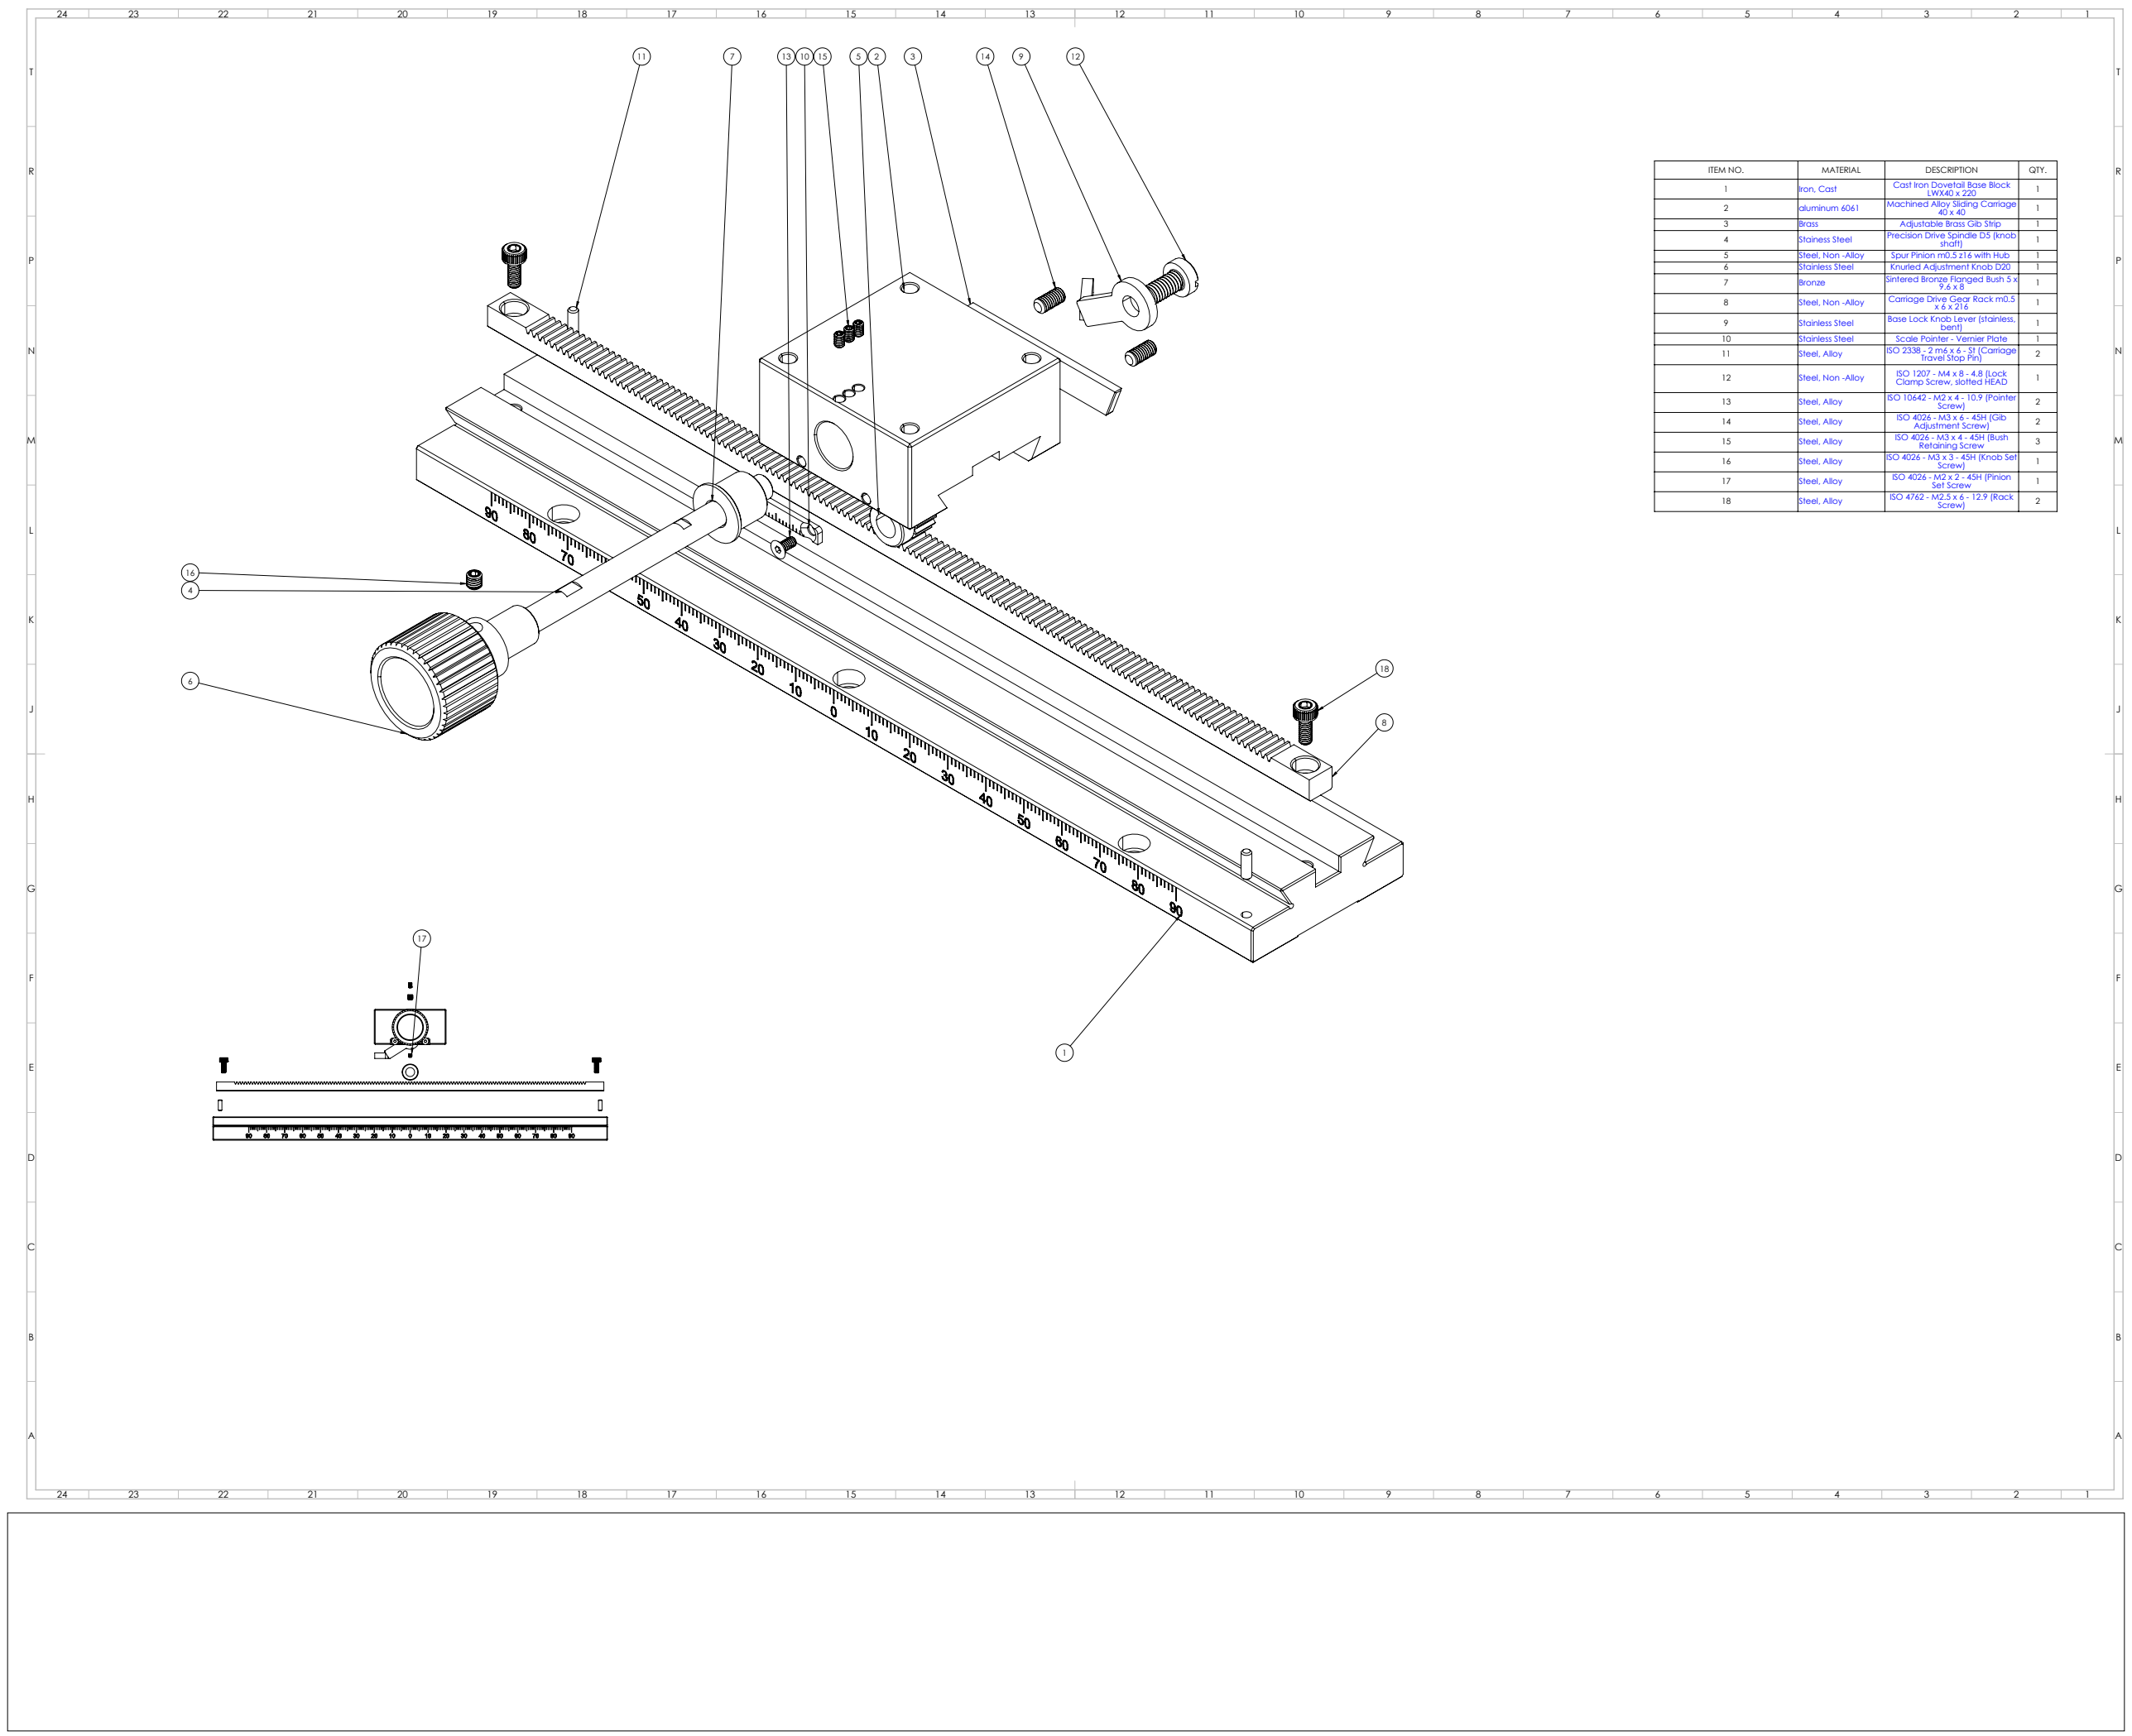
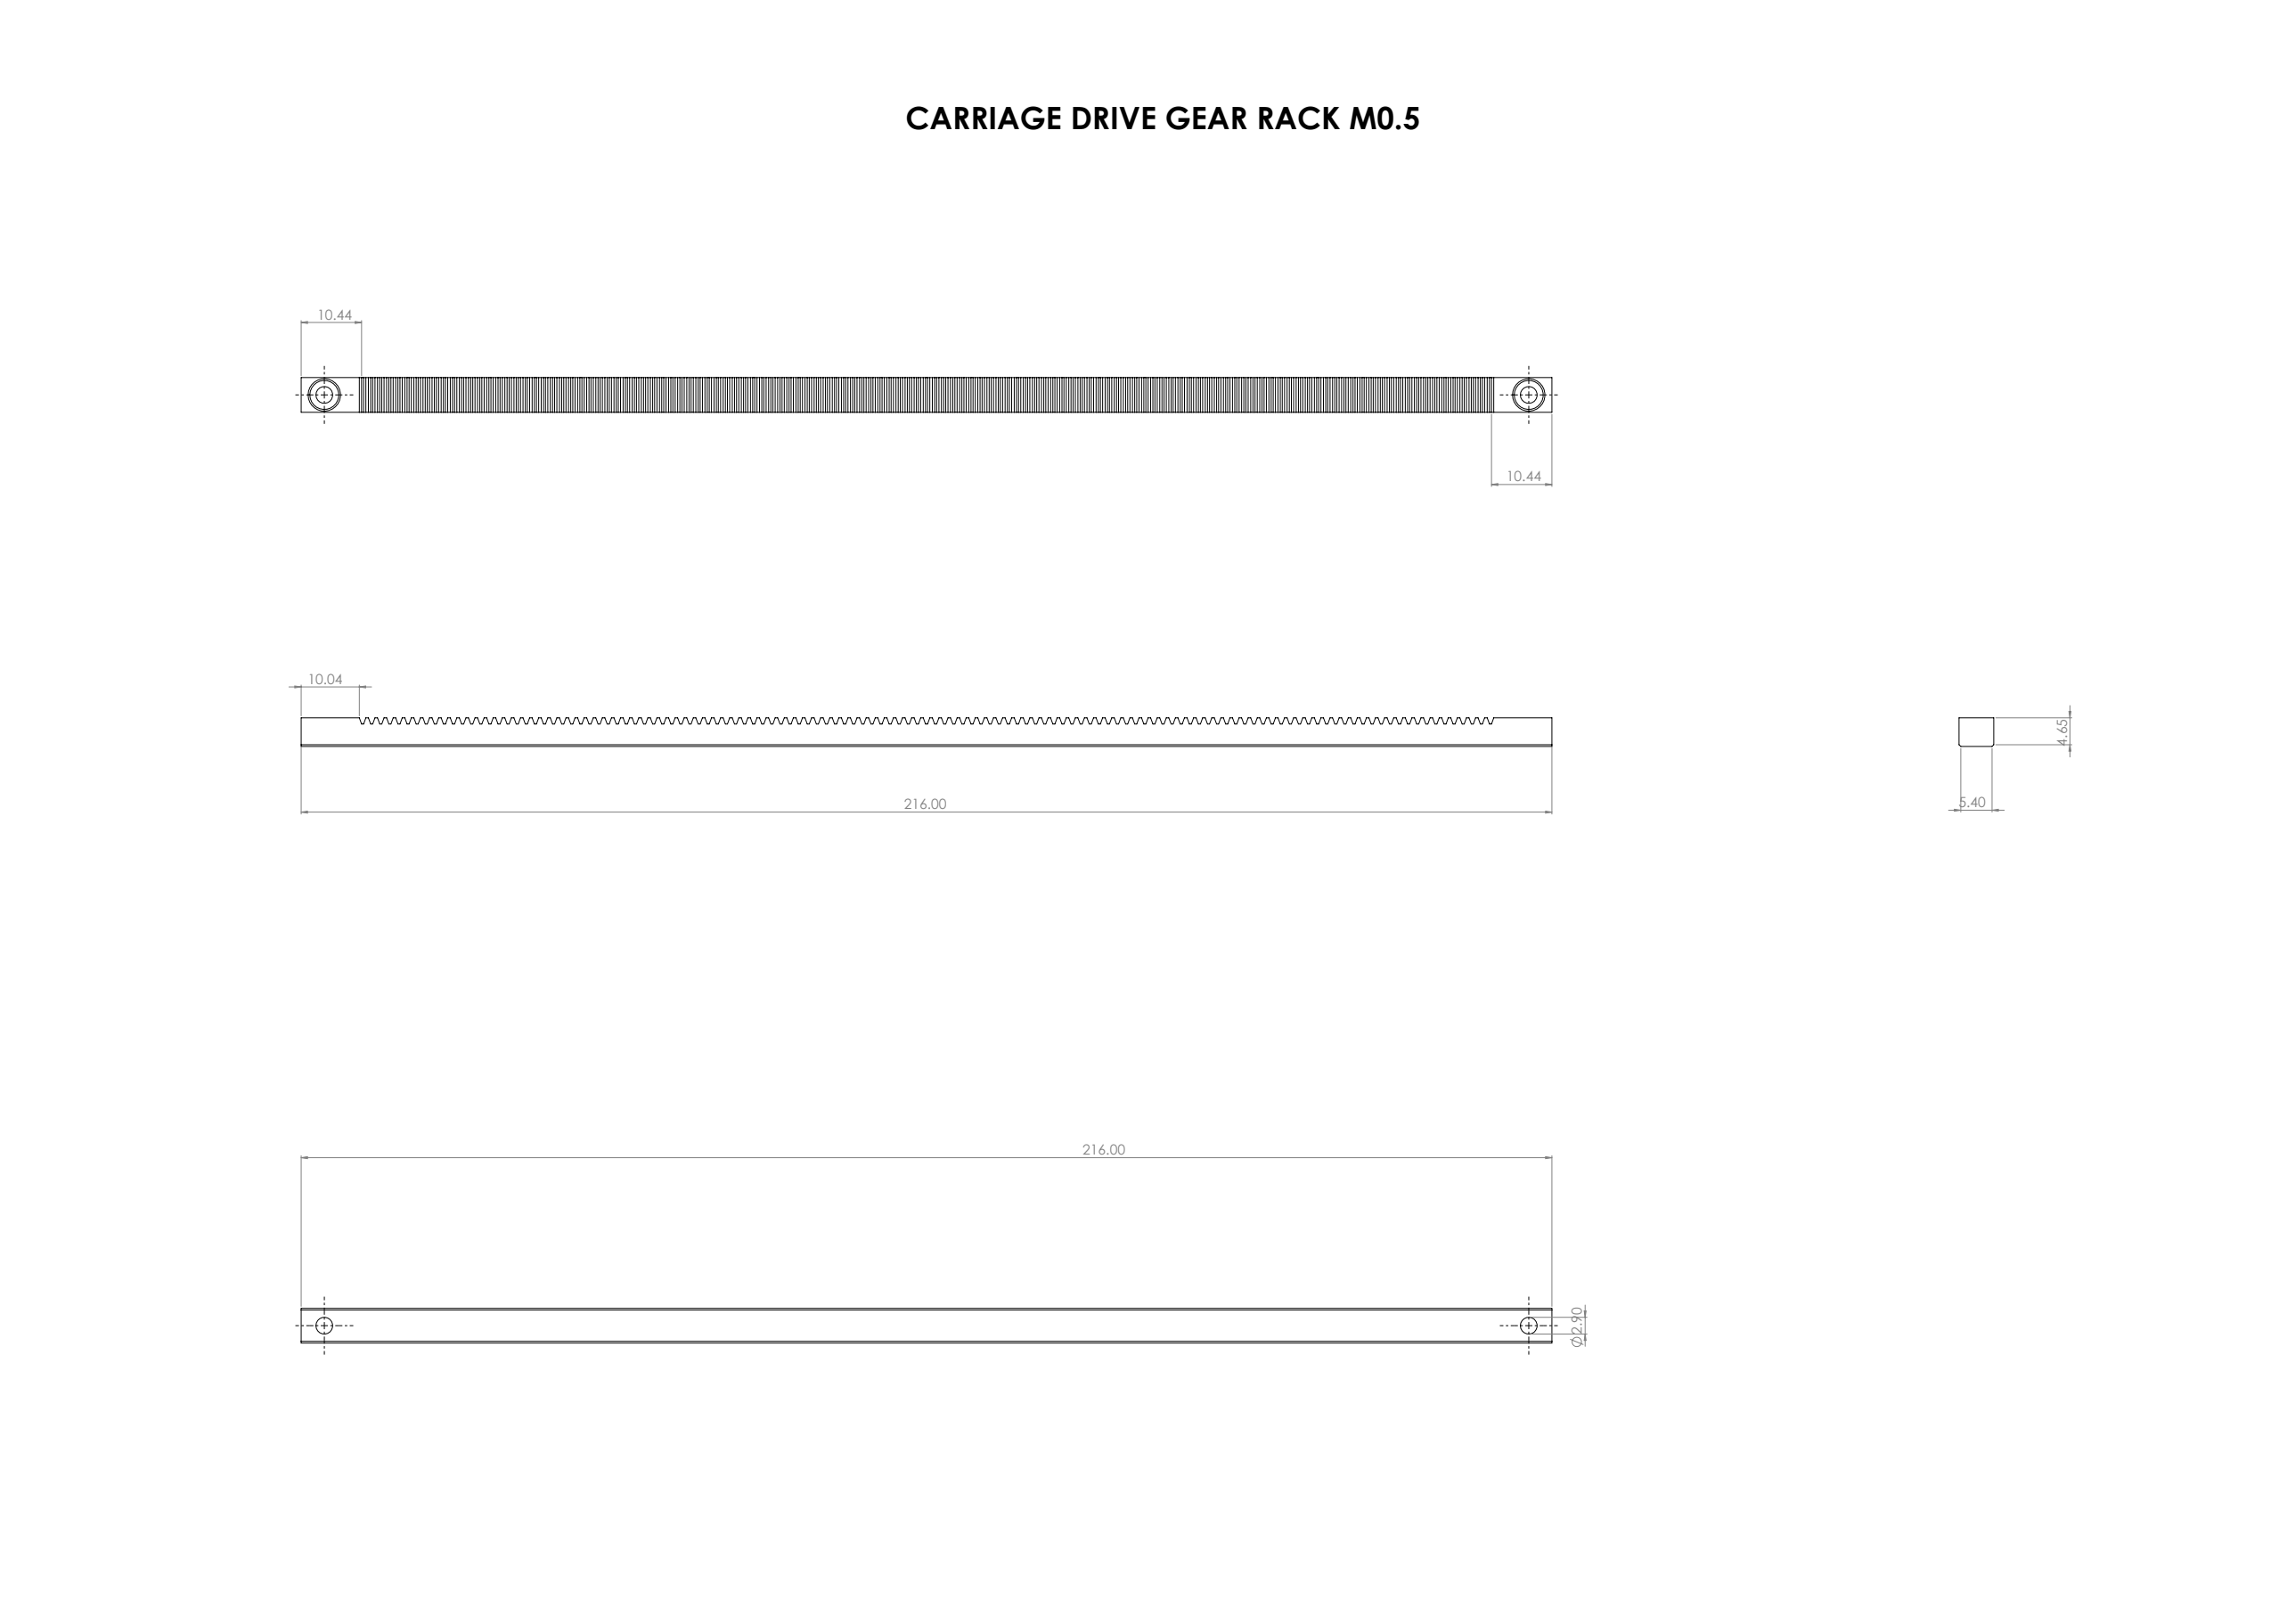
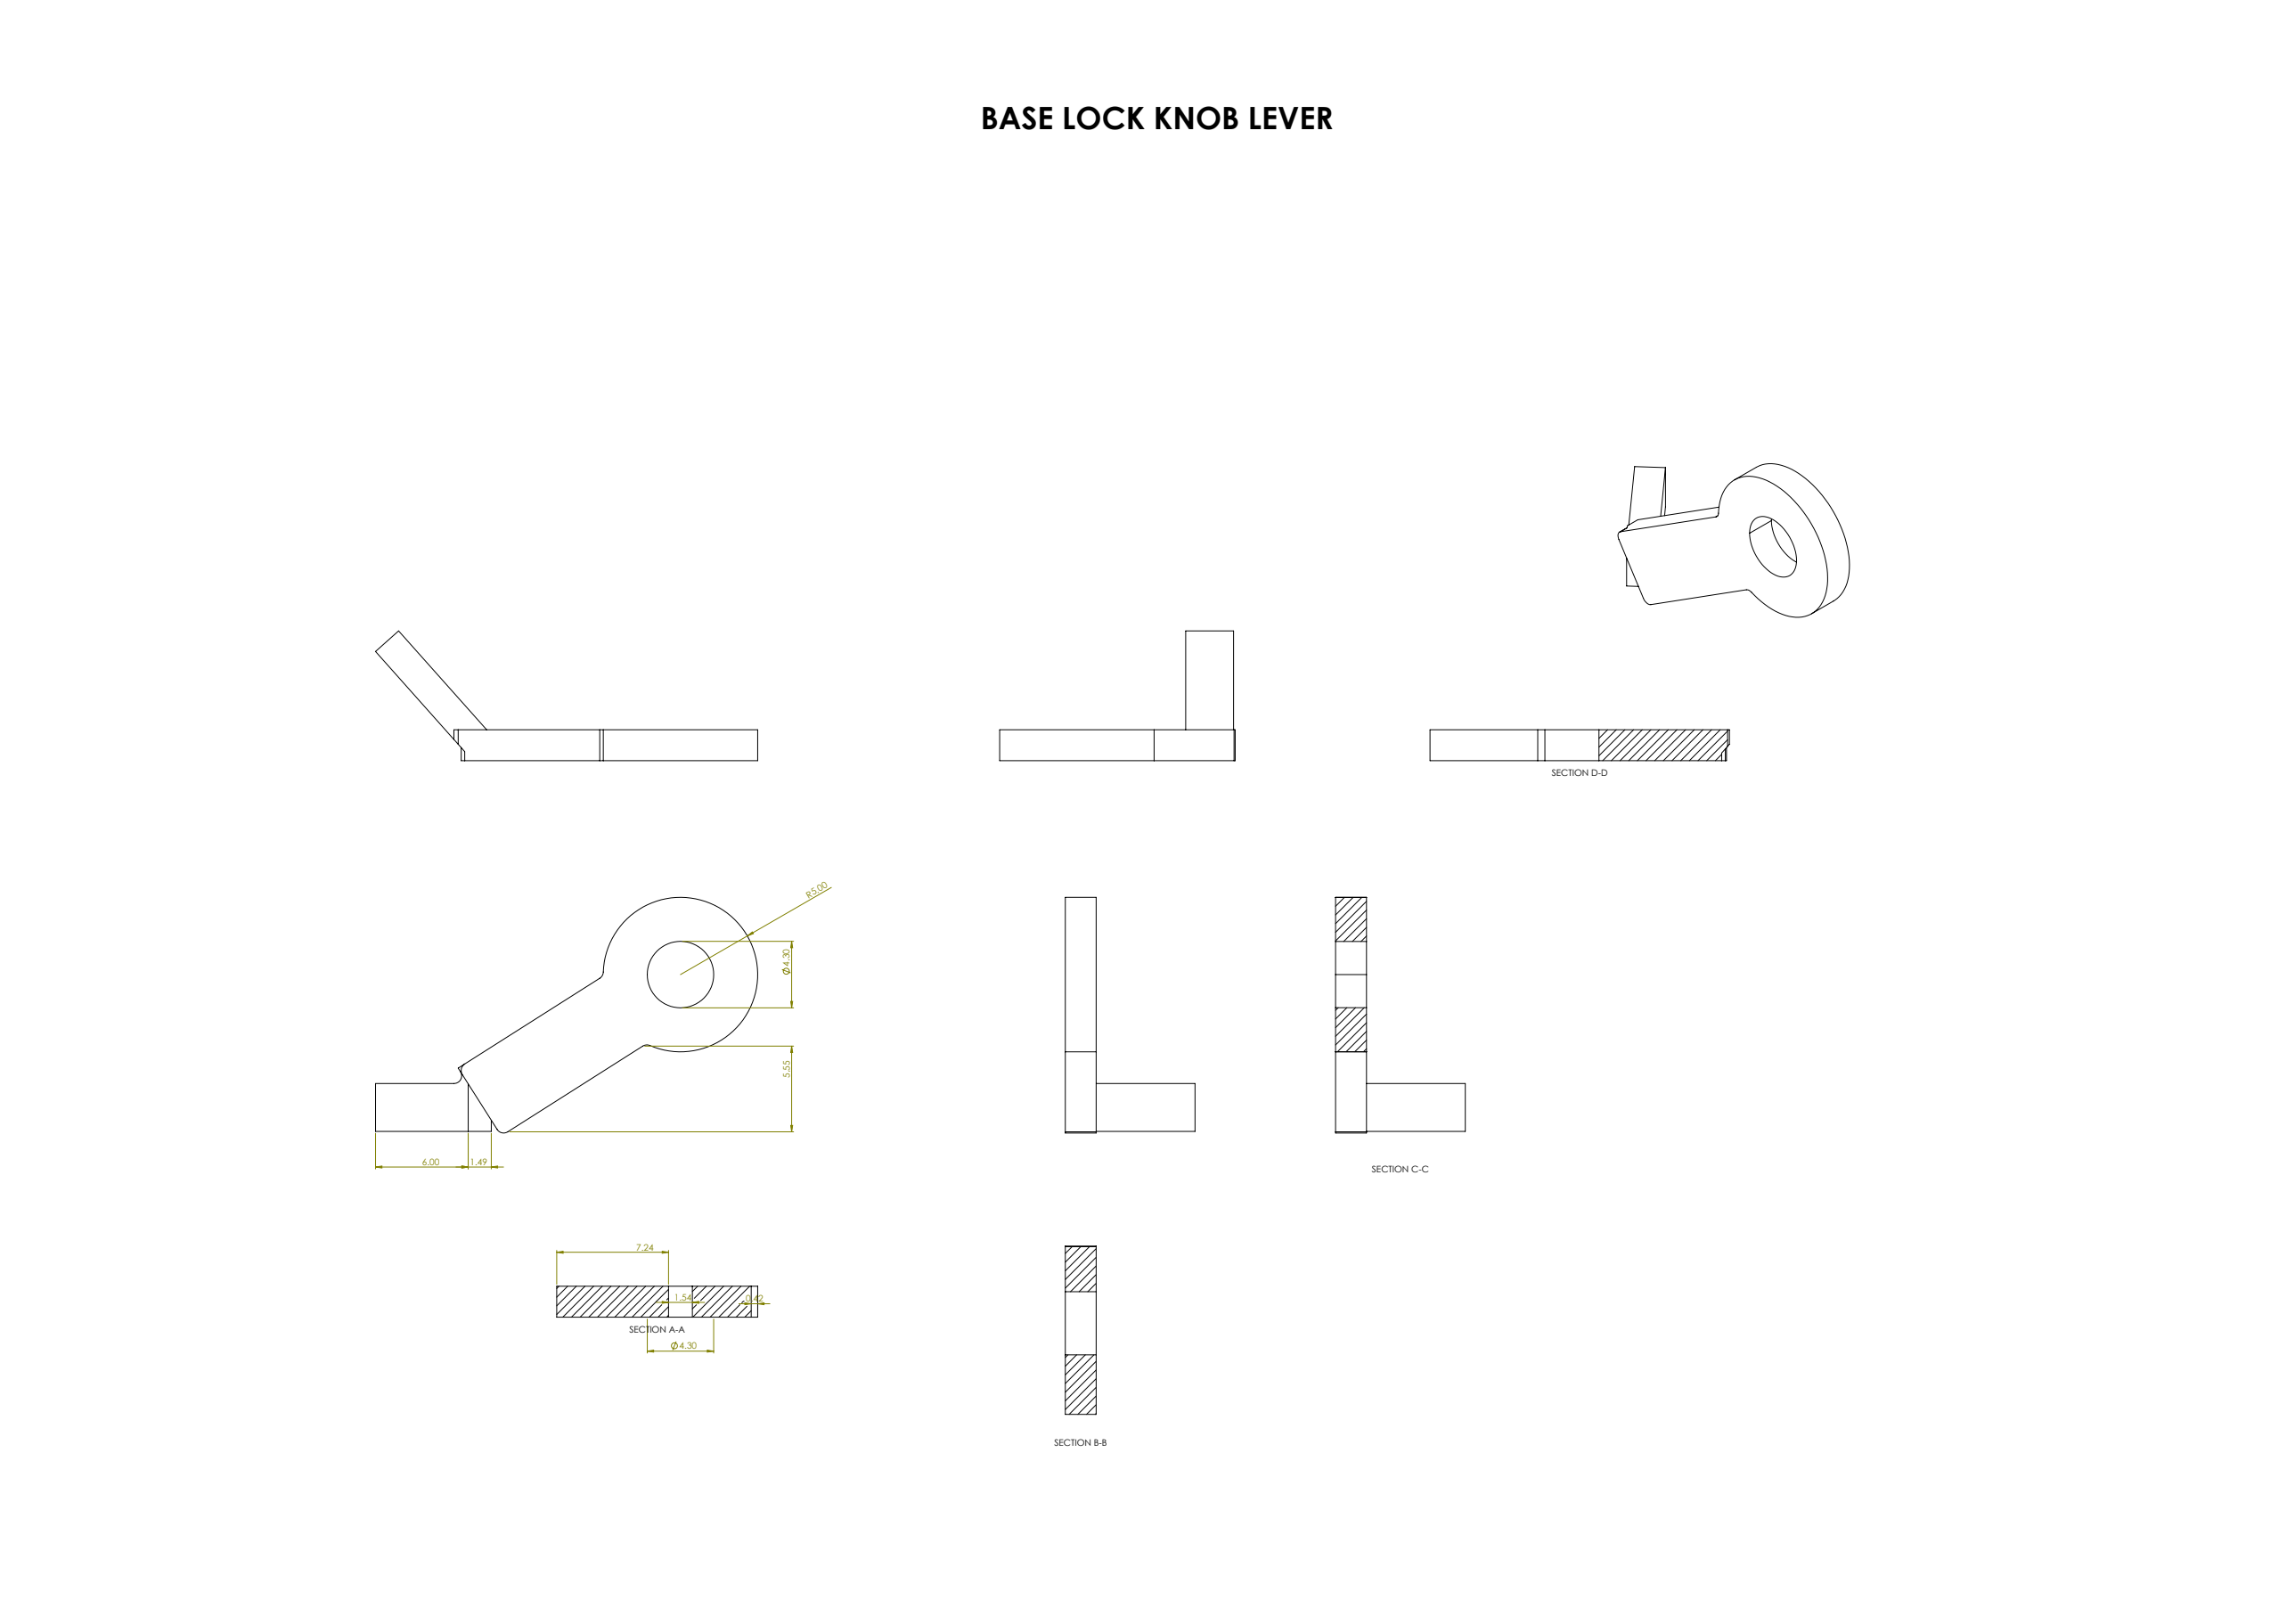
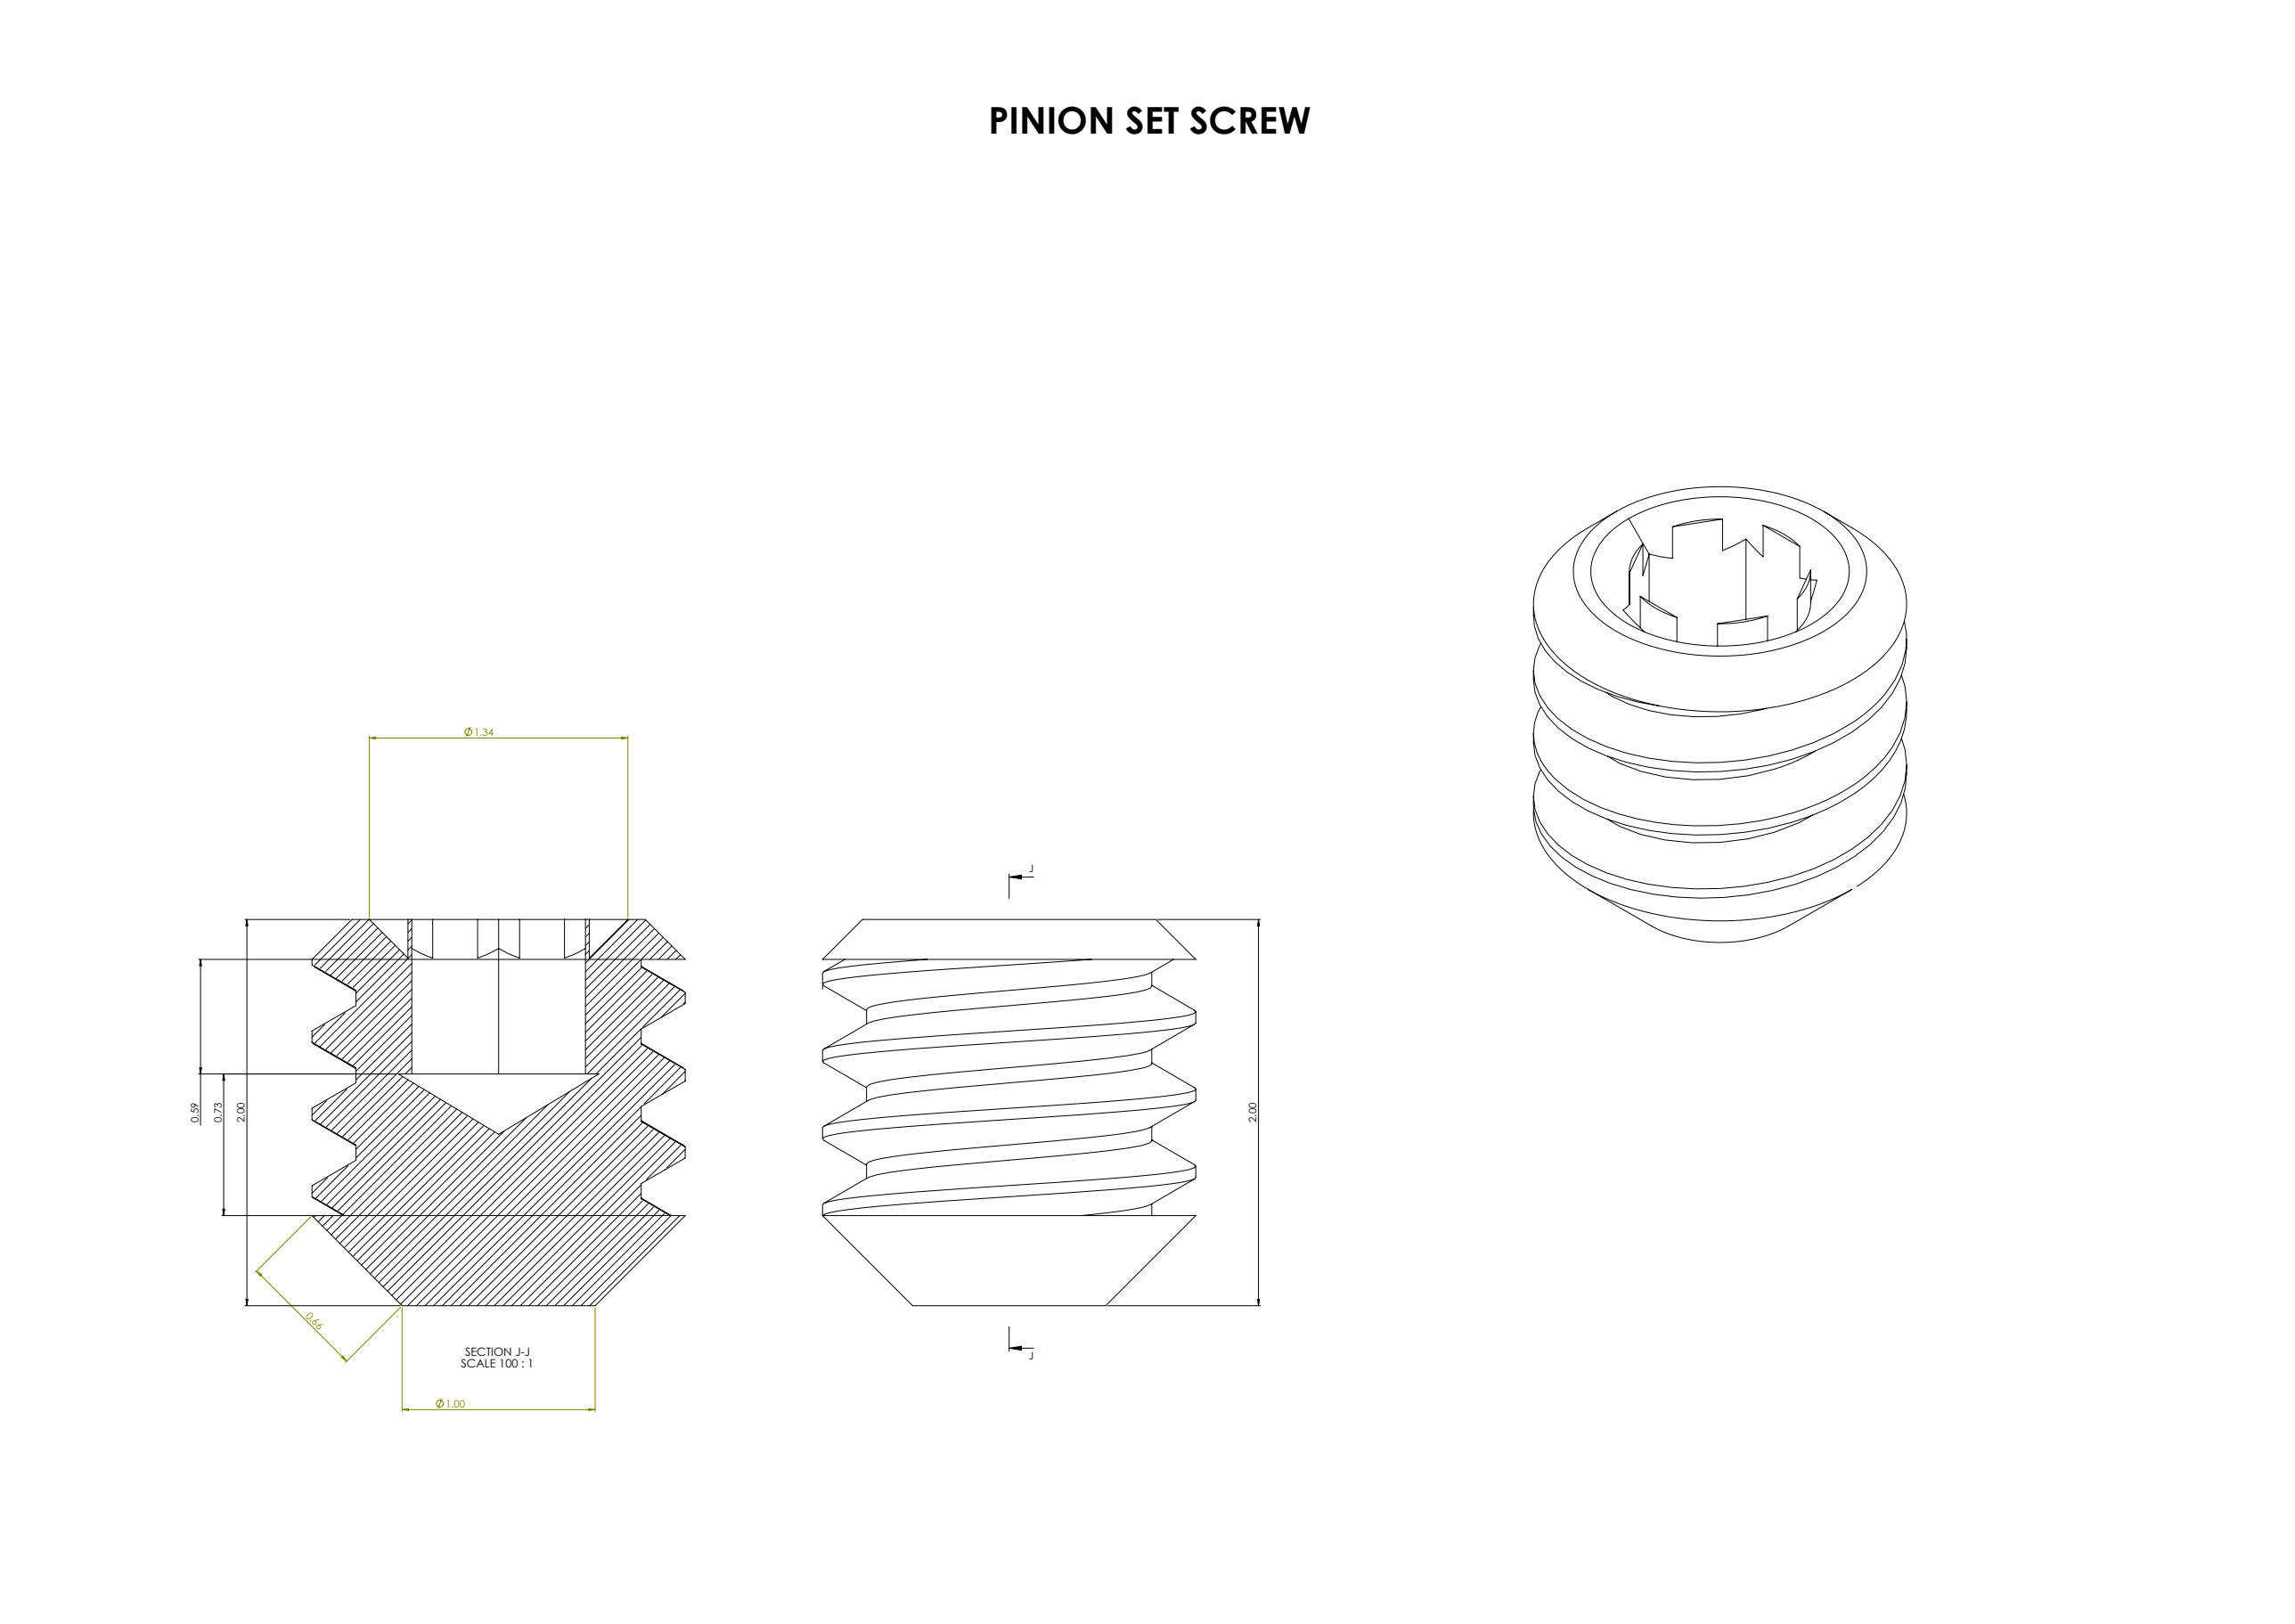
ISO-10303-21;
HEADER;
/* Generated by software containing ST-Developer
 * from STEP Tools, Inc. (www.steptools.com) 
 */

FILE_DESCRIPTION(
/* description */ (''),
/* implementation_level */ '2;1');

FILE_NAME(
/* name */ 'MAS-254',
/* time_stamp */ '2026-10-05T09:57:53+05:00',
/* author */ (''),
/* organization */ (''),
/* preprocessor_version */ 'ST-DEVELOPER v20.2',
/* originating_system */ 'Autodesk Translation Framework v15.15.0.0',
/* authorisation */ '');

FILE_SCHEMA (('AUTOMOTIVE_DESIGN { 1 0 10303 214 3 1 1 }'));
ENDSEC;

DATA;
#10=MECHANICAL_DESIGN_GEOMETRIC_PRESENTATION_REPRESENTATION('',(#551,#552,
#553,#554,#555,#556,#557,#558,#559,#560,#561,#562,#563,#564,#565,#566,#567,
#568),#113984);
#11=ITEM_DEFINED_TRANSFORMATION($,$,#60610,#63752);
#12=ITEM_DEFINED_TRANSFORMATION($,$,#61812,#63753);
#13=ITEM_DEFINED_TRANSFORMATION($,$,#61948,#63754);
#14=ITEM_DEFINED_TRANSFORMATION($,$,#61969,#63755);
#15=ITEM_DEFINED_TRANSFORMATION($,$,#61989,#63756);
#16=ITEM_DEFINED_TRANSFORMATION($,$,#62138,#63757);
#17=ITEM_DEFINED_TRANSFORMATION($,$,#62375,#63758);
#18=ITEM_DEFINED_TRANSFORMATION($,$,#62396,#63759);
#19=ITEM_DEFINED_TRANSFORMATION($,$,#62923,#63760);
#20=ITEM_DEFINED_TRANSFORMATION($,$,#62957,#63761);
#21=ITEM_DEFINED_TRANSFORMATION($,$,#63742,#63762);
#22=ITEM_DEFINED_TRANSFORMATION($,$,#63058,#63763);
#23=ITEM_DEFINED_TRANSFORMATION($,$,#63421,#63764);
#24=ITEM_DEFINED_TRANSFORMATION($,$,#63259,#63765);
#25=ITEM_DEFINED_TRANSFORMATION($,$,#63344,#63766);
#26=ITEM_DEFINED_TRANSFORMATION($,$,#63115,#63767);
#27=ITEM_DEFINED_TRANSFORMATION($,$,#63188,#63768);
#28=ITEM_DEFINED_TRANSFORMATION($,$,#63462,#63769);
#29=ITEM_DEFINED_TRANSFORMATION($,$,#63259,#63770);
#30=ITEM_DEFINED_TRANSFORMATION($,$,#63344,#63771);
#31=ITEM_DEFINED_TRANSFORMATION($,$,#63344,#63772);
#32=ITEM_DEFINED_TRANSFORMATION($,$,#63421,#63773);
#33=ITEM_DEFINED_TRANSFORMATION($,$,#63462,#63774);
#34=ITEM_DEFINED_TRANSFORMATION($,$,#63742,#63775);
#35=(
REPRESENTATION_RELATIONSHIP($,$,#114052,#114051)
REPRESENTATION_RELATIONSHIP_WITH_TRANSFORMATION(#11)
SHAPE_REPRESENTATION_RELATIONSHIP()
);
#36=(
REPRESENTATION_RELATIONSHIP($,$,#114053,#114051)
REPRESENTATION_RELATIONSHIP_WITH_TRANSFORMATION(#12)
SHAPE_REPRESENTATION_RELATIONSHIP()
);
#37=(
REPRESENTATION_RELATIONSHIP($,$,#114054,#114051)
REPRESENTATION_RELATIONSHIP_WITH_TRANSFORMATION(#13)
SHAPE_REPRESENTATION_RELATIONSHIP()
);
#38=(
REPRESENTATION_RELATIONSHIP($,$,#114055,#114051)
REPRESENTATION_RELATIONSHIP_WITH_TRANSFORMATION(#14)
SHAPE_REPRESENTATION_RELATIONSHIP()
);
#39=(
REPRESENTATION_RELATIONSHIP($,$,#114056,#114051)
REPRESENTATION_RELATIONSHIP_WITH_TRANSFORMATION(#15)
SHAPE_REPRESENTATION_RELATIONSHIP()
);
#40=(
REPRESENTATION_RELATIONSHIP($,$,#114057,#114051)
REPRESENTATION_RELATIONSHIP_WITH_TRANSFORMATION(#16)
SHAPE_REPRESENTATION_RELATIONSHIP()
);
#41=(
REPRESENTATION_RELATIONSHIP($,$,#114058,#114051)
REPRESENTATION_RELATIONSHIP_WITH_TRANSFORMATION(#17)
SHAPE_REPRESENTATION_RELATIONSHIP()
);
#42=(
REPRESENTATION_RELATIONSHIP($,$,#114059,#114051)
REPRESENTATION_RELATIONSHIP_WITH_TRANSFORMATION(#18)
SHAPE_REPRESENTATION_RELATIONSHIP()
);
#43=(
REPRESENTATION_RELATIONSHIP($,$,#114060,#114051)
REPRESENTATION_RELATIONSHIP_WITH_TRANSFORMATION(#19)
SHAPE_REPRESENTATION_RELATIONSHIP()
);
#44=(
REPRESENTATION_RELATIONSHIP($,$,#114061,#114051)
REPRESENTATION_RELATIONSHIP_WITH_TRANSFORMATION(#20)
SHAPE_REPRESENTATION_RELATIONSHIP()
);
#45=(
REPRESENTATION_RELATIONSHIP($,$,#114069,#114051)
REPRESENTATION_RELATIONSHIP_WITH_TRANSFORMATION(#21)
SHAPE_REPRESENTATION_RELATIONSHIP()
);
#46=(
REPRESENTATION_RELATIONSHIP($,$,#114062,#114051)
REPRESENTATION_RELATIONSHIP_WITH_TRANSFORMATION(#22)
SHAPE_REPRESENTATION_RELATIONSHIP()
);
#47=(
REPRESENTATION_RELATIONSHIP($,$,#114067,#114051)
REPRESENTATION_RELATIONSHIP_WITH_TRANSFORMATION(#23)
SHAPE_REPRESENTATION_RELATIONSHIP()
);
#48=(
REPRESENTATION_RELATIONSHIP($,$,#114065,#114051)
REPRESENTATION_RELATIONSHIP_WITH_TRANSFORMATION(#24)
SHAPE_REPRESENTATION_RELATIONSHIP()
);
#49=(
REPRESENTATION_RELATIONSHIP($,$,#114066,#114051)
REPRESENTATION_RELATIONSHIP_WITH_TRANSFORMATION(#25)
SHAPE_REPRESENTATION_RELATIONSHIP()
);
#50=(
REPRESENTATION_RELATIONSHIP($,$,#114063,#114051)
REPRESENTATION_RELATIONSHIP_WITH_TRANSFORMATION(#26)
SHAPE_REPRESENTATION_RELATIONSHIP()
);
#51=(
REPRESENTATION_RELATIONSHIP($,$,#114064,#114051)
REPRESENTATION_RELATIONSHIP_WITH_TRANSFORMATION(#27)
SHAPE_REPRESENTATION_RELATIONSHIP()
);
#52=(
REPRESENTATION_RELATIONSHIP($,$,#114068,#114051)
REPRESENTATION_RELATIONSHIP_WITH_TRANSFORMATION(#28)
SHAPE_REPRESENTATION_RELATIONSHIP()
);
#53=(
REPRESENTATION_RELATIONSHIP($,$,#114065,#114051)
REPRESENTATION_RELATIONSHIP_WITH_TRANSFORMATION(#29)
SHAPE_REPRESENTATION_RELATIONSHIP()
);
#54=(
REPRESENTATION_RELATIONSHIP($,$,#114066,#114051)
REPRESENTATION_RELATIONSHIP_WITH_TRANSFORMATION(#30)
SHAPE_REPRESENTATION_RELATIONSHIP()
);
#55=(
REPRESENTATION_RELATIONSHIP($,$,#114066,#114051)
REPRESENTATION_RELATIONSHIP_WITH_TRANSFORMATION(#31)
SHAPE_REPRESENTATION_RELATIONSHIP()
);
#56=(
REPRESENTATION_RELATIONSHIP($,$,#114067,#114051)
REPRESENTATION_RELATIONSHIP_WITH_TRANSFORMATION(#32)
SHAPE_REPRESENTATION_RELATIONSHIP()
);
#57=(
REPRESENTATION_RELATIONSHIP($,$,#114068,#114051)
REPRESENTATION_RELATIONSHIP_WITH_TRANSFORMATION(#33)
SHAPE_REPRESENTATION_RELATIONSHIP()
);
#58=(
REPRESENTATION_RELATIONSHIP($,$,#114069,#114051)
REPRESENTATION_RELATIONSHIP_WITH_TRANSFORMATION(#34)
SHAPE_REPRESENTATION_RELATIONSHIP()
);
#59=CONTEXT_DEPENDENT_SHAPE_REPRESENTATION(#35,#114027);
#60=CONTEXT_DEPENDENT_SHAPE_REPRESENTATION(#36,#114028);
#61=CONTEXT_DEPENDENT_SHAPE_REPRESENTATION(#37,#114029);
#62=CONTEXT_DEPENDENT_SHAPE_REPRESENTATION(#38,#114030);
#63=CONTEXT_DEPENDENT_SHAPE_REPRESENTATION(#39,#114031);
#64=CONTEXT_DEPENDENT_SHAPE_REPRESENTATION(#40,#114032);
#65=CONTEXT_DEPENDENT_SHAPE_REPRESENTATION(#41,#114033);
#66=CONTEXT_DEPENDENT_SHAPE_REPRESENTATION(#42,#114034);
#67=CONTEXT_DEPENDENT_SHAPE_REPRESENTATION(#43,#114035);
#68=CONTEXT_DEPENDENT_SHAPE_REPRESENTATION(#44,#114036);
#69=CONTEXT_DEPENDENT_SHAPE_REPRESENTATION(#45,#114037);
#70=CONTEXT_DEPENDENT_SHAPE_REPRESENTATION(#46,#114038);
#71=CONTEXT_DEPENDENT_SHAPE_REPRESENTATION(#47,#114039);
#72=CONTEXT_DEPENDENT_SHAPE_REPRESENTATION(#48,#114040);
#73=CONTEXT_DEPENDENT_SHAPE_REPRESENTATION(#49,#114041);
#74=CONTEXT_DEPENDENT_SHAPE_REPRESENTATION(#50,#114042);
#75=CONTEXT_DEPENDENT_SHAPE_REPRESENTATION(#51,#114043);
#76=CONTEXT_DEPENDENT_SHAPE_REPRESENTATION(#52,#114044);
#77=CONTEXT_DEPENDENT_SHAPE_REPRESENTATION(#53,#114045);
#78=CONTEXT_DEPENDENT_SHAPE_REPRESENTATION(#54,#114046);
#79=CONTEXT_DEPENDENT_SHAPE_REPRESENTATION(#55,#114047);
#80=CONTEXT_DEPENDENT_SHAPE_REPRESENTATION(#56,#114048);
#81=CONTEXT_DEPENDENT_SHAPE_REPRESENTATION(#57,#114049);
#82=CONTEXT_DEPENDENT_SHAPE_REPRESENTATION(#58,#114050);
#83=NEXT_ASSEMBLY_USAGE_OCCURRENCE(
'Cast Iron Dovetail Base Block LWX40 x 220:1',
'Cast Iron Dovetail Base Block LWX40 x 220:1',
'Cast Iron Dovetail Base Block LWX40 x 220:1',#114071,#114072,
'Cast Iron Dovetail Base Block LWX40 x 220:1');
#84=NEXT_ASSEMBLY_USAGE_OCCURRENCE(
'Machined Alloy Sliding Carriage 40 x 40:1',
'Machined Alloy Sliding Carriage 40 x 40:1',
'Machined Alloy Sliding Carriage 40 x 40:1',#114071,#114073,
'Machined Alloy Sliding Carriage 40 x 40:1');
#85=NEXT_ASSEMBLY_USAGE_OCCURRENCE('Adjustable Brass Gib Strip:1',
'Adjustable Brass Gib Strip:1','Adjustable Brass Gib Strip:1',#114071,#114074,
'Adjustable Brass Gib Strip:1');
#86=NEXT_ASSEMBLY_USAGE_OCCURRENCE(
'Precision Drive Spindle D5 (knob shaft):1',
'Precision Drive Spindle D5 (knob shaft):1',
'Precision Drive Spindle D5 (knob shaft):1',#114071,#114075,
'Precision Drive Spindle D5 (knob shaft):1');
#87=NEXT_ASSEMBLY_USAGE_OCCURRENCE('Spur Pinion m0.5 z16 with Hub:1',
'Spur Pinion m0.5 z16 with Hub:1','Spur Pinion m0.5 z16 with Hub:1',#114071,
#114076,'Spur Pinion m0.5 z16 with Hub:1');
#88=NEXT_ASSEMBLY_USAGE_OCCURRENCE('Knurled Adjustment Knob D20:1',
'Knurled Adjustment Knob D20:1','Knurled Adjustment Knob D20:1',#114071,
#114077,'Knurled Adjustment Knob D20:1');
#89=NEXT_ASSEMBLY_USAGE_OCCURRENCE(
'Sintered Bronze Flanged Bush 5 x 9.6 x 8:1',
'Sintered Bronze Flanged Bush 5 x 9.6 x 8:1',
'Sintered Bronze Flanged Bush 5 x 9.6 x 8:1',#114071,#114078,
'Sintered Bronze Flanged Bush 5 x 9.6 x 8:1');
#90=NEXT_ASSEMBLY_USAGE_OCCURRENCE(
'Carriage Drive Gear Rack m0.5 x 6 x 216:1',
'Carriage Drive Gear Rack m0.5 x 6 x 216:1',
'Carriage Drive Gear Rack m0.5 x 6 x 216:1',#114071,#114079,
'Carriage Drive Gear Rack m0.5 x 6 x 216:1');
#91=NEXT_ASSEMBLY_USAGE_OCCURRENCE(
'Base Lock Knob Lever (stainless, bent):1',
'Base Lock Knob Lever (stainless, bent):1',
'Base Lock Knob Lever (stainless, bent):1',#114071,#114080,
'Base Lock Knob Lever (stainless, bent):1');
#92=NEXT_ASSEMBLY_USAGE_OCCURRENCE('Scale Pointer - Vernier Plate:1',
'Scale Pointer - Vernier Plate:1','Scale Pointer - Vernier Plate:1',#114071,
#114081,'Scale Pointer - Vernier Plate:1');
#93=NEXT_ASSEMBLY_USAGE_OCCURRENCE(
'ISO 2338 - 2 m6 x 6 - St (Carriage Travel Stop Pin):1',
'ISO 2338 - 2 m6 x 6 - St (Carriage Travel Stop Pin):1',
'ISO 2338 - 2 m6 x 6 - St (Carriage Travel Stop Pin):1',#114071,#114089,
'ISO 2338 - 2 m6 x 6 - St (Carriage Travel Stop Pin):1');
#94=NEXT_ASSEMBLY_USAGE_OCCURRENCE(
'ISO 1207 - M4 x 8 - 4.8 (Lock Clamp Screw, slotted cheese head):1',
'ISO 1207 - M4 x 8 - 4.8 (Lock Clamp Screw, slotted cheese head):1',
'ISO 1207 - M4 x 8 - 4.8 (Lock Clamp Screw, slotted cheese head):1',#114071,
#114082,
'ISO 1207 - M4 x 8 - 4.8 (Lock Clamp Screw, slotted cheese head):1');
#95=NEXT_ASSEMBLY_USAGE_OCCURRENCE(
'ISO 10642 - M2 x 4 - 10.9 (Pointer Screw):1',
'ISO 10642 - M2 x 4 - 10.9 (Pointer Screw):1',
'ISO 10642 - M2 x 4 - 10.9 (Pointer Screw):1',#114071,#114087,
'ISO 10642 - M2 x 4 - 10.9 (Pointer Screw):1');
#96=NEXT_ASSEMBLY_USAGE_OCCURRENCE(
'ISO 4026 - M3 x 6 - 45H (Gib Adjustment Screw):1',
'ISO 4026 - M3 x 6 - 45H (Gib Adjustment Screw):1',
'ISO 4026 - M3 x 6 - 45H (Gib Adjustment Screw):1',#114071,#114085,
'ISO 4026 - M3 x 6 - 45H (Gib Adjustment Screw):1');
#97=NEXT_ASSEMBLY_USAGE_OCCURRENCE(
'ISO 4026 - M3 x 4 - 45H (Bush Retaining Screw):1',
'ISO 4026 - M3 x 4 - 45H (Bush Retaining Screw):1',
'ISO 4026 - M3 x 4 - 45H (Bush Retaining Screw):1',#114071,#114086,
'ISO 4026 - M3 x 4 - 45H (Bush Retaining Screw):1');
#98=NEXT_ASSEMBLY_USAGE_OCCURRENCE(
'ISO 4026 - M3 x 3 - 45H (Knob Set Screw):1',
'ISO 4026 - M3 x 3 - 45H (Knob Set Screw):1',
'ISO 4026 - M3 x 3 - 45H (Knob Set Screw):1',#114071,#114083,
'ISO 4026 - M3 x 3 - 45H (Knob Set Screw):1');
#99=NEXT_ASSEMBLY_USAGE_OCCURRENCE(
'ISO 4026 - M2 x 2 - 45H (Pinion Set Screw):1',
'ISO 4026 - M2 x 2 - 45H (Pinion Set Screw):1',
'ISO 4026 - M2 x 2 - 45H (Pinion Set Screw):1',#114071,#114084,
'ISO 4026 - M2 x 2 - 45H (Pinion Set Screw):1');
#100=NEXT_ASSEMBLY_USAGE_OCCURRENCE(
'ISO 4762 - M2.5 x 6 - 12.9 (Rack Screw):1',
'ISO 4762 - M2.5 x 6 - 12.9 (Rack Screw):1',
'ISO 4762 - M2.5 x 6 - 12.9 (Rack Screw):1',#114071,#114088,
'ISO 4762 - M2.5 x 6 - 12.9 (Rack Screw):1');
#101=NEXT_ASSEMBLY_USAGE_OCCURRENCE(
'ISO 4026 - M3 x 6 - 45H (Gib Adjustment Screw):2',
'ISO 4026 - M3 x 6 - 45H (Gib Adjustment Screw):2',
'ISO 4026 - M3 x 6 - 45H (Gib Adjustment Screw):2',#114071,#114085,
'ISO 4026 - M3 x 6 - 45H (Gib Adjustment Screw):2');
#102=NEXT_ASSEMBLY_USAGE_OCCURRENCE(
'ISO 4026 - M3 x 4 - 45H (Bush Retaining Screw):2',
'ISO 4026 - M3 x 4 - 45H (Bush Retaining Screw):2',
'ISO 4026 - M3 x 4 - 45H (Bush Retaining Screw):2',#114071,#114086,
'ISO 4026 - M3 x 4 - 45H (Bush Retaining Screw):2');
#103=NEXT_ASSEMBLY_USAGE_OCCURRENCE(
'ISO 4026 - M3 x 4 - 45H (Bush Retaining Screw):3',
'ISO 4026 - M3 x 4 - 45H (Bush Retaining Screw):3',
'ISO 4026 - M3 x 4 - 45H (Bush Retaining Screw):3',#114071,#114086,
'ISO 4026 - M3 x 4 - 45H (Bush Retaining Screw):3');
#104=NEXT_ASSEMBLY_USAGE_OCCURRENCE(
'ISO 10642 - M2 x 4 - 10.9 (Pointer Screw):2',
'ISO 10642 - M2 x 4 - 10.9 (Pointer Screw):2',
'ISO 10642 - M2 x 4 - 10.9 (Pointer Screw):2',#114071,#114087,
'ISO 10642 - M2 x 4 - 10.9 (Pointer Screw):2');
#105=NEXT_ASSEMBLY_USAGE_OCCURRENCE(
'ISO 4762 - M2.5 x 6 - 12.9 (Rack Screw):2',
'ISO 4762 - M2.5 x 6 - 12.9 (Rack Screw):2',
'ISO 4762 - M2.5 x 6 - 12.9 (Rack Screw):2',#114071,#114088,
'ISO 4762 - M2.5 x 6 - 12.9 (Rack Screw):2');
#106=NEXT_ASSEMBLY_USAGE_OCCURRENCE(
'ISO 2338 - 2 m6 x 6 - St (Carriage Travel Stop Pin):2',
'ISO 2338 - 2 m6 x 6 - St (Carriage Travel Stop Pin):2',
'ISO 2338 - 2 m6 x 6 - St (Carriage Travel Stop Pin):2',#114071,#114089,
'ISO 2338 - 2 m6 x 6 - St (Carriage Travel Stop Pin):2');
#107=TOROIDAL_SURFACE('',#63090,2.154,0.2);
#108=TOROIDAL_SURFACE('',#63498,1.315,0.1);
#109=TOROIDAL_SURFACE('',#63692,2.05,0.2);
#110=(
BOUNDED_SURFACE()
B_SPLINE_SURFACE(5,1,((#92751,#92752),(#92753,#92754),(#92755,#92756),(#92757,
#92758),(#92759,#92760),(#92761,#92762),(#92763,#92764),(#92765,#92766),
(#92767,#92768),(#92769,#92770),(#92771,#92772),(#92773,#92774),(#92775,
#92776),(#92777,#92778),(#92779,#92780),(#92781,#92782),(#92783,#92784),
(#92785,#92786),(#92787,#92788),(#92789,#92790),(#92791,#92792),(#92793,
#92794),(#92795,#92796),(#92797,#92798),(#92799,#92800),(#92801,#92802),
(#92803,#92804),(#92805,#92806),(#92807,#92808),(#92809,#92810),(#92811,
#92812),(#92813,#92814),(#92815,#92816),(#92817,#92818),(#92819,#92820)),
 .UNSPECIFIED.,.F.,.F.,.F.)
B_SPLINE_SURFACE_WITH_KNOTS((6,1,1,1,1,1,1,1,1,1,1,1,1,1,1,1,1,1,1,1,1,
1,1,1,1,1,1,1,1,1,6),(2,2),(-1.,-0.966666666666667,-0.933333333333333,-0.9,
-0.866666666666667,-0.833333333333333,-0.8,-0.766666666666667,-0.733333333333333,
-0.7,-0.666666666666667,-0.633333333333333,-0.6,-0.566666666666667,-0.533333333333333,
-0.5,-0.466666666666667,-0.433333333333333,-0.4,-0.366666666666667,-0.333333333333333,
-0.3,-0.266666666666667,-0.233333333333333,-0.2,-0.166666666666667,-0.133333333333333,
-0.1,-0.0666666666666667,-0.0333333333333333,0.),(0.,0.5),.UNSPECIFIED.)
GEOMETRIC_REPRESENTATION_ITEM()
RATIONAL_B_SPLINE_SURFACE(((1.,1.),(1.,1.),(1.,1.),(1.,1.),(1.,1.),(1.,
1.),(1.,1.),(1.,1.),(1.,1.),(1.,1.),(1.,1.),(1.,1.),(1.,1.),(1.,1.),(1.,
1.),(1.,1.),(1.,1.),(1.,1.),(1.,1.),(1.,1.),(1.,1.),(1.,1.),(1.,1.),(1.,
1.),(1.,1.),(1.,1.),(1.,1.),(1.,1.),(1.,1.),(1.,1.),(1.,1.),(1.,1.),(1.,
1.),(1.,1.),(1.,1.)))
REPRESENTATION_ITEM('')
SURFACE()
);
#111=(
BOUNDED_SURFACE()
B_SPLINE_SURFACE(5,1,((#92900,#92901),(#92902,#92903),(#92904,#92905),(#92906,
#92907),(#92908,#92909),(#92910,#92911),(#92912,#92913),(#92914,#92915),
(#92916,#92917),(#92918,#92919),(#92920,#92921),(#92922,#92923),(#92924,
#92925),(#92926,#92927),(#92928,#92929),(#92930,#92931),(#92932,#92933),
(#92934,#92935),(#92936,#92937),(#92938,#92939),(#92940,#92941),(#92942,
#92943),(#92944,#92945),(#92946,#92947),(#92948,#92949),(#92950,#92951),
(#92952,#92953),(#92954,#92955),(#92956,#92957),(#92958,#92959),(#92960,
#92961),(#92962,#92963),(#92964,#92965),(#92966,#92967),(#92968,#92969)),
 .UNSPECIFIED.,.F.,.F.,.F.)
B_SPLINE_SURFACE_WITH_KNOTS((6,1,1,1,1,1,1,1,1,1,1,1,1,1,1,1,1,1,1,1,1,
1,1,1,1,1,1,1,1,1,6),(2,2),(0.,0.0333333333333333,0.0666666666666667,0.1,
0.133333333333333,0.166666666666667,0.2,0.233333333333333,0.266666666666667,
0.3,0.333333333333333,0.366666666666667,0.4,0.433333333333333,0.466666666666667,
0.5,0.533333333333333,0.566666666666667,0.6,0.633333333333333,0.666666666666667,
0.7,0.733333333333333,0.766666666666667,0.8,0.833333333333333,0.866666666666667,
0.9,0.933333333333333,0.966666666666667,1.),(0.,0.5),.UNSPECIFIED.)
GEOMETRIC_REPRESENTATION_ITEM()
RATIONAL_B_SPLINE_SURFACE(((1.,1.),(1.,1.),(1.,1.),(1.,1.),(1.,1.),(1.,
1.),(1.,1.),(1.,1.),(1.,1.),(1.,1.),(1.,1.),(1.,1.),(1.,1.),(1.,1.),(1.,
1.),(1.,1.),(1.,1.),(1.,1.),(1.,1.),(1.,1.),(1.,1.),(1.,1.),(1.,1.),(1.,
1.),(1.,1.),(1.,1.),(1.,1.),(1.,1.),(1.,1.),(1.,1.),(1.,1.),(1.,1.),(1.,
1.),(1.,1.),(1.,1.)))
REPRESENTATION_ITEM('')
SURFACE()
);
#112=(
BOUNDED_SURFACE()
B_SPLINE_SURFACE(5,1,((#93181,#93182),(#93183,#93184),(#93185,#93186),(#93187,
#93188),(#93189,#93190),(#93191,#93192),(#93193,#93194),(#93195,#93196),
(#93197,#93198),(#93199,#93200),(#93201,#93202),(#93203,#93204),(#93205,
#93206),(#93207,#93208),(#93209,#93210),(#93211,#93212),(#93213,#93214),
(#93215,#93216),(#93217,#93218),(#93219,#93220),(#93221,#93222),(#93223,
#93224),(#93225,#93226),(#93227,#93228),(#93229,#93230),(#93231,#93232),
(#93233,#93234),(#93235,#93236),(#93237,#93238),(#93239,#93240),(#93241,
#93242),(#93243,#93244),(#93245,#93246),(#93247,#93248),(#93249,#93250)),
 .UNSPECIFIED.,.F.,.F.,.F.)
B_SPLINE_SURFACE_WITH_KNOTS((6,1,1,1,1,1,1,1,1,1,1,1,1,1,1,1,1,1,1,1,1,
1,1,1,1,1,1,1,1,1,6),(2,2),(-1.,-0.966666666666667,-0.933333333333333,-0.9,
-0.866666666666667,-0.833333333333333,-0.8,-0.766666666666667,-0.733333333333333,
-0.7,-0.666666666666667,-0.633333333333333,-0.6,-0.566666666666667,-0.533333333333333,
-0.5,-0.466666666666667,-0.433333333333333,-0.4,-0.366666666666667,-0.333333333333333,
-0.3,-0.266666666666667,-0.233333333333333,-0.2,-0.166666666666667,-0.133333333333333,
-0.1,-0.0666666666666667,-0.0333333333333333,0.),(0.,0.5),.UNSPECIFIED.)
GEOMETRIC_REPRESENTATION_ITEM()
RATIONAL_B_SPLINE_SURFACE(((1.,1.),(1.,1.),(1.,1.),(1.,1.),(1.,1.),(1.,
1.),(1.,1.),(1.,1.),(1.,1.),(1.,1.),(1.,1.),(1.,1.),(1.,1.),(1.,1.),(1.,
1.),(1.,1.),(1.,1.),(1.,1.),(1.,1.),(1.,1.),(1.,1.),(1.,1.),(1.,1.),(1.,
1.),(1.,1.),(1.,1.),(1.,1.),(1.,1.),(1.,1.),(1.,1.),(1.,1.),(1.,1.),(1.,
1.),(1.,1.),(1.,1.)))
REPRESENTATION_ITEM('')
SURFACE()
);
#113=(
BOUNDED_SURFACE()
B_SPLINE_SURFACE(5,1,((#93330,#93331),(#93332,#93333),(#93334,#93335),(#93336,
#93337),(#93338,#93339),(#93340,#93341),(#93342,#93343),(#93344,#93345),
(#93346,#93347),(#93348,#93349),(#93350,#93351),(#93352,#93353),(#93354,
#93355),(#93356,#93357),(#93358,#93359),(#93360,#93361),(#93362,#93363),
(#93364,#93365),(#93366,#93367),(#93368,#93369),(#93370,#93371),(#93372,
#93373),(#93374,#93375),(#93376,#93377),(#93378,#93379),(#93380,#93381),
(#93382,#93383),(#93384,#93385),(#93386,#93387),(#93388,#93389),(#93390,
#93391),(#93392,#93393),(#93394,#93395),(#93396,#93397),(#93398,#93399)),
 .UNSPECIFIED.,.F.,.F.,.F.)
B_SPLINE_SURFACE_WITH_KNOTS((6,1,1,1,1,1,1,1,1,1,1,1,1,1,1,1,1,1,1,1,1,
1,1,1,1,1,1,1,1,1,6),(2,2),(0.,0.0333333333333333,0.0666666666666667,0.1,
0.133333333333333,0.166666666666667,0.2,0.233333333333333,0.266666666666667,
0.3,0.333333333333333,0.366666666666667,0.4,0.433333333333333,0.466666666666667,
0.5,0.533333333333333,0.566666666666667,0.6,0.633333333333333,0.666666666666667,
0.7,0.733333333333333,0.766666666666667,0.8,0.833333333333333,0.866666666666667,
0.9,0.933333333333333,0.966666666666667,1.),(0.,0.5),.UNSPECIFIED.)
GEOMETRIC_REPRESENTATION_ITEM()
RATIONAL_B_SPLINE_SURFACE(((1.,1.),(1.,1.),(1.,1.),(1.,1.),(1.,1.),(1.,
1.),(1.,1.),(1.,1.),(1.,1.),(1.,1.),(1.,1.),(1.,1.),(1.,1.),(1.,1.),(1.,
1.),(1.,1.),(1.,1.),(1.,1.),(1.,1.),(1.,1.),(1.,1.),(1.,1.),(1.,1.),(1.,
1.),(1.,1.),(1.,1.),(1.,1.),(1.,1.),(1.,1.),(1.,1.),(1.,1.),(1.,1.),(1.,
1.),(1.,1.),(1.,1.)))
REPRESENTATION_ITEM('')
SURFACE()
);
#114=(
BOUNDED_SURFACE()
B_SPLINE_SURFACE(5,1,((#93483,#93484),(#93485,#93486),(#93487,#93488),(#93489,
#93490),(#93491,#93492),(#93493,#93494),(#93495,#93496),(#93497,#93498),
(#93499,#93500),(#93501,#93502),(#93503,#93504),(#93505,#93506),(#93507,
#93508),(#93509,#93510),(#93511,#93512),(#93513,#93514),(#93515,#93516),
(#93517,#93518),(#93519,#93520),(#93521,#93522),(#93523,#93524),(#93525,
#93526),(#93527,#93528),(#93529,#93530),(#93531,#93532),(#93533,#93534),
(#93535,#93536),(#93537,#93538),(#93539,#93540),(#93541,#93542),(#93543,
#93544),(#93545,#93546),(#93547,#93548),(#93549,#93550),(#93551,#93552)),
 .UNSPECIFIED.,.F.,.F.,.F.)
B_SPLINE_SURFACE_WITH_KNOTS((6,1,1,1,1,1,1,1,1,1,1,1,1,1,1,1,1,1,1,1,1,
1,1,1,1,1,1,1,1,1,6),(2,2),(-1.,-0.966666666666667,-0.933333333333333,-0.9,
-0.866666666666667,-0.833333333333333,-0.8,-0.766666666666667,-0.733333333333333,
-0.7,-0.666666666666667,-0.633333333333333,-0.6,-0.566666666666667,-0.533333333333333,
-0.5,-0.466666666666667,-0.433333333333333,-0.4,-0.366666666666667,-0.333333333333333,
-0.3,-0.266666666666667,-0.233333333333333,-0.2,-0.166666666666667,-0.133333333333333,
-0.1,-0.0666666666666667,-0.0333333333333333,0.),(0.,0.5),.UNSPECIFIED.)
GEOMETRIC_REPRESENTATION_ITEM()
RATIONAL_B_SPLINE_SURFACE(((1.,1.),(1.,1.),(1.,1.),(1.,1.),(1.,1.),(1.,
1.),(1.,1.),(1.,1.),(1.,1.),(1.,1.),(1.,1.),(1.,1.),(1.,1.),(1.,1.),(1.,
1.),(1.,1.),(1.,1.),(1.,1.),(1.,1.),(1.,1.),(1.,1.),(1.,1.),(1.,1.),(1.,
1.),(1.,1.),(1.,1.),(1.,1.),(1.,1.),(1.,1.),(1.,1.),(1.,1.),(1.,1.),(1.,
1.),(1.,1.),(1.,1.)))
REPRESENTATION_ITEM('')
SURFACE()
);
#115=(
BOUNDED_SURFACE()
B_SPLINE_SURFACE(5,1,((#93632,#93633),(#93634,#93635),(#93636,#93637),(#93638,
#93639),(#93640,#93641),(#93642,#93643),(#93644,#93645),(#93646,#93647),
(#93648,#93649),(#93650,#93651),(#93652,#93653),(#93654,#93655),(#93656,
#93657),(#93658,#93659),(#93660,#93661),(#93662,#93663),(#93664,#93665),
(#93666,#93667),(#93668,#93669),(#93670,#93671),(#93672,#93673),(#93674,
#93675),(#93676,#93677),(#93678,#93679),(#93680,#93681),(#93682,#93683),
(#93684,#93685),(#93686,#93687),(#93688,#93689),(#93690,#93691),(#93692,
#93693),(#93694,#93695),(#93696,#93697),(#93698,#93699),(#93700,#93701)),
 .UNSPECIFIED.,.F.,.F.,.F.)
B_SPLINE_SURFACE_WITH_KNOTS((6,1,1,1,1,1,1,1,1,1,1,1,1,1,1,1,1,1,1,1,1,
1,1,1,1,1,1,1,1,1,6),(2,2),(0.,0.0333333333333333,0.0666666666666667,0.1,
0.133333333333333,0.166666666666667,0.2,0.233333333333333,0.266666666666667,
0.3,0.333333333333333,0.366666666666667,0.4,0.433333333333333,0.466666666666667,
0.5,0.533333333333333,0.566666666666667,0.6,0.633333333333333,0.666666666666667,
0.7,0.733333333333333,0.766666666666667,0.8,0.833333333333333,0.866666666666667,
0.9,0.933333333333333,0.966666666666667,1.),(0.,0.5),.UNSPECIFIED.)
GEOMETRIC_REPRESENTATION_ITEM()
RATIONAL_B_SPLINE_SURFACE(((1.,1.),(1.,1.),(1.,1.),(1.,1.),(1.,1.),(1.,
1.),(1.,1.),(1.,1.),(1.,1.),(1.,1.),(1.,1.),(1.,1.),(1.,1.),(1.,1.),(1.,
1.),(1.,1.),(1.,1.),(1.,1.),(1.,1.),(1.,1.),(1.,1.),(1.,1.),(1.,1.),(1.,
1.),(1.,1.),(1.,1.),(1.,1.),(1.,1.),(1.,1.),(1.,1.),(1.,1.),(1.,1.),(1.,
1.),(1.,1.),(1.,1.)))
REPRESENTATION_ITEM('')
SURFACE()
);
#116=(
BOUNDED_SURFACE()
B_SPLINE_SURFACE(5,1,((#93785,#93786),(#93787,#93788),(#93789,#93790),(#93791,
#93792),(#93793,#93794),(#93795,#93796),(#93797,#93798),(#93799,#93800),
(#93801,#93802),(#93803,#93804),(#93805,#93806),(#93807,#93808),(#93809,
#93810),(#93811,#93812),(#93813,#93814),(#93815,#93816),(#93817,#93818),
(#93819,#93820),(#93821,#93822),(#93823,#93824),(#93825,#93826),(#93827,
#93828),(#93829,#93830),(#93831,#93832),(#93833,#93834),(#93835,#93836),
(#93837,#93838),(#93839,#93840),(#93841,#93842),(#93843,#93844),(#93845,
#93846),(#93847,#93848),(#93849,#93850),(#93851,#93852),(#93853,#93854)),
 .UNSPECIFIED.,.F.,.F.,.F.)
B_SPLINE_SURFACE_WITH_KNOTS((6,1,1,1,1,1,1,1,1,1,1,1,1,1,1,1,1,1,1,1,1,
1,1,1,1,1,1,1,1,1,6),(2,2),(-1.,-0.966666666666667,-0.933333333333333,-0.9,
-0.866666666666667,-0.833333333333333,-0.8,-0.766666666666667,-0.733333333333333,
-0.7,-0.666666666666667,-0.633333333333333,-0.6,-0.566666666666667,-0.533333333333333,
-0.5,-0.466666666666667,-0.433333333333333,-0.4,-0.366666666666667,-0.333333333333333,
-0.3,-0.266666666666667,-0.233333333333333,-0.2,-0.166666666666667,-0.133333333333333,
-0.1,-0.0666666666666667,-0.0333333333333333,0.),(0.,0.5),.UNSPECIFIED.)
GEOMETRIC_REPRESENTATION_ITEM()
RATIONAL_B_SPLINE_SURFACE(((1.,1.),(1.,1.),(1.,1.),(1.,1.),(1.,1.),(1.,
1.),(1.,1.),(1.,1.),(1.,1.),(1.,1.),(1.,1.),(1.,1.),(1.,1.),(1.,1.),(1.,
1.),(1.,1.),(1.,1.),(1.,1.),(1.,1.),(1.,1.),(1.,1.),(1.,1.),(1.,1.),(1.,
1.),(1.,1.),(1.,1.),(1.,1.),(1.,1.),(1.,1.),(1.,1.),(1.,1.),(1.,1.),(1.,
1.),(1.,1.),(1.,1.)))
REPRESENTATION_ITEM('')
SURFACE()
);
#117=(
BOUNDED_SURFACE()
B_SPLINE_SURFACE(5,1,((#93934,#93935),(#93936,#93937),(#93938,#93939),(#93940,
#93941),(#93942,#93943),(#93944,#93945),(#93946,#93947),(#93948,#93949),
(#93950,#93951),(#93952,#93953),(#93954,#93955),(#93956,#93957),(#93958,
#93959),(#93960,#93961),(#93962,#93963),(#93964,#93965),(#93966,#93967),
(#93968,#93969),(#93970,#93971),(#93972,#93973),(#93974,#93975),(#93976,
#93977),(#93978,#93979),(#93980,#93981),(#93982,#93983),(#93984,#93985),
(#93986,#93987),(#93988,#93989),(#93990,#93991),(#93992,#93993),(#93994,
#93995),(#93996,#93997),(#93998,#93999),(#94000,#94001),(#94002,#94003)),
 .UNSPECIFIED.,.F.,.F.,.F.)
B_SPLINE_SURFACE_WITH_KNOTS((6,1,1,1,1,1,1,1,1,1,1,1,1,1,1,1,1,1,1,1,1,
1,1,1,1,1,1,1,1,1,6),(2,2),(0.,0.0333333333333333,0.0666666666666667,0.1,
0.133333333333333,0.166666666666667,0.2,0.233333333333333,0.266666666666667,
0.3,0.333333333333333,0.366666666666667,0.4,0.433333333333333,0.466666666666667,
0.5,0.533333333333333,0.566666666666667,0.6,0.633333333333333,0.666666666666667,
0.7,0.733333333333333,0.766666666666667,0.8,0.833333333333333,0.866666666666667,
0.9,0.933333333333333,0.966666666666667,1.),(0.,0.5),.UNSPECIFIED.)
GEOMETRIC_REPRESENTATION_ITEM()
RATIONAL_B_SPLINE_SURFACE(((1.,1.),(1.,1.),(1.,1.),(1.,1.),(1.,1.),(1.,
1.),(1.,1.),(1.,1.),(1.,1.),(1.,1.),(1.,1.),(1.,1.),(1.,1.),(1.,1.),(1.,
1.),(1.,1.),(1.,1.),(1.,1.),(1.,1.),(1.,1.),(1.,1.),(1.,1.),(1.,1.),(1.,
1.),(1.,1.),(1.,1.),(1.,1.),(1.,1.),(1.,1.),(1.,1.),(1.,1.),(1.,1.),(1.,
1.),(1.,1.),(1.,1.)))
REPRESENTATION_ITEM('')
SURFACE()
);
#118=(
BOUNDED_SURFACE()
B_SPLINE_SURFACE(5,1,((#94087,#94088),(#94089,#94090),(#94091,#94092),(#94093,
#94094),(#94095,#94096),(#94097,#94098),(#94099,#94100),(#94101,#94102),
(#94103,#94104),(#94105,#94106),(#94107,#94108),(#94109,#94110),(#94111,
#94112),(#94113,#94114),(#94115,#94116),(#94117,#94118),(#94119,#94120),
(#94121,#94122),(#94123,#94124),(#94125,#94126),(#94127,#94128),(#94129,
#94130),(#94131,#94132),(#94133,#94134),(#94135,#94136),(#94137,#94138),
(#94139,#94140),(#94141,#94142),(#94143,#94144),(#94145,#94146),(#94147,
#94148),(#94149,#94150),(#94151,#94152),(#94153,#94154),(#94155,#94156)),
 .UNSPECIFIED.,.F.,.F.,.F.)
B_SPLINE_SURFACE_WITH_KNOTS((6,1,1,1,1,1,1,1,1,1,1,1,1,1,1,1,1,1,1,1,1,
1,1,1,1,1,1,1,1,1,6),(2,2),(-1.,-0.966666666666667,-0.933333333333333,-0.9,
-0.866666666666667,-0.833333333333333,-0.8,-0.766666666666667,-0.733333333333333,
-0.7,-0.666666666666667,-0.633333333333333,-0.6,-0.566666666666667,-0.533333333333333,
-0.5,-0.466666666666667,-0.433333333333333,-0.4,-0.366666666666667,-0.333333333333333,
-0.3,-0.266666666666667,-0.233333333333333,-0.2,-0.166666666666667,-0.133333333333333,
-0.1,-0.0666666666666667,-0.0333333333333333,0.),(0.,0.5),.UNSPECIFIED.)
GEOMETRIC_REPRESENTATION_ITEM()
RATIONAL_B_SPLINE_SURFACE(((1.,1.),(1.,1.),(1.,1.),(1.,1.),(1.,1.),(1.,
1.),(1.,1.),(1.,1.),(1.,1.),(1.,1.),(1.,1.),(1.,1.),(1.,1.),(1.,1.),(1.,
1.),(1.,1.),(1.,1.),(1.,1.),(1.,1.),(1.,1.),(1.,1.),(1.,1.),(1.,1.),(1.,
1.),(1.,1.),(1.,1.),(1.,1.),(1.,1.),(1.,1.),(1.,1.),(1.,1.),(1.,1.),(1.,
1.),(1.,1.),(1.,1.)))
REPRESENTATION_ITEM('')
SURFACE()
);
#119=(
BOUNDED_SURFACE()
B_SPLINE_SURFACE(5,1,((#94236,#94237),(#94238,#94239),(#94240,#94241),(#94242,
#94243),(#94244,#94245),(#94246,#94247),(#94248,#94249),(#94250,#94251),
(#94252,#94253),(#94254,#94255),(#94256,#94257),(#94258,#94259),(#94260,
#94261),(#94262,#94263),(#94264,#94265),(#94266,#94267),(#94268,#94269),
(#94270,#94271),(#94272,#94273),(#94274,#94275),(#94276,#94277),(#94278,
#94279),(#94280,#94281),(#94282,#94283),(#94284,#94285),(#94286,#94287),
(#94288,#94289),(#94290,#94291),(#94292,#94293),(#94294,#94295),(#94296,
#94297),(#94298,#94299),(#94300,#94301),(#94302,#94303),(#94304,#94305)),
 .UNSPECIFIED.,.F.,.F.,.F.)
B_SPLINE_SURFACE_WITH_KNOTS((6,1,1,1,1,1,1,1,1,1,1,1,1,1,1,1,1,1,1,1,1,
1,1,1,1,1,1,1,1,1,6),(2,2),(0.,0.0333333333333333,0.0666666666666667,0.1,
0.133333333333333,0.166666666666667,0.2,0.233333333333333,0.266666666666667,
0.3,0.333333333333333,0.366666666666667,0.4,0.433333333333333,0.466666666666667,
0.5,0.533333333333333,0.566666666666667,0.6,0.633333333333333,0.666666666666667,
0.7,0.733333333333333,0.766666666666667,0.8,0.833333333333333,0.866666666666667,
0.9,0.933333333333333,0.966666666666667,1.),(0.,0.5),.UNSPECIFIED.)
GEOMETRIC_REPRESENTATION_ITEM()
RATIONAL_B_SPLINE_SURFACE(((1.,1.),(1.,1.),(1.,1.),(1.,1.),(1.,1.),(1.,
1.),(1.,1.),(1.,1.),(1.,1.),(1.,1.),(1.,1.),(1.,1.),(1.,1.),(1.,1.),(1.,
1.),(1.,1.),(1.,1.),(1.,1.),(1.,1.),(1.,1.),(1.,1.),(1.,1.),(1.,1.),(1.,
1.),(1.,1.),(1.,1.),(1.,1.),(1.,1.),(1.,1.),(1.,1.),(1.,1.),(1.,1.),(1.,
1.),(1.,1.),(1.,1.)))
REPRESENTATION_ITEM('')
SURFACE()
);
#120=(
BOUNDED_SURFACE()
B_SPLINE_SURFACE(5,1,((#94389,#94390),(#94391,#94392),(#94393,#94394),(#94395,
#94396),(#94397,#94398),(#94399,#94400),(#94401,#94402),(#94403,#94404),
(#94405,#94406),(#94407,#94408),(#94409,#94410),(#94411,#94412),(#94413,
#94414),(#94415,#94416),(#94417,#94418),(#94419,#94420),(#94421,#94422),
(#94423,#94424),(#94425,#94426),(#94427,#94428),(#94429,#94430),(#94431,
#94432),(#94433,#94434),(#94435,#94436),(#94437,#94438),(#94439,#94440),
(#94441,#94442),(#94443,#94444),(#94445,#94446),(#94447,#94448),(#94449,
#94450),(#94451,#94452),(#94453,#94454),(#94455,#94456),(#94457,#94458)),
 .UNSPECIFIED.,.F.,.F.,.F.)
B_SPLINE_SURFACE_WITH_KNOTS((6,1,1,1,1,1,1,1,1,1,1,1,1,1,1,1,1,1,1,1,1,
1,1,1,1,1,1,1,1,1,6),(2,2),(-1.,-0.966666666666667,-0.933333333333333,-0.9,
-0.866666666666667,-0.833333333333333,-0.8,-0.766666666666667,-0.733333333333333,
-0.7,-0.666666666666667,-0.633333333333333,-0.6,-0.566666666666667,-0.533333333333333,
-0.5,-0.466666666666667,-0.433333333333333,-0.4,-0.366666666666667,-0.333333333333333,
-0.3,-0.266666666666667,-0.233333333333333,-0.2,-0.166666666666667,-0.133333333333333,
-0.1,-0.0666666666666667,-0.0333333333333333,0.),(0.,0.5),.UNSPECIFIED.)
GEOMETRIC_REPRESENTATION_ITEM()
RATIONAL_B_SPLINE_SURFACE(((1.,1.),(1.,1.),(1.,1.),(1.,1.),(1.,1.),(1.,
1.),(1.,1.),(1.,1.),(1.,1.),(1.,1.),(1.,1.),(1.,1.),(1.,1.),(1.,1.),(1.,
1.),(1.,1.),(1.,1.),(1.,1.),(1.,1.),(1.,1.),(1.,1.),(1.,1.),(1.,1.),(1.,
1.),(1.,1.),(1.,1.),(1.,1.),(1.,1.),(1.,1.),(1.,1.),(1.,1.),(1.,1.),(1.,
1.),(1.,1.),(1.,1.)))
REPRESENTATION_ITEM('')
SURFACE()
);
#121=(
BOUNDED_SURFACE()
B_SPLINE_SURFACE(5,1,((#94538,#94539),(#94540,#94541),(#94542,#94543),(#94544,
#94545),(#94546,#94547),(#94548,#94549),(#94550,#94551),(#94552,#94553),
(#94554,#94555),(#94556,#94557),(#94558,#94559),(#94560,#94561),(#94562,
#94563),(#94564,#94565),(#94566,#94567),(#94568,#94569),(#94570,#94571),
(#94572,#94573),(#94574,#94575),(#94576,#94577),(#94578,#94579),(#94580,
#94581),(#94582,#94583),(#94584,#94585),(#94586,#94587),(#94588,#94589),
(#94590,#94591),(#94592,#94593),(#94594,#94595),(#94596,#94597),(#94598,
#94599),(#94600,#94601),(#94602,#94603),(#94604,#94605),(#94606,#94607)),
 .UNSPECIFIED.,.F.,.F.,.F.)
B_SPLINE_SURFACE_WITH_KNOTS((6,1,1,1,1,1,1,1,1,1,1,1,1,1,1,1,1,1,1,1,1,
1,1,1,1,1,1,1,1,1,6),(2,2),(0.,0.0333333333333333,0.0666666666666667,0.1,
0.133333333333333,0.166666666666667,0.2,0.233333333333333,0.266666666666667,
0.3,0.333333333333333,0.366666666666667,0.4,0.433333333333333,0.466666666666667,
0.5,0.533333333333333,0.566666666666667,0.6,0.633333333333333,0.666666666666667,
0.7,0.733333333333333,0.766666666666667,0.8,0.833333333333333,0.866666666666667,
0.9,0.933333333333333,0.966666666666667,1.),(0.,0.5),.UNSPECIFIED.)
GEOMETRIC_REPRESENTATION_ITEM()
RATIONAL_B_SPLINE_SURFACE(((1.,1.),(1.,1.),(1.,1.),(1.,1.),(1.,1.),(1.,
1.),(1.,1.),(1.,1.),(1.,1.),(1.,1.),(1.,1.),(1.,1.),(1.,1.),(1.,1.),(1.,
1.),(1.,1.),(1.,1.),(1.,1.),(1.,1.),(1.,1.),(1.,1.),(1.,1.),(1.,1.),(1.,
1.),(1.,1.),(1.,1.),(1.,1.),(1.,1.),(1.,1.),(1.,1.),(1.,1.),(1.,1.),(1.,
1.),(1.,1.),(1.,1.)))
REPRESENTATION_ITEM('')
SURFACE()
);
#122=(
BOUNDED_SURFACE()
B_SPLINE_SURFACE(5,1,((#94691,#94692),(#94693,#94694),(#94695,#94696),(#94697,
#94698),(#94699,#94700),(#94701,#94702),(#94703,#94704),(#94705,#94706),
(#94707,#94708),(#94709,#94710),(#94711,#94712),(#94713,#94714),(#94715,
#94716),(#94717,#94718),(#94719,#94720),(#94721,#94722),(#94723,#94724),
(#94725,#94726),(#94727,#94728),(#94729,#94730),(#94731,#94732),(#94733,
#94734),(#94735,#94736),(#94737,#94738),(#94739,#94740),(#94741,#94742),
(#94743,#94744),(#94745,#94746),(#94747,#94748),(#94749,#94750),(#94751,
#94752),(#94753,#94754),(#94755,#94756),(#94757,#94758),(#94759,#94760)),
 .UNSPECIFIED.,.F.,.F.,.F.)
B_SPLINE_SURFACE_WITH_KNOTS((6,1,1,1,1,1,1,1,1,1,1,1,1,1,1,1,1,1,1,1,1,
1,1,1,1,1,1,1,1,1,6),(2,2),(-1.,-0.966666666666667,-0.933333333333333,-0.9,
-0.866666666666667,-0.833333333333333,-0.8,-0.766666666666667,-0.733333333333333,
-0.7,-0.666666666666667,-0.633333333333333,-0.6,-0.566666666666667,-0.533333333333333,
-0.5,-0.466666666666667,-0.433333333333333,-0.4,-0.366666666666667,-0.333333333333333,
-0.3,-0.266666666666667,-0.233333333333333,-0.2,-0.166666666666667,-0.133333333333333,
-0.1,-0.0666666666666667,-0.0333333333333333,0.),(0.,0.5),.UNSPECIFIED.)
GEOMETRIC_REPRESENTATION_ITEM()
RATIONAL_B_SPLINE_SURFACE(((1.,1.),(1.,1.),(1.,1.),(1.,1.),(1.,1.),(1.,
1.),(1.,1.),(1.,1.),(1.,1.),(1.,1.),(1.,1.),(1.,1.),(1.,1.),(1.,1.),(1.,
1.),(1.,1.),(1.,1.),(1.,1.),(1.,1.),(1.,1.),(1.,1.),(1.,1.),(1.,1.),(1.,
1.),(1.,1.),(1.,1.),(1.,1.),(1.,1.),(1.,1.),(1.,1.),(1.,1.),(1.,1.),(1.,
1.),(1.,1.),(1.,1.)))
REPRESENTATION_ITEM('')
SURFACE()
);
#123=(
BOUNDED_SURFACE()
B_SPLINE_SURFACE(5,1,((#94840,#94841),(#94842,#94843),(#94844,#94845),(#94846,
#94847),(#94848,#94849),(#94850,#94851),(#94852,#94853),(#94854,#94855),
(#94856,#94857),(#94858,#94859),(#94860,#94861),(#94862,#94863),(#94864,
#94865),(#94866,#94867),(#94868,#94869),(#94870,#94871),(#94872,#94873),
(#94874,#94875),(#94876,#94877),(#94878,#94879),(#94880,#94881),(#94882,
#94883),(#94884,#94885),(#94886,#94887),(#94888,#94889),(#94890,#94891),
(#94892,#94893),(#94894,#94895),(#94896,#94897),(#94898,#94899),(#94900,
#94901),(#94902,#94903),(#94904,#94905),(#94906,#94907),(#94908,#94909)),
 .UNSPECIFIED.,.F.,.F.,.F.)
B_SPLINE_SURFACE_WITH_KNOTS((6,1,1,1,1,1,1,1,1,1,1,1,1,1,1,1,1,1,1,1,1,
1,1,1,1,1,1,1,1,1,6),(2,2),(0.,0.0333333333333333,0.0666666666666667,0.1,
0.133333333333333,0.166666666666667,0.2,0.233333333333333,0.266666666666667,
0.3,0.333333333333333,0.366666666666667,0.4,0.433333333333333,0.466666666666667,
0.5,0.533333333333333,0.566666666666667,0.6,0.633333333333333,0.666666666666667,
0.7,0.733333333333333,0.766666666666667,0.8,0.833333333333333,0.866666666666667,
0.9,0.933333333333333,0.966666666666667,1.),(0.,0.5),.UNSPECIFIED.)
GEOMETRIC_REPRESENTATION_ITEM()
RATIONAL_B_SPLINE_SURFACE(((1.,1.),(1.,1.),(1.,1.),(1.,1.),(1.,1.),(1.,
1.),(1.,1.),(1.,1.),(1.,1.),(1.,1.),(1.,1.),(1.,1.),(1.,1.),(1.,1.),(1.,
1.),(1.,1.),(1.,1.),(1.,1.),(1.,1.),(1.,1.),(1.,1.),(1.,1.),(1.,1.),(1.,
1.),(1.,1.),(1.,1.),(1.,1.),(1.,1.),(1.,1.),(1.,1.),(1.,1.),(1.,1.),(1.,
1.),(1.,1.),(1.,1.)))
REPRESENTATION_ITEM('')
SURFACE()
);
#124=(
BOUNDED_SURFACE()
B_SPLINE_SURFACE(5,1,((#94993,#94994),(#94995,#94996),(#94997,#94998),(#94999,
#95000),(#95001,#95002),(#95003,#95004),(#95005,#95006),(#95007,#95008),
(#95009,#95010),(#95011,#95012),(#95013,#95014),(#95015,#95016),(#95017,
#95018),(#95019,#95020),(#95021,#95022),(#95023,#95024),(#95025,#95026),
(#95027,#95028),(#95029,#95030),(#95031,#95032),(#95033,#95034),(#95035,
#95036),(#95037,#95038),(#95039,#95040),(#95041,#95042),(#95043,#95044),
(#95045,#95046),(#95047,#95048),(#95049,#95050),(#95051,#95052),(#95053,
#95054),(#95055,#95056),(#95057,#95058),(#95059,#95060),(#95061,#95062)),
 .UNSPECIFIED.,.F.,.F.,.F.)
B_SPLINE_SURFACE_WITH_KNOTS((6,1,1,1,1,1,1,1,1,1,1,1,1,1,1,1,1,1,1,1,1,
1,1,1,1,1,1,1,1,1,6),(2,2),(-1.,-0.966666666666667,-0.933333333333333,-0.9,
-0.866666666666667,-0.833333333333333,-0.8,-0.766666666666667,-0.733333333333333,
-0.7,-0.666666666666667,-0.633333333333333,-0.6,-0.566666666666667,-0.533333333333333,
-0.5,-0.466666666666667,-0.433333333333333,-0.4,-0.366666666666667,-0.333333333333333,
-0.3,-0.266666666666667,-0.233333333333333,-0.2,-0.166666666666667,-0.133333333333333,
-0.1,-0.0666666666666667,-0.0333333333333333,0.),(0.,0.5),.UNSPECIFIED.)
GEOMETRIC_REPRESENTATION_ITEM()
RATIONAL_B_SPLINE_SURFACE(((1.,1.),(1.,1.),(1.,1.),(1.,1.),(1.,1.),(1.,
1.),(1.,1.),(1.,1.),(1.,1.),(1.,1.),(1.,1.),(1.,1.),(1.,1.),(1.,1.),(1.,
1.),(1.,1.),(1.,1.),(1.,1.),(1.,1.),(1.,1.),(1.,1.),(1.,1.),(1.,1.),(1.,
1.),(1.,1.),(1.,1.),(1.,1.),(1.,1.),(1.,1.),(1.,1.),(1.,1.),(1.,1.),(1.,
1.),(1.,1.),(1.,1.)))
REPRESENTATION_ITEM('')
SURFACE()
);
#125=(
BOUNDED_SURFACE()
B_SPLINE_SURFACE(5,1,((#95142,#95143),(#95144,#95145),(#95146,#95147),(#95148,
#95149),(#95150,#95151),(#95152,#95153),(#95154,#95155),(#95156,#95157),
(#95158,#95159),(#95160,#95161),(#95162,#95163),(#95164,#95165),(#95166,
#95167),(#95168,#95169),(#95170,#95171),(#95172,#95173),(#95174,#95175),
(#95176,#95177),(#95178,#95179),(#95180,#95181),(#95182,#95183),(#95184,
#95185),(#95186,#95187),(#95188,#95189),(#95190,#95191),(#95192,#95193),
(#95194,#95195),(#95196,#95197),(#95198,#95199),(#95200,#95201),(#95202,
#95203),(#95204,#95205),(#95206,#95207),(#95208,#95209),(#95210,#95211)),
 .UNSPECIFIED.,.F.,.F.,.F.)
B_SPLINE_SURFACE_WITH_KNOTS((6,1,1,1,1,1,1,1,1,1,1,1,1,1,1,1,1,1,1,1,1,
1,1,1,1,1,1,1,1,1,6),(2,2),(0.,0.0333333333333333,0.0666666666666667,0.1,
0.133333333333333,0.166666666666667,0.2,0.233333333333333,0.266666666666667,
0.3,0.333333333333333,0.366666666666667,0.4,0.433333333333333,0.466666666666667,
0.5,0.533333333333333,0.566666666666667,0.6,0.633333333333333,0.666666666666667,
0.7,0.733333333333333,0.766666666666667,0.8,0.833333333333333,0.866666666666667,
0.9,0.933333333333333,0.966666666666667,1.),(0.,0.5),.UNSPECIFIED.)
GEOMETRIC_REPRESENTATION_ITEM()
RATIONAL_B_SPLINE_SURFACE(((1.,1.),(1.,1.),(1.,1.),(1.,1.),(1.,1.),(1.,
1.),(1.,1.),(1.,1.),(1.,1.),(1.,1.),(1.,1.),(1.,1.),(1.,1.),(1.,1.),(1.,
1.),(1.,1.),(1.,1.),(1.,1.),(1.,1.),(1.,1.),(1.,1.),(1.,1.),(1.,1.),(1.,
1.),(1.,1.),(1.,1.),(1.,1.),(1.,1.),(1.,1.),(1.,1.),(1.,1.),(1.,1.),(1.,
1.),(1.,1.),(1.,1.)))
REPRESENTATION_ITEM('')
SURFACE()
);
#126=(
BOUNDED_SURFACE()
B_SPLINE_SURFACE(5,1,((#95295,#95296),(#95297,#95298),(#95299,#95300),(#95301,
#95302),(#95303,#95304),(#95305,#95306),(#95307,#95308),(#95309,#95310),
(#95311,#95312),(#95313,#95314),(#95315,#95316),(#95317,#95318),(#95319,
#95320),(#95321,#95322),(#95323,#95324),(#95325,#95326),(#95327,#95328),
(#95329,#95330),(#95331,#95332),(#95333,#95334),(#95335,#95336),(#95337,
#95338),(#95339,#95340),(#95341,#95342),(#95343,#95344),(#95345,#95346),
(#95347,#95348),(#95349,#95350),(#95351,#95352),(#95353,#95354),(#95355,
#95356),(#95357,#95358),(#95359,#95360),(#95361,#95362),(#95363,#95364)),
 .UNSPECIFIED.,.F.,.F.,.F.)
B_SPLINE_SURFACE_WITH_KNOTS((6,1,1,1,1,1,1,1,1,1,1,1,1,1,1,1,1,1,1,1,1,
1,1,1,1,1,1,1,1,1,6),(2,2),(-1.,-0.966666666666667,-0.933333333333333,-0.9,
-0.866666666666667,-0.833333333333333,-0.8,-0.766666666666667,-0.733333333333333,
-0.7,-0.666666666666667,-0.633333333333333,-0.6,-0.566666666666667,-0.533333333333333,
-0.5,-0.466666666666667,-0.433333333333333,-0.4,-0.366666666666667,-0.333333333333333,
-0.3,-0.266666666666667,-0.233333333333333,-0.2,-0.166666666666667,-0.133333333333333,
-0.1,-0.0666666666666667,-0.0333333333333333,0.),(0.,0.5),.UNSPECIFIED.)
GEOMETRIC_REPRESENTATION_ITEM()
RATIONAL_B_SPLINE_SURFACE(((1.,1.),(1.,1.),(1.,1.),(1.,1.),(1.,1.),(1.,
1.),(1.,1.),(1.,1.),(1.,1.),(1.,1.),(1.,1.),(1.,1.),(1.,1.),(1.,1.),(1.,
1.),(1.,1.),(1.,1.),(1.,1.),(1.,1.),(1.,1.),(1.,1.),(1.,1.),(1.,1.),(1.,
1.),(1.,1.),(1.,1.),(1.,1.),(1.,1.),(1.,1.),(1.,1.),(1.,1.),(1.,1.),(1.,
1.),(1.,1.),(1.,1.)))
REPRESENTATION_ITEM('')
SURFACE()
);
#127=(
BOUNDED_SURFACE()
B_SPLINE_SURFACE(5,1,((#95444,#95445),(#95446,#95447),(#95448,#95449),(#95450,
#95451),(#95452,#95453),(#95454,#95455),(#95456,#95457),(#95458,#95459),
(#95460,#95461),(#95462,#95463),(#95464,#95465),(#95466,#95467),(#95468,
#95469),(#95470,#95471),(#95472,#95473),(#95474,#95475),(#95476,#95477),
(#95478,#95479),(#95480,#95481),(#95482,#95483),(#95484,#95485),(#95486,
#95487),(#95488,#95489),(#95490,#95491),(#95492,#95493),(#95494,#95495),
(#95496,#95497),(#95498,#95499),(#95500,#95501),(#95502,#95503),(#95504,
#95505),(#95506,#95507),(#95508,#95509),(#95510,#95511),(#95512,#95513)),
 .UNSPECIFIED.,.F.,.F.,.F.)
B_SPLINE_SURFACE_WITH_KNOTS((6,1,1,1,1,1,1,1,1,1,1,1,1,1,1,1,1,1,1,1,1,
1,1,1,1,1,1,1,1,1,6),(2,2),(0.,0.0333333333333333,0.0666666666666667,0.1,
0.133333333333333,0.166666666666667,0.2,0.233333333333333,0.266666666666667,
0.3,0.333333333333333,0.366666666666667,0.4,0.433333333333333,0.466666666666667,
0.5,0.533333333333333,0.566666666666667,0.6,0.633333333333333,0.666666666666667,
0.7,0.733333333333333,0.766666666666667,0.8,0.833333333333333,0.866666666666667,
0.9,0.933333333333333,0.966666666666667,1.),(0.,0.5),.UNSPECIFIED.)
GEOMETRIC_REPRESENTATION_ITEM()
RATIONAL_B_SPLINE_SURFACE(((1.,1.),(1.,1.),(1.,1.),(1.,1.),(1.,1.),(1.,
1.),(1.,1.),(1.,1.),(1.,1.),(1.,1.),(1.,1.),(1.,1.),(1.,1.),(1.,1.),(1.,
1.),(1.,1.),(1.,1.),(1.,1.),(1.,1.),(1.,1.),(1.,1.),(1.,1.),(1.,1.),(1.,
1.),(1.,1.),(1.,1.),(1.,1.),(1.,1.),(1.,1.),(1.,1.),(1.,1.),(1.,1.),(1.,
1.),(1.,1.),(1.,1.)))
REPRESENTATION_ITEM('')
SURFACE()
);
#128=(
BOUNDED_SURFACE()
B_SPLINE_SURFACE(5,1,((#95597,#95598),(#95599,#95600),(#95601,#95602),(#95603,
#95604),(#95605,#95606),(#95607,#95608),(#95609,#95610),(#95611,#95612),
(#95613,#95614),(#95615,#95616),(#95617,#95618),(#95619,#95620),(#95621,
#95622),(#95623,#95624),(#95625,#95626),(#95627,#95628),(#95629,#95630),
(#95631,#95632),(#95633,#95634),(#95635,#95636),(#95637,#95638),(#95639,
#95640),(#95641,#95642),(#95643,#95644),(#95645,#95646),(#95647,#95648),
(#95649,#95650),(#95651,#95652),(#95653,#95654),(#95655,#95656),(#95657,
#95658),(#95659,#95660),(#95661,#95662),(#95663,#95664),(#95665,#95666)),
 .UNSPECIFIED.,.F.,.F.,.F.)
B_SPLINE_SURFACE_WITH_KNOTS((6,1,1,1,1,1,1,1,1,1,1,1,1,1,1,1,1,1,1,1,1,
1,1,1,1,1,1,1,1,1,6),(2,2),(-1.,-0.966666666666667,-0.933333333333333,-0.9,
-0.866666666666667,-0.833333333333333,-0.8,-0.766666666666667,-0.733333333333333,
-0.7,-0.666666666666667,-0.633333333333333,-0.6,-0.566666666666667,-0.533333333333333,
-0.5,-0.466666666666667,-0.433333333333333,-0.4,-0.366666666666667,-0.333333333333333,
-0.3,-0.266666666666667,-0.233333333333333,-0.2,-0.166666666666667,-0.133333333333333,
-0.1,-0.0666666666666667,-0.0333333333333333,0.),(0.,0.5),.UNSPECIFIED.)
GEOMETRIC_REPRESENTATION_ITEM()
RATIONAL_B_SPLINE_SURFACE(((1.,1.),(1.,1.),(1.,1.),(1.,1.),(1.,1.),(1.,
1.),(1.,1.),(1.,1.),(1.,1.),(1.,1.),(1.,1.),(1.,1.),(1.,1.),(1.,1.),(1.,
1.),(1.,1.),(1.,1.),(1.,1.),(1.,1.),(1.,1.),(1.,1.),(1.,1.),(1.,1.),(1.,
1.),(1.,1.),(1.,1.),(1.,1.),(1.,1.),(1.,1.),(1.,1.),(1.,1.),(1.,1.),(1.,
1.),(1.,1.),(1.,1.)))
REPRESENTATION_ITEM('')
SURFACE()
);
#129=(
BOUNDED_SURFACE()
B_SPLINE_SURFACE(5,1,((#95746,#95747),(#95748,#95749),(#95750,#95751),(#95752,
#95753),(#95754,#95755),(#95756,#95757),(#95758,#95759),(#95760,#95761),
(#95762,#95763),(#95764,#95765),(#95766,#95767),(#95768,#95769),(#95770,
#95771),(#95772,#95773),(#95774,#95775),(#95776,#95777),(#95778,#95779),
(#95780,#95781),(#95782,#95783),(#95784,#95785),(#95786,#95787),(#95788,
#95789),(#95790,#95791),(#95792,#95793),(#95794,#95795),(#95796,#95797),
(#95798,#95799),(#95800,#95801),(#95802,#95803),(#95804,#95805),(#95806,
#95807),(#95808,#95809),(#95810,#95811),(#95812,#95813),(#95814,#95815)),
 .UNSPECIFIED.,.F.,.F.,.F.)
B_SPLINE_SURFACE_WITH_KNOTS((6,1,1,1,1,1,1,1,1,1,1,1,1,1,1,1,1,1,1,1,1,
1,1,1,1,1,1,1,1,1,6),(2,2),(0.,0.0333333333333333,0.0666666666666667,0.1,
0.133333333333333,0.166666666666667,0.2,0.233333333333333,0.266666666666667,
0.3,0.333333333333333,0.366666666666667,0.4,0.433333333333333,0.466666666666667,
0.5,0.533333333333333,0.566666666666667,0.6,0.633333333333333,0.666666666666667,
0.7,0.733333333333333,0.766666666666667,0.8,0.833333333333333,0.866666666666667,
0.9,0.933333333333333,0.966666666666667,1.),(0.,0.5),.UNSPECIFIED.)
GEOMETRIC_REPRESENTATION_ITEM()
RATIONAL_B_SPLINE_SURFACE(((1.,1.),(1.,1.),(1.,1.),(1.,1.),(1.,1.),(1.,
1.),(1.,1.),(1.,1.),(1.,1.),(1.,1.),(1.,1.),(1.,1.),(1.,1.),(1.,1.),(1.,
1.),(1.,1.),(1.,1.),(1.,1.),(1.,1.),(1.,1.),(1.,1.),(1.,1.),(1.,1.),(1.,
1.),(1.,1.),(1.,1.),(1.,1.),(1.,1.),(1.,1.),(1.,1.),(1.,1.),(1.,1.),(1.,
1.),(1.,1.),(1.,1.)))
REPRESENTATION_ITEM('')
SURFACE()
);
#130=(
BOUNDED_SURFACE()
B_SPLINE_SURFACE(5,1,((#95899,#95900),(#95901,#95902),(#95903,#95904),(#95905,
#95906),(#95907,#95908),(#95909,#95910),(#95911,#95912),(#95913,#95914),
(#95915,#95916),(#95917,#95918),(#95919,#95920),(#95921,#95922),(#95923,
#95924),(#95925,#95926),(#95927,#95928),(#95929,#95930),(#95931,#95932),
(#95933,#95934),(#95935,#95936),(#95937,#95938),(#95939,#95940),(#95941,
#95942),(#95943,#95944),(#95945,#95946),(#95947,#95948),(#95949,#95950),
(#95951,#95952),(#95953,#95954),(#95955,#95956),(#95957,#95958),(#95959,
#95960),(#95961,#95962),(#95963,#95964),(#95965,#95966),(#95967,#95968)),
 .UNSPECIFIED.,.F.,.F.,.F.)
B_SPLINE_SURFACE_WITH_KNOTS((6,1,1,1,1,1,1,1,1,1,1,1,1,1,1,1,1,1,1,1,1,
1,1,1,1,1,1,1,1,1,6),(2,2),(-1.,-0.966666666666667,-0.933333333333333,-0.9,
-0.866666666666667,-0.833333333333333,-0.8,-0.766666666666667,-0.733333333333333,
-0.7,-0.666666666666667,-0.633333333333333,-0.6,-0.566666666666667,-0.533333333333333,
-0.5,-0.466666666666667,-0.433333333333333,-0.4,-0.366666666666667,-0.333333333333333,
-0.3,-0.266666666666667,-0.233333333333333,-0.2,-0.166666666666667,-0.133333333333333,
-0.1,-0.0666666666666667,-0.0333333333333333,0.),(0.,0.5),.UNSPECIFIED.)
GEOMETRIC_REPRESENTATION_ITEM()
RATIONAL_B_SPLINE_SURFACE(((1.,1.),(1.,1.),(1.,1.),(1.,1.),(1.,1.),(1.,
1.),(1.,1.),(1.,1.),(1.,1.),(1.,1.),(1.,1.),(1.,1.),(1.,1.),(1.,1.),(1.,
1.),(1.,1.),(1.,1.),(1.,1.),(1.,1.),(1.,1.),(1.,1.),(1.,1.),(1.,1.),(1.,
1.),(1.,1.),(1.,1.),(1.,1.),(1.,1.),(1.,1.),(1.,1.),(1.,1.),(1.,1.),(1.,
1.),(1.,1.),(1.,1.)))
REPRESENTATION_ITEM('')
SURFACE()
);
#131=(
BOUNDED_SURFACE()
B_SPLINE_SURFACE(5,1,((#96048,#96049),(#96050,#96051),(#96052,#96053),(#96054,
#96055),(#96056,#96057),(#96058,#96059),(#96060,#96061),(#96062,#96063),
(#96064,#96065),(#96066,#96067),(#96068,#96069),(#96070,#96071),(#96072,
#96073),(#96074,#96075),(#96076,#96077),(#96078,#96079),(#96080,#96081),
(#96082,#96083),(#96084,#96085),(#96086,#96087),(#96088,#96089),(#96090,
#96091),(#96092,#96093),(#96094,#96095),(#96096,#96097),(#96098,#96099),
(#96100,#96101),(#96102,#96103),(#96104,#96105),(#96106,#96107),(#96108,
#96109),(#96110,#96111),(#96112,#96113),(#96114,#96115),(#96116,#96117)),
 .UNSPECIFIED.,.F.,.F.,.F.)
B_SPLINE_SURFACE_WITH_KNOTS((6,1,1,1,1,1,1,1,1,1,1,1,1,1,1,1,1,1,1,1,1,
1,1,1,1,1,1,1,1,1,6),(2,2),(0.,0.0333333333333333,0.0666666666666667,0.1,
0.133333333333333,0.166666666666667,0.2,0.233333333333333,0.266666666666667,
0.3,0.333333333333333,0.366666666666667,0.4,0.433333333333333,0.466666666666667,
0.5,0.533333333333333,0.566666666666667,0.6,0.633333333333333,0.666666666666667,
0.7,0.733333333333333,0.766666666666667,0.8,0.833333333333333,0.866666666666667,
0.9,0.933333333333333,0.966666666666667,1.),(0.,0.5),.UNSPECIFIED.)
GEOMETRIC_REPRESENTATION_ITEM()
RATIONAL_B_SPLINE_SURFACE(((1.,1.),(1.,1.),(1.,1.),(1.,1.),(1.,1.),(1.,
1.),(1.,1.),(1.,1.),(1.,1.),(1.,1.),(1.,1.),(1.,1.),(1.,1.),(1.,1.),(1.,
1.),(1.,1.),(1.,1.),(1.,1.),(1.,1.),(1.,1.),(1.,1.),(1.,1.),(1.,1.),(1.,
1.),(1.,1.),(1.,1.),(1.,1.),(1.,1.),(1.,1.),(1.,1.),(1.,1.),(1.,1.),(1.,
1.),(1.,1.),(1.,1.)))
REPRESENTATION_ITEM('')
SURFACE()
);
#132=(
BOUNDED_SURFACE()
B_SPLINE_SURFACE(5,1,((#96201,#96202),(#96203,#96204),(#96205,#96206),(#96207,
#96208),(#96209,#96210),(#96211,#96212),(#96213,#96214),(#96215,#96216),
(#96217,#96218),(#96219,#96220),(#96221,#96222),(#96223,#96224),(#96225,
#96226),(#96227,#96228),(#96229,#96230),(#96231,#96232),(#96233,#96234),
(#96235,#96236),(#96237,#96238),(#96239,#96240),(#96241,#96242),(#96243,
#96244),(#96245,#96246),(#96247,#96248),(#96249,#96250),(#96251,#96252),
(#96253,#96254),(#96255,#96256),(#96257,#96258),(#96259,#96260),(#96261,
#96262),(#96263,#96264),(#96265,#96266),(#96267,#96268),(#96269,#96270)),
 .UNSPECIFIED.,.F.,.F.,.F.)
B_SPLINE_SURFACE_WITH_KNOTS((6,1,1,1,1,1,1,1,1,1,1,1,1,1,1,1,1,1,1,1,1,
1,1,1,1,1,1,1,1,1,6),(2,2),(-1.,-0.966666666666667,-0.933333333333333,-0.9,
-0.866666666666667,-0.833333333333333,-0.8,-0.766666666666667,-0.733333333333333,
-0.7,-0.666666666666667,-0.633333333333333,-0.6,-0.566666666666667,-0.533333333333333,
-0.5,-0.466666666666667,-0.433333333333333,-0.4,-0.366666666666667,-0.333333333333333,
-0.3,-0.266666666666667,-0.233333333333333,-0.2,-0.166666666666667,-0.133333333333333,
-0.1,-0.0666666666666667,-0.0333333333333333,0.),(0.,0.5),.UNSPECIFIED.)
GEOMETRIC_REPRESENTATION_ITEM()
RATIONAL_B_SPLINE_SURFACE(((1.,1.),(1.,1.),(1.,1.),(1.,1.),(1.,1.),(1.,
1.),(1.,1.),(1.,1.),(1.,1.),(1.,1.),(1.,1.),(1.,1.),(1.,1.),(1.,1.),(1.,
1.),(1.,1.),(1.,1.),(1.,1.),(1.,1.),(1.,1.),(1.,1.),(1.,1.),(1.,1.),(1.,
1.),(1.,1.),(1.,1.),(1.,1.),(1.,1.),(1.,1.),(1.,1.),(1.,1.),(1.,1.),(1.,
1.),(1.,1.),(1.,1.)))
REPRESENTATION_ITEM('')
SURFACE()
);
#133=(
BOUNDED_SURFACE()
B_SPLINE_SURFACE(5,1,((#96350,#96351),(#96352,#96353),(#96354,#96355),(#96356,
#96357),(#96358,#96359),(#96360,#96361),(#96362,#96363),(#96364,#96365),
(#96366,#96367),(#96368,#96369),(#96370,#96371),(#96372,#96373),(#96374,
#96375),(#96376,#96377),(#96378,#96379),(#96380,#96381),(#96382,#96383),
(#96384,#96385),(#96386,#96387),(#96388,#96389),(#96390,#96391),(#96392,
#96393),(#96394,#96395),(#96396,#96397),(#96398,#96399),(#96400,#96401),
(#96402,#96403),(#96404,#96405),(#96406,#96407),(#96408,#96409),(#96410,
#96411),(#96412,#96413),(#96414,#96415),(#96416,#96417),(#96418,#96419)),
 .UNSPECIFIED.,.F.,.F.,.F.)
B_SPLINE_SURFACE_WITH_KNOTS((6,1,1,1,1,1,1,1,1,1,1,1,1,1,1,1,1,1,1,1,1,
1,1,1,1,1,1,1,1,1,6),(2,2),(0.,0.0333333333333333,0.0666666666666667,0.1,
0.133333333333333,0.166666666666667,0.2,0.233333333333333,0.266666666666667,
0.3,0.333333333333333,0.366666666666667,0.4,0.433333333333333,0.466666666666667,
0.5,0.533333333333333,0.566666666666667,0.6,0.633333333333333,0.666666666666667,
0.7,0.733333333333333,0.766666666666667,0.8,0.833333333333333,0.866666666666667,
0.9,0.933333333333333,0.966666666666667,1.),(0.,0.5),.UNSPECIFIED.)
GEOMETRIC_REPRESENTATION_ITEM()
RATIONAL_B_SPLINE_SURFACE(((1.,1.),(1.,1.),(1.,1.),(1.,1.),(1.,1.),(1.,
1.),(1.,1.),(1.,1.),(1.,1.),(1.,1.),(1.,1.),(1.,1.),(1.,1.),(1.,1.),(1.,
1.),(1.,1.),(1.,1.),(1.,1.),(1.,1.),(1.,1.),(1.,1.),(1.,1.),(1.,1.),(1.,
1.),(1.,1.),(1.,1.),(1.,1.),(1.,1.),(1.,1.),(1.,1.),(1.,1.),(1.,1.),(1.,
1.),(1.,1.),(1.,1.)))
REPRESENTATION_ITEM('')
SURFACE()
);
#134=(
BOUNDED_SURFACE()
B_SPLINE_SURFACE(5,1,((#96503,#96504),(#96505,#96506),(#96507,#96508),(#96509,
#96510),(#96511,#96512),(#96513,#96514),(#96515,#96516),(#96517,#96518),
(#96519,#96520),(#96521,#96522),(#96523,#96524),(#96525,#96526),(#96527,
#96528),(#96529,#96530),(#96531,#96532),(#96533,#96534),(#96535,#96536),
(#96537,#96538),(#96539,#96540),(#96541,#96542),(#96543,#96544),(#96545,
#96546),(#96547,#96548),(#96549,#96550),(#96551,#96552),(#96553,#96554),
(#96555,#96556),(#96557,#96558),(#96559,#96560),(#96561,#96562),(#96563,
#96564),(#96565,#96566),(#96567,#96568),(#96569,#96570),(#96571,#96572)),
 .UNSPECIFIED.,.F.,.F.,.F.)
B_SPLINE_SURFACE_WITH_KNOTS((6,1,1,1,1,1,1,1,1,1,1,1,1,1,1,1,1,1,1,1,1,
1,1,1,1,1,1,1,1,1,6),(2,2),(-1.,-0.966666666666667,-0.933333333333333,-0.9,
-0.866666666666667,-0.833333333333333,-0.8,-0.766666666666667,-0.733333333333333,
-0.7,-0.666666666666667,-0.633333333333333,-0.6,-0.566666666666667,-0.533333333333333,
-0.5,-0.466666666666667,-0.433333333333333,-0.4,-0.366666666666667,-0.333333333333333,
-0.3,-0.266666666666667,-0.233333333333333,-0.2,-0.166666666666667,-0.133333333333333,
-0.1,-0.0666666666666667,-0.0333333333333333,0.),(0.,0.5),.UNSPECIFIED.)
GEOMETRIC_REPRESENTATION_ITEM()
RATIONAL_B_SPLINE_SURFACE(((1.,1.),(1.,1.),(1.,1.),(1.,1.),(1.,1.),(1.,
1.),(1.,1.),(1.,1.),(1.,1.),(1.,1.),(1.,1.),(1.,1.),(1.,1.),(1.,1.),(1.,
1.),(1.,1.),(1.,1.),(1.,1.),(1.,1.),(1.,1.),(1.,1.),(1.,1.),(1.,1.),(1.,
1.),(1.,1.),(1.,1.),(1.,1.),(1.,1.),(1.,1.),(1.,1.),(1.,1.),(1.,1.),(1.,
1.),(1.,1.),(1.,1.)))
REPRESENTATION_ITEM('')
SURFACE()
);
#135=(
BOUNDED_SURFACE()
B_SPLINE_SURFACE(5,1,((#96652,#96653),(#96654,#96655),(#96656,#96657),(#96658,
#96659),(#96660,#96661),(#96662,#96663),(#96664,#96665),(#96666,#96667),
(#96668,#96669),(#96670,#96671),(#96672,#96673),(#96674,#96675),(#96676,
#96677),(#96678,#96679),(#96680,#96681),(#96682,#96683),(#96684,#96685),
(#96686,#96687),(#96688,#96689),(#96690,#96691),(#96692,#96693),(#96694,
#96695),(#96696,#96697),(#96698,#96699),(#96700,#96701),(#96702,#96703),
(#96704,#96705),(#96706,#96707),(#96708,#96709),(#96710,#96711),(#96712,
#96713),(#96714,#96715),(#96716,#96717),(#96718,#96719),(#96720,#96721)),
 .UNSPECIFIED.,.F.,.F.,.F.)
B_SPLINE_SURFACE_WITH_KNOTS((6,1,1,1,1,1,1,1,1,1,1,1,1,1,1,1,1,1,1,1,1,
1,1,1,1,1,1,1,1,1,6),(2,2),(0.,0.0333333333333333,0.0666666666666667,0.1,
0.133333333333333,0.166666666666667,0.2,0.233333333333333,0.266666666666667,
0.3,0.333333333333333,0.366666666666667,0.4,0.433333333333333,0.466666666666667,
0.5,0.533333333333333,0.566666666666667,0.6,0.633333333333333,0.666666666666667,
0.7,0.733333333333333,0.766666666666667,0.8,0.833333333333333,0.866666666666667,
0.9,0.933333333333333,0.966666666666667,1.),(0.,0.5),.UNSPECIFIED.)
GEOMETRIC_REPRESENTATION_ITEM()
RATIONAL_B_SPLINE_SURFACE(((1.,1.),(1.,1.),(1.,1.),(1.,1.),(1.,1.),(1.,
1.),(1.,1.),(1.,1.),(1.,1.),(1.,1.),(1.,1.),(1.,1.),(1.,1.),(1.,1.),(1.,
1.),(1.,1.),(1.,1.),(1.,1.),(1.,1.),(1.,1.),(1.,1.),(1.,1.),(1.,1.),(1.,
1.),(1.,1.),(1.,1.),(1.,1.),(1.,1.),(1.,1.),(1.,1.),(1.,1.),(1.,1.),(1.,
1.),(1.,1.),(1.,1.)))
REPRESENTATION_ITEM('')
SURFACE()
);
#136=(
BOUNDED_SURFACE()
B_SPLINE_SURFACE(5,1,((#96805,#96806),(#96807,#96808),(#96809,#96810),(#96811,
#96812),(#96813,#96814),(#96815,#96816),(#96817,#96818),(#96819,#96820),
(#96821,#96822),(#96823,#96824),(#96825,#96826),(#96827,#96828),(#96829,
#96830),(#96831,#96832),(#96833,#96834),(#96835,#96836),(#96837,#96838),
(#96839,#96840),(#96841,#96842),(#96843,#96844),(#96845,#96846),(#96847,
#96848),(#96849,#96850),(#96851,#96852),(#96853,#96854),(#96855,#96856),
(#96857,#96858),(#96859,#96860),(#96861,#96862),(#96863,#96864),(#96865,
#96866),(#96867,#96868),(#96869,#96870),(#96871,#96872),(#96873,#96874)),
 .UNSPECIFIED.,.F.,.F.,.F.)
B_SPLINE_SURFACE_WITH_KNOTS((6,1,1,1,1,1,1,1,1,1,1,1,1,1,1,1,1,1,1,1,1,
1,1,1,1,1,1,1,1,1,6),(2,2),(-1.,-0.966666666666667,-0.933333333333333,-0.9,
-0.866666666666667,-0.833333333333333,-0.8,-0.766666666666667,-0.733333333333333,
-0.7,-0.666666666666667,-0.633333333333333,-0.6,-0.566666666666667,-0.533333333333333,
-0.5,-0.466666666666667,-0.433333333333333,-0.4,-0.366666666666667,-0.333333333333333,
-0.3,-0.266666666666667,-0.233333333333333,-0.2,-0.166666666666667,-0.133333333333333,
-0.1,-0.0666666666666667,-0.0333333333333333,0.),(0.,0.5),.UNSPECIFIED.)
GEOMETRIC_REPRESENTATION_ITEM()
RATIONAL_B_SPLINE_SURFACE(((1.,1.),(1.,1.),(1.,1.),(1.,1.),(1.,1.),(1.,
1.),(1.,1.),(1.,1.),(1.,1.),(1.,1.),(1.,1.),(1.,1.),(1.,1.),(1.,1.),(1.,
1.),(1.,1.),(1.,1.),(1.,1.),(1.,1.),(1.,1.),(1.,1.),(1.,1.),(1.,1.),(1.,
1.),(1.,1.),(1.,1.),(1.,1.),(1.,1.),(1.,1.),(1.,1.),(1.,1.),(1.,1.),(1.,
1.),(1.,1.),(1.,1.)))
REPRESENTATION_ITEM('')
SURFACE()
);
#137=(
BOUNDED_SURFACE()
B_SPLINE_SURFACE(5,1,((#96954,#96955),(#96956,#96957),(#96958,#96959),(#96960,
#96961),(#96962,#96963),(#96964,#96965),(#96966,#96967),(#96968,#96969),
(#96970,#96971),(#96972,#96973),(#96974,#96975),(#96976,#96977),(#96978,
#96979),(#96980,#96981),(#96982,#96983),(#96984,#96985),(#96986,#96987),
(#96988,#96989),(#96990,#96991),(#96992,#96993),(#96994,#96995),(#96996,
#96997),(#96998,#96999),(#97000,#97001),(#97002,#97003),(#97004,#97005),
(#97006,#97007),(#97008,#97009),(#97010,#97011),(#97012,#97013),(#97014,
#97015),(#97016,#97017),(#97018,#97019),(#97020,#97021),(#97022,#97023)),
 .UNSPECIFIED.,.F.,.F.,.F.)
B_SPLINE_SURFACE_WITH_KNOTS((6,1,1,1,1,1,1,1,1,1,1,1,1,1,1,1,1,1,1,1,1,
1,1,1,1,1,1,1,1,1,6),(2,2),(0.,0.0333333333333333,0.0666666666666667,0.1,
0.133333333333333,0.166666666666667,0.2,0.233333333333333,0.266666666666667,
0.3,0.333333333333333,0.366666666666667,0.4,0.433333333333333,0.466666666666667,
0.5,0.533333333333333,0.566666666666667,0.6,0.633333333333333,0.666666666666667,
0.7,0.733333333333333,0.766666666666667,0.8,0.833333333333333,0.866666666666667,
0.9,0.933333333333333,0.966666666666667,1.),(0.,0.5),.UNSPECIFIED.)
GEOMETRIC_REPRESENTATION_ITEM()
RATIONAL_B_SPLINE_SURFACE(((1.,1.),(1.,1.),(1.,1.),(1.,1.),(1.,1.),(1.,
1.),(1.,1.),(1.,1.),(1.,1.),(1.,1.),(1.,1.),(1.,1.),(1.,1.),(1.,1.),(1.,
1.),(1.,1.),(1.,1.),(1.,1.),(1.,1.),(1.,1.),(1.,1.),(1.,1.),(1.,1.),(1.,
1.),(1.,1.),(1.,1.),(1.,1.),(1.,1.),(1.,1.),(1.,1.),(1.,1.),(1.,1.),(1.,
1.),(1.,1.),(1.,1.)))
REPRESENTATION_ITEM('')
SURFACE()
);
#138=(
BOUNDED_SURFACE()
B_SPLINE_SURFACE(5,1,((#97107,#97108),(#97109,#97110),(#97111,#97112),(#97113,
#97114),(#97115,#97116),(#97117,#97118),(#97119,#97120),(#97121,#97122),
(#97123,#97124),(#97125,#97126),(#97127,#97128),(#97129,#97130),(#97131,
#97132),(#97133,#97134),(#97135,#97136),(#97137,#97138),(#97139,#97140),
(#97141,#97142),(#97143,#97144),(#97145,#97146),(#97147,#97148),(#97149,
#97150),(#97151,#97152),(#97153,#97154),(#97155,#97156),(#97157,#97158),
(#97159,#97160),(#97161,#97162),(#97163,#97164),(#97165,#97166),(#97167,
#97168),(#97169,#97170),(#97171,#97172),(#97173,#97174),(#97175,#97176)),
 .UNSPECIFIED.,.F.,.F.,.F.)
B_SPLINE_SURFACE_WITH_KNOTS((6,1,1,1,1,1,1,1,1,1,1,1,1,1,1,1,1,1,1,1,1,
1,1,1,1,1,1,1,1,1,6),(2,2),(-1.,-0.966666666666667,-0.933333333333333,-0.9,
-0.866666666666667,-0.833333333333333,-0.8,-0.766666666666667,-0.733333333333333,
-0.7,-0.666666666666667,-0.633333333333333,-0.6,-0.566666666666667,-0.533333333333333,
-0.5,-0.466666666666667,-0.433333333333333,-0.4,-0.366666666666667,-0.333333333333333,
-0.3,-0.266666666666667,-0.233333333333333,-0.2,-0.166666666666667,-0.133333333333333,
-0.1,-0.0666666666666667,-0.0333333333333333,0.),(0.,0.5),.UNSPECIFIED.)
GEOMETRIC_REPRESENTATION_ITEM()
RATIONAL_B_SPLINE_SURFACE(((1.,1.),(1.,1.),(1.,1.),(1.,1.),(1.,1.),(1.,
1.),(1.,1.),(1.,1.),(1.,1.),(1.,1.),(1.,1.),(1.,1.),(1.,1.),(1.,1.),(1.,
1.),(1.,1.),(1.,1.),(1.,1.),(1.,1.),(1.,1.),(1.,1.),(1.,1.),(1.,1.),(1.,
1.),(1.,1.),(1.,1.),(1.,1.),(1.,1.),(1.,1.),(1.,1.),(1.,1.),(1.,1.),(1.,
1.),(1.,1.),(1.,1.)))
REPRESENTATION_ITEM('')
SURFACE()
);
#139=(
BOUNDED_SURFACE()
B_SPLINE_SURFACE(5,1,((#97256,#97257),(#97258,#97259),(#97260,#97261),(#97262,
#97263),(#97264,#97265),(#97266,#97267),(#97268,#97269),(#97270,#97271),
(#97272,#97273),(#97274,#97275),(#97276,#97277),(#97278,#97279),(#97280,
#97281),(#97282,#97283),(#97284,#97285),(#97286,#97287),(#97288,#97289),
(#97290,#97291),(#97292,#97293),(#97294,#97295),(#97296,#97297),(#97298,
#97299),(#97300,#97301),(#97302,#97303),(#97304,#97305),(#97306,#97307),
(#97308,#97309),(#97310,#97311),(#97312,#97313),(#97314,#97315),(#97316,
#97317),(#97318,#97319),(#97320,#97321),(#97322,#97323),(#97324,#97325)),
 .UNSPECIFIED.,.F.,.F.,.F.)
B_SPLINE_SURFACE_WITH_KNOTS((6,1,1,1,1,1,1,1,1,1,1,1,1,1,1,1,1,1,1,1,1,
1,1,1,1,1,1,1,1,1,6),(2,2),(0.,0.0333333333333333,0.0666666666666667,0.1,
0.133333333333333,0.166666666666667,0.2,0.233333333333333,0.266666666666667,
0.3,0.333333333333333,0.366666666666667,0.4,0.433333333333333,0.466666666666667,
0.5,0.533333333333333,0.566666666666667,0.6,0.633333333333333,0.666666666666667,
0.7,0.733333333333333,0.766666666666667,0.8,0.833333333333333,0.866666666666667,
0.9,0.933333333333333,0.966666666666667,1.),(0.,0.5),.UNSPECIFIED.)
GEOMETRIC_REPRESENTATION_ITEM()
RATIONAL_B_SPLINE_SURFACE(((1.,1.),(1.,1.),(1.,1.),(1.,1.),(1.,1.),(1.,
1.),(1.,1.),(1.,1.),(1.,1.),(1.,1.),(1.,1.),(1.,1.),(1.,1.),(1.,1.),(1.,
1.),(1.,1.),(1.,1.),(1.,1.),(1.,1.),(1.,1.),(1.,1.),(1.,1.),(1.,1.),(1.,
1.),(1.,1.),(1.,1.),(1.,1.),(1.,1.),(1.,1.),(1.,1.),(1.,1.),(1.,1.),(1.,
1.),(1.,1.),(1.,1.)))
REPRESENTATION_ITEM('')
SURFACE()
);
#140=(
BOUNDED_SURFACE()
B_SPLINE_SURFACE(5,1,((#97403,#97404),(#97405,#97406),(#97407,#97408),(#97409,
#97410),(#97411,#97412),(#97413,#97414),(#97415,#97416),(#97417,#97418),
(#97419,#97420),(#97421,#97422),(#97423,#97424),(#97425,#97426),(#97427,
#97428),(#97429,#97430),(#97431,#97432),(#97433,#97434),(#97435,#97436),
(#97437,#97438),(#97439,#97440),(#97441,#97442),(#97443,#97444),(#97445,
#97446),(#97447,#97448),(#97449,#97450),(#97451,#97452),(#97453,#97454),
(#97455,#97456),(#97457,#97458),(#97459,#97460),(#97461,#97462),(#97463,
#97464),(#97465,#97466),(#97467,#97468),(#97469,#97470),(#97471,#97472)),
 .UNSPECIFIED.,.F.,.F.,.F.)
B_SPLINE_SURFACE_WITH_KNOTS((6,1,1,1,1,1,1,1,1,1,1,1,1,1,1,1,1,1,1,1,1,
1,1,1,1,1,1,1,1,1,6),(2,2),(-1.,-0.966666666666667,-0.933333333333333,-0.9,
-0.866666666666667,-0.833333333333333,-0.8,-0.766666666666667,-0.733333333333333,
-0.7,-0.666666666666667,-0.633333333333333,-0.6,-0.566666666666667,-0.533333333333333,
-0.5,-0.466666666666667,-0.433333333333333,-0.4,-0.366666666666667,-0.333333333333333,
-0.3,-0.266666666666667,-0.233333333333333,-0.2,-0.166666666666667,-0.133333333333333,
-0.1,-0.0666666666666667,-0.0333333333333333,0.),(0.,0.5),.UNSPECIFIED.)
GEOMETRIC_REPRESENTATION_ITEM()
RATIONAL_B_SPLINE_SURFACE(((1.,1.),(1.,1.),(1.,1.),(1.,1.),(1.,1.),(1.,
1.),(1.,1.),(1.,1.),(1.,1.),(1.,1.),(1.,1.),(1.,1.),(1.,1.),(1.,1.),(1.,
1.),(1.,1.),(1.,1.),(1.,1.),(1.,1.),(1.,1.),(1.,1.),(1.,1.),(1.,1.),(1.,
1.),(1.,1.),(1.,1.),(1.,1.),(1.,1.),(1.,1.),(1.,1.),(1.,1.),(1.,1.),(1.,
1.),(1.,1.),(1.,1.)))
REPRESENTATION_ITEM('')
SURFACE()
);
#141=(
BOUNDED_SURFACE()
B_SPLINE_SURFACE(5,1,((#97552,#97553),(#97554,#97555),(#97556,#97557),(#97558,
#97559),(#97560,#97561),(#97562,#97563),(#97564,#97565),(#97566,#97567),
(#97568,#97569),(#97570,#97571),(#97572,#97573),(#97574,#97575),(#97576,
#97577),(#97578,#97579),(#97580,#97581),(#97582,#97583),(#97584,#97585),
(#97586,#97587),(#97588,#97589),(#97590,#97591),(#97592,#97593),(#97594,
#97595),(#97596,#97597),(#97598,#97599),(#97600,#97601),(#97602,#97603),
(#97604,#97605),(#97606,#97607),(#97608,#97609),(#97610,#97611),(#97612,
#97613),(#97614,#97615),(#97616,#97617),(#97618,#97619),(#97620,#97621)),
 .UNSPECIFIED.,.F.,.F.,.F.)
B_SPLINE_SURFACE_WITH_KNOTS((6,1,1,1,1,1,1,1,1,1,1,1,1,1,1,1,1,1,1,1,1,
1,1,1,1,1,1,1,1,1,6),(2,2),(0.,0.0333333333333333,0.0666666666666667,0.1,
0.133333333333333,0.166666666666667,0.2,0.233333333333333,0.266666666666667,
0.3,0.333333333333333,0.366666666666667,0.4,0.433333333333333,0.466666666666667,
0.5,0.533333333333333,0.566666666666667,0.6,0.633333333333333,0.666666666666667,
0.7,0.733333333333333,0.766666666666667,0.8,0.833333333333333,0.866666666666667,
0.9,0.933333333333333,0.966666666666667,1.),(0.,0.5),.UNSPECIFIED.)
GEOMETRIC_REPRESENTATION_ITEM()
RATIONAL_B_SPLINE_SURFACE(((1.,1.),(1.,1.),(1.,1.),(1.,1.),(1.,1.),(1.,
1.),(1.,1.),(1.,1.),(1.,1.),(1.,1.),(1.,1.),(1.,1.),(1.,1.),(1.,1.),(1.,
1.),(1.,1.),(1.,1.),(1.,1.),(1.,1.),(1.,1.),(1.,1.),(1.,1.),(1.,1.),(1.,
1.),(1.,1.),(1.,1.),(1.,1.),(1.,1.),(1.,1.),(1.,1.),(1.,1.),(1.,1.),(1.,
1.),(1.,1.),(1.,1.)))
REPRESENTATION_ITEM('')
SURFACE()
);
#142=(
BOUNDED_CURVE()
B_SPLINE_CURVE(2,(#92151,#92152,#92153),.UNSPECIFIED.,.F.,.F.)
B_SPLINE_CURVE_WITH_KNOTS((3,3),(0.,0.16248076809272),.UNSPECIFIED.)
CURVE()
GEOMETRIC_REPRESENTATION_ITEM()
RATIONAL_B_SPLINE_CURVE((1.,1.,1.))
REPRESENTATION_ITEM('')
);
#143=(
BOUNDED_CURVE()
B_SPLINE_CURVE(2,(#92201,#92202,#92203),.UNSPECIFIED.,.F.,.F.)
B_SPLINE_CURVE_WITH_KNOTS((3,3),(0.,0.0845576726264383),.UNSPECIFIED.)
CURVE()
GEOMETRIC_REPRESENTATION_ITEM()
RATIONAL_B_SPLINE_CURVE((1.,1.,1.))
REPRESENTATION_ITEM('')
);
#144=(
BOUNDED_CURVE()
B_SPLINE_CURVE(2,(#92222,#92223,#92224),.UNSPECIFIED.,.F.,.F.)
B_SPLINE_CURVE_WITH_KNOTS((3,3),(0.,0.0845576726264383),.UNSPECIFIED.)
CURVE()
GEOMETRIC_REPRESENTATION_ITEM()
RATIONAL_B_SPLINE_CURVE((1.,1.,1.))
REPRESENTATION_ITEM('')
);
#145=(
BOUNDED_CURVE()
B_SPLINE_CURVE(2,(#92227,#92228,#92229),.UNSPECIFIED.,.F.,.F.)
B_SPLINE_CURVE_WITH_KNOTS((3,3),(0.16248076809272,0.324961536185439),
 .UNSPECIFIED.)
CURVE()
GEOMETRIC_REPRESENTATION_ITEM()
RATIONAL_B_SPLINE_CURVE((1.,1.,1.))
REPRESENTATION_ITEM('')
);
#146=(
BOUNDED_CURVE()
B_SPLINE_CURVE(2,(#92262,#92263,#92264),.UNSPECIFIED.,.F.,.F.)
B_SPLINE_CURVE_WITH_KNOTS((3,3),(0.,0.13564659966251),.UNSPECIFIED.)
CURVE()
GEOMETRIC_REPRESENTATION_ITEM()
RATIONAL_B_SPLINE_CURVE((1.,1.,1.))
REPRESENTATION_ITEM('')
);
#147=(
BOUNDED_CURVE()
B_SPLINE_CURVE(5,(#92822,#92823,#92824,#92825,#92826,#92827,#92828,#92829,
#92830,#92831,#92832,#92833,#92834,#92835,#92836,#92837,#92838,#92839,#92840,
#92841,#92842,#92843,#92844,#92845,#92846,#92847,#92848,#92849,#92850,#92851,
#92852,#92853,#92854,#92855,#92856),.UNSPECIFIED.,.F.,.F.)
B_SPLINE_CURVE_WITH_KNOTS((6,1,1,1,1,1,1,1,1,1,1,1,1,1,1,1,1,1,1,1,1,1,
1,1,1,1,1,1,1,1,6),(0.,0.0333333333333333,0.0666666666666667,0.1,0.133333333333333,
0.166666666666667,0.2,0.233333333333333,0.266666666666667,0.3,0.333333333333333,
0.366666666666667,0.4,0.433333333333333,0.466666666666667,0.5,0.533333333333333,
0.566666666666667,0.6,0.633333333333333,0.666666666666667,0.7,0.733333333333333,
0.766666666666667,0.8,0.833333333333333,0.866666666666667,0.9,0.933333333333333,
0.966666666666667,1.),.UNSPECIFIED.)
CURVE()
GEOMETRIC_REPRESENTATION_ITEM()
RATIONAL_B_SPLINE_CURVE((1.,1.,1.,1.,1.,1.,1.,1.,1.,1.,1.,1.,1.,1.,1.,1.,
1.,1.,1.,1.,1.,1.,1.,1.,1.,1.,1.,1.,1.,1.,1.,1.,1.,1.,1.))
REPRESENTATION_ITEM('')
);
#148=(
BOUNDED_CURVE()
B_SPLINE_CURVE(5,(#92858,#92859,#92860,#92861,#92862,#92863,#92864,#92865,
#92866,#92867,#92868,#92869,#92870,#92871,#92872,#92873,#92874,#92875,#92876,
#92877,#92878,#92879,#92880,#92881,#92882,#92883,#92884,#92885,#92886,#92887,
#92888,#92889,#92890,#92891,#92892),.UNSPECIFIED.,.F.,.F.)
B_SPLINE_CURVE_WITH_KNOTS((6,1,1,1,1,1,1,1,1,1,1,1,1,1,1,1,1,1,1,1,1,1,
1,1,1,1,1,1,1,1,6),(-1.,-0.966666666666667,-0.933333333333333,-0.9,-0.866666666666667,
-0.833333333333333,-0.8,-0.766666666666667,-0.733333333333333,-0.7,-0.666666666666667,
-0.633333333333333,-0.6,-0.566666666666667,-0.533333333333333,-0.5,-0.466666666666667,
-0.433333333333333,-0.4,-0.366666666666667,-0.333333333333333,-0.3,-0.266666666666667,
-0.233333333333333,-0.2,-0.166666666666667,-0.133333333333333,-0.1,-0.0666666666666667,
-0.0333333333333333,0.),.UNSPECIFIED.)
CURVE()
GEOMETRIC_REPRESENTATION_ITEM()
RATIONAL_B_SPLINE_CURVE((1.,1.,1.,1.,1.,1.,1.,1.,1.,1.,1.,1.,1.,1.,1.,1.,
1.,1.,1.,1.,1.,1.,1.,1.,1.,1.,1.,1.,1.,1.,1.,1.,1.,1.,1.))
REPRESENTATION_ITEM('')
);
#149=(
BOUNDED_CURVE()
B_SPLINE_CURVE(5,(#92970,#92971,#92972,#92973,#92974,#92975,#92976,#92977,
#92978,#92979,#92980,#92981,#92982,#92983,#92984,#92985,#92986,#92987,#92988,
#92989,#92990,#92991,#92992,#92993,#92994,#92995,#92996,#92997,#92998,#92999,
#93000,#93001,#93002,#93003,#93004),.UNSPECIFIED.,.F.,.F.)
B_SPLINE_CURVE_WITH_KNOTS((6,1,1,1,1,1,1,1,1,1,1,1,1,1,1,1,1,1,1,1,1,1,
1,1,1,1,1,1,1,1,6),(0.,0.0333333333333333,0.0666666666666667,0.1,0.133333333333333,
0.166666666666667,0.2,0.233333333333333,0.266666666666667,0.3,0.333333333333333,
0.366666666666667,0.4,0.433333333333333,0.466666666666667,0.5,0.533333333333333,
0.566666666666667,0.6,0.633333333333333,0.666666666666667,0.7,0.733333333333333,
0.766666666666667,0.8,0.833333333333333,0.866666666666667,0.9,0.933333333333333,
0.966666666666667,1.),.UNSPECIFIED.)
CURVE()
GEOMETRIC_REPRESENTATION_ITEM()
RATIONAL_B_SPLINE_CURVE((1.,1.,1.,1.,1.,1.,1.,1.,1.,1.,1.,1.,1.,1.,1.,1.,
1.,1.,1.,1.,1.,1.,1.,1.,1.,1.,1.,1.,1.,1.,1.,1.,1.,1.,1.))
REPRESENTATION_ITEM('')
);
#150=(
BOUNDED_CURVE()
B_SPLINE_CURVE(5,(#93005,#93006,#93007,#93008,#93009,#93010,#93011,#93012,
#93013,#93014,#93015,#93016,#93017,#93018,#93019,#93020,#93021,#93022,#93023,
#93024,#93025,#93026,#93027,#93028,#93029,#93030,#93031,#93032,#93033,#93034,
#93035,#93036,#93037,#93038,#93039),.UNSPECIFIED.,.F.,.F.)
B_SPLINE_CURVE_WITH_KNOTS((6,1,1,1,1,1,1,1,1,1,1,1,1,1,1,1,1,1,1,1,1,1,
1,1,1,1,1,1,1,1,6),(0.,0.0333333333333333,0.0666666666666667,0.1,0.133333333333333,
0.166666666666667,0.2,0.233333333333333,0.266666666666667,0.3,0.333333333333333,
0.366666666666667,0.4,0.433333333333333,0.466666666666667,0.5,0.533333333333333,
0.566666666666667,0.6,0.633333333333333,0.666666666666667,0.7,0.733333333333333,
0.766666666666667,0.8,0.833333333333333,0.866666666666667,0.9,0.933333333333333,
0.966666666666667,1.),.UNSPECIFIED.)
CURVE()
GEOMETRIC_REPRESENTATION_ITEM()
RATIONAL_B_SPLINE_CURVE((1.,1.,1.,1.,1.,1.,1.,1.,1.,1.,1.,1.,1.,1.,1.,1.,
1.,1.,1.,1.,1.,1.,1.,1.,1.,1.,1.,1.,1.,1.,1.,1.,1.,1.,1.))
REPRESENTATION_ITEM('')
);
#151=(
BOUNDED_CURVE()
B_SPLINE_CURVE(5,(#93252,#93253,#93254,#93255,#93256,#93257,#93258,#93259,
#93260,#93261,#93262,#93263,#93264,#93265,#93266,#93267,#93268,#93269,#93270,
#93271,#93272,#93273,#93274,#93275,#93276,#93277,#93278,#93279,#93280,#93281,
#93282,#93283,#93284,#93285,#93286),.UNSPECIFIED.,.F.,.F.)
B_SPLINE_CURVE_WITH_KNOTS((6,1,1,1,1,1,1,1,1,1,1,1,1,1,1,1,1,1,1,1,1,1,
1,1,1,1,1,1,1,1,6),(0.,0.0333333333333333,0.0666666666666667,0.1,0.133333333333333,
0.166666666666667,0.2,0.233333333333333,0.266666666666667,0.3,0.333333333333333,
0.366666666666667,0.4,0.433333333333333,0.466666666666667,0.5,0.533333333333333,
0.566666666666667,0.6,0.633333333333333,0.666666666666667,0.7,0.733333333333333,
0.766666666666667,0.8,0.833333333333333,0.866666666666667,0.9,0.933333333333333,
0.966666666666667,1.),.UNSPECIFIED.)
CURVE()
GEOMETRIC_REPRESENTATION_ITEM()
RATIONAL_B_SPLINE_CURVE((1.,1.,1.,1.,1.,1.,1.,1.,1.,1.,1.,1.,1.,1.,1.,1.,
1.,1.,1.,1.,1.,1.,1.,1.,1.,1.,1.,1.,1.,1.,1.,1.,1.,1.,1.))
REPRESENTATION_ITEM('')
);
#152=(
BOUNDED_CURVE()
B_SPLINE_CURVE(5,(#93288,#93289,#93290,#93291,#93292,#93293,#93294,#93295,
#93296,#93297,#93298,#93299,#93300,#93301,#93302,#93303,#93304,#93305,#93306,
#93307,#93308,#93309,#93310,#93311,#93312,#93313,#93314,#93315,#93316,#93317,
#93318,#93319,#93320,#93321,#93322),.UNSPECIFIED.,.F.,.F.)
B_SPLINE_CURVE_WITH_KNOTS((6,1,1,1,1,1,1,1,1,1,1,1,1,1,1,1,1,1,1,1,1,1,
1,1,1,1,1,1,1,1,6),(-1.,-0.966666666666667,-0.933333333333333,-0.9,-0.866666666666667,
-0.833333333333333,-0.8,-0.766666666666667,-0.733333333333333,-0.7,-0.666666666666667,
-0.633333333333333,-0.6,-0.566666666666667,-0.533333333333333,-0.5,-0.466666666666667,
-0.433333333333333,-0.4,-0.366666666666667,-0.333333333333333,-0.3,-0.266666666666667,
-0.233333333333333,-0.2,-0.166666666666667,-0.133333333333333,-0.1,-0.0666666666666667,
-0.0333333333333333,0.),.UNSPECIFIED.)
CURVE()
GEOMETRIC_REPRESENTATION_ITEM()
RATIONAL_B_SPLINE_CURVE((1.,1.,1.,1.,1.,1.,1.,1.,1.,1.,1.,1.,1.,1.,1.,1.,
1.,1.,1.,1.,1.,1.,1.,1.,1.,1.,1.,1.,1.,1.,1.,1.,1.,1.,1.))
REPRESENTATION_ITEM('')
);
#153=(
BOUNDED_CURVE()
B_SPLINE_CURVE(5,(#93400,#93401,#93402,#93403,#93404,#93405,#93406,#93407,
#93408,#93409,#93410,#93411,#93412,#93413,#93414,#93415,#93416,#93417,#93418,
#93419,#93420,#93421,#93422,#93423,#93424,#93425,#93426,#93427,#93428,#93429,
#93430,#93431,#93432,#93433,#93434),.UNSPECIFIED.,.F.,.F.)
B_SPLINE_CURVE_WITH_KNOTS((6,1,1,1,1,1,1,1,1,1,1,1,1,1,1,1,1,1,1,1,1,1,
1,1,1,1,1,1,1,1,6),(0.,0.0333333333333333,0.0666666666666667,0.1,0.133333333333333,
0.166666666666667,0.2,0.233333333333333,0.266666666666667,0.3,0.333333333333333,
0.366666666666667,0.4,0.433333333333333,0.466666666666667,0.5,0.533333333333333,
0.566666666666667,0.6,0.633333333333333,0.666666666666667,0.7,0.733333333333333,
0.766666666666667,0.8,0.833333333333333,0.866666666666667,0.9,0.933333333333333,
0.966666666666667,1.),.UNSPECIFIED.)
CURVE()
GEOMETRIC_REPRESENTATION_ITEM()
RATIONAL_B_SPLINE_CURVE((1.,1.,1.,1.,1.,1.,1.,1.,1.,1.,1.,1.,1.,1.,1.,1.,
1.,1.,1.,1.,1.,1.,1.,1.,1.,1.,1.,1.,1.,1.,1.,1.,1.,1.,1.))
REPRESENTATION_ITEM('')
);
#154=(
BOUNDED_CURVE()
B_SPLINE_CURVE(5,(#93435,#93436,#93437,#93438,#93439,#93440,#93441,#93442,
#93443,#93444,#93445,#93446,#93447,#93448,#93449,#93450,#93451,#93452,#93453,
#93454,#93455,#93456,#93457,#93458,#93459,#93460,#93461,#93462,#93463,#93464,
#93465,#93466,#93467,#93468,#93469),.UNSPECIFIED.,.F.,.F.)
B_SPLINE_CURVE_WITH_KNOTS((6,1,1,1,1,1,1,1,1,1,1,1,1,1,1,1,1,1,1,1,1,1,
1,1,1,1,1,1,1,1,6),(0.,0.0333333333333333,0.0666666666666667,0.1,0.133333333333333,
0.166666666666667,0.2,0.233333333333333,0.266666666666667,0.3,0.333333333333333,
0.366666666666667,0.4,0.433333333333333,0.466666666666667,0.5,0.533333333333333,
0.566666666666667,0.6,0.633333333333333,0.666666666666667,0.7,0.733333333333333,
0.766666666666667,0.8,0.833333333333333,0.866666666666667,0.9,0.933333333333333,
0.966666666666667,1.),.UNSPECIFIED.)
CURVE()
GEOMETRIC_REPRESENTATION_ITEM()
RATIONAL_B_SPLINE_CURVE((1.,1.,1.,1.,1.,1.,1.,1.,1.,1.,1.,1.,1.,1.,1.,1.,
1.,1.,1.,1.,1.,1.,1.,1.,1.,1.,1.,1.,1.,1.,1.,1.,1.,1.,1.))
REPRESENTATION_ITEM('')
);
#155=(
BOUNDED_CURVE()
B_SPLINE_CURVE(5,(#93554,#93555,#93556,#93557,#93558,#93559,#93560,#93561,
#93562,#93563,#93564,#93565,#93566,#93567,#93568,#93569,#93570,#93571,#93572,
#93573,#93574,#93575,#93576,#93577,#93578,#93579,#93580,#93581,#93582,#93583,
#93584,#93585,#93586,#93587,#93588),.UNSPECIFIED.,.F.,.F.)
B_SPLINE_CURVE_WITH_KNOTS((6,1,1,1,1,1,1,1,1,1,1,1,1,1,1,1,1,1,1,1,1,1,
1,1,1,1,1,1,1,1,6),(0.,0.0333333333333333,0.0666666666666667,0.1,0.133333333333333,
0.166666666666667,0.2,0.233333333333333,0.266666666666667,0.3,0.333333333333333,
0.366666666666667,0.4,0.433333333333333,0.466666666666667,0.5,0.533333333333333,
0.566666666666667,0.6,0.633333333333333,0.666666666666667,0.7,0.733333333333333,
0.766666666666667,0.8,0.833333333333333,0.866666666666667,0.9,0.933333333333333,
0.966666666666667,1.),.UNSPECIFIED.)
CURVE()
GEOMETRIC_REPRESENTATION_ITEM()
RATIONAL_B_SPLINE_CURVE((1.,1.,1.,1.,1.,1.,1.,1.,1.,1.,1.,1.,1.,1.,1.,1.,
1.,1.,1.,1.,1.,1.,1.,1.,1.,1.,1.,1.,1.,1.,1.,1.,1.,1.,1.))
REPRESENTATION_ITEM('')
);
#156=(
BOUNDED_CURVE()
B_SPLINE_CURVE(5,(#93590,#93591,#93592,#93593,#93594,#93595,#93596,#93597,
#93598,#93599,#93600,#93601,#93602,#93603,#93604,#93605,#93606,#93607,#93608,
#93609,#93610,#93611,#93612,#93613,#93614,#93615,#93616,#93617,#93618,#93619,
#93620,#93621,#93622,#93623,#93624),.UNSPECIFIED.,.F.,.F.)
B_SPLINE_CURVE_WITH_KNOTS((6,1,1,1,1,1,1,1,1,1,1,1,1,1,1,1,1,1,1,1,1,1,
1,1,1,1,1,1,1,1,6),(-1.,-0.966666666666667,-0.933333333333333,-0.9,-0.866666666666667,
-0.833333333333333,-0.8,-0.766666666666667,-0.733333333333333,-0.7,-0.666666666666667,
-0.633333333333333,-0.6,-0.566666666666667,-0.533333333333333,-0.5,-0.466666666666667,
-0.433333333333333,-0.4,-0.366666666666667,-0.333333333333333,-0.3,-0.266666666666667,
-0.233333333333333,-0.2,-0.166666666666667,-0.133333333333333,-0.1,-0.0666666666666667,
-0.0333333333333333,0.),.UNSPECIFIED.)
CURVE()
GEOMETRIC_REPRESENTATION_ITEM()
RATIONAL_B_SPLINE_CURVE((1.,1.,1.,1.,1.,1.,1.,1.,1.,1.,1.,1.,1.,1.,1.,1.,
1.,1.,1.,1.,1.,1.,1.,1.,1.,1.,1.,1.,1.,1.,1.,1.,1.,1.,1.))
REPRESENTATION_ITEM('')
);
#157=(
BOUNDED_CURVE()
B_SPLINE_CURVE(5,(#93702,#93703,#93704,#93705,#93706,#93707,#93708,#93709,
#93710,#93711,#93712,#93713,#93714,#93715,#93716,#93717,#93718,#93719,#93720,
#93721,#93722,#93723,#93724,#93725,#93726,#93727,#93728,#93729,#93730,#93731,
#93732,#93733,#93734,#93735,#93736),.UNSPECIFIED.,.F.,.F.)
B_SPLINE_CURVE_WITH_KNOTS((6,1,1,1,1,1,1,1,1,1,1,1,1,1,1,1,1,1,1,1,1,1,
1,1,1,1,1,1,1,1,6),(0.,0.0333333333333333,0.0666666666666667,0.1,0.133333333333333,
0.166666666666667,0.2,0.233333333333333,0.266666666666667,0.3,0.333333333333333,
0.366666666666667,0.4,0.433333333333333,0.466666666666667,0.5,0.533333333333333,
0.566666666666667,0.6,0.633333333333333,0.666666666666667,0.7,0.733333333333333,
0.766666666666667,0.8,0.833333333333333,0.866666666666667,0.9,0.933333333333333,
0.966666666666667,1.),.UNSPECIFIED.)
CURVE()
GEOMETRIC_REPRESENTATION_ITEM()
RATIONAL_B_SPLINE_CURVE((1.,1.,1.,1.,1.,1.,1.,1.,1.,1.,1.,1.,1.,1.,1.,1.,
1.,1.,1.,1.,1.,1.,1.,1.,1.,1.,1.,1.,1.,1.,1.,1.,1.,1.,1.))
REPRESENTATION_ITEM('')
);
#158=(
BOUNDED_CURVE()
B_SPLINE_CURVE(5,(#93737,#93738,#93739,#93740,#93741,#93742,#93743,#93744,
#93745,#93746,#93747,#93748,#93749,#93750,#93751,#93752,#93753,#93754,#93755,
#93756,#93757,#93758,#93759,#93760,#93761,#93762,#93763,#93764,#93765,#93766,
#93767,#93768,#93769,#93770,#93771),.UNSPECIFIED.,.F.,.F.)
B_SPLINE_CURVE_WITH_KNOTS((6,1,1,1,1,1,1,1,1,1,1,1,1,1,1,1,1,1,1,1,1,1,
1,1,1,1,1,1,1,1,6),(0.,0.0333333333333333,0.0666666666666667,0.1,0.133333333333333,
0.166666666666667,0.2,0.233333333333333,0.266666666666667,0.3,0.333333333333333,
0.366666666666667,0.4,0.433333333333333,0.466666666666667,0.5,0.533333333333333,
0.566666666666667,0.6,0.633333333333333,0.666666666666667,0.7,0.733333333333333,
0.766666666666667,0.8,0.833333333333333,0.866666666666667,0.9,0.933333333333333,
0.966666666666667,1.),.UNSPECIFIED.)
CURVE()
GEOMETRIC_REPRESENTATION_ITEM()
RATIONAL_B_SPLINE_CURVE((1.,1.,1.,1.,1.,1.,1.,1.,1.,1.,1.,1.,1.,1.,1.,1.,
1.,1.,1.,1.,1.,1.,1.,1.,1.,1.,1.,1.,1.,1.,1.,1.,1.,1.,1.))
REPRESENTATION_ITEM('')
);
#159=(
BOUNDED_CURVE()
B_SPLINE_CURVE(5,(#93856,#93857,#93858,#93859,#93860,#93861,#93862,#93863,
#93864,#93865,#93866,#93867,#93868,#93869,#93870,#93871,#93872,#93873,#93874,
#93875,#93876,#93877,#93878,#93879,#93880,#93881,#93882,#93883,#93884,#93885,
#93886,#93887,#93888,#93889,#93890),.UNSPECIFIED.,.F.,.F.)
B_SPLINE_CURVE_WITH_KNOTS((6,1,1,1,1,1,1,1,1,1,1,1,1,1,1,1,1,1,1,1,1,1,
1,1,1,1,1,1,1,1,6),(0.,0.0333333333333333,0.0666666666666667,0.1,0.133333333333333,
0.166666666666667,0.2,0.233333333333333,0.266666666666667,0.3,0.333333333333333,
0.366666666666667,0.4,0.433333333333333,0.466666666666667,0.5,0.533333333333333,
0.566666666666667,0.6,0.633333333333333,0.666666666666667,0.7,0.733333333333333,
0.766666666666667,0.8,0.833333333333333,0.866666666666667,0.9,0.933333333333333,
0.966666666666667,1.),.UNSPECIFIED.)
CURVE()
GEOMETRIC_REPRESENTATION_ITEM()
RATIONAL_B_SPLINE_CURVE((1.,1.,1.,1.,1.,1.,1.,1.,1.,1.,1.,1.,1.,1.,1.,1.,
1.,1.,1.,1.,1.,1.,1.,1.,1.,1.,1.,1.,1.,1.,1.,1.,1.,1.,1.))
REPRESENTATION_ITEM('')
);
#160=(
BOUNDED_CURVE()
B_SPLINE_CURVE(5,(#93892,#93893,#93894,#93895,#93896,#93897,#93898,#93899,
#93900,#93901,#93902,#93903,#93904,#93905,#93906,#93907,#93908,#93909,#93910,
#93911,#93912,#93913,#93914,#93915,#93916,#93917,#93918,#93919,#93920,#93921,
#93922,#93923,#93924,#93925,#93926),.UNSPECIFIED.,.F.,.F.)
B_SPLINE_CURVE_WITH_KNOTS((6,1,1,1,1,1,1,1,1,1,1,1,1,1,1,1,1,1,1,1,1,1,
1,1,1,1,1,1,1,1,6),(-1.,-0.966666666666667,-0.933333333333333,-0.9,-0.866666666666667,
-0.833333333333333,-0.8,-0.766666666666667,-0.733333333333333,-0.7,-0.666666666666667,
-0.633333333333333,-0.6,-0.566666666666667,-0.533333333333333,-0.5,-0.466666666666667,
-0.433333333333333,-0.4,-0.366666666666667,-0.333333333333333,-0.3,-0.266666666666667,
-0.233333333333333,-0.2,-0.166666666666667,-0.133333333333333,-0.1,-0.0666666666666667,
-0.0333333333333333,0.),.UNSPECIFIED.)
CURVE()
GEOMETRIC_REPRESENTATION_ITEM()
RATIONAL_B_SPLINE_CURVE((1.,1.,1.,1.,1.,1.,1.,1.,1.,1.,1.,1.,1.,1.,1.,1.,
1.,1.,1.,1.,1.,1.,1.,1.,1.,1.,1.,1.,1.,1.,1.,1.,1.,1.,1.))
REPRESENTATION_ITEM('')
);
#161=(
BOUNDED_CURVE()
B_SPLINE_CURVE(5,(#94004,#94005,#94006,#94007,#94008,#94009,#94010,#94011,
#94012,#94013,#94014,#94015,#94016,#94017,#94018,#94019,#94020,#94021,#94022,
#94023,#94024,#94025,#94026,#94027,#94028,#94029,#94030,#94031,#94032,#94033,
#94034,#94035,#94036,#94037,#94038),.UNSPECIFIED.,.F.,.F.)
B_SPLINE_CURVE_WITH_KNOTS((6,1,1,1,1,1,1,1,1,1,1,1,1,1,1,1,1,1,1,1,1,1,
1,1,1,1,1,1,1,1,6),(0.,0.0333333333333333,0.0666666666666667,0.1,0.133333333333333,
0.166666666666667,0.2,0.233333333333333,0.266666666666667,0.3,0.333333333333333,
0.366666666666667,0.4,0.433333333333333,0.466666666666667,0.5,0.533333333333333,
0.566666666666667,0.6,0.633333333333333,0.666666666666667,0.7,0.733333333333333,
0.766666666666667,0.8,0.833333333333333,0.866666666666667,0.9,0.933333333333333,
0.966666666666667,1.),.UNSPECIFIED.)
CURVE()
GEOMETRIC_REPRESENTATION_ITEM()
RATIONAL_B_SPLINE_CURVE((1.,1.,1.,1.,1.,1.,1.,1.,1.,1.,1.,1.,1.,1.,1.,1.,
1.,1.,1.,1.,1.,1.,1.,1.,1.,1.,1.,1.,1.,1.,1.,1.,1.,1.,1.))
REPRESENTATION_ITEM('')
);
#162=(
BOUNDED_CURVE()
B_SPLINE_CURVE(5,(#94039,#94040,#94041,#94042,#94043,#94044,#94045,#94046,
#94047,#94048,#94049,#94050,#94051,#94052,#94053,#94054,#94055,#94056,#94057,
#94058,#94059,#94060,#94061,#94062,#94063,#94064,#94065,#94066,#94067,#94068,
#94069,#94070,#94071,#94072,#94073),.UNSPECIFIED.,.F.,.F.)
B_SPLINE_CURVE_WITH_KNOTS((6,1,1,1,1,1,1,1,1,1,1,1,1,1,1,1,1,1,1,1,1,1,
1,1,1,1,1,1,1,1,6),(0.,0.0333333333333333,0.0666666666666667,0.1,0.133333333333333,
0.166666666666667,0.2,0.233333333333333,0.266666666666667,0.3,0.333333333333333,
0.366666666666667,0.4,0.433333333333333,0.466666666666667,0.5,0.533333333333333,
0.566666666666667,0.6,0.633333333333333,0.666666666666667,0.7,0.733333333333333,
0.766666666666667,0.8,0.833333333333333,0.866666666666667,0.9,0.933333333333333,
0.966666666666667,1.),.UNSPECIFIED.)
CURVE()
GEOMETRIC_REPRESENTATION_ITEM()
RATIONAL_B_SPLINE_CURVE((1.,1.,1.,1.,1.,1.,1.,1.,1.,1.,1.,1.,1.,1.,1.,1.,
1.,1.,1.,1.,1.,1.,1.,1.,1.,1.,1.,1.,1.,1.,1.,1.,1.,1.,1.))
REPRESENTATION_ITEM('')
);
#163=(
BOUNDED_CURVE()
B_SPLINE_CURVE(5,(#94158,#94159,#94160,#94161,#94162,#94163,#94164,#94165,
#94166,#94167,#94168,#94169,#94170,#94171,#94172,#94173,#94174,#94175,#94176,
#94177,#94178,#94179,#94180,#94181,#94182,#94183,#94184,#94185,#94186,#94187,
#94188,#94189,#94190,#94191,#94192),.UNSPECIFIED.,.F.,.F.)
B_SPLINE_CURVE_WITH_KNOTS((6,1,1,1,1,1,1,1,1,1,1,1,1,1,1,1,1,1,1,1,1,1,
1,1,1,1,1,1,1,1,6),(0.,0.0333333333333333,0.0666666666666667,0.1,0.133333333333333,
0.166666666666667,0.2,0.233333333333333,0.266666666666667,0.3,0.333333333333333,
0.366666666666667,0.4,0.433333333333333,0.466666666666667,0.5,0.533333333333333,
0.566666666666667,0.6,0.633333333333333,0.666666666666667,0.7,0.733333333333333,
0.766666666666667,0.8,0.833333333333333,0.866666666666667,0.9,0.933333333333333,
0.966666666666667,1.),.UNSPECIFIED.)
CURVE()
GEOMETRIC_REPRESENTATION_ITEM()
RATIONAL_B_SPLINE_CURVE((1.,1.,1.,1.,1.,1.,1.,1.,1.,1.,1.,1.,1.,1.,1.,1.,
1.,1.,1.,1.,1.,1.,1.,1.,1.,1.,1.,1.,1.,1.,1.,1.,1.,1.,1.))
REPRESENTATION_ITEM('')
);
#164=(
BOUNDED_CURVE()
B_SPLINE_CURVE(5,(#94194,#94195,#94196,#94197,#94198,#94199,#94200,#94201,
#94202,#94203,#94204,#94205,#94206,#94207,#94208,#94209,#94210,#94211,#94212,
#94213,#94214,#94215,#94216,#94217,#94218,#94219,#94220,#94221,#94222,#94223,
#94224,#94225,#94226,#94227,#94228),.UNSPECIFIED.,.F.,.F.)
B_SPLINE_CURVE_WITH_KNOTS((6,1,1,1,1,1,1,1,1,1,1,1,1,1,1,1,1,1,1,1,1,1,
1,1,1,1,1,1,1,1,6),(-1.,-0.966666666666667,-0.933333333333333,-0.9,-0.866666666666667,
-0.833333333333333,-0.8,-0.766666666666667,-0.733333333333333,-0.7,-0.666666666666667,
-0.633333333333333,-0.6,-0.566666666666667,-0.533333333333333,-0.5,-0.466666666666667,
-0.433333333333333,-0.4,-0.366666666666667,-0.333333333333333,-0.3,-0.266666666666667,
-0.233333333333333,-0.2,-0.166666666666667,-0.133333333333333,-0.1,-0.0666666666666667,
-0.0333333333333333,0.),.UNSPECIFIED.)
CURVE()
GEOMETRIC_REPRESENTATION_ITEM()
RATIONAL_B_SPLINE_CURVE((1.,1.,1.,1.,1.,1.,1.,1.,1.,1.,1.,1.,1.,1.,1.,1.,
1.,1.,1.,1.,1.,1.,1.,1.,1.,1.,1.,1.,1.,1.,1.,1.,1.,1.,1.))
REPRESENTATION_ITEM('')
);
#165=(
BOUNDED_CURVE()
B_SPLINE_CURVE(5,(#94306,#94307,#94308,#94309,#94310,#94311,#94312,#94313,
#94314,#94315,#94316,#94317,#94318,#94319,#94320,#94321,#94322,#94323,#94324,
#94325,#94326,#94327,#94328,#94329,#94330,#94331,#94332,#94333,#94334,#94335,
#94336,#94337,#94338,#94339,#94340),.UNSPECIFIED.,.F.,.F.)
B_SPLINE_CURVE_WITH_KNOTS((6,1,1,1,1,1,1,1,1,1,1,1,1,1,1,1,1,1,1,1,1,1,
1,1,1,1,1,1,1,1,6),(0.,0.0333333333333333,0.0666666666666667,0.1,0.133333333333333,
0.166666666666667,0.2,0.233333333333333,0.266666666666667,0.3,0.333333333333333,
0.366666666666667,0.4,0.433333333333333,0.466666666666667,0.5,0.533333333333333,
0.566666666666667,0.6,0.633333333333333,0.666666666666667,0.7,0.733333333333333,
0.766666666666667,0.8,0.833333333333333,0.866666666666667,0.9,0.933333333333333,
0.966666666666667,1.),.UNSPECIFIED.)
CURVE()
GEOMETRIC_REPRESENTATION_ITEM()
RATIONAL_B_SPLINE_CURVE((1.,1.,1.,1.,1.,1.,1.,1.,1.,1.,1.,1.,1.,1.,1.,1.,
1.,1.,1.,1.,1.,1.,1.,1.,1.,1.,1.,1.,1.,1.,1.,1.,1.,1.,1.))
REPRESENTATION_ITEM('')
);
#166=(
BOUNDED_CURVE()
B_SPLINE_CURVE(5,(#94341,#94342,#94343,#94344,#94345,#94346,#94347,#94348,
#94349,#94350,#94351,#94352,#94353,#94354,#94355,#94356,#94357,#94358,#94359,
#94360,#94361,#94362,#94363,#94364,#94365,#94366,#94367,#94368,#94369,#94370,
#94371,#94372,#94373,#94374,#94375),.UNSPECIFIED.,.F.,.F.)
B_SPLINE_CURVE_WITH_KNOTS((6,1,1,1,1,1,1,1,1,1,1,1,1,1,1,1,1,1,1,1,1,1,
1,1,1,1,1,1,1,1,6),(0.,0.0333333333333333,0.0666666666666667,0.1,0.133333333333333,
0.166666666666667,0.2,0.233333333333333,0.266666666666667,0.3,0.333333333333333,
0.366666666666667,0.4,0.433333333333333,0.466666666666667,0.5,0.533333333333333,
0.566666666666667,0.6,0.633333333333333,0.666666666666667,0.7,0.733333333333333,
0.766666666666667,0.8,0.833333333333333,0.866666666666667,0.9,0.933333333333333,
0.966666666666667,1.),.UNSPECIFIED.)
CURVE()
GEOMETRIC_REPRESENTATION_ITEM()
RATIONAL_B_SPLINE_CURVE((1.,1.,1.,1.,1.,1.,1.,1.,1.,1.,1.,1.,1.,1.,1.,1.,
1.,1.,1.,1.,1.,1.,1.,1.,1.,1.,1.,1.,1.,1.,1.,1.,1.,1.,1.))
REPRESENTATION_ITEM('')
);
#167=(
BOUNDED_CURVE()
B_SPLINE_CURVE(5,(#94460,#94461,#94462,#94463,#94464,#94465,#94466,#94467,
#94468,#94469,#94470,#94471,#94472,#94473,#94474,#94475,#94476,#94477,#94478,
#94479,#94480,#94481,#94482,#94483,#94484,#94485,#94486,#94487,#94488,#94489,
#94490,#94491,#94492,#94493,#94494),.UNSPECIFIED.,.F.,.F.)
B_SPLINE_CURVE_WITH_KNOTS((6,1,1,1,1,1,1,1,1,1,1,1,1,1,1,1,1,1,1,1,1,1,
1,1,1,1,1,1,1,1,6),(0.,0.0333333333333333,0.0666666666666667,0.1,0.133333333333333,
0.166666666666667,0.2,0.233333333333333,0.266666666666667,0.3,0.333333333333333,
0.366666666666667,0.4,0.433333333333333,0.466666666666667,0.5,0.533333333333333,
0.566666666666667,0.6,0.633333333333333,0.666666666666667,0.7,0.733333333333333,
0.766666666666667,0.8,0.833333333333333,0.866666666666667,0.9,0.933333333333333,
0.966666666666667,1.),.UNSPECIFIED.)
CURVE()
GEOMETRIC_REPRESENTATION_ITEM()
RATIONAL_B_SPLINE_CURVE((1.,1.,1.,1.,1.,1.,1.,1.,1.,1.,1.,1.,1.,1.,1.,1.,
1.,1.,1.,1.,1.,1.,1.,1.,1.,1.,1.,1.,1.,1.,1.,1.,1.,1.,1.))
REPRESENTATION_ITEM('')
);
#168=(
BOUNDED_CURVE()
B_SPLINE_CURVE(5,(#94496,#94497,#94498,#94499,#94500,#94501,#94502,#94503,
#94504,#94505,#94506,#94507,#94508,#94509,#94510,#94511,#94512,#94513,#94514,
#94515,#94516,#94517,#94518,#94519,#94520,#94521,#94522,#94523,#94524,#94525,
#94526,#94527,#94528,#94529,#94530),.UNSPECIFIED.,.F.,.F.)
B_SPLINE_CURVE_WITH_KNOTS((6,1,1,1,1,1,1,1,1,1,1,1,1,1,1,1,1,1,1,1,1,1,
1,1,1,1,1,1,1,1,6),(-1.,-0.966666666666667,-0.933333333333333,-0.9,-0.866666666666667,
-0.833333333333333,-0.8,-0.766666666666667,-0.733333333333333,-0.7,-0.666666666666667,
-0.633333333333333,-0.6,-0.566666666666667,-0.533333333333333,-0.5,-0.466666666666667,
-0.433333333333333,-0.4,-0.366666666666667,-0.333333333333333,-0.3,-0.266666666666667,
-0.233333333333333,-0.2,-0.166666666666667,-0.133333333333333,-0.1,-0.0666666666666667,
-0.0333333333333333,0.),.UNSPECIFIED.)
CURVE()
GEOMETRIC_REPRESENTATION_ITEM()
RATIONAL_B_SPLINE_CURVE((1.,1.,1.,1.,1.,1.,1.,1.,1.,1.,1.,1.,1.,1.,1.,1.,
1.,1.,1.,1.,1.,1.,1.,1.,1.,1.,1.,1.,1.,1.,1.,1.,1.,1.,1.))
REPRESENTATION_ITEM('')
);
#169=(
BOUNDED_CURVE()
B_SPLINE_CURVE(5,(#94608,#94609,#94610,#94611,#94612,#94613,#94614,#94615,
#94616,#94617,#94618,#94619,#94620,#94621,#94622,#94623,#94624,#94625,#94626,
#94627,#94628,#94629,#94630,#94631,#94632,#94633,#94634,#94635,#94636,#94637,
#94638,#94639,#94640,#94641,#94642),.UNSPECIFIED.,.F.,.F.)
B_SPLINE_CURVE_WITH_KNOTS((6,1,1,1,1,1,1,1,1,1,1,1,1,1,1,1,1,1,1,1,1,1,
1,1,1,1,1,1,1,1,6),(0.,0.0333333333333333,0.0666666666666667,0.1,0.133333333333333,
0.166666666666667,0.2,0.233333333333333,0.266666666666667,0.3,0.333333333333333,
0.366666666666667,0.4,0.433333333333333,0.466666666666667,0.5,0.533333333333333,
0.566666666666667,0.6,0.633333333333333,0.666666666666667,0.7,0.733333333333333,
0.766666666666667,0.8,0.833333333333333,0.866666666666667,0.9,0.933333333333333,
0.966666666666667,1.),.UNSPECIFIED.)
CURVE()
GEOMETRIC_REPRESENTATION_ITEM()
RATIONAL_B_SPLINE_CURVE((1.,1.,1.,1.,1.,1.,1.,1.,1.,1.,1.,1.,1.,1.,1.,1.,
1.,1.,1.,1.,1.,1.,1.,1.,1.,1.,1.,1.,1.,1.,1.,1.,1.,1.,1.))
REPRESENTATION_ITEM('')
);
#170=(
BOUNDED_CURVE()
B_SPLINE_CURVE(5,(#94643,#94644,#94645,#94646,#94647,#94648,#94649,#94650,
#94651,#94652,#94653,#94654,#94655,#94656,#94657,#94658,#94659,#94660,#94661,
#94662,#94663,#94664,#94665,#94666,#94667,#94668,#94669,#94670,#94671,#94672,
#94673,#94674,#94675,#94676,#94677),.UNSPECIFIED.,.F.,.F.)
B_SPLINE_CURVE_WITH_KNOTS((6,1,1,1,1,1,1,1,1,1,1,1,1,1,1,1,1,1,1,1,1,1,
1,1,1,1,1,1,1,1,6),(0.,0.0333333333333333,0.0666666666666667,0.1,0.133333333333333,
0.166666666666667,0.2,0.233333333333333,0.266666666666667,0.3,0.333333333333333,
0.366666666666667,0.4,0.433333333333333,0.466666666666667,0.5,0.533333333333333,
0.566666666666667,0.6,0.633333333333333,0.666666666666667,0.7,0.733333333333333,
0.766666666666667,0.8,0.833333333333333,0.866666666666667,0.9,0.933333333333333,
0.966666666666667,1.),.UNSPECIFIED.)
CURVE()
GEOMETRIC_REPRESENTATION_ITEM()
RATIONAL_B_SPLINE_CURVE((1.,1.,1.,1.,1.,1.,1.,1.,1.,1.,1.,1.,1.,1.,1.,1.,
1.,1.,1.,1.,1.,1.,1.,1.,1.,1.,1.,1.,1.,1.,1.,1.,1.,1.,1.))
REPRESENTATION_ITEM('')
);
#171=(
BOUNDED_CURVE()
B_SPLINE_CURVE(5,(#94762,#94763,#94764,#94765,#94766,#94767,#94768,#94769,
#94770,#94771,#94772,#94773,#94774,#94775,#94776,#94777,#94778,#94779,#94780,
#94781,#94782,#94783,#94784,#94785,#94786,#94787,#94788,#94789,#94790,#94791,
#94792,#94793,#94794,#94795,#94796),.UNSPECIFIED.,.F.,.F.)
B_SPLINE_CURVE_WITH_KNOTS((6,1,1,1,1,1,1,1,1,1,1,1,1,1,1,1,1,1,1,1,1,1,
1,1,1,1,1,1,1,1,6),(0.,0.0333333333333333,0.0666666666666667,0.1,0.133333333333333,
0.166666666666667,0.2,0.233333333333333,0.266666666666667,0.3,0.333333333333333,
0.366666666666667,0.4,0.433333333333333,0.466666666666667,0.5,0.533333333333333,
0.566666666666667,0.6,0.633333333333333,0.666666666666667,0.7,0.733333333333333,
0.766666666666667,0.8,0.833333333333333,0.866666666666667,0.9,0.933333333333333,
0.966666666666667,1.),.UNSPECIFIED.)
CURVE()
GEOMETRIC_REPRESENTATION_ITEM()
RATIONAL_B_SPLINE_CURVE((1.,1.,1.,1.,1.,1.,1.,1.,1.,1.,1.,1.,1.,1.,1.,1.,
1.,1.,1.,1.,1.,1.,1.,1.,1.,1.,1.,1.,1.,1.,1.,1.,1.,1.,1.))
REPRESENTATION_ITEM('')
);
#172=(
BOUNDED_CURVE()
B_SPLINE_CURVE(5,(#94798,#94799,#94800,#94801,#94802,#94803,#94804,#94805,
#94806,#94807,#94808,#94809,#94810,#94811,#94812,#94813,#94814,#94815,#94816,
#94817,#94818,#94819,#94820,#94821,#94822,#94823,#94824,#94825,#94826,#94827,
#94828,#94829,#94830,#94831,#94832),.UNSPECIFIED.,.F.,.F.)
B_SPLINE_CURVE_WITH_KNOTS((6,1,1,1,1,1,1,1,1,1,1,1,1,1,1,1,1,1,1,1,1,1,
1,1,1,1,1,1,1,1,6),(-1.,-0.966666666666667,-0.933333333333333,-0.9,-0.866666666666667,
-0.833333333333333,-0.8,-0.766666666666667,-0.733333333333333,-0.7,-0.666666666666667,
-0.633333333333333,-0.6,-0.566666666666667,-0.533333333333333,-0.5,-0.466666666666667,
-0.433333333333333,-0.4,-0.366666666666667,-0.333333333333333,-0.3,-0.266666666666667,
-0.233333333333333,-0.2,-0.166666666666667,-0.133333333333333,-0.1,-0.0666666666666667,
-0.0333333333333333,0.),.UNSPECIFIED.)
CURVE()
GEOMETRIC_REPRESENTATION_ITEM()
RATIONAL_B_SPLINE_CURVE((1.,1.,1.,1.,1.,1.,1.,1.,1.,1.,1.,1.,1.,1.,1.,1.,
1.,1.,1.,1.,1.,1.,1.,1.,1.,1.,1.,1.,1.,1.,1.,1.,1.,1.,1.))
REPRESENTATION_ITEM('')
);
#173=(
BOUNDED_CURVE()
B_SPLINE_CURVE(5,(#94910,#94911,#94912,#94913,#94914,#94915,#94916,#94917,
#94918,#94919,#94920,#94921,#94922,#94923,#94924,#94925,#94926,#94927,#94928,
#94929,#94930,#94931,#94932,#94933,#94934,#94935,#94936,#94937,#94938,#94939,
#94940,#94941,#94942,#94943,#94944),.UNSPECIFIED.,.F.,.F.)
B_SPLINE_CURVE_WITH_KNOTS((6,1,1,1,1,1,1,1,1,1,1,1,1,1,1,1,1,1,1,1,1,1,
1,1,1,1,1,1,1,1,6),(0.,0.0333333333333333,0.0666666666666667,0.1,0.133333333333333,
0.166666666666667,0.2,0.233333333333333,0.266666666666667,0.3,0.333333333333333,
0.366666666666667,0.4,0.433333333333333,0.466666666666667,0.5,0.533333333333333,
0.566666666666667,0.6,0.633333333333333,0.666666666666667,0.7,0.733333333333333,
0.766666666666667,0.8,0.833333333333333,0.866666666666667,0.9,0.933333333333333,
0.966666666666667,1.),.UNSPECIFIED.)
CURVE()
GEOMETRIC_REPRESENTATION_ITEM()
RATIONAL_B_SPLINE_CURVE((1.,1.,1.,1.,1.,1.,1.,1.,1.,1.,1.,1.,1.,1.,1.,1.,
1.,1.,1.,1.,1.,1.,1.,1.,1.,1.,1.,1.,1.,1.,1.,1.,1.,1.,1.))
REPRESENTATION_ITEM('')
);
#174=(
BOUNDED_CURVE()
B_SPLINE_CURVE(5,(#94945,#94946,#94947,#94948,#94949,#94950,#94951,#94952,
#94953,#94954,#94955,#94956,#94957,#94958,#94959,#94960,#94961,#94962,#94963,
#94964,#94965,#94966,#94967,#94968,#94969,#94970,#94971,#94972,#94973,#94974,
#94975,#94976,#94977,#94978,#94979),.UNSPECIFIED.,.F.,.F.)
B_SPLINE_CURVE_WITH_KNOTS((6,1,1,1,1,1,1,1,1,1,1,1,1,1,1,1,1,1,1,1,1,1,
1,1,1,1,1,1,1,1,6),(0.,0.0333333333333333,0.0666666666666667,0.1,0.133333333333333,
0.166666666666667,0.2,0.233333333333333,0.266666666666667,0.3,0.333333333333333,
0.366666666666667,0.4,0.433333333333333,0.466666666666667,0.5,0.533333333333333,
0.566666666666667,0.6,0.633333333333333,0.666666666666667,0.7,0.733333333333333,
0.766666666666667,0.8,0.833333333333333,0.866666666666667,0.9,0.933333333333333,
0.966666666666667,1.),.UNSPECIFIED.)
CURVE()
GEOMETRIC_REPRESENTATION_ITEM()
RATIONAL_B_SPLINE_CURVE((1.,1.,1.,1.,1.,1.,1.,1.,1.,1.,1.,1.,1.,1.,1.,1.,
1.,1.,1.,1.,1.,1.,1.,1.,1.,1.,1.,1.,1.,1.,1.,1.,1.,1.,1.))
REPRESENTATION_ITEM('')
);
#175=(
BOUNDED_CURVE()
B_SPLINE_CURVE(5,(#95064,#95065,#95066,#95067,#95068,#95069,#95070,#95071,
#95072,#95073,#95074,#95075,#95076,#95077,#95078,#95079,#95080,#95081,#95082,
#95083,#95084,#95085,#95086,#95087,#95088,#95089,#95090,#95091,#95092,#95093,
#95094,#95095,#95096,#95097,#95098),.UNSPECIFIED.,.F.,.F.)
B_SPLINE_CURVE_WITH_KNOTS((6,1,1,1,1,1,1,1,1,1,1,1,1,1,1,1,1,1,1,1,1,1,
1,1,1,1,1,1,1,1,6),(0.,0.0333333333333333,0.0666666666666667,0.1,0.133333333333333,
0.166666666666667,0.2,0.233333333333333,0.266666666666667,0.3,0.333333333333333,
0.366666666666667,0.4,0.433333333333333,0.466666666666667,0.5,0.533333333333333,
0.566666666666667,0.6,0.633333333333333,0.666666666666667,0.7,0.733333333333333,
0.766666666666667,0.8,0.833333333333333,0.866666666666667,0.9,0.933333333333333,
0.966666666666667,1.),.UNSPECIFIED.)
CURVE()
GEOMETRIC_REPRESENTATION_ITEM()
RATIONAL_B_SPLINE_CURVE((1.,1.,1.,1.,1.,1.,1.,1.,1.,1.,1.,1.,1.,1.,1.,1.,
1.,1.,1.,1.,1.,1.,1.,1.,1.,1.,1.,1.,1.,1.,1.,1.,1.,1.,1.))
REPRESENTATION_ITEM('')
);
#176=(
BOUNDED_CURVE()
B_SPLINE_CURVE(5,(#95100,#95101,#95102,#95103,#95104,#95105,#95106,#95107,
#95108,#95109,#95110,#95111,#95112,#95113,#95114,#95115,#95116,#95117,#95118,
#95119,#95120,#95121,#95122,#95123,#95124,#95125,#95126,#95127,#95128,#95129,
#95130,#95131,#95132,#95133,#95134),.UNSPECIFIED.,.F.,.F.)
B_SPLINE_CURVE_WITH_KNOTS((6,1,1,1,1,1,1,1,1,1,1,1,1,1,1,1,1,1,1,1,1,1,
1,1,1,1,1,1,1,1,6),(-1.,-0.966666666666667,-0.933333333333333,-0.9,-0.866666666666667,
-0.833333333333333,-0.8,-0.766666666666667,-0.733333333333333,-0.7,-0.666666666666667,
-0.633333333333333,-0.6,-0.566666666666667,-0.533333333333333,-0.5,-0.466666666666667,
-0.433333333333333,-0.4,-0.366666666666667,-0.333333333333333,-0.3,-0.266666666666667,
-0.233333333333333,-0.2,-0.166666666666667,-0.133333333333333,-0.1,-0.0666666666666667,
-0.0333333333333333,0.),.UNSPECIFIED.)
CURVE()
GEOMETRIC_REPRESENTATION_ITEM()
RATIONAL_B_SPLINE_CURVE((1.,1.,1.,1.,1.,1.,1.,1.,1.,1.,1.,1.,1.,1.,1.,1.,
1.,1.,1.,1.,1.,1.,1.,1.,1.,1.,1.,1.,1.,1.,1.,1.,1.,1.,1.))
REPRESENTATION_ITEM('')
);
#177=(
BOUNDED_CURVE()
B_SPLINE_CURVE(5,(#95212,#95213,#95214,#95215,#95216,#95217,#95218,#95219,
#95220,#95221,#95222,#95223,#95224,#95225,#95226,#95227,#95228,#95229,#95230,
#95231,#95232,#95233,#95234,#95235,#95236,#95237,#95238,#95239,#95240,#95241,
#95242,#95243,#95244,#95245,#95246),.UNSPECIFIED.,.F.,.F.)
B_SPLINE_CURVE_WITH_KNOTS((6,1,1,1,1,1,1,1,1,1,1,1,1,1,1,1,1,1,1,1,1,1,
1,1,1,1,1,1,1,1,6),(0.,0.0333333333333333,0.0666666666666667,0.1,0.133333333333333,
0.166666666666667,0.2,0.233333333333333,0.266666666666667,0.3,0.333333333333333,
0.366666666666667,0.4,0.433333333333333,0.466666666666667,0.5,0.533333333333333,
0.566666666666667,0.6,0.633333333333333,0.666666666666667,0.7,0.733333333333333,
0.766666666666667,0.8,0.833333333333333,0.866666666666667,0.9,0.933333333333333,
0.966666666666667,1.),.UNSPECIFIED.)
CURVE()
GEOMETRIC_REPRESENTATION_ITEM()
RATIONAL_B_SPLINE_CURVE((1.,1.,1.,1.,1.,1.,1.,1.,1.,1.,1.,1.,1.,1.,1.,1.,
1.,1.,1.,1.,1.,1.,1.,1.,1.,1.,1.,1.,1.,1.,1.,1.,1.,1.,1.))
REPRESENTATION_ITEM('')
);
#178=(
BOUNDED_CURVE()
B_SPLINE_CURVE(5,(#95247,#95248,#95249,#95250,#95251,#95252,#95253,#95254,
#95255,#95256,#95257,#95258,#95259,#95260,#95261,#95262,#95263,#95264,#95265,
#95266,#95267,#95268,#95269,#95270,#95271,#95272,#95273,#95274,#95275,#95276,
#95277,#95278,#95279,#95280,#95281),.UNSPECIFIED.,.F.,.F.)
B_SPLINE_CURVE_WITH_KNOTS((6,1,1,1,1,1,1,1,1,1,1,1,1,1,1,1,1,1,1,1,1,1,
1,1,1,1,1,1,1,1,6),(0.,0.0333333333333333,0.0666666666666667,0.1,0.133333333333333,
0.166666666666667,0.2,0.233333333333333,0.266666666666667,0.3,0.333333333333333,
0.366666666666667,0.4,0.433333333333333,0.466666666666667,0.5,0.533333333333333,
0.566666666666667,0.6,0.633333333333333,0.666666666666667,0.7,0.733333333333333,
0.766666666666667,0.8,0.833333333333333,0.866666666666667,0.9,0.933333333333333,
0.966666666666667,1.),.UNSPECIFIED.)
CURVE()
GEOMETRIC_REPRESENTATION_ITEM()
RATIONAL_B_SPLINE_CURVE((1.,1.,1.,1.,1.,1.,1.,1.,1.,1.,1.,1.,1.,1.,1.,1.,
1.,1.,1.,1.,1.,1.,1.,1.,1.,1.,1.,1.,1.,1.,1.,1.,1.,1.,1.))
REPRESENTATION_ITEM('')
);
#179=(
BOUNDED_CURVE()
B_SPLINE_CURVE(5,(#95366,#95367,#95368,#95369,#95370,#95371,#95372,#95373,
#95374,#95375,#95376,#95377,#95378,#95379,#95380,#95381,#95382,#95383,#95384,
#95385,#95386,#95387,#95388,#95389,#95390,#95391,#95392,#95393,#95394,#95395,
#95396,#95397,#95398,#95399,#95400),.UNSPECIFIED.,.F.,.F.)
B_SPLINE_CURVE_WITH_KNOTS((6,1,1,1,1,1,1,1,1,1,1,1,1,1,1,1,1,1,1,1,1,1,
1,1,1,1,1,1,1,1,6),(0.,0.0333333333333333,0.0666666666666667,0.1,0.133333333333333,
0.166666666666667,0.2,0.233333333333333,0.266666666666667,0.3,0.333333333333333,
0.366666666666667,0.4,0.433333333333333,0.466666666666667,0.5,0.533333333333333,
0.566666666666667,0.6,0.633333333333333,0.666666666666667,0.7,0.733333333333333,
0.766666666666667,0.8,0.833333333333333,0.866666666666667,0.9,0.933333333333333,
0.966666666666667,1.),.UNSPECIFIED.)
CURVE()
GEOMETRIC_REPRESENTATION_ITEM()
RATIONAL_B_SPLINE_CURVE((1.,1.,1.,1.,1.,1.,1.,1.,1.,1.,1.,1.,1.,1.,1.,1.,
1.,1.,1.,1.,1.,1.,1.,1.,1.,1.,1.,1.,1.,1.,1.,1.,1.,1.,1.))
REPRESENTATION_ITEM('')
);
#180=(
BOUNDED_CURVE()
B_SPLINE_CURVE(5,(#95402,#95403,#95404,#95405,#95406,#95407,#95408,#95409,
#95410,#95411,#95412,#95413,#95414,#95415,#95416,#95417,#95418,#95419,#95420,
#95421,#95422,#95423,#95424,#95425,#95426,#95427,#95428,#95429,#95430,#95431,
#95432,#95433,#95434,#95435,#95436),.UNSPECIFIED.,.F.,.F.)
B_SPLINE_CURVE_WITH_KNOTS((6,1,1,1,1,1,1,1,1,1,1,1,1,1,1,1,1,1,1,1,1,1,
1,1,1,1,1,1,1,1,6),(-1.,-0.966666666666667,-0.933333333333333,-0.9,-0.866666666666667,
-0.833333333333333,-0.8,-0.766666666666667,-0.733333333333333,-0.7,-0.666666666666667,
-0.633333333333333,-0.6,-0.566666666666667,-0.533333333333333,-0.5,-0.466666666666667,
-0.433333333333333,-0.4,-0.366666666666667,-0.333333333333333,-0.3,-0.266666666666667,
-0.233333333333333,-0.2,-0.166666666666667,-0.133333333333333,-0.1,-0.0666666666666667,
-0.0333333333333333,0.),.UNSPECIFIED.)
CURVE()
GEOMETRIC_REPRESENTATION_ITEM()
RATIONAL_B_SPLINE_CURVE((1.,1.,1.,1.,1.,1.,1.,1.,1.,1.,1.,1.,1.,1.,1.,1.,
1.,1.,1.,1.,1.,1.,1.,1.,1.,1.,1.,1.,1.,1.,1.,1.,1.,1.,1.))
REPRESENTATION_ITEM('')
);
#181=(
BOUNDED_CURVE()
B_SPLINE_CURVE(5,(#95514,#95515,#95516,#95517,#95518,#95519,#95520,#95521,
#95522,#95523,#95524,#95525,#95526,#95527,#95528,#95529,#95530,#95531,#95532,
#95533,#95534,#95535,#95536,#95537,#95538,#95539,#95540,#95541,#95542,#95543,
#95544,#95545,#95546,#95547,#95548),.UNSPECIFIED.,.F.,.F.)
B_SPLINE_CURVE_WITH_KNOTS((6,1,1,1,1,1,1,1,1,1,1,1,1,1,1,1,1,1,1,1,1,1,
1,1,1,1,1,1,1,1,6),(0.,0.0333333333333333,0.0666666666666667,0.1,0.133333333333333,
0.166666666666667,0.2,0.233333333333333,0.266666666666667,0.3,0.333333333333333,
0.366666666666667,0.4,0.433333333333333,0.466666666666667,0.5,0.533333333333333,
0.566666666666667,0.6,0.633333333333333,0.666666666666667,0.7,0.733333333333333,
0.766666666666667,0.8,0.833333333333333,0.866666666666667,0.9,0.933333333333333,
0.966666666666667,1.),.UNSPECIFIED.)
CURVE()
GEOMETRIC_REPRESENTATION_ITEM()
RATIONAL_B_SPLINE_CURVE((1.,1.,1.,1.,1.,1.,1.,1.,1.,1.,1.,1.,1.,1.,1.,1.,
1.,1.,1.,1.,1.,1.,1.,1.,1.,1.,1.,1.,1.,1.,1.,1.,1.,1.,1.))
REPRESENTATION_ITEM('')
);
#182=(
BOUNDED_CURVE()
B_SPLINE_CURVE(5,(#95549,#95550,#95551,#95552,#95553,#95554,#95555,#95556,
#95557,#95558,#95559,#95560,#95561,#95562,#95563,#95564,#95565,#95566,#95567,
#95568,#95569,#95570,#95571,#95572,#95573,#95574,#95575,#95576,#95577,#95578,
#95579,#95580,#95581,#95582,#95583),.UNSPECIFIED.,.F.,.F.)
B_SPLINE_CURVE_WITH_KNOTS((6,1,1,1,1,1,1,1,1,1,1,1,1,1,1,1,1,1,1,1,1,1,
1,1,1,1,1,1,1,1,6),(0.,0.0333333333333333,0.0666666666666667,0.1,0.133333333333333,
0.166666666666667,0.2,0.233333333333333,0.266666666666667,0.3,0.333333333333333,
0.366666666666667,0.4,0.433333333333333,0.466666666666667,0.5,0.533333333333333,
0.566666666666667,0.6,0.633333333333333,0.666666666666667,0.7,0.733333333333333,
0.766666666666667,0.8,0.833333333333333,0.866666666666667,0.9,0.933333333333333,
0.966666666666667,1.),.UNSPECIFIED.)
CURVE()
GEOMETRIC_REPRESENTATION_ITEM()
RATIONAL_B_SPLINE_CURVE((1.,1.,1.,1.,1.,1.,1.,1.,1.,1.,1.,1.,1.,1.,1.,1.,
1.,1.,1.,1.,1.,1.,1.,1.,1.,1.,1.,1.,1.,1.,1.,1.,1.,1.,1.))
REPRESENTATION_ITEM('')
);
#183=(
BOUNDED_CURVE()
B_SPLINE_CURVE(5,(#95668,#95669,#95670,#95671,#95672,#95673,#95674,#95675,
#95676,#95677,#95678,#95679,#95680,#95681,#95682,#95683,#95684,#95685,#95686,
#95687,#95688,#95689,#95690,#95691,#95692,#95693,#95694,#95695,#95696,#95697,
#95698,#95699,#95700,#95701,#95702),.UNSPECIFIED.,.F.,.F.)
B_SPLINE_CURVE_WITH_KNOTS((6,1,1,1,1,1,1,1,1,1,1,1,1,1,1,1,1,1,1,1,1,1,
1,1,1,1,1,1,1,1,6),(0.,0.0333333333333333,0.0666666666666667,0.1,0.133333333333333,
0.166666666666667,0.2,0.233333333333333,0.266666666666667,0.3,0.333333333333333,
0.366666666666667,0.4,0.433333333333333,0.466666666666667,0.5,0.533333333333333,
0.566666666666667,0.6,0.633333333333333,0.666666666666667,0.7,0.733333333333333,
0.766666666666667,0.8,0.833333333333333,0.866666666666667,0.9,0.933333333333333,
0.966666666666667,1.),.UNSPECIFIED.)
CURVE()
GEOMETRIC_REPRESENTATION_ITEM()
RATIONAL_B_SPLINE_CURVE((1.,1.,1.,1.,1.,1.,1.,1.,1.,1.,1.,1.,1.,1.,1.,1.,
1.,1.,1.,1.,1.,1.,1.,1.,1.,1.,1.,1.,1.,1.,1.,1.,1.,1.,1.))
REPRESENTATION_ITEM('')
);
#184=(
BOUNDED_CURVE()
B_SPLINE_CURVE(5,(#95704,#95705,#95706,#95707,#95708,#95709,#95710,#95711,
#95712,#95713,#95714,#95715,#95716,#95717,#95718,#95719,#95720,#95721,#95722,
#95723,#95724,#95725,#95726,#95727,#95728,#95729,#95730,#95731,#95732,#95733,
#95734,#95735,#95736,#95737,#95738),.UNSPECIFIED.,.F.,.F.)
B_SPLINE_CURVE_WITH_KNOTS((6,1,1,1,1,1,1,1,1,1,1,1,1,1,1,1,1,1,1,1,1,1,
1,1,1,1,1,1,1,1,6),(-1.,-0.966666666666667,-0.933333333333333,-0.9,-0.866666666666667,
-0.833333333333333,-0.8,-0.766666666666667,-0.733333333333333,-0.7,-0.666666666666667,
-0.633333333333333,-0.6,-0.566666666666667,-0.533333333333333,-0.5,-0.466666666666667,
-0.433333333333333,-0.4,-0.366666666666667,-0.333333333333333,-0.3,-0.266666666666667,
-0.233333333333333,-0.2,-0.166666666666667,-0.133333333333333,-0.1,-0.0666666666666667,
-0.0333333333333333,0.),.UNSPECIFIED.)
CURVE()
GEOMETRIC_REPRESENTATION_ITEM()
RATIONAL_B_SPLINE_CURVE((1.,1.,1.,1.,1.,1.,1.,1.,1.,1.,1.,1.,1.,1.,1.,1.,
1.,1.,1.,1.,1.,1.,1.,1.,1.,1.,1.,1.,1.,1.,1.,1.,1.,1.,1.))
REPRESENTATION_ITEM('')
);
#185=(
BOUNDED_CURVE()
B_SPLINE_CURVE(5,(#95816,#95817,#95818,#95819,#95820,#95821,#95822,#95823,
#95824,#95825,#95826,#95827,#95828,#95829,#95830,#95831,#95832,#95833,#95834,
#95835,#95836,#95837,#95838,#95839,#95840,#95841,#95842,#95843,#95844,#95845,
#95846,#95847,#95848,#95849,#95850),.UNSPECIFIED.,.F.,.F.)
B_SPLINE_CURVE_WITH_KNOTS((6,1,1,1,1,1,1,1,1,1,1,1,1,1,1,1,1,1,1,1,1,1,
1,1,1,1,1,1,1,1,6),(0.,0.0333333333333333,0.0666666666666667,0.1,0.133333333333333,
0.166666666666667,0.2,0.233333333333333,0.266666666666667,0.3,0.333333333333333,
0.366666666666667,0.4,0.433333333333333,0.466666666666667,0.5,0.533333333333333,
0.566666666666667,0.6,0.633333333333333,0.666666666666667,0.7,0.733333333333333,
0.766666666666667,0.8,0.833333333333333,0.866666666666667,0.9,0.933333333333333,
0.966666666666667,1.),.UNSPECIFIED.)
CURVE()
GEOMETRIC_REPRESENTATION_ITEM()
RATIONAL_B_SPLINE_CURVE((1.,1.,1.,1.,1.,1.,1.,1.,1.,1.,1.,1.,1.,1.,1.,1.,
1.,1.,1.,1.,1.,1.,1.,1.,1.,1.,1.,1.,1.,1.,1.,1.,1.,1.,1.))
REPRESENTATION_ITEM('')
);
#186=(
BOUNDED_CURVE()
B_SPLINE_CURVE(5,(#95851,#95852,#95853,#95854,#95855,#95856,#95857,#95858,
#95859,#95860,#95861,#95862,#95863,#95864,#95865,#95866,#95867,#95868,#95869,
#95870,#95871,#95872,#95873,#95874,#95875,#95876,#95877,#95878,#95879,#95880,
#95881,#95882,#95883,#95884,#95885),.UNSPECIFIED.,.F.,.F.)
B_SPLINE_CURVE_WITH_KNOTS((6,1,1,1,1,1,1,1,1,1,1,1,1,1,1,1,1,1,1,1,1,1,
1,1,1,1,1,1,1,1,6),(0.,0.0333333333333333,0.0666666666666667,0.1,0.133333333333333,
0.166666666666667,0.2,0.233333333333333,0.266666666666667,0.3,0.333333333333333,
0.366666666666667,0.4,0.433333333333333,0.466666666666667,0.5,0.533333333333333,
0.566666666666667,0.6,0.633333333333333,0.666666666666667,0.7,0.733333333333333,
0.766666666666667,0.8,0.833333333333333,0.866666666666667,0.9,0.933333333333333,
0.966666666666667,1.),.UNSPECIFIED.)
CURVE()
GEOMETRIC_REPRESENTATION_ITEM()
RATIONAL_B_SPLINE_CURVE((1.,1.,1.,1.,1.,1.,1.,1.,1.,1.,1.,1.,1.,1.,1.,1.,
1.,1.,1.,1.,1.,1.,1.,1.,1.,1.,1.,1.,1.,1.,1.,1.,1.,1.,1.))
REPRESENTATION_ITEM('')
);
#187=(
BOUNDED_CURVE()
B_SPLINE_CURVE(5,(#95970,#95971,#95972,#95973,#95974,#95975,#95976,#95977,
#95978,#95979,#95980,#95981,#95982,#95983,#95984,#95985,#95986,#95987,#95988,
#95989,#95990,#95991,#95992,#95993,#95994,#95995,#95996,#95997,#95998,#95999,
#96000,#96001,#96002,#96003,#96004),.UNSPECIFIED.,.F.,.F.)
B_SPLINE_CURVE_WITH_KNOTS((6,1,1,1,1,1,1,1,1,1,1,1,1,1,1,1,1,1,1,1,1,1,
1,1,1,1,1,1,1,1,6),(0.,0.0333333333333333,0.0666666666666667,0.1,0.133333333333333,
0.166666666666667,0.2,0.233333333333333,0.266666666666667,0.3,0.333333333333333,
0.366666666666667,0.4,0.433333333333333,0.466666666666667,0.5,0.533333333333333,
0.566666666666667,0.6,0.633333333333333,0.666666666666667,0.7,0.733333333333333,
0.766666666666667,0.8,0.833333333333333,0.866666666666667,0.9,0.933333333333333,
0.966666666666667,1.),.UNSPECIFIED.)
CURVE()
GEOMETRIC_REPRESENTATION_ITEM()
RATIONAL_B_SPLINE_CURVE((1.,1.,1.,1.,1.,1.,1.,1.,1.,1.,1.,1.,1.,1.,1.,1.,
1.,1.,1.,1.,1.,1.,1.,1.,1.,1.,1.,1.,1.,1.,1.,1.,1.,1.,1.))
REPRESENTATION_ITEM('')
);
#188=(
BOUNDED_CURVE()
B_SPLINE_CURVE(5,(#96006,#96007,#96008,#96009,#96010,#96011,#96012,#96013,
#96014,#96015,#96016,#96017,#96018,#96019,#96020,#96021,#96022,#96023,#96024,
#96025,#96026,#96027,#96028,#96029,#96030,#96031,#96032,#96033,#96034,#96035,
#96036,#96037,#96038,#96039,#96040),.UNSPECIFIED.,.F.,.F.)
B_SPLINE_CURVE_WITH_KNOTS((6,1,1,1,1,1,1,1,1,1,1,1,1,1,1,1,1,1,1,1,1,1,
1,1,1,1,1,1,1,1,6),(-1.,-0.966666666666667,-0.933333333333333,-0.9,-0.866666666666667,
-0.833333333333333,-0.8,-0.766666666666667,-0.733333333333333,-0.7,-0.666666666666667,
-0.633333333333333,-0.6,-0.566666666666667,-0.533333333333333,-0.5,-0.466666666666667,
-0.433333333333333,-0.4,-0.366666666666667,-0.333333333333333,-0.3,-0.266666666666667,
-0.233333333333333,-0.2,-0.166666666666667,-0.133333333333333,-0.1,-0.0666666666666667,
-0.0333333333333333,0.),.UNSPECIFIED.)
CURVE()
GEOMETRIC_REPRESENTATION_ITEM()
RATIONAL_B_SPLINE_CURVE((1.,1.,1.,1.,1.,1.,1.,1.,1.,1.,1.,1.,1.,1.,1.,1.,
1.,1.,1.,1.,1.,1.,1.,1.,1.,1.,1.,1.,1.,1.,1.,1.,1.,1.,1.))
REPRESENTATION_ITEM('')
);
#189=(
BOUNDED_CURVE()
B_SPLINE_CURVE(5,(#96118,#96119,#96120,#96121,#96122,#96123,#96124,#96125,
#96126,#96127,#96128,#96129,#96130,#96131,#96132,#96133,#96134,#96135,#96136,
#96137,#96138,#96139,#96140,#96141,#96142,#96143,#96144,#96145,#96146,#96147,
#96148,#96149,#96150,#96151,#96152),.UNSPECIFIED.,.F.,.F.)
B_SPLINE_CURVE_WITH_KNOTS((6,1,1,1,1,1,1,1,1,1,1,1,1,1,1,1,1,1,1,1,1,1,
1,1,1,1,1,1,1,1,6),(0.,0.0333333333333333,0.0666666666666667,0.1,0.133333333333333,
0.166666666666667,0.2,0.233333333333333,0.266666666666667,0.3,0.333333333333333,
0.366666666666667,0.4,0.433333333333333,0.466666666666667,0.5,0.533333333333333,
0.566666666666667,0.6,0.633333333333333,0.666666666666667,0.7,0.733333333333333,
0.766666666666667,0.8,0.833333333333333,0.866666666666667,0.9,0.933333333333333,
0.966666666666667,1.),.UNSPECIFIED.)
CURVE()
GEOMETRIC_REPRESENTATION_ITEM()
RATIONAL_B_SPLINE_CURVE((1.,1.,1.,1.,1.,1.,1.,1.,1.,1.,1.,1.,1.,1.,1.,1.,
1.,1.,1.,1.,1.,1.,1.,1.,1.,1.,1.,1.,1.,1.,1.,1.,1.,1.,1.))
REPRESENTATION_ITEM('')
);
#190=(
BOUNDED_CURVE()
B_SPLINE_CURVE(5,(#96153,#96154,#96155,#96156,#96157,#96158,#96159,#96160,
#96161,#96162,#96163,#96164,#96165,#96166,#96167,#96168,#96169,#96170,#96171,
#96172,#96173,#96174,#96175,#96176,#96177,#96178,#96179,#96180,#96181,#96182,
#96183,#96184,#96185,#96186,#96187),.UNSPECIFIED.,.F.,.F.)
B_SPLINE_CURVE_WITH_KNOTS((6,1,1,1,1,1,1,1,1,1,1,1,1,1,1,1,1,1,1,1,1,1,
1,1,1,1,1,1,1,1,6),(0.,0.0333333333333333,0.0666666666666667,0.1,0.133333333333333,
0.166666666666667,0.2,0.233333333333333,0.266666666666667,0.3,0.333333333333333,
0.366666666666667,0.4,0.433333333333333,0.466666666666667,0.5,0.533333333333333,
0.566666666666667,0.6,0.633333333333333,0.666666666666667,0.7,0.733333333333333,
0.766666666666667,0.8,0.833333333333333,0.866666666666667,0.9,0.933333333333333,
0.966666666666667,1.),.UNSPECIFIED.)
CURVE()
GEOMETRIC_REPRESENTATION_ITEM()
RATIONAL_B_SPLINE_CURVE((1.,1.,1.,1.,1.,1.,1.,1.,1.,1.,1.,1.,1.,1.,1.,1.,
1.,1.,1.,1.,1.,1.,1.,1.,1.,1.,1.,1.,1.,1.,1.,1.,1.,1.,1.))
REPRESENTATION_ITEM('')
);
#191=(
BOUNDED_CURVE()
B_SPLINE_CURVE(5,(#96272,#96273,#96274,#96275,#96276,#96277,#96278,#96279,
#96280,#96281,#96282,#96283,#96284,#96285,#96286,#96287,#96288,#96289,#96290,
#96291,#96292,#96293,#96294,#96295,#96296,#96297,#96298,#96299,#96300,#96301,
#96302,#96303,#96304,#96305,#96306),.UNSPECIFIED.,.F.,.F.)
B_SPLINE_CURVE_WITH_KNOTS((6,1,1,1,1,1,1,1,1,1,1,1,1,1,1,1,1,1,1,1,1,1,
1,1,1,1,1,1,1,1,6),(0.,0.0333333333333333,0.0666666666666667,0.1,0.133333333333333,
0.166666666666667,0.2,0.233333333333333,0.266666666666667,0.3,0.333333333333333,
0.366666666666667,0.4,0.433333333333333,0.466666666666667,0.5,0.533333333333333,
0.566666666666667,0.6,0.633333333333333,0.666666666666667,0.7,0.733333333333333,
0.766666666666667,0.8,0.833333333333333,0.866666666666667,0.9,0.933333333333333,
0.966666666666667,1.),.UNSPECIFIED.)
CURVE()
GEOMETRIC_REPRESENTATION_ITEM()
RATIONAL_B_SPLINE_CURVE((1.,1.,1.,1.,1.,1.,1.,1.,1.,1.,1.,1.,1.,1.,1.,1.,
1.,1.,1.,1.,1.,1.,1.,1.,1.,1.,1.,1.,1.,1.,1.,1.,1.,1.,1.))
REPRESENTATION_ITEM('')
);
#192=(
BOUNDED_CURVE()
B_SPLINE_CURVE(5,(#96308,#96309,#96310,#96311,#96312,#96313,#96314,#96315,
#96316,#96317,#96318,#96319,#96320,#96321,#96322,#96323,#96324,#96325,#96326,
#96327,#96328,#96329,#96330,#96331,#96332,#96333,#96334,#96335,#96336,#96337,
#96338,#96339,#96340,#96341,#96342),.UNSPECIFIED.,.F.,.F.)
B_SPLINE_CURVE_WITH_KNOTS((6,1,1,1,1,1,1,1,1,1,1,1,1,1,1,1,1,1,1,1,1,1,
1,1,1,1,1,1,1,1,6),(-1.,-0.966666666666667,-0.933333333333333,-0.9,-0.866666666666667,
-0.833333333333333,-0.8,-0.766666666666667,-0.733333333333333,-0.7,-0.666666666666667,
-0.633333333333333,-0.6,-0.566666666666667,-0.533333333333333,-0.5,-0.466666666666667,
-0.433333333333333,-0.4,-0.366666666666667,-0.333333333333333,-0.3,-0.266666666666667,
-0.233333333333333,-0.2,-0.166666666666667,-0.133333333333333,-0.1,-0.0666666666666667,
-0.0333333333333333,0.),.UNSPECIFIED.)
CURVE()
GEOMETRIC_REPRESENTATION_ITEM()
RATIONAL_B_SPLINE_CURVE((1.,1.,1.,1.,1.,1.,1.,1.,1.,1.,1.,1.,1.,1.,1.,1.,
1.,1.,1.,1.,1.,1.,1.,1.,1.,1.,1.,1.,1.,1.,1.,1.,1.,1.,1.))
REPRESENTATION_ITEM('')
);
#193=(
BOUNDED_CURVE()
B_SPLINE_CURVE(5,(#96420,#96421,#96422,#96423,#96424,#96425,#96426,#96427,
#96428,#96429,#96430,#96431,#96432,#96433,#96434,#96435,#96436,#96437,#96438,
#96439,#96440,#96441,#96442,#96443,#96444,#96445,#96446,#96447,#96448,#96449,
#96450,#96451,#96452,#96453,#96454),.UNSPECIFIED.,.F.,.F.)
B_SPLINE_CURVE_WITH_KNOTS((6,1,1,1,1,1,1,1,1,1,1,1,1,1,1,1,1,1,1,1,1,1,
1,1,1,1,1,1,1,1,6),(0.,0.0333333333333333,0.0666666666666667,0.1,0.133333333333333,
0.166666666666667,0.2,0.233333333333333,0.266666666666667,0.3,0.333333333333333,
0.366666666666667,0.4,0.433333333333333,0.466666666666667,0.5,0.533333333333333,
0.566666666666667,0.6,0.633333333333333,0.666666666666667,0.7,0.733333333333333,
0.766666666666667,0.8,0.833333333333333,0.866666666666667,0.9,0.933333333333333,
0.966666666666667,1.),.UNSPECIFIED.)
CURVE()
GEOMETRIC_REPRESENTATION_ITEM()
RATIONAL_B_SPLINE_CURVE((1.,1.,1.,1.,1.,1.,1.,1.,1.,1.,1.,1.,1.,1.,1.,1.,
1.,1.,1.,1.,1.,1.,1.,1.,1.,1.,1.,1.,1.,1.,1.,1.,1.,1.,1.))
REPRESENTATION_ITEM('')
);
#194=(
BOUNDED_CURVE()
B_SPLINE_CURVE(5,(#96455,#96456,#96457,#96458,#96459,#96460,#96461,#96462,
#96463,#96464,#96465,#96466,#96467,#96468,#96469,#96470,#96471,#96472,#96473,
#96474,#96475,#96476,#96477,#96478,#96479,#96480,#96481,#96482,#96483,#96484,
#96485,#96486,#96487,#96488,#96489),.UNSPECIFIED.,.F.,.F.)
B_SPLINE_CURVE_WITH_KNOTS((6,1,1,1,1,1,1,1,1,1,1,1,1,1,1,1,1,1,1,1,1,1,
1,1,1,1,1,1,1,1,6),(0.,0.0333333333333333,0.0666666666666667,0.1,0.133333333333333,
0.166666666666667,0.2,0.233333333333333,0.266666666666667,0.3,0.333333333333333,
0.366666666666667,0.4,0.433333333333333,0.466666666666667,0.5,0.533333333333333,
0.566666666666667,0.6,0.633333333333333,0.666666666666667,0.7,0.733333333333333,
0.766666666666667,0.8,0.833333333333333,0.866666666666667,0.9,0.933333333333333,
0.966666666666667,1.),.UNSPECIFIED.)
CURVE()
GEOMETRIC_REPRESENTATION_ITEM()
RATIONAL_B_SPLINE_CURVE((1.,1.,1.,1.,1.,1.,1.,1.,1.,1.,1.,1.,1.,1.,1.,1.,
1.,1.,1.,1.,1.,1.,1.,1.,1.,1.,1.,1.,1.,1.,1.,1.,1.,1.,1.))
REPRESENTATION_ITEM('')
);
#195=(
BOUNDED_CURVE()
B_SPLINE_CURVE(5,(#96574,#96575,#96576,#96577,#96578,#96579,#96580,#96581,
#96582,#96583,#96584,#96585,#96586,#96587,#96588,#96589,#96590,#96591,#96592,
#96593,#96594,#96595,#96596,#96597,#96598,#96599,#96600,#96601,#96602,#96603,
#96604,#96605,#96606,#96607,#96608),.UNSPECIFIED.,.F.,.F.)
B_SPLINE_CURVE_WITH_KNOTS((6,1,1,1,1,1,1,1,1,1,1,1,1,1,1,1,1,1,1,1,1,1,
1,1,1,1,1,1,1,1,6),(0.,0.0333333333333333,0.0666666666666667,0.1,0.133333333333333,
0.166666666666667,0.2,0.233333333333333,0.266666666666667,0.3,0.333333333333333,
0.366666666666667,0.4,0.433333333333333,0.466666666666667,0.5,0.533333333333333,
0.566666666666667,0.6,0.633333333333333,0.666666666666667,0.7,0.733333333333333,
0.766666666666667,0.8,0.833333333333333,0.866666666666667,0.9,0.933333333333333,
0.966666666666667,1.),.UNSPECIFIED.)
CURVE()
GEOMETRIC_REPRESENTATION_ITEM()
RATIONAL_B_SPLINE_CURVE((1.,1.,1.,1.,1.,1.,1.,1.,1.,1.,1.,1.,1.,1.,1.,1.,
1.,1.,1.,1.,1.,1.,1.,1.,1.,1.,1.,1.,1.,1.,1.,1.,1.,1.,1.))
REPRESENTATION_ITEM('')
);
#196=(
BOUNDED_CURVE()
B_SPLINE_CURVE(5,(#96610,#96611,#96612,#96613,#96614,#96615,#96616,#96617,
#96618,#96619,#96620,#96621,#96622,#96623,#96624,#96625,#96626,#96627,#96628,
#96629,#96630,#96631,#96632,#96633,#96634,#96635,#96636,#96637,#96638,#96639,
#96640,#96641,#96642,#96643,#96644),.UNSPECIFIED.,.F.,.F.)
B_SPLINE_CURVE_WITH_KNOTS((6,1,1,1,1,1,1,1,1,1,1,1,1,1,1,1,1,1,1,1,1,1,
1,1,1,1,1,1,1,1,6),(-1.,-0.966666666666667,-0.933333333333333,-0.9,-0.866666666666667,
-0.833333333333333,-0.8,-0.766666666666667,-0.733333333333333,-0.7,-0.666666666666667,
-0.633333333333333,-0.6,-0.566666666666667,-0.533333333333333,-0.5,-0.466666666666667,
-0.433333333333333,-0.4,-0.366666666666667,-0.333333333333333,-0.3,-0.266666666666667,
-0.233333333333333,-0.2,-0.166666666666667,-0.133333333333333,-0.1,-0.0666666666666667,
-0.0333333333333333,0.),.UNSPECIFIED.)
CURVE()
GEOMETRIC_REPRESENTATION_ITEM()
RATIONAL_B_SPLINE_CURVE((1.,1.,1.,1.,1.,1.,1.,1.,1.,1.,1.,1.,1.,1.,1.,1.,
1.,1.,1.,1.,1.,1.,1.,1.,1.,1.,1.,1.,1.,1.,1.,1.,1.,1.,1.))
REPRESENTATION_ITEM('')
);
#197=(
BOUNDED_CURVE()
B_SPLINE_CURVE(5,(#96722,#96723,#96724,#96725,#96726,#96727,#96728,#96729,
#96730,#96731,#96732,#96733,#96734,#96735,#96736,#96737,#96738,#96739,#96740,
#96741,#96742,#96743,#96744,#96745,#96746,#96747,#96748,#96749,#96750,#96751,
#96752,#96753,#96754,#96755,#96756),.UNSPECIFIED.,.F.,.F.)
B_SPLINE_CURVE_WITH_KNOTS((6,1,1,1,1,1,1,1,1,1,1,1,1,1,1,1,1,1,1,1,1,1,
1,1,1,1,1,1,1,1,6),(0.,0.0333333333333333,0.0666666666666667,0.1,0.133333333333333,
0.166666666666667,0.2,0.233333333333333,0.266666666666667,0.3,0.333333333333333,
0.366666666666667,0.4,0.433333333333333,0.466666666666667,0.5,0.533333333333333,
0.566666666666667,0.6,0.633333333333333,0.666666666666667,0.7,0.733333333333333,
0.766666666666667,0.8,0.833333333333333,0.866666666666667,0.9,0.933333333333333,
0.966666666666667,1.),.UNSPECIFIED.)
CURVE()
GEOMETRIC_REPRESENTATION_ITEM()
RATIONAL_B_SPLINE_CURVE((1.,1.,1.,1.,1.,1.,1.,1.,1.,1.,1.,1.,1.,1.,1.,1.,
1.,1.,1.,1.,1.,1.,1.,1.,1.,1.,1.,1.,1.,1.,1.,1.,1.,1.,1.))
REPRESENTATION_ITEM('')
);
#198=(
BOUNDED_CURVE()
B_SPLINE_CURVE(5,(#96757,#96758,#96759,#96760,#96761,#96762,#96763,#96764,
#96765,#96766,#96767,#96768,#96769,#96770,#96771,#96772,#96773,#96774,#96775,
#96776,#96777,#96778,#96779,#96780,#96781,#96782,#96783,#96784,#96785,#96786,
#96787,#96788,#96789,#96790,#96791),.UNSPECIFIED.,.F.,.F.)
B_SPLINE_CURVE_WITH_KNOTS((6,1,1,1,1,1,1,1,1,1,1,1,1,1,1,1,1,1,1,1,1,1,
1,1,1,1,1,1,1,1,6),(0.,0.0333333333333333,0.0666666666666667,0.1,0.133333333333333,
0.166666666666667,0.2,0.233333333333333,0.266666666666667,0.3,0.333333333333333,
0.366666666666667,0.4,0.433333333333333,0.466666666666667,0.5,0.533333333333333,
0.566666666666667,0.6,0.633333333333333,0.666666666666667,0.7,0.733333333333333,
0.766666666666667,0.8,0.833333333333333,0.866666666666667,0.9,0.933333333333333,
0.966666666666667,1.),.UNSPECIFIED.)
CURVE()
GEOMETRIC_REPRESENTATION_ITEM()
RATIONAL_B_SPLINE_CURVE((1.,1.,1.,1.,1.,1.,1.,1.,1.,1.,1.,1.,1.,1.,1.,1.,
1.,1.,1.,1.,1.,1.,1.,1.,1.,1.,1.,1.,1.,1.,1.,1.,1.,1.,1.))
REPRESENTATION_ITEM('')
);
#199=(
BOUNDED_CURVE()
B_SPLINE_CURVE(5,(#96876,#96877,#96878,#96879,#96880,#96881,#96882,#96883,
#96884,#96885,#96886,#96887,#96888,#96889,#96890,#96891,#96892,#96893,#96894,
#96895,#96896,#96897,#96898,#96899,#96900,#96901,#96902,#96903,#96904,#96905,
#96906,#96907,#96908,#96909,#96910),.UNSPECIFIED.,.F.,.F.)
B_SPLINE_CURVE_WITH_KNOTS((6,1,1,1,1,1,1,1,1,1,1,1,1,1,1,1,1,1,1,1,1,1,
1,1,1,1,1,1,1,1,6),(0.,0.0333333333333333,0.0666666666666667,0.1,0.133333333333333,
0.166666666666667,0.2,0.233333333333333,0.266666666666667,0.3,0.333333333333333,
0.366666666666667,0.4,0.433333333333333,0.466666666666667,0.5,0.533333333333333,
0.566666666666667,0.6,0.633333333333333,0.666666666666667,0.7,0.733333333333333,
0.766666666666667,0.8,0.833333333333333,0.866666666666667,0.9,0.933333333333333,
0.966666666666667,1.),.UNSPECIFIED.)
CURVE()
GEOMETRIC_REPRESENTATION_ITEM()
RATIONAL_B_SPLINE_CURVE((1.,1.,1.,1.,1.,1.,1.,1.,1.,1.,1.,1.,1.,1.,1.,1.,
1.,1.,1.,1.,1.,1.,1.,1.,1.,1.,1.,1.,1.,1.,1.,1.,1.,1.,1.))
REPRESENTATION_ITEM('')
);
#200=(
BOUNDED_CURVE()
B_SPLINE_CURVE(5,(#96912,#96913,#96914,#96915,#96916,#96917,#96918,#96919,
#96920,#96921,#96922,#96923,#96924,#96925,#96926,#96927,#96928,#96929,#96930,
#96931,#96932,#96933,#96934,#96935,#96936,#96937,#96938,#96939,#96940,#96941,
#96942,#96943,#96944,#96945,#96946),.UNSPECIFIED.,.F.,.F.)
B_SPLINE_CURVE_WITH_KNOTS((6,1,1,1,1,1,1,1,1,1,1,1,1,1,1,1,1,1,1,1,1,1,
1,1,1,1,1,1,1,1,6),(-1.,-0.966666666666667,-0.933333333333333,-0.9,-0.866666666666667,
-0.833333333333333,-0.8,-0.766666666666667,-0.733333333333333,-0.7,-0.666666666666667,
-0.633333333333333,-0.6,-0.566666666666667,-0.533333333333333,-0.5,-0.466666666666667,
-0.433333333333333,-0.4,-0.366666666666667,-0.333333333333333,-0.3,-0.266666666666667,
-0.233333333333333,-0.2,-0.166666666666667,-0.133333333333333,-0.1,-0.0666666666666667,
-0.0333333333333333,0.),.UNSPECIFIED.)
CURVE()
GEOMETRIC_REPRESENTATION_ITEM()
RATIONAL_B_SPLINE_CURVE((1.,1.,1.,1.,1.,1.,1.,1.,1.,1.,1.,1.,1.,1.,1.,1.,
1.,1.,1.,1.,1.,1.,1.,1.,1.,1.,1.,1.,1.,1.,1.,1.,1.,1.,1.))
REPRESENTATION_ITEM('')
);
#201=(
BOUNDED_CURVE()
B_SPLINE_CURVE(5,(#97024,#97025,#97026,#97027,#97028,#97029,#97030,#97031,
#97032,#97033,#97034,#97035,#97036,#97037,#97038,#97039,#97040,#97041,#97042,
#97043,#97044,#97045,#97046,#97047,#97048,#97049,#97050,#97051,#97052,#97053,
#97054,#97055,#97056,#97057,#97058),.UNSPECIFIED.,.F.,.F.)
B_SPLINE_CURVE_WITH_KNOTS((6,1,1,1,1,1,1,1,1,1,1,1,1,1,1,1,1,1,1,1,1,1,
1,1,1,1,1,1,1,1,6),(0.,0.0333333333333333,0.0666666666666667,0.1,0.133333333333333,
0.166666666666667,0.2,0.233333333333333,0.266666666666667,0.3,0.333333333333333,
0.366666666666667,0.4,0.433333333333333,0.466666666666667,0.5,0.533333333333333,
0.566666666666667,0.6,0.633333333333333,0.666666666666667,0.7,0.733333333333333,
0.766666666666667,0.8,0.833333333333333,0.866666666666667,0.9,0.933333333333333,
0.966666666666667,1.),.UNSPECIFIED.)
CURVE()
GEOMETRIC_REPRESENTATION_ITEM()
RATIONAL_B_SPLINE_CURVE((1.,1.,1.,1.,1.,1.,1.,1.,1.,1.,1.,1.,1.,1.,1.,1.,
1.,1.,1.,1.,1.,1.,1.,1.,1.,1.,1.,1.,1.,1.,1.,1.,1.,1.,1.))
REPRESENTATION_ITEM('')
);
#202=(
BOUNDED_CURVE()
B_SPLINE_CURVE(5,(#97059,#97060,#97061,#97062,#97063,#97064,#97065,#97066,
#97067,#97068,#97069,#97070,#97071,#97072,#97073,#97074,#97075,#97076,#97077,
#97078,#97079,#97080,#97081,#97082,#97083,#97084,#97085,#97086,#97087,#97088,
#97089,#97090,#97091,#97092,#97093),.UNSPECIFIED.,.F.,.F.)
B_SPLINE_CURVE_WITH_KNOTS((6,1,1,1,1,1,1,1,1,1,1,1,1,1,1,1,1,1,1,1,1,1,
1,1,1,1,1,1,1,1,6),(0.,0.0333333333333333,0.0666666666666667,0.1,0.133333333333333,
0.166666666666667,0.2,0.233333333333333,0.266666666666667,0.3,0.333333333333333,
0.366666666666667,0.4,0.433333333333333,0.466666666666667,0.5,0.533333333333333,
0.566666666666667,0.6,0.633333333333333,0.666666666666667,0.7,0.733333333333333,
0.766666666666667,0.8,0.833333333333333,0.866666666666667,0.9,0.933333333333333,
0.966666666666667,1.),.UNSPECIFIED.)
CURVE()
GEOMETRIC_REPRESENTATION_ITEM()
RATIONAL_B_SPLINE_CURVE((1.,1.,1.,1.,1.,1.,1.,1.,1.,1.,1.,1.,1.,1.,1.,1.,
1.,1.,1.,1.,1.,1.,1.,1.,1.,1.,1.,1.,1.,1.,1.,1.,1.,1.,1.))
REPRESENTATION_ITEM('')
);
#203=(
BOUNDED_CURVE()
B_SPLINE_CURVE(5,(#97178,#97179,#97180,#97181,#97182,#97183,#97184,#97185,
#97186,#97187,#97188,#97189,#97190,#97191,#97192,#97193,#97194,#97195,#97196,
#97197,#97198,#97199,#97200,#97201,#97202,#97203,#97204,#97205,#97206,#97207,
#97208,#97209,#97210,#97211,#97212),.UNSPECIFIED.,.F.,.F.)
B_SPLINE_CURVE_WITH_KNOTS((6,1,1,1,1,1,1,1,1,1,1,1,1,1,1,1,1,1,1,1,1,1,
1,1,1,1,1,1,1,1,6),(0.,0.0333333333333333,0.0666666666666667,0.1,0.133333333333333,
0.166666666666667,0.2,0.233333333333333,0.266666666666667,0.3,0.333333333333333,
0.366666666666667,0.4,0.433333333333333,0.466666666666667,0.5,0.533333333333333,
0.566666666666667,0.6,0.633333333333333,0.666666666666667,0.7,0.733333333333333,
0.766666666666667,0.8,0.833333333333333,0.866666666666667,0.9,0.933333333333333,
0.966666666666667,1.),.UNSPECIFIED.)
CURVE()
GEOMETRIC_REPRESENTATION_ITEM()
RATIONAL_B_SPLINE_CURVE((1.,1.,1.,1.,1.,1.,1.,1.,1.,1.,1.,1.,1.,1.,1.,1.,
1.,1.,1.,1.,1.,1.,1.,1.,1.,1.,1.,1.,1.,1.,1.,1.,1.,1.,1.))
REPRESENTATION_ITEM('')
);
#204=(
BOUNDED_CURVE()
B_SPLINE_CURVE(5,(#97214,#97215,#97216,#97217,#97218,#97219,#97220,#97221,
#97222,#97223,#97224,#97225,#97226,#97227,#97228,#97229,#97230,#97231,#97232,
#97233,#97234,#97235,#97236,#97237,#97238,#97239,#97240,#97241,#97242,#97243,
#97244,#97245,#97246,#97247,#97248),.UNSPECIFIED.,.F.,.F.)
B_SPLINE_CURVE_WITH_KNOTS((6,1,1,1,1,1,1,1,1,1,1,1,1,1,1,1,1,1,1,1,1,1,
1,1,1,1,1,1,1,1,6),(-1.,-0.966666666666667,-0.933333333333333,-0.9,-0.866666666666667,
-0.833333333333333,-0.8,-0.766666666666667,-0.733333333333333,-0.7,-0.666666666666667,
-0.633333333333333,-0.6,-0.566666666666667,-0.533333333333333,-0.5,-0.466666666666667,
-0.433333333333333,-0.4,-0.366666666666667,-0.333333333333333,-0.3,-0.266666666666667,
-0.233333333333333,-0.2,-0.166666666666667,-0.133333333333333,-0.1,-0.0666666666666667,
-0.0333333333333333,0.),.UNSPECIFIED.)
CURVE()
GEOMETRIC_REPRESENTATION_ITEM()
RATIONAL_B_SPLINE_CURVE((1.,1.,1.,1.,1.,1.,1.,1.,1.,1.,1.,1.,1.,1.,1.,1.,
1.,1.,1.,1.,1.,1.,1.,1.,1.,1.,1.,1.,1.,1.,1.,1.,1.,1.,1.))
REPRESENTATION_ITEM('')
);
#205=(
BOUNDED_CURVE()
B_SPLINE_CURVE(5,(#97326,#97327,#97328,#97329,#97330,#97331,#97332,#97333,
#97334,#97335,#97336,#97337,#97338,#97339,#97340,#97341,#97342,#97343,#97344,
#97345,#97346,#97347,#97348,#97349,#97350,#97351,#97352,#97353,#97354,#97355,
#97356,#97357,#97358,#97359,#97360),.UNSPECIFIED.,.F.,.F.)
B_SPLINE_CURVE_WITH_KNOTS((6,1,1,1,1,1,1,1,1,1,1,1,1,1,1,1,1,1,1,1,1,1,
1,1,1,1,1,1,1,1,6),(0.,0.0333333333333333,0.0666666666666667,0.1,0.133333333333333,
0.166666666666667,0.2,0.233333333333333,0.266666666666667,0.3,0.333333333333333,
0.366666666666667,0.4,0.433333333333333,0.466666666666667,0.5,0.533333333333333,
0.566666666666667,0.6,0.633333333333333,0.666666666666667,0.7,0.733333333333333,
0.766666666666667,0.8,0.833333333333333,0.866666666666667,0.9,0.933333333333333,
0.966666666666667,1.),.UNSPECIFIED.)
CURVE()
GEOMETRIC_REPRESENTATION_ITEM()
RATIONAL_B_SPLINE_CURVE((1.,1.,1.,1.,1.,1.,1.,1.,1.,1.,1.,1.,1.,1.,1.,1.,
1.,1.,1.,1.,1.,1.,1.,1.,1.,1.,1.,1.,1.,1.,1.,1.,1.,1.,1.))
REPRESENTATION_ITEM('')
);
#206=(
BOUNDED_CURVE()
B_SPLINE_CURVE(5,(#97361,#97362,#97363,#97364,#97365,#97366,#97367,#97368,
#97369,#97370,#97371,#97372,#97373,#97374,#97375,#97376,#97377,#97378,#97379,
#97380,#97381,#97382,#97383,#97384,#97385,#97386,#97387,#97388,#97389,#97390,
#97391,#97392,#97393,#97394,#97395),.UNSPECIFIED.,.F.,.F.)
B_SPLINE_CURVE_WITH_KNOTS((6,1,1,1,1,1,1,1,1,1,1,1,1,1,1,1,1,1,1,1,1,1,
1,1,1,1,1,1,1,1,6),(0.,0.0333333333333333,0.0666666666666667,0.1,0.133333333333333,
0.166666666666667,0.2,0.233333333333333,0.266666666666667,0.3,0.333333333333333,
0.366666666666667,0.4,0.433333333333333,0.466666666666667,0.5,0.533333333333333,
0.566666666666667,0.6,0.633333333333333,0.666666666666667,0.7,0.733333333333333,
0.766666666666667,0.8,0.833333333333333,0.866666666666667,0.9,0.933333333333333,
0.966666666666667,1.),.UNSPECIFIED.)
CURVE()
GEOMETRIC_REPRESENTATION_ITEM()
RATIONAL_B_SPLINE_CURVE((1.,1.,1.,1.,1.,1.,1.,1.,1.,1.,1.,1.,1.,1.,1.,1.,
1.,1.,1.,1.,1.,1.,1.,1.,1.,1.,1.,1.,1.,1.,1.,1.,1.,1.,1.))
REPRESENTATION_ITEM('')
);
#207=(
BOUNDED_CURVE()
B_SPLINE_CURVE(5,(#97474,#97475,#97476,#97477,#97478,#97479,#97480,#97481,
#97482,#97483,#97484,#97485,#97486,#97487,#97488,#97489,#97490,#97491,#97492,
#97493,#97494,#97495,#97496,#97497,#97498,#97499,#97500,#97501,#97502,#97503,
#97504,#97505,#97506,#97507,#97508),.UNSPECIFIED.,.F.,.F.)
B_SPLINE_CURVE_WITH_KNOTS((6,1,1,1,1,1,1,1,1,1,1,1,1,1,1,1,1,1,1,1,1,1,
1,1,1,1,1,1,1,1,6),(0.,0.0333333333333333,0.0666666666666667,0.1,0.133333333333333,
0.166666666666667,0.2,0.233333333333333,0.266666666666667,0.3,0.333333333333333,
0.366666666666667,0.4,0.433333333333333,0.466666666666667,0.5,0.533333333333333,
0.566666666666667,0.6,0.633333333333333,0.666666666666667,0.7,0.733333333333333,
0.766666666666667,0.8,0.833333333333333,0.866666666666667,0.9,0.933333333333333,
0.966666666666667,1.),.UNSPECIFIED.)
CURVE()
GEOMETRIC_REPRESENTATION_ITEM()
RATIONAL_B_SPLINE_CURVE((1.,1.,1.,1.,1.,1.,1.,1.,1.,1.,1.,1.,1.,1.,1.,1.,
1.,1.,1.,1.,1.,1.,1.,1.,1.,1.,1.,1.,1.,1.,1.,1.,1.,1.,1.))
REPRESENTATION_ITEM('')
);
#208=(
BOUNDED_CURVE()
B_SPLINE_CURVE(5,(#97510,#97511,#97512,#97513,#97514,#97515,#97516,#97517,
#97518,#97519,#97520,#97521,#97522,#97523,#97524,#97525,#97526,#97527,#97528,
#97529,#97530,#97531,#97532,#97533,#97534,#97535,#97536,#97537,#97538,#97539,
#97540,#97541,#97542,#97543,#97544),.UNSPECIFIED.,.F.,.F.)
B_SPLINE_CURVE_WITH_KNOTS((6,1,1,1,1,1,1,1,1,1,1,1,1,1,1,1,1,1,1,1,1,1,
1,1,1,1,1,1,1,1,6),(-1.,-0.966666666666667,-0.933333333333333,-0.9,-0.866666666666667,
-0.833333333333333,-0.8,-0.766666666666667,-0.733333333333333,-0.7,-0.666666666666667,
-0.633333333333333,-0.6,-0.566666666666667,-0.533333333333333,-0.5,-0.466666666666667,
-0.433333333333333,-0.4,-0.366666666666667,-0.333333333333333,-0.3,-0.266666666666667,
-0.233333333333333,-0.2,-0.166666666666667,-0.133333333333333,-0.1,-0.0666666666666667,
-0.0333333333333333,0.),.UNSPECIFIED.)
CURVE()
GEOMETRIC_REPRESENTATION_ITEM()
RATIONAL_B_SPLINE_CURVE((1.,1.,1.,1.,1.,1.,1.,1.,1.,1.,1.,1.,1.,1.,1.,1.,
1.,1.,1.,1.,1.,1.,1.,1.,1.,1.,1.,1.,1.,1.,1.,1.,1.,1.,1.))
REPRESENTATION_ITEM('')
);
#209=(
BOUNDED_CURVE()
B_SPLINE_CURVE(5,(#97623,#97624,#97625,#97626,#97627,#97628,#97629,#97630,
#97631,#97632,#97633,#97634,#97635,#97636,#97637,#97638,#97639,#97640,#97641,
#97642,#97643,#97644,#97645,#97646,#97647,#97648,#97649,#97650,#97651,#97652,
#97653,#97654,#97655,#97656,#97657),.UNSPECIFIED.,.F.,.F.)
B_SPLINE_CURVE_WITH_KNOTS((6,1,1,1,1,1,1,1,1,1,1,1,1,1,1,1,1,1,1,1,1,1,
1,1,1,1,1,1,1,1,6),(0.,0.0333333333333333,0.0666666666666667,0.1,0.133333333333333,
0.166666666666667,0.2,0.233333333333333,0.266666666666667,0.3,0.333333333333333,
0.366666666666667,0.4,0.433333333333333,0.466666666666667,0.5,0.533333333333333,
0.566666666666667,0.6,0.633333333333333,0.666666666666667,0.7,0.733333333333333,
0.766666666666667,0.8,0.833333333333333,0.866666666666667,0.9,0.933333333333333,
0.966666666666667,1.),.UNSPECIFIED.)
CURVE()
GEOMETRIC_REPRESENTATION_ITEM()
RATIONAL_B_SPLINE_CURVE((1.,1.,1.,1.,1.,1.,1.,1.,1.,1.,1.,1.,1.,1.,1.,1.,
1.,1.,1.,1.,1.,1.,1.,1.,1.,1.,1.,1.,1.,1.,1.,1.,1.,1.,1.))
REPRESENTATION_ITEM('')
);
#210=(
BOUNDED_CURVE()
B_SPLINE_CURVE(5,(#97659,#97660,#97661,#97662,#97663,#97664,#97665,#97666,
#97667,#97668,#97669,#97670,#97671,#97672,#97673,#97674,#97675,#97676,#97677,
#97678,#97679,#97680,#97681,#97682,#97683,#97684,#97685,#97686,#97687,#97688,
#97689,#97690,#97691,#97692,#97693),.UNSPECIFIED.,.F.,.F.)
B_SPLINE_CURVE_WITH_KNOTS((6,1,1,1,1,1,1,1,1,1,1,1,1,1,1,1,1,1,1,1,1,1,
1,1,1,1,1,1,1,1,6),(0.,0.0333333333333333,0.0666666666666667,0.1,0.133333333333333,
0.166666666666667,0.2,0.233333333333333,0.266666666666667,0.3,0.333333333333333,
0.366666666666667,0.4,0.433333333333333,0.466666666666667,0.5,0.533333333333333,
0.566666666666667,0.6,0.633333333333333,0.666666666666667,0.7,0.733333333333333,
0.766666666666667,0.8,0.833333333333333,0.866666666666667,0.9,0.933333333333333,
0.966666666666667,1.),.UNSPECIFIED.)
CURVE()
GEOMETRIC_REPRESENTATION_ITEM()
RATIONAL_B_SPLINE_CURVE((1.,1.,1.,1.,1.,1.,1.,1.,1.,1.,1.,1.,1.,1.,1.,1.,
1.,1.,1.,1.,1.,1.,1.,1.,1.,1.,1.,1.,1.,1.,1.,1.,1.,1.,1.))
REPRESENTATION_ITEM('')
);
#211=(
BOUNDED_CURVE()
B_SPLINE_CURVE(2,(#97814,#97815,#97816),.UNSPECIFIED.,.F.,.F.)
B_SPLINE_CURVE_WITH_KNOTS((3,3),(0.0639904841458714,0.1243156910283),
 .UNSPECIFIED.)
CURVE()
GEOMETRIC_REPRESENTATION_ITEM()
RATIONAL_B_SPLINE_CURVE((1.0006146198185,1.00059701757594,1.))
REPRESENTATION_ITEM('')
);
#212=(
BOUNDED_CURVE()
B_SPLINE_CURVE(2,(#97820,#97821,#97822),.UNSPECIFIED.,.F.,.F.)
B_SPLINE_CURVE_WITH_KNOTS((3,3),(0.,0.0603252068824429),.UNSPECIFIED.)
CURVE()
GEOMETRIC_REPRESENTATION_ITEM()
RATIONAL_B_SPLINE_CURVE((1.,1.00059701758504,1.00061461982786))
REPRESENTATION_ITEM('')
);
#213=(
BOUNDED_CURVE()
B_SPLINE_CURVE(2,(#97826,#97827,#97828),.UNSPECIFIED.,.F.,.F.)
B_SPLINE_CURVE_WITH_KNOTS((3,3),(0.,0.0603252068824511),.UNSPECIFIED.)
CURVE()
GEOMETRIC_REPRESENTATION_ITEM()
RATIONAL_B_SPLINE_CURVE((1.,1.00059701757207,1.00061461981452))
REPRESENTATION_ITEM('')
);
#214=(
BOUNDED_CURVE()
B_SPLINE_CURVE(2,(#97831,#97832,#97833),.UNSPECIFIED.,.F.,.F.)
B_SPLINE_CURVE_WITH_KNOTS((3,3),(0.0639904841458541,0.124315691028304),
 .UNSPECIFIED.)
CURVE()
GEOMETRIC_REPRESENTATION_ITEM()
RATIONAL_B_SPLINE_CURVE((1.00061461982307,1.00059701758038,1.))
REPRESENTATION_ITEM('')
);
#215=(
BOUNDED_CURVE()
B_SPLINE_CURVE(2,(#97838,#97839,#97840),.UNSPECIFIED.,.F.,.F.)
B_SPLINE_CURVE_WITH_KNOTS((3,3),(0.,0.0603252068825254),.UNSPECIFIED.)
CURVE()
GEOMETRIC_REPRESENTATION_ITEM()
RATIONAL_B_SPLINE_CURVE((1.,1.00059701756463,1.00061461980685))
REPRESENTATION_ITEM('')
);
#216=(
BOUNDED_CURVE()
B_SPLINE_CURVE(2,(#97842,#97843,#97844),.UNSPECIFIED.,.F.,.F.)
B_SPLINE_CURVE_WITH_KNOTS((3,3),(0.0639904841458276,0.124315691028306),
 .UNSPECIFIED.)
CURVE()
GEOMETRIC_REPRESENTATION_ITEM()
RATIONAL_B_SPLINE_CURVE((1.00061461981098,1.00059701756864,1.))
REPRESENTATION_ITEM('')
);
#217=(
BOUNDED_CURVE()
B_SPLINE_CURVE(2,(#97848,#97849,#97850),.UNSPECIFIED.,.F.,.F.)
B_SPLINE_CURVE_WITH_KNOTS((3,3),(0.,0.0603252068824394),.UNSPECIFIED.)
CURVE()
GEOMETRIC_REPRESENTATION_ITEM()
RATIONAL_B_SPLINE_CURVE((1.,1.00059701757103,1.00061461981344))
REPRESENTATION_ITEM('')
);
#218=(
BOUNDED_CURVE()
B_SPLINE_CURVE(2,(#97852,#97853,#97854),.UNSPECIFIED.,.F.,.F.)
B_SPLINE_CURVE_WITH_KNOTS((3,3),(0.0639904841458415,0.124315691028305),
 .UNSPECIFIED.)
CURVE()
GEOMETRIC_REPRESENTATION_ITEM()
RATIONAL_B_SPLINE_CURVE((1.00061461981036,1.00059701756804,1.))
REPRESENTATION_ITEM('')
);
#219=(
BOUNDED_CURVE()
B_SPLINE_CURVE(2,(#97858,#97859,#97860),.UNSPECIFIED.,.F.,.F.)
B_SPLINE_CURVE_WITH_KNOTS((3,3),(0.,0.0603252068825714),.UNSPECIFIED.)
CURVE()
GEOMETRIC_REPRESENTATION_ITEM()
RATIONAL_B_SPLINE_CURVE((1.,1.00059701757132,1.00061461981374))
REPRESENTATION_ITEM('')
);
#220=(
BOUNDED_CURVE()
B_SPLINE_CURVE(2,(#97862,#97863,#97864),.UNSPECIFIED.,.F.,.F.)
B_SPLINE_CURVE_WITH_KNOTS((3,3),(0.0639904841458359,0.124315691028304),
 .UNSPECIFIED.)
CURVE()
GEOMETRIC_REPRESENTATION_ITEM()
RATIONAL_B_SPLINE_CURVE((1.00061461982205,1.00059701757939,1.))
REPRESENTATION_ITEM('')
);
#221=(
BOUNDED_CURVE()
B_SPLINE_CURVE(2,(#97868,#97869,#97870),.UNSPECIFIED.,.F.,.F.)
B_SPLINE_CURVE_WITH_KNOTS((3,3),(0.,0.0603252068824456),.UNSPECIFIED.)
CURVE()
GEOMETRIC_REPRESENTATION_ITEM()
RATIONAL_B_SPLINE_CURVE((1.,1.00059701756571,1.00061461980796))
REPRESENTATION_ITEM('')
);
#222=(
BOUNDED_CURVE()
B_SPLINE_CURVE(2,(#97872,#97873,#97874),.UNSPECIFIED.,.F.,.F.)
B_SPLINE_CURVE_WITH_KNOTS((3,3),(0.0639904841458113,0.124315691028305),
 .UNSPECIFIED.)
CURVE()
GEOMETRIC_REPRESENTATION_ITEM()
RATIONAL_B_SPLINE_CURVE((1.00061461980765,1.00059701756541,1.))
REPRESENTATION_ITEM('')
);
#223=(
BOUNDED_CURVE()
B_SPLINE_CURVE(2,(#97878,#97879,#97880),.UNSPECIFIED.,.F.,.F.)
B_SPLINE_CURVE_WITH_KNOTS((3,3),(0.,0.0603252068824822),.UNSPECIFIED.)
CURVE()
GEOMETRIC_REPRESENTATION_ITEM()
RATIONAL_B_SPLINE_CURVE((1.,1.00059701756982,1.0006146198122))
REPRESENTATION_ITEM('')
);
#224=(
BOUNDED_CURVE()
B_SPLINE_CURVE(2,(#97882,#97883,#97884),.UNSPECIFIED.,.F.,.F.)
B_SPLINE_CURVE_WITH_KNOTS((3,3),(0.0639904841458351,0.124315691028304),
 .UNSPECIFIED.)
CURVE()
GEOMETRIC_REPRESENTATION_ITEM()
RATIONAL_B_SPLINE_CURVE((1.0006146198107,1.00059701756837,1.))
REPRESENTATION_ITEM('')
);
#225=(
BOUNDED_CURVE()
B_SPLINE_CURVE(2,(#97888,#97889,#97890),.UNSPECIFIED.,.F.,.F.)
B_SPLINE_CURVE_WITH_KNOTS((3,3),(0.,0.0603252068824583),.UNSPECIFIED.)
CURVE()
GEOMETRIC_REPRESENTATION_ITEM()
RATIONAL_B_SPLINE_CURVE((1.,1.00059701757041,1.0006146198128))
REPRESENTATION_ITEM('')
);
#226=(
BOUNDED_CURVE()
B_SPLINE_CURVE(2,(#97892,#97893,#97894),.UNSPECIFIED.,.F.,.F.)
B_SPLINE_CURVE_WITH_KNOTS((3,3),(0.0639904841458709,0.124315691028304),
 .UNSPECIFIED.)
CURVE()
GEOMETRIC_REPRESENTATION_ITEM()
RATIONAL_B_SPLINE_CURVE((1.00061461981124,1.00059701756889,1.))
REPRESENTATION_ITEM('')
);
#227=(
BOUNDED_CURVE()
B_SPLINE_CURVE(2,(#97898,#97899,#97900),.UNSPECIFIED.,.F.,.F.)
B_SPLINE_CURVE_WITH_KNOTS((3,3),(0.,0.0603252068824821),.UNSPECIFIED.)
CURVE()
GEOMETRIC_REPRESENTATION_ITEM()
RATIONAL_B_SPLINE_CURVE((1.,1.0005970175711,1.00061461981351))
REPRESENTATION_ITEM('')
);
#228=(
BOUNDED_CURVE()
B_SPLINE_CURVE(2,(#97902,#97903,#97904),.UNSPECIFIED.,.F.,.F.)
B_SPLINE_CURVE_WITH_KNOTS((3,3),(0.0639904841458647,0.124315691028304),
 .UNSPECIFIED.)
CURVE()
GEOMETRIC_REPRESENTATION_ITEM()
RATIONAL_B_SPLINE_CURVE((1.00061461981158,1.00059701756922,1.))
REPRESENTATION_ITEM('')
);
#229=(
BOUNDED_CURVE()
B_SPLINE_CURVE(2,(#97908,#97909,#97910),.UNSPECIFIED.,.F.,.F.)
B_SPLINE_CURVE_WITH_KNOTS((3,3),(0.,0.0603252068825191),.UNSPECIFIED.)
CURVE()
GEOMETRIC_REPRESENTATION_ITEM()
RATIONAL_B_SPLINE_CURVE((1.,1.00059701757121,1.00061461981363))
REPRESENTATION_ITEM('')
);
#230=(
BOUNDED_CURVE()
B_SPLINE_CURVE(2,(#97912,#97913,#97914),.UNSPECIFIED.,.F.,.F.)
B_SPLINE_CURVE_WITH_KNOTS((3,3),(0.063990484145815,0.124315691028306),
 .UNSPECIFIED.)
CURVE()
GEOMETRIC_REPRESENTATION_ITEM()
RATIONAL_B_SPLINE_CURVE((1.00061461981174,1.00059701756938,1.))
REPRESENTATION_ITEM('')
);
#231=(
BOUNDED_CURVE()
B_SPLINE_CURVE(2,(#97918,#97919,#97920),.UNSPECIFIED.,.F.,.F.)
B_SPLINE_CURVE_WITH_KNOTS((3,3),(0.,0.0603252068824783),.UNSPECIFIED.)
CURVE()
GEOMETRIC_REPRESENTATION_ITEM()
RATIONAL_B_SPLINE_CURVE((1.,1.00059701757256,1.00061461981502))
REPRESENTATION_ITEM('')
);
#232=(
BOUNDED_CURVE()
B_SPLINE_CURVE(2,(#97922,#97923,#97924),.UNSPECIFIED.,.F.,.F.)
B_SPLINE_CURVE_WITH_KNOTS((3,3),(0.0639904841458416,0.124315691028306),
 .UNSPECIFIED.)
CURVE()
GEOMETRIC_REPRESENTATION_ITEM()
RATIONAL_B_SPLINE_CURVE((1.00061461981231,1.00059701756993,1.))
REPRESENTATION_ITEM('')
);
#233=(
BOUNDED_CURVE()
B_SPLINE_CURVE(2,(#97928,#97929,#97930),.UNSPECIFIED.,.F.,.F.)
B_SPLINE_CURVE_WITH_KNOTS((3,3),(0.,0.0603252068824794),.UNSPECIFIED.)
CURVE()
GEOMETRIC_REPRESENTATION_ITEM()
RATIONAL_B_SPLINE_CURVE((1.,1.00059701756815,1.00061461981048))
REPRESENTATION_ITEM('')
);
#234=(
BOUNDED_CURVE()
B_SPLINE_CURVE(2,(#97932,#97933,#97934),.UNSPECIFIED.,.F.,.F.)
B_SPLINE_CURVE_WITH_KNOTS((3,3),(0.0639904841457963,0.124315691028306),
 .UNSPECIFIED.)
CURVE()
GEOMETRIC_REPRESENTATION_ITEM()
RATIONAL_B_SPLINE_CURVE((1.00061461981017,1.00059701756786,1.))
REPRESENTATION_ITEM('')
);
#235=(
BOUNDED_CURVE()
B_SPLINE_CURVE(2,(#97938,#97939,#97940),.UNSPECIFIED.,.F.,.F.)
B_SPLINE_CURVE_WITH_KNOTS((3,3),(0.,0.0603252068824883),.UNSPECIFIED.)
CURVE()
GEOMETRIC_REPRESENTATION_ITEM()
RATIONAL_B_SPLINE_CURVE((1.,1.00059701756951,1.00061461981188))
REPRESENTATION_ITEM('')
);
#236=(
BOUNDED_CURVE()
B_SPLINE_CURVE(2,(#97942,#97943,#97944),.UNSPECIFIED.,.F.,.F.)
B_SPLINE_CURVE_WITH_KNOTS((3,3),(0.0639904841458018,0.124315691028305),
 .UNSPECIFIED.)
CURVE()
GEOMETRIC_REPRESENTATION_ITEM()
RATIONAL_B_SPLINE_CURVE((1.00061461980912,1.00059701756684,1.))
REPRESENTATION_ITEM('')
);
#237=(
BOUNDED_CURVE()
B_SPLINE_CURVE(2,(#97948,#97949,#97950),.UNSPECIFIED.,.F.,.F.)
B_SPLINE_CURVE_WITH_KNOTS((3,3),(0.,0.0603252068824852),.UNSPECIFIED.)
CURVE()
GEOMETRIC_REPRESENTATION_ITEM()
RATIONAL_B_SPLINE_CURVE((1.,1.00059701756809,1.00061461981042))
REPRESENTATION_ITEM('')
);
#238=(
BOUNDED_CURVE()
B_SPLINE_CURVE(2,(#97952,#97953,#97954),.UNSPECIFIED.,.F.,.F.)
B_SPLINE_CURVE_WITH_KNOTS((3,3),(0.0639904841458453,0.124315691028304),
 .UNSPECIFIED.)
CURVE()
GEOMETRIC_REPRESENTATION_ITEM()
RATIONAL_B_SPLINE_CURVE((1.0006146198128,1.00059701757041,1.))
REPRESENTATION_ITEM('')
);
#239=(
BOUNDED_CURVE()
B_SPLINE_CURVE(2,(#97958,#97959,#97960),.UNSPECIFIED.,.F.,.F.)
B_SPLINE_CURVE_WITH_KNOTS((3,3),(0.,0.06032520688249),.UNSPECIFIED.)
CURVE()
GEOMETRIC_REPRESENTATION_ITEM()
RATIONAL_B_SPLINE_CURVE((1.,1.00059701756971,1.00061461981208))
REPRESENTATION_ITEM('')
);
#240=(
BOUNDED_CURVE()
B_SPLINE_CURVE(2,(#97962,#97963,#97964),.UNSPECIFIED.,.F.,.F.)
B_SPLINE_CURVE_WITH_KNOTS((3,3),(0.0639904841458239,0.124315691028304),
 .UNSPECIFIED.)
CURVE()
GEOMETRIC_REPRESENTATION_ITEM()
RATIONAL_B_SPLINE_CURVE((1.0006146198114,1.00059701756905,1.))
REPRESENTATION_ITEM('')
);
#241=(
BOUNDED_CURVE()
B_SPLINE_CURVE(2,(#97968,#97969,#97970),.UNSPECIFIED.,.F.,.F.)
B_SPLINE_CURVE_WITH_KNOTS((3,3),(0.,0.0603252068824721),.UNSPECIFIED.)
CURVE()
GEOMETRIC_REPRESENTATION_ITEM()
RATIONAL_B_SPLINE_CURVE((1.,1.0005970175654,1.00061461980764))
REPRESENTATION_ITEM('')
);
#242=(
BOUNDED_CURVE()
B_SPLINE_CURVE(2,(#97972,#97973,#97974),.UNSPECIFIED.,.F.,.F.)
B_SPLINE_CURVE_WITH_KNOTS((3,3),(0.0639904841458158,0.124315691028305),
 .UNSPECIFIED.)
CURVE()
GEOMETRIC_REPRESENTATION_ITEM()
RATIONAL_B_SPLINE_CURVE((1.00061461980759,1.00059701756535,1.))
REPRESENTATION_ITEM('')
);
#243=(
BOUNDED_CURVE()
B_SPLINE_CURVE(2,(#97978,#97979,#97980),.UNSPECIFIED.,.F.,.F.)
B_SPLINE_CURVE_WITH_KNOTS((3,3),(0.,0.0603252068824717),.UNSPECIFIED.)
CURVE()
GEOMETRIC_REPRESENTATION_ITEM()
RATIONAL_B_SPLINE_CURVE((1.,1.00059701757901,1.00061461982166))
REPRESENTATION_ITEM('')
);
#244=(
BOUNDED_CURVE()
B_SPLINE_CURVE(2,(#97982,#97983,#97984),.UNSPECIFIED.,.F.,.F.)
B_SPLINE_CURVE_WITH_KNOTS((3,3),(0.063990484145796,0.124315691028302),
 .UNSPECIFIED.)
CURVE()
GEOMETRIC_REPRESENTATION_ITEM()
RATIONAL_B_SPLINE_CURVE((1.0006146198112,1.00059701756885,1.))
REPRESENTATION_ITEM('')
);
#245=(
BOUNDED_CURVE()
B_SPLINE_CURVE(2,(#97988,#97989,#97990),.UNSPECIFIED.,.F.,.F.)
B_SPLINE_CURVE_WITH_KNOTS((3,3),(0.,0.0603252068824572),.UNSPECIFIED.)
CURVE()
GEOMETRIC_REPRESENTATION_ITEM()
RATIONAL_B_SPLINE_CURVE((1.,1.00059701757014,1.00061461981252))
REPRESENTATION_ITEM('')
);
#246=(
BOUNDED_CURVE()
B_SPLINE_CURVE(2,(#97992,#97993,#97994),.UNSPECIFIED.,.F.,.F.)
B_SPLINE_CURVE_WITH_KNOTS((3,3),(0.0639904841458277,0.124315691028304),
 .UNSPECIFIED.)
CURVE()
GEOMETRIC_REPRESENTATION_ITEM()
RATIONAL_B_SPLINE_CURVE((1.00061461981263,1.00059701757024,1.))
REPRESENTATION_ITEM('')
);
#247=(
BOUNDED_CURVE()
B_SPLINE_CURVE(2,(#97998,#97999,#98000),.UNSPECIFIED.,.F.,.F.)
B_SPLINE_CURVE_WITH_KNOTS((3,3),(0.,0.0603252068824675),.UNSPECIFIED.)
CURVE()
GEOMETRIC_REPRESENTATION_ITEM()
RATIONAL_B_SPLINE_CURVE((1.,1.00059701756283,1.000614619805))
REPRESENTATION_ITEM('')
);
#248=(
BOUNDED_CURVE()
B_SPLINE_CURVE(2,(#98002,#98003,#98004),.UNSPECIFIED.,.F.,.F.)
B_SPLINE_CURVE_WITH_KNOTS((3,3),(0.0639904841458849,0.124315691028304),
 .UNSPECIFIED.)
CURVE()
GEOMETRIC_REPRESENTATION_ITEM()
RATIONAL_B_SPLINE_CURVE((1.00061461981573,1.00059701757326,1.))
REPRESENTATION_ITEM('')
);
#249=(
BOUNDED_CURVE()
B_SPLINE_CURVE(2,(#98008,#98009,#98010),.UNSPECIFIED.,.F.,.F.)
B_SPLINE_CURVE_WITH_KNOTS((3,3),(0.,0.0603252068824598),.UNSPECIFIED.)
CURVE()
GEOMETRIC_REPRESENTATION_ITEM()
RATIONAL_B_SPLINE_CURVE((1.,1.0005970175702,1.00061461981259))
REPRESENTATION_ITEM('')
);
#250=(
BOUNDED_CURVE()
B_SPLINE_CURVE(2,(#98012,#98013,#98014),.UNSPECIFIED.,.F.,.F.)
B_SPLINE_CURVE_WITH_KNOTS((3,3),(0.0639904841458239,0.124315691028304),
 .UNSPECIFIED.)
CURVE()
GEOMETRIC_REPRESENTATION_ITEM()
RATIONAL_B_SPLINE_CURVE((1.00061461981594,1.00059701757346,1.))
REPRESENTATION_ITEM('')
);
#251=(
BOUNDED_CURVE()
B_SPLINE_CURVE(2,(#98018,#98019,#98020),.UNSPECIFIED.,.F.,.F.)
B_SPLINE_CURVE_WITH_KNOTS((3,3),(0.,0.0603252068824849),.UNSPECIFIED.)
CURVE()
GEOMETRIC_REPRESENTATION_ITEM()
RATIONAL_B_SPLINE_CURVE((1.,1.00059701756587,1.00061461980812))
REPRESENTATION_ITEM('')
);
#252=(
BOUNDED_CURVE()
B_SPLINE_CURVE(2,(#98025,#98026,#98027),.UNSPECIFIED.,.F.,.F.)
B_SPLINE_CURVE_WITH_KNOTS((3,3),(0.0639904841458217,0.124315691028305),
 .UNSPECIFIED.)
CURVE()
GEOMETRIC_REPRESENTATION_ITEM()
RATIONAL_B_SPLINE_CURVE((1.00061461980612,1.00059701756392,1.))
REPRESENTATION_ITEM('')
);
#253=(
BOUNDED_CURVE()
B_SPLINE_CURVE(2,(#98031,#98032,#98033),.UNSPECIFIED.,.F.,.F.)
B_SPLINE_CURVE_WITH_KNOTS((3,3),(0.,0.060325206882456),.UNSPECIFIED.)
CURVE()
GEOMETRIC_REPRESENTATION_ITEM()
RATIONAL_B_SPLINE_CURVE((1.,1.00059701757113,1.00061461981354))
REPRESENTATION_ITEM('')
);
#254=(
BOUNDED_CURVE()
B_SPLINE_CURVE(2,(#98035,#98036,#98037),.UNSPECIFIED.,.F.,.F.)
B_SPLINE_CURVE_WITH_KNOTS((3,3),(0.0639904841458245,0.124315691028306),
 .UNSPECIFIED.)
CURVE()
GEOMETRIC_REPRESENTATION_ITEM()
RATIONAL_B_SPLINE_CURVE((1.00061461981538,1.00059701757292,1.))
REPRESENTATION_ITEM('')
);
#255=(
BOUNDED_CURVE()
B_SPLINE_CURVE(2,(#98041,#98042,#98043),.UNSPECIFIED.,.F.,.F.)
B_SPLINE_CURVE_WITH_KNOTS((3,3),(0.,0.0603252068824492),.UNSPECIFIED.)
CURVE()
GEOMETRIC_REPRESENTATION_ITEM()
RATIONAL_B_SPLINE_CURVE((1.,1.0005970175686,1.00061461981094))
REPRESENTATION_ITEM('')
);
#256=(
BOUNDED_CURVE()
B_SPLINE_CURVE(2,(#98045,#98046,#98047),.UNSPECIFIED.,.F.,.F.)
B_SPLINE_CURVE_WITH_KNOTS((3,3),(0.0639904841457976,0.124315691028306),
 .UNSPECIFIED.)
CURVE()
GEOMETRIC_REPRESENTATION_ITEM()
RATIONAL_B_SPLINE_CURVE((1.00061461981101,1.00059701756867,1.))
REPRESENTATION_ITEM('')
);
#257=(
BOUNDED_CURVE()
B_SPLINE_CURVE(2,(#98051,#98052,#98053),.UNSPECIFIED.,.F.,.F.)
B_SPLINE_CURVE_WITH_KNOTS((3,3),(0.,0.0603252068824974),.UNSPECIFIED.)
CURVE()
GEOMETRIC_REPRESENTATION_ITEM()
RATIONAL_B_SPLINE_CURVE((1.,1.00059701757075,1.00061461981315))
REPRESENTATION_ITEM('')
);
#258=(
BOUNDED_CURVE()
B_SPLINE_CURVE(2,(#98055,#98056,#98057),.UNSPECIFIED.,.F.,.F.)
B_SPLINE_CURVE_WITH_KNOTS((3,3),(0.0639904841458211,0.124315691028304),
 .UNSPECIFIED.)
CURVE()
GEOMETRIC_REPRESENTATION_ITEM()
RATIONAL_B_SPLINE_CURVE((1.00061461981339,1.00059701757099,1.))
REPRESENTATION_ITEM('')
);
#259=(
BOUNDED_CURVE()
B_SPLINE_CURVE(2,(#98061,#98062,#98063),.UNSPECIFIED.,.F.,.F.)
B_SPLINE_CURVE_WITH_KNOTS((3,3),(0.,0.0603252068824656),.UNSPECIFIED.)
CURVE()
GEOMETRIC_REPRESENTATION_ITEM()
RATIONAL_B_SPLINE_CURVE((1.,1.00059701757014,1.00061461981252))
REPRESENTATION_ITEM('')
);
#260=(
BOUNDED_CURVE()
B_SPLINE_CURVE(2,(#98065,#98066,#98067),.UNSPECIFIED.,.F.,.F.)
B_SPLINE_CURVE_WITH_KNOTS((3,3),(0.0639904841457857,0.124315691028306),
 .UNSPECIFIED.)
CURVE()
GEOMETRIC_REPRESENTATION_ITEM()
RATIONAL_B_SPLINE_CURVE((1.00061461980911,1.00059701756683,1.))
REPRESENTATION_ITEM('')
);
#261=(
BOUNDED_CURVE()
B_SPLINE_CURVE(2,(#98071,#98072,#98073),.UNSPECIFIED.,.F.,.F.)
B_SPLINE_CURVE_WITH_KNOTS((3,3),(0.,0.0603252068825302),.UNSPECIFIED.)
CURVE()
GEOMETRIC_REPRESENTATION_ITEM()
RATIONAL_B_SPLINE_CURVE((1.,1.00059701756736,1.00061461980966))
REPRESENTATION_ITEM('')
);
#262=(
BOUNDED_CURVE()
B_SPLINE_CURVE(2,(#98075,#98076,#98077),.UNSPECIFIED.,.F.,.F.)
B_SPLINE_CURVE_WITH_KNOTS((3,3),(0.0639904841458149,0.124315691028305),
 .UNSPECIFIED.)
CURVE()
GEOMETRIC_REPRESENTATION_ITEM()
RATIONAL_B_SPLINE_CURVE((1.00061461980823,1.00059701756597,1.))
REPRESENTATION_ITEM('')
);
#263=(
BOUNDED_CURVE()
B_SPLINE_CURVE(2,(#98081,#98082,#98083),.UNSPECIFIED.,.F.,.F.)
B_SPLINE_CURVE_WITH_KNOTS((3,3),(0.,0.0603252068825094),.UNSPECIFIED.)
CURVE()
GEOMETRIC_REPRESENTATION_ITEM()
RATIONAL_B_SPLINE_CURVE((1.,1.00059701757625,1.00061461981881))
REPRESENTATION_ITEM('')
);
#264=(
BOUNDED_CURVE()
B_SPLINE_CURVE(2,(#98085,#98086,#98087),.UNSPECIFIED.,.F.,.F.)
B_SPLINE_CURVE_WITH_KNOTS((3,3),(0.0639904841458013,0.124315691028303),
 .UNSPECIFIED.)
CURVE()
GEOMETRIC_REPRESENTATION_ITEM()
RATIONAL_B_SPLINE_CURVE((1.00061461981526,1.0005970175728,1.))
REPRESENTATION_ITEM('')
);
#265=(
BOUNDED_CURVE()
B_SPLINE_CURVE(2,(#98091,#98092,#98093),.UNSPECIFIED.,.F.,.F.)
B_SPLINE_CURVE_WITH_KNOTS((3,3),(0.,0.060325206882548),.UNSPECIFIED.)
CURVE()
GEOMETRIC_REPRESENTATION_ITEM()
RATIONAL_B_SPLINE_CURVE((1.,1.0005970175677,1.00061461981001))
REPRESENTATION_ITEM('')
);
#266=(
BOUNDED_CURVE()
B_SPLINE_CURVE(2,(#98095,#98096,#98097),.UNSPECIFIED.,.F.,.F.)
B_SPLINE_CURVE_WITH_KNOTS((3,3),(0.0639904841458135,0.124315691028304),
 .UNSPECIFIED.)
CURVE()
GEOMETRIC_REPRESENTATION_ITEM()
RATIONAL_B_SPLINE_CURVE((1.00061461981065,1.00059701756832,1.))
REPRESENTATION_ITEM('')
);
#267=(
BOUNDED_CURVE()
B_SPLINE_CURVE(2,(#98101,#98102,#98103),.UNSPECIFIED.,.F.,.F.)
B_SPLINE_CURVE_WITH_KNOTS((3,3),(0.,0.0603252068824779),.UNSPECIFIED.)
CURVE()
GEOMETRIC_REPRESENTATION_ITEM()
RATIONAL_B_SPLINE_CURVE((1.,1.00059701756951,1.00061461981188))
REPRESENTATION_ITEM('')
);
#268=(
BOUNDED_CURVE()
B_SPLINE_CURVE(2,(#98105,#98106,#98107),.UNSPECIFIED.,.F.,.F.)
B_SPLINE_CURVE_WITH_KNOTS((3,3),(0.0639904841458649,0.124315691028304),
 .UNSPECIFIED.)
CURVE()
GEOMETRIC_REPRESENTATION_ITEM()
RATIONAL_B_SPLINE_CURVE((1.00061461981009,1.00059701756778,1.))
REPRESENTATION_ITEM('')
);
#269=(
BOUNDED_CURVE()
B_SPLINE_CURVE(2,(#98111,#98112,#98113),.UNSPECIFIED.,.F.,.F.)
B_SPLINE_CURVE_WITH_KNOTS((3,3),(0.,0.0603252068824628),.UNSPECIFIED.)
CURVE()
GEOMETRIC_REPRESENTATION_ITEM()
RATIONAL_B_SPLINE_CURVE((1.,1.00059701757151,1.00061461981393))
REPRESENTATION_ITEM('')
);
#270=(
BOUNDED_CURVE()
B_SPLINE_CURVE(2,(#98115,#98116,#98117),.UNSPECIFIED.,.F.,.F.)
B_SPLINE_CURVE_WITH_KNOTS((3,3),(0.0639904841458699,0.124315691028302),
 .UNSPECIFIED.)
CURVE()
GEOMETRIC_REPRESENTATION_ITEM()
RATIONAL_B_SPLINE_CURVE((1.000614619814,1.00059701757158,1.))
REPRESENTATION_ITEM('')
);
#271=(
BOUNDED_CURVE()
B_SPLINE_CURVE(2,(#98121,#98122,#98123),.UNSPECIFIED.,.F.,.F.)
B_SPLINE_CURVE_WITH_KNOTS((3,3),(0.,0.0603252068824368),.UNSPECIFIED.)
CURVE()
GEOMETRIC_REPRESENTATION_ITEM()
RATIONAL_B_SPLINE_CURVE((1.,1.00059701757288,1.00061461981535))
REPRESENTATION_ITEM('')
);
#272=(
BOUNDED_CURVE()
B_SPLINE_CURVE(2,(#98125,#98126,#98127),.UNSPECIFIED.,.F.,.F.)
B_SPLINE_CURVE_WITH_KNOTS((3,3),(0.0639904841458755,0.124315691028302),
 .UNSPECIFIED.)
CURVE()
GEOMETRIC_REPRESENTATION_ITEM()
RATIONAL_B_SPLINE_CURVE((1.00061461981817,1.00059701757562,1.))
REPRESENTATION_ITEM('')
);
#273=(
BOUNDED_CURVE()
B_SPLINE_CURVE(2,(#98131,#98132,#98133),.UNSPECIFIED.,.F.,.F.)
B_SPLINE_CURVE_WITH_KNOTS((3,3),(0.,0.0603252068823799),.UNSPECIFIED.)
CURVE()
GEOMETRIC_REPRESENTATION_ITEM()
RATIONAL_B_SPLINE_CURVE((1.,1.00059701757321,1.00061461981569))
REPRESENTATION_ITEM('')
);
#274=(
BOUNDED_CURVE()
B_SPLINE_CURVE(2,(#98135,#98136,#98137),.UNSPECIFIED.,.F.,.F.)
B_SPLINE_CURVE_WITH_KNOTS((3,3),(0.0639904841458814,0.1243156910283),
 .UNSPECIFIED.)
CURVE()
GEOMETRIC_REPRESENTATION_ITEM()
RATIONAL_B_SPLINE_CURVE((1.00061461981777,1.00059701757523,1.))
REPRESENTATION_ITEM('')
);
#275=(
BOUNDED_CURVE()
B_SPLINE_CURVE(2,(#98141,#98142,#98143),.UNSPECIFIED.,.F.,.F.)
B_SPLINE_CURVE_WITH_KNOTS((3,3),(0.,0.0603252068824466),.UNSPECIFIED.)
CURVE()
GEOMETRIC_REPRESENTATION_ITEM()
RATIONAL_B_SPLINE_CURVE((1.,1.0005970175777,1.00061461982031))
REPRESENTATION_ITEM('')
);
#276=(
BOUNDED_CURVE()
B_SPLINE_CURVE(2,(#98145,#98146,#98147),.UNSPECIFIED.,.F.,.F.)
B_SPLINE_CURVE_WITH_KNOTS((3,3),(0.0639904841458398,0.124315691028299),
 .UNSPECIFIED.)
CURVE()
GEOMETRIC_REPRESENTATION_ITEM()
RATIONAL_B_SPLINE_CURVE((1.00061461981638,1.00059701757389,1.))
REPRESENTATION_ITEM('')
);
#277=(
BOUNDED_CURVE()
B_SPLINE_CURVE(2,(#98151,#98152,#98153),.UNSPECIFIED.,.F.,.F.)
B_SPLINE_CURVE_WITH_KNOTS((3,3),(0.,0.06032520688241),.UNSPECIFIED.)
CURVE()
GEOMETRIC_REPRESENTATION_ITEM()
RATIONAL_B_SPLINE_CURVE((1.,1.00059701757236,1.00061461981481))
REPRESENTATION_ITEM('')
);
#278=(
BOUNDED_CURVE()
B_SPLINE_CURVE(2,(#98155,#98156,#98157),.UNSPECIFIED.,.F.,.F.)
B_SPLINE_CURVE_WITH_KNOTS((3,3),(0.0639904841458318,0.124315691028302),
 .UNSPECIFIED.)
CURVE()
GEOMETRIC_REPRESENTATION_ITEM()
RATIONAL_B_SPLINE_CURVE((1.00061461981596,1.00059701757347,1.))
REPRESENTATION_ITEM('')
);
#279=(
BOUNDED_CURVE()
B_SPLINE_CURVE(2,(#98161,#98162,#98163),.UNSPECIFIED.,.F.,.F.)
B_SPLINE_CURVE_WITH_KNOTS((3,3),(0.,0.0603252068823898),.UNSPECIFIED.)
CURVE()
GEOMETRIC_REPRESENTATION_ITEM()
RATIONAL_B_SPLINE_CURVE((1.,1.00059701757645,1.00061461981902))
REPRESENTATION_ITEM('')
);
#280=(
BOUNDED_CURVE()
B_SPLINE_CURVE(2,(#98165,#98166,#98167),.UNSPECIFIED.,.F.,.F.)
B_SPLINE_CURVE_WITH_KNOTS((3,3),(0.0639904841459118,0.1243156910283),
 .UNSPECIFIED.)
CURVE()
GEOMETRIC_REPRESENTATION_ITEM()
RATIONAL_B_SPLINE_CURVE((1.00061461981901,1.00059701757644,1.))
REPRESENTATION_ITEM('')
);
#281=(
BOUNDED_CURVE()
B_SPLINE_CURVE(2,(#98171,#98172,#98173),.UNSPECIFIED.,.F.,.F.)
B_SPLINE_CURVE_WITH_KNOTS((3,3),(0.,0.0603252068824294),.UNSPECIFIED.)
CURVE()
GEOMETRIC_REPRESENTATION_ITEM()
RATIONAL_B_SPLINE_CURVE((1.,1.00059701757539,1.00061461981793))
REPRESENTATION_ITEM('')
);
#282=(
BOUNDED_CURVE()
B_SPLINE_CURVE(2,(#98175,#98176,#98177),.UNSPECIFIED.,.F.,.F.)
B_SPLINE_CURVE_WITH_KNOTS((3,3),(0.0639904841458455,0.1243156910283),
 .UNSPECIFIED.)
CURVE()
GEOMETRIC_REPRESENTATION_ITEM()
RATIONAL_B_SPLINE_CURVE((1.00061461982149,1.00059701757885,1.))
REPRESENTATION_ITEM('')
);
#283=(
BOUNDED_CURVE()
B_SPLINE_CURVE(2,(#98181,#98182,#98183),.UNSPECIFIED.,.F.,.F.)
B_SPLINE_CURVE_WITH_KNOTS((3,3),(0.,0.0603252068824333),.UNSPECIFIED.)
CURVE()
GEOMETRIC_REPRESENTATION_ITEM()
RATIONAL_B_SPLINE_CURVE((1.,1.00059701757328,1.00061461981575))
REPRESENTATION_ITEM('')
);
#284=(
BOUNDED_CURVE()
B_SPLINE_CURVE(2,(#98185,#98186,#98187),.UNSPECIFIED.,.F.,.F.)
B_SPLINE_CURVE_WITH_KNOTS((3,3),(0.0639904841458647,0.124315691028299),
 .UNSPECIFIED.)
CURVE()
GEOMETRIC_REPRESENTATION_ITEM()
RATIONAL_B_SPLINE_CURVE((1.00061461981117,1.00059701756882,1.))
REPRESENTATION_ITEM('')
);
#285=(
BOUNDED_CURVE()
B_SPLINE_CURVE(2,(#98191,#98192,#98193),.UNSPECIFIED.,.F.,.F.)
B_SPLINE_CURVE_WITH_KNOTS((3,3),(0.,0.060325206882429),.UNSPECIFIED.)
CURVE()
GEOMETRIC_REPRESENTATION_ITEM()
RATIONAL_B_SPLINE_CURVE((1.,1.00059701757149,1.00061461981392))
REPRESENTATION_ITEM('')
);
#286=(
BOUNDED_CURVE()
B_SPLINE_CURVE(2,(#98195,#98196,#98197),.UNSPECIFIED.,.F.,.F.)
B_SPLINE_CURVE_WITH_KNOTS((3,3),(0.0639904841459033,0.1243156910283),
 .UNSPECIFIED.)
CURVE()
GEOMETRIC_REPRESENTATION_ITEM()
RATIONAL_B_SPLINE_CURVE((1.00061461981837,1.00059701757582,1.))
REPRESENTATION_ITEM('')
);
#287=(
BOUNDED_CURVE()
B_SPLINE_CURVE(2,(#98201,#98202,#98203),.UNSPECIFIED.,.F.,.F.)
B_SPLINE_CURVE_WITH_KNOTS((3,3),(0.,0.0603252068824625),.UNSPECIFIED.)
CURVE()
GEOMETRIC_REPRESENTATION_ITEM()
RATIONAL_B_SPLINE_CURVE((1.,1.00059701757607,1.00061461981863))
REPRESENTATION_ITEM('')
);
#288=(
BOUNDED_CURVE()
B_SPLINE_CURVE(2,(#98205,#98206,#98207),.UNSPECIFIED.,.F.,.F.)
B_SPLINE_CURVE_WITH_KNOTS((3,3),(0.0639904841458564,0.124315691028299),
 .UNSPECIFIED.)
CURVE()
GEOMETRIC_REPRESENTATION_ITEM()
RATIONAL_B_SPLINE_CURVE((1.00061461981741,1.00059701757488,1.))
REPRESENTATION_ITEM('')
);
#289=(
BOUNDED_CURVE()
B_SPLINE_CURVE(2,(#98211,#98212,#98213),.UNSPECIFIED.,.F.,.F.)
B_SPLINE_CURVE_WITH_KNOTS((3,3),(0.,0.0603252068824167),.UNSPECIFIED.)
CURVE()
GEOMETRIC_REPRESENTATION_ITEM()
RATIONAL_B_SPLINE_CURVE((1.,1.00059701757614,1.0006146198187))
REPRESENTATION_ITEM('')
);
#290=(
BOUNDED_CURVE()
B_SPLINE_CURVE(2,(#98215,#98216,#98217),.UNSPECIFIED.,.F.,.F.)
B_SPLINE_CURVE_WITH_KNOTS((3,3),(0.0639904841458993,0.1243156910283),
 .UNSPECIFIED.)
CURVE()
GEOMETRIC_REPRESENTATION_ITEM()
RATIONAL_B_SPLINE_CURVE((1.00061461981727,1.00059701757475,1.))
REPRESENTATION_ITEM('')
);
#291=(
BOUNDED_CURVE()
B_SPLINE_CURVE(2,(#98221,#98222,#98223),.UNSPECIFIED.,.F.,.F.)
B_SPLINE_CURVE_WITH_KNOTS((3,3),(0.,0.0603252068824493),.UNSPECIFIED.)
CURVE()
GEOMETRIC_REPRESENTATION_ITEM()
RATIONAL_B_SPLINE_CURVE((1.,1.00059701757429,1.00061461981679))
REPRESENTATION_ITEM('')
);
#292=(
BOUNDED_CURVE()
B_SPLINE_CURVE(2,(#98225,#98226,#98227),.UNSPECIFIED.,.F.,.F.)
B_SPLINE_CURVE_WITH_KNOTS((3,3),(0.0639904841458732,0.124315691028301),
 .UNSPECIFIED.)
CURVE()
GEOMETRIC_REPRESENTATION_ITEM()
RATIONAL_B_SPLINE_CURVE((1.00061461981735,1.00059701757483,1.))
REPRESENTATION_ITEM('')
);
#293=(
BOUNDED_CURVE()
B_SPLINE_CURVE(2,(#98241,#98242,#98243),.UNSPECIFIED.,.F.,.F.)
B_SPLINE_CURVE_WITH_KNOTS((3,3),(0.,0.0603252068824331),.UNSPECIFIED.)
CURVE()
GEOMETRIC_REPRESENTATION_ITEM()
RATIONAL_B_SPLINE_CURVE((1.,1.00059701757411,1.00061461981661))
REPRESENTATION_ITEM('')
);
#294=(
BOUNDED_CURVE()
B_SPLINE_CURVE(2,(#98246,#98247,#98248),.UNSPECIFIED.,.F.,.F.)
B_SPLINE_CURVE_WITH_KNOTS((3,3),(0.0639904841458569,0.124315691028302),
 .UNSPECIFIED.)
CURVE()
GEOMETRIC_REPRESENTATION_ITEM()
RATIONAL_B_SPLINE_CURVE((1.00061461981636,1.00059701757387,1.))
REPRESENTATION_ITEM('')
);
#295=(
BOUNDED_CURVE()
B_SPLINE_CURVE(2,(#98259,#98260,#98261),.UNSPECIFIED.,.F.,.F.)
B_SPLINE_CURVE_WITH_KNOTS((3,3),(0.0639904841458384,0.124315691028303),
 .UNSPECIFIED.)
CURVE()
GEOMETRIC_REPRESENTATION_ITEM()
RATIONAL_B_SPLINE_CURVE((1.00061461981704,1.00059701757453,1.))
REPRESENTATION_ITEM('')
);
#296=(
BOUNDED_CURVE()
B_SPLINE_CURVE(2,(#98265,#98266,#98267),.UNSPECIFIED.,.F.,.F.)
B_SPLINE_CURVE_WITH_KNOTS((3,3),(0.,0.060325206882409),.UNSPECIFIED.)
CURVE()
GEOMETRIC_REPRESENTATION_ITEM()
RATIONAL_B_SPLINE_CURVE((1.,1.00059701758008,1.00061461982276))
REPRESENTATION_ITEM('')
);
#297=(
BOUNDED_CURVE()
B_SPLINE_CURVE(2,(#98269,#98270,#98271),.UNSPECIFIED.,.F.,.F.)
B_SPLINE_CURVE_WITH_KNOTS((3,3),(0.0639904841458431,0.124315691028302),
 .UNSPECIFIED.)
CURVE()
GEOMETRIC_REPRESENTATION_ITEM()
RATIONAL_B_SPLINE_CURVE((1.00061461982011,1.0005970175775,1.))
REPRESENTATION_ITEM('')
);
#298=(
BOUNDED_CURVE()
B_SPLINE_CURVE(2,(#98275,#98276,#98277),.UNSPECIFIED.,.F.,.F.)
B_SPLINE_CURVE_WITH_KNOTS((3,3),(0.,0.0603252068824613),.UNSPECIFIED.)
CURVE()
GEOMETRIC_REPRESENTATION_ITEM()
RATIONAL_B_SPLINE_CURVE((1.,1.00059701757306,1.00061461981553))
REPRESENTATION_ITEM('')
);
#299=(
BOUNDED_CURVE()
B_SPLINE_CURVE(2,(#98279,#98280,#98281),.UNSPECIFIED.,.F.,.F.)
B_SPLINE_CURVE_WITH_KNOTS((3,3),(0.0639904841458487,0.124315691028303),
 .UNSPECIFIED.)
CURVE()
GEOMETRIC_REPRESENTATION_ITEM()
RATIONAL_B_SPLINE_CURVE((1.00061461981873,1.00059701757616,1.))
REPRESENTATION_ITEM('')
);
#300=(
BOUNDED_CURVE()
B_SPLINE_CURVE(2,(#98285,#98286,#98287),.UNSPECIFIED.,.F.,.F.)
B_SPLINE_CURVE_WITH_KNOTS((3,3),(0.,0.0603252068824276),.UNSPECIFIED.)
CURVE()
GEOMETRIC_REPRESENTATION_ITEM()
RATIONAL_B_SPLINE_CURVE((1.,1.00059701757807,1.00061461982069))
REPRESENTATION_ITEM('')
);
#301=(
BOUNDED_CURVE()
B_SPLINE_CURVE(2,(#98289,#98290,#98291),.UNSPECIFIED.,.F.,.F.)
B_SPLINE_CURVE_WITH_KNOTS((3,3),(0.0639904841458727,0.124315691028301),
 .UNSPECIFIED.)
CURVE()
GEOMETRIC_REPRESENTATION_ITEM()
RATIONAL_B_SPLINE_CURVE((1.00061461981734,1.00059701757482,1.))
REPRESENTATION_ITEM('')
);
#302=(
BOUNDED_CURVE()
B_SPLINE_CURVE(2,(#98295,#98296,#98297),.UNSPECIFIED.,.F.,.F.)
B_SPLINE_CURVE_WITH_KNOTS((3,3),(0.,0.0603252068823914),.UNSPECIFIED.)
CURVE()
GEOMETRIC_REPRESENTATION_ITEM()
RATIONAL_B_SPLINE_CURVE((1.,1.00059701757592,1.00061461981848))
REPRESENTATION_ITEM('')
);
#303=(
BOUNDED_CURVE()
B_SPLINE_CURVE(2,(#98299,#98300,#98301),.UNSPECIFIED.,.F.,.F.)
B_SPLINE_CURVE_WITH_KNOTS((3,3),(0.063990484145862,0.124315691028302),
 .UNSPECIFIED.)
CURVE()
GEOMETRIC_REPRESENTATION_ITEM()
RATIONAL_B_SPLINE_CURVE((1.00061461982072,1.0005970175781,1.))
REPRESENTATION_ITEM('')
);
#304=(
BOUNDED_CURVE()
B_SPLINE_CURVE(2,(#98305,#98306,#98307),.UNSPECIFIED.,.F.,.F.)
B_SPLINE_CURVE_WITH_KNOTS((3,3),(0.,0.0603252068824525),.UNSPECIFIED.)
CURVE()
GEOMETRIC_REPRESENTATION_ITEM()
RATIONAL_B_SPLINE_CURVE((1.,1.00059701757595,1.00061461981851))
REPRESENTATION_ITEM('')
);
#305=(
BOUNDED_CURVE()
B_SPLINE_CURVE(2,(#98309,#98310,#98311),.UNSPECIFIED.,.F.,.F.)
B_SPLINE_CURVE_WITH_KNOTS((3,3),(0.0639904841458752,0.124315691028301),
 .UNSPECIFIED.)
CURVE()
GEOMETRIC_REPRESENTATION_ITEM()
RATIONAL_B_SPLINE_CURVE((1.00061461981711,1.0005970175746,1.))
REPRESENTATION_ITEM('')
);
#306=(
BOUNDED_CURVE()
B_SPLINE_CURVE(2,(#98315,#98316,#98317),.UNSPECIFIED.,.F.,.F.)
B_SPLINE_CURVE_WITH_KNOTS((3,3),(0.,0.0603252068824554),.UNSPECIFIED.)
CURVE()
GEOMETRIC_REPRESENTATION_ITEM()
RATIONAL_B_SPLINE_CURVE((1.,1.00059701757617,1.00061461981873))
REPRESENTATION_ITEM('')
);
#307=(
BOUNDED_CURVE()
B_SPLINE_CURVE(2,(#98319,#98320,#98321),.UNSPECIFIED.,.F.,.F.)
B_SPLINE_CURVE_WITH_KNOTS((3,3),(0.0639904841458758,0.124315691028301),
 .UNSPECIFIED.)
CURVE()
GEOMETRIC_REPRESENTATION_ITEM()
RATIONAL_B_SPLINE_CURVE((1.00061461982041,1.0005970175778,1.))
REPRESENTATION_ITEM('')
);
#308=(
BOUNDED_CURVE()
B_SPLINE_CURVE(2,(#98325,#98326,#98327),.UNSPECIFIED.,.F.,.F.)
B_SPLINE_CURVE_WITH_KNOTS((3,3),(0.,0.0603252068824492),.UNSPECIFIED.)
CURVE()
GEOMETRIC_REPRESENTATION_ITEM()
RATIONAL_B_SPLINE_CURVE((1.,1.00059701757446,1.00061461981697))
REPRESENTATION_ITEM('')
);
#309=(
BOUNDED_CURVE()
B_SPLINE_CURVE(2,(#98329,#98330,#98331),.UNSPECIFIED.,.F.,.F.)
B_SPLINE_CURVE_WITH_KNOTS((3,3),(0.0639904841458399,0.124315691028302),
 .UNSPECIFIED.)
CURVE()
GEOMETRIC_REPRESENTATION_ITEM()
RATIONAL_B_SPLINE_CURVE((1.00061461981953,1.00059701757694,1.))
REPRESENTATION_ITEM('')
);
#310=(
BOUNDED_CURVE()
B_SPLINE_CURVE(2,(#98335,#98336,#98337),.UNSPECIFIED.,.F.,.F.)
B_SPLINE_CURVE_WITH_KNOTS((3,3),(0.,0.060325206882422),.UNSPECIFIED.)
CURVE()
GEOMETRIC_REPRESENTATION_ITEM()
RATIONAL_B_SPLINE_CURVE((1.,1.00059701757302,1.00061461981549))
REPRESENTATION_ITEM('')
);
#311=(
BOUNDED_CURVE()
B_SPLINE_CURVE(2,(#98339,#98340,#98341),.UNSPECIFIED.,.F.,.F.)
B_SPLINE_CURVE_WITH_KNOTS((3,3),(0.0639904841458821,0.124315691028301),
 .UNSPECIFIED.)
CURVE()
GEOMETRIC_REPRESENTATION_ITEM()
RATIONAL_B_SPLINE_CURVE((1.00061461982,1.0005970175774,1.))
REPRESENTATION_ITEM('')
);
#312=(
BOUNDED_CURVE()
B_SPLINE_CURVE(2,(#98345,#98346,#98347),.UNSPECIFIED.,.F.,.F.)
B_SPLINE_CURVE_WITH_KNOTS((3,3),(0.,0.060325206882426),.UNSPECIFIED.)
CURVE()
GEOMETRIC_REPRESENTATION_ITEM()
RATIONAL_B_SPLINE_CURVE((1.,1.0005970175762,1.00061461981876))
REPRESENTATION_ITEM('')
);
#313=(
BOUNDED_CURVE()
B_SPLINE_CURVE(2,(#98349,#98350,#98351),.UNSPECIFIED.,.F.,.F.)
B_SPLINE_CURVE_WITH_KNOTS((3,3),(0.0639904841458618,0.124315691028301),
 .UNSPECIFIED.)
CURVE()
GEOMETRIC_REPRESENTATION_ITEM()
RATIONAL_B_SPLINE_CURVE((1.00061461981851,1.00059701757596,1.))
REPRESENTATION_ITEM('')
);
#314=(
BOUNDED_CURVE()
B_SPLINE_CURVE(2,(#98355,#98356,#98357),.UNSPECIFIED.,.F.,.F.)
B_SPLINE_CURVE_WITH_KNOTS((3,3),(0.,0.060325206882439),.UNSPECIFIED.)
CURVE()
GEOMETRIC_REPRESENTATION_ITEM()
RATIONAL_B_SPLINE_CURVE((1.,1.000597017576,1.00061461981855))
REPRESENTATION_ITEM('')
);
#315=(
BOUNDED_CURVE()
B_SPLINE_CURVE(2,(#98359,#98360,#98361),.UNSPECIFIED.,.F.,.F.)
B_SPLINE_CURVE_WITH_KNOTS((3,3),(0.0639904841458451,0.124315691028302),
 .UNSPECIFIED.)
CURVE()
GEOMETRIC_REPRESENTATION_ITEM()
RATIONAL_B_SPLINE_CURVE((1.00061461981588,1.0005970175734,1.))
REPRESENTATION_ITEM('')
);
#316=(
BOUNDED_CURVE()
B_SPLINE_CURVE(2,(#98365,#98366,#98367),.UNSPECIFIED.,.F.,.F.)
B_SPLINE_CURVE_WITH_KNOTS((3,3),(0.,0.0603252068824284),.UNSPECIFIED.)
CURVE()
GEOMETRIC_REPRESENTATION_ITEM()
RATIONAL_B_SPLINE_CURVE((1.,1.0005970175755,1.00061461981804))
REPRESENTATION_ITEM('')
);
#317=(
BOUNDED_CURVE()
B_SPLINE_CURVE(2,(#98369,#98370,#98371),.UNSPECIFIED.,.F.,.F.)
B_SPLINE_CURVE_WITH_KNOTS((3,3),(0.063990484145897,0.124315691028301),
 .UNSPECIFIED.)
CURVE()
GEOMETRIC_REPRESENTATION_ITEM()
RATIONAL_B_SPLINE_CURVE((1.00061461982066,1.00059701757804,1.))
REPRESENTATION_ITEM('')
);
#318=(
BOUNDED_CURVE()
B_SPLINE_CURVE(2,(#98375,#98376,#98377),.UNSPECIFIED.,.F.,.F.)
B_SPLINE_CURVE_WITH_KNOTS((3,3),(0.,0.0603252068824418),.UNSPECIFIED.)
CURVE()
GEOMETRIC_REPRESENTATION_ITEM()
RATIONAL_B_SPLINE_CURVE((1.,1.00059701757692,1.00061461981951))
REPRESENTATION_ITEM('')
);
#319=(
BOUNDED_CURVE()
B_SPLINE_CURVE(2,(#98379,#98380,#98381),.UNSPECIFIED.,.F.,.F.)
B_SPLINE_CURVE_WITH_KNOTS((3,3),(0.063990484145828,0.124315691028302),
 .UNSPECIFIED.)
CURVE()
GEOMETRIC_REPRESENTATION_ITEM()
RATIONAL_B_SPLINE_CURVE((1.00061461982019,1.00059701757759,1.))
REPRESENTATION_ITEM('')
);
#320=(
BOUNDED_CURVE()
B_SPLINE_CURVE(2,(#98385,#98386,#98387),.UNSPECIFIED.,.F.,.F.)
B_SPLINE_CURVE_WITH_KNOTS((3,3),(0.,0.0603252068824602),.UNSPECIFIED.)
CURVE()
GEOMETRIC_REPRESENTATION_ITEM()
RATIONAL_B_SPLINE_CURVE((1.,1.00059701757713,1.00061461981972))
REPRESENTATION_ITEM('')
);
#321=(
BOUNDED_CURVE()
B_SPLINE_CURVE(2,(#98389,#98390,#98391),.UNSPECIFIED.,.F.,.F.)
B_SPLINE_CURVE_WITH_KNOTS((3,3),(0.0639904841458735,0.124315691028303),
 .UNSPECIFIED.)
CURVE()
GEOMETRIC_REPRESENTATION_ITEM()
RATIONAL_B_SPLINE_CURVE((1.00061461982132,1.00059701757868,1.))
REPRESENTATION_ITEM('')
);
#322=(
BOUNDED_CURVE()
B_SPLINE_CURVE(2,(#98395,#98396,#98397),.UNSPECIFIED.,.F.,.F.)
B_SPLINE_CURVE_WITH_KNOTS((3,3),(0.,0.060325206882423),.UNSPECIFIED.)
CURVE()
GEOMETRIC_REPRESENTATION_ITEM()
RATIONAL_B_SPLINE_CURVE((1.,1.00059701757739,1.00061461981999))
REPRESENTATION_ITEM('')
);
#323=(
BOUNDED_CURVE()
B_SPLINE_CURVE(2,(#98399,#98400,#98401),.UNSPECIFIED.,.F.,.F.)
B_SPLINE_CURVE_WITH_KNOTS((3,3),(0.0639904841458232,0.124315691028303),
 .UNSPECIFIED.)
CURVE()
GEOMETRIC_REPRESENTATION_ITEM()
RATIONAL_B_SPLINE_CURVE((1.00061461981322,1.00059701757082,1.))
REPRESENTATION_ITEM('')
);
#324=(
BOUNDED_CURVE()
B_SPLINE_CURVE(2,(#98405,#98406,#98407),.UNSPECIFIED.,.F.,.F.)
B_SPLINE_CURVE_WITH_KNOTS((3,3),(0.,0.0603252068824245),.UNSPECIFIED.)
CURVE()
GEOMETRIC_REPRESENTATION_ITEM()
RATIONAL_B_SPLINE_CURVE((1.,1.0005970175778,1.00061461982041))
REPRESENTATION_ITEM('')
);
#325=(
BOUNDED_CURVE()
B_SPLINE_CURVE(2,(#98409,#98410,#98411),.UNSPECIFIED.,.F.,.F.)
B_SPLINE_CURVE_WITH_KNOTS((3,3),(0.0639904841458354,0.124315691028301),
 .UNSPECIFIED.)
CURVE()
GEOMETRIC_REPRESENTATION_ITEM()
RATIONAL_B_SPLINE_CURVE((1.00061461981561,1.00059701757313,1.))
REPRESENTATION_ITEM('')
);
#326=(
BOUNDED_CURVE()
B_SPLINE_CURVE(2,(#98415,#98416,#98417),.UNSPECIFIED.,.F.,.F.)
B_SPLINE_CURVE_WITH_KNOTS((3,3),(0.,0.0603252068824727),.UNSPECIFIED.)
CURVE()
GEOMETRIC_REPRESENTATION_ITEM()
RATIONAL_B_SPLINE_CURVE((1.,1.00059701757521,1.00061461981774))
REPRESENTATION_ITEM('')
);
#327=(
BOUNDED_CURVE()
B_SPLINE_CURVE(2,(#98419,#98420,#98421),.UNSPECIFIED.,.F.,.F.)
B_SPLINE_CURVE_WITH_KNOTS((3,3),(0.0639904841458599,0.124315691028302),
 .UNSPECIFIED.)
CURVE()
GEOMETRIC_REPRESENTATION_ITEM()
RATIONAL_B_SPLINE_CURVE((1.00061461981724,1.00059701757472,1.))
REPRESENTATION_ITEM('')
);
#328=(
BOUNDED_CURVE()
B_SPLINE_CURVE(2,(#98425,#98426,#98427),.UNSPECIFIED.,.F.,.F.)
B_SPLINE_CURVE_WITH_KNOTS((3,3),(0.,0.060325206882435),.UNSPECIFIED.)
CURVE()
GEOMETRIC_REPRESENTATION_ITEM()
RATIONAL_B_SPLINE_CURVE((1.,1.000597017572,1.00061461981444))
REPRESENTATION_ITEM('')
);
#329=(
BOUNDED_CURVE()
B_SPLINE_CURVE(2,(#98428,#98429,#98430),.UNSPECIFIED.,.F.,.F.)
B_SPLINE_CURVE_WITH_KNOTS((3,3),(0.0639904841458783,0.124315691028301),
 .UNSPECIFIED.)
CURVE()
GEOMETRIC_REPRESENTATION_ITEM()
RATIONAL_B_SPLINE_CURVE((1.00061461981787,1.00059701757533,1.))
REPRESENTATION_ITEM('')
);
#330=(
BOUNDED_CURVE()
B_SPLINE_CURVE(2,(#98432,#98433,#98434),.UNSPECIFIED.,.F.,.F.)
B_SPLINE_CURVE_WITH_KNOTS((3,3),(0.,0.0603252068824676),.UNSPECIFIED.)
CURVE()
GEOMETRIC_REPRESENTATION_ITEM()
RATIONAL_B_SPLINE_CURVE((1.,1.00059701757413,1.00061461981663))
REPRESENTATION_ITEM('')
);
#331=(
BOUNDED_CURVE()
B_SPLINE_CURVE(2,(#98436,#98437,#98438),.UNSPECIFIED.,.F.,.F.)
B_SPLINE_CURVE_WITH_KNOTS((3,3),(0.0639904841458132,0.124315691028303),
 .UNSPECIFIED.)
CURVE()
GEOMETRIC_REPRESENTATION_ITEM()
RATIONAL_B_SPLINE_CURVE((1.00061461981527,1.0005970175728,1.))
REPRESENTATION_ITEM('')
);
#332=(
BOUNDED_CURVE()
B_SPLINE_CURVE(2,(#98442,#98443,#98444),.UNSPECIFIED.,.F.,.F.)
B_SPLINE_CURVE_WITH_KNOTS((3,3),(0.,0.0603252068824029),.UNSPECIFIED.)
CURVE()
GEOMETRIC_REPRESENTATION_ITEM()
RATIONAL_B_SPLINE_CURVE((1.,1.00059701757378,1.00061461981628))
REPRESENTATION_ITEM('')
);
#333=(
BOUNDED_CURVE()
B_SPLINE_CURVE(2,(#98446,#98447,#98448),.UNSPECIFIED.,.F.,.F.)
B_SPLINE_CURVE_WITH_KNOTS((3,3),(0.0639904841458425,0.124315691028302),
 .UNSPECIFIED.)
CURVE()
GEOMETRIC_REPRESENTATION_ITEM()
RATIONAL_B_SPLINE_CURVE((1.0006146198229,1.00059701758022,1.))
REPRESENTATION_ITEM('')
);
#334=(
BOUNDED_CURVE()
B_SPLINE_CURVE(2,(#98452,#98453,#98454),.UNSPECIFIED.,.F.,.F.)
B_SPLINE_CURVE_WITH_KNOTS((3,3),(0.,0.0603252068824536),.UNSPECIFIED.)
CURVE()
GEOMETRIC_REPRESENTATION_ITEM()
RATIONAL_B_SPLINE_CURVE((1.,1.00059701757467,1.00061461981719))
REPRESENTATION_ITEM('')
);
#335=(
BOUNDED_CURVE()
B_SPLINE_CURVE(2,(#98456,#98457,#98458),.UNSPECIFIED.,.F.,.F.)
B_SPLINE_CURVE_WITH_KNOTS((3,3),(0.0639904841458365,0.124315691028303),
 .UNSPECIFIED.)
CURVE()
GEOMETRIC_REPRESENTATION_ITEM()
RATIONAL_B_SPLINE_CURVE((1.00061461981477,1.00059701757232,1.))
REPRESENTATION_ITEM('')
);
#336=(
BOUNDED_CURVE()
B_SPLINE_CURVE(2,(#98462,#98463,#98464),.UNSPECIFIED.,.F.,.F.)
B_SPLINE_CURVE_WITH_KNOTS((3,3),(0.,0.0603252068824354),.UNSPECIFIED.)
CURVE()
GEOMETRIC_REPRESENTATION_ITEM()
RATIONAL_B_SPLINE_CURVE((1.,1.00059701758002,1.0006146198227))
REPRESENTATION_ITEM('')
);
#337=(
BOUNDED_CURVE()
B_SPLINE_CURVE(2,(#98466,#98467,#98468),.UNSPECIFIED.,.F.,.F.)
B_SPLINE_CURVE_WITH_KNOTS((3,3),(0.0639904841458278,0.124315691028302),
 .UNSPECIFIED.)
CURVE()
GEOMETRIC_REPRESENTATION_ITEM()
RATIONAL_B_SPLINE_CURVE((1.00061461981225,1.00059701756987,1.))
REPRESENTATION_ITEM('')
);
#338=(
BOUNDED_CURVE()
B_SPLINE_CURVE(2,(#98472,#98473,#98474),.UNSPECIFIED.,.F.,.F.)
B_SPLINE_CURVE_WITH_KNOTS((3,3),(0.,0.0603252068824639),.UNSPECIFIED.)
CURVE()
GEOMETRIC_REPRESENTATION_ITEM()
RATIONAL_B_SPLINE_CURVE((1.,1.000597017572,1.00061461981444))
REPRESENTATION_ITEM('')
);
#339=(
BOUNDED_CURVE()
B_SPLINE_CURVE(2,(#98476,#98477,#98478),.UNSPECIFIED.,.F.,.F.)
B_SPLINE_CURVE_WITH_KNOTS((3,3),(0.0639904841458256,0.124315691028302),
 .UNSPECIFIED.)
CURVE()
GEOMETRIC_REPRESENTATION_ITEM()
RATIONAL_B_SPLINE_CURVE((1.00061461981674,1.00059701757424,1.))
REPRESENTATION_ITEM('')
);
#340=(
BOUNDED_CURVE()
B_SPLINE_CURVE(2,(#98482,#98483,#98484),.UNSPECIFIED.,.F.,.F.)
B_SPLINE_CURVE_WITH_KNOTS((3,3),(0.,0.0603252068824755),.UNSPECIFIED.)
CURVE()
GEOMETRIC_REPRESENTATION_ITEM()
RATIONAL_B_SPLINE_CURVE((1.,1.00059701757238,1.00061461981483))
REPRESENTATION_ITEM('')
);
#341=(
BOUNDED_CURVE()
B_SPLINE_CURVE(2,(#98486,#98487,#98488),.UNSPECIFIED.,.F.,.F.)
B_SPLINE_CURVE_WITH_KNOTS((3,3),(0.0639904841458611,0.124315691028301),
 .UNSPECIFIED.)
CURVE()
GEOMETRIC_REPRESENTATION_ITEM()
RATIONAL_B_SPLINE_CURVE((1.00061461981833,1.00059701757578,1.))
REPRESENTATION_ITEM('')
);
#342=(
BOUNDED_CURVE()
B_SPLINE_CURVE(2,(#98492,#98493,#98494),.UNSPECIFIED.,.F.,.F.)
B_SPLINE_CURVE_WITH_KNOTS((3,3),(0.,0.0603252068824602),.UNSPECIFIED.)
CURVE()
GEOMETRIC_REPRESENTATION_ITEM()
RATIONAL_B_SPLINE_CURVE((1.,1.00059701757416,1.00061461981667))
REPRESENTATION_ITEM('')
);
#343=(
BOUNDED_CURVE()
B_SPLINE_CURVE(2,(#98496,#98497,#98498),.UNSPECIFIED.,.F.,.F.)
B_SPLINE_CURVE_WITH_KNOTS((3,3),(0.063990484145903,0.124315691028301),
 .UNSPECIFIED.)
CURVE()
GEOMETRIC_REPRESENTATION_ITEM()
RATIONAL_B_SPLINE_CURVE((1.00061461981856,1.00059701757601,1.))
REPRESENTATION_ITEM('')
);
#344=(
BOUNDED_CURVE()
B_SPLINE_CURVE(2,(#98502,#98503,#98504),.UNSPECIFIED.,.F.,.F.)
B_SPLINE_CURVE_WITH_KNOTS((3,3),(0.,0.060325206882481),.UNSPECIFIED.)
CURVE()
GEOMETRIC_REPRESENTATION_ITEM()
RATIONAL_B_SPLINE_CURVE((1.,1.00059701757576,1.00061461981831))
REPRESENTATION_ITEM('')
);
#345=(
BOUNDED_CURVE()
B_SPLINE_CURVE(2,(#98506,#98507,#98508),.UNSPECIFIED.,.F.,.F.)
B_SPLINE_CURVE_WITH_KNOTS((3,3),(0.0639904841458541,0.124315691028302),
 .UNSPECIFIED.)
CURVE()
GEOMETRIC_REPRESENTATION_ITEM()
RATIONAL_B_SPLINE_CURVE((1.00061461982049,1.00059701757788,1.))
REPRESENTATION_ITEM('')
);
#346=(
BOUNDED_CURVE()
B_SPLINE_CURVE(2,(#98512,#98513,#98514),.UNSPECIFIED.,.F.,.F.)
B_SPLINE_CURVE_WITH_KNOTS((3,3),(0.,0.0603252068824261),.UNSPECIFIED.)
CURVE()
GEOMETRIC_REPRESENTATION_ITEM()
RATIONAL_B_SPLINE_CURVE((1.,1.00059701757482,1.00061461981734))
REPRESENTATION_ITEM('')
);
#347=(
BOUNDED_CURVE()
B_SPLINE_CURVE(2,(#98516,#98517,#98518),.UNSPECIFIED.,.F.,.F.)
B_SPLINE_CURVE_WITH_KNOTS((3,3),(0.0639904841458672,0.124315691028302),
 .UNSPECIFIED.)
CURVE()
GEOMETRIC_REPRESENTATION_ITEM()
RATIONAL_B_SPLINE_CURVE((1.00061461981919,1.00059701757661,1.))
REPRESENTATION_ITEM('')
);
#348=(
BOUNDED_CURVE()
B_SPLINE_CURVE(2,(#98522,#98523,#98524),.UNSPECIFIED.,.F.,.F.)
B_SPLINE_CURVE_WITH_KNOTS((3,3),(0.,0.0603252068824262),.UNSPECIFIED.)
CURVE()
GEOMETRIC_REPRESENTATION_ITEM()
RATIONAL_B_SPLINE_CURVE((1.,1.00059701757468,1.0006146198172))
REPRESENTATION_ITEM('')
);
#349=(
BOUNDED_CURVE()
B_SPLINE_CURVE(2,(#98526,#98527,#98528),.UNSPECIFIED.,.F.,.F.)
B_SPLINE_CURVE_WITH_KNOTS((3,3),(0.0639904841458652,0.124315691028301),
 .UNSPECIFIED.)
CURVE()
GEOMETRIC_REPRESENTATION_ITEM()
RATIONAL_B_SPLINE_CURVE((1.00061461982038,1.00059701757777,1.))
REPRESENTATION_ITEM('')
);
#350=(
BOUNDED_CURVE()
B_SPLINE_CURVE(2,(#98532,#98533,#98534),.UNSPECIFIED.,.F.,.F.)
B_SPLINE_CURVE_WITH_KNOTS((3,3),(0.,0.0603252068824703),.UNSPECIFIED.)
CURVE()
GEOMETRIC_REPRESENTATION_ITEM()
RATIONAL_B_SPLINE_CURVE((1.,1.00059701757448,1.00061461981699))
REPRESENTATION_ITEM('')
);
#351=(
BOUNDED_CURVE()
B_SPLINE_CURVE(2,(#98536,#98537,#98538),.UNSPECIFIED.,.F.,.F.)
B_SPLINE_CURVE_WITH_KNOTS((3,3),(0.0639904841458294,0.124315691028302),
 .UNSPECIFIED.)
CURVE()
GEOMETRIC_REPRESENTATION_ITEM()
RATIONAL_B_SPLINE_CURVE((1.00061461981863,1.00059701757607,1.))
REPRESENTATION_ITEM('')
);
#352=(
BOUNDED_CURVE()
B_SPLINE_CURVE(2,(#98542,#98543,#98544),.UNSPECIFIED.,.F.,.F.)
B_SPLINE_CURVE_WITH_KNOTS((3,3),(0.,0.0603252068824115),.UNSPECIFIED.)
CURVE()
GEOMETRIC_REPRESENTATION_ITEM()
RATIONAL_B_SPLINE_CURVE((1.,1.00059701757804,1.00061461982066))
REPRESENTATION_ITEM('')
);
#353=(
BOUNDED_CURVE()
B_SPLINE_CURVE(2,(#98546,#98547,#98548),.UNSPECIFIED.,.F.,.F.)
B_SPLINE_CURVE_WITH_KNOTS((3,3),(0.0639904841458776,0.124315691028301),
 .UNSPECIFIED.)
CURVE()
GEOMETRIC_REPRESENTATION_ITEM()
RATIONAL_B_SPLINE_CURVE((1.00061461981868,1.00059701757612,1.))
REPRESENTATION_ITEM('')
);
#354=(
BOUNDED_CURVE()
B_SPLINE_CURVE(2,(#98552,#98553,#98554),.UNSPECIFIED.,.F.,.F.)
B_SPLINE_CURVE_WITH_KNOTS((3,3),(0.,0.0603252068824542),.UNSPECIFIED.)
CURVE()
GEOMETRIC_REPRESENTATION_ITEM()
RATIONAL_B_SPLINE_CURVE((1.,1.00059701757636,1.00061461981893))
REPRESENTATION_ITEM('')
);
#355=(
BOUNDED_CURVE()
B_SPLINE_CURVE(2,(#98556,#98557,#98558),.UNSPECIFIED.,.F.,.F.)
B_SPLINE_CURVE_WITH_KNOTS((3,3),(0.0639904841459132,0.124315691028299),
 .UNSPECIFIED.)
CURVE()
GEOMETRIC_REPRESENTATION_ITEM()
RATIONAL_B_SPLINE_CURVE((1.00061461981658,1.00059701757408,1.))
REPRESENTATION_ITEM('')
);
#356=(
BOUNDED_CURVE()
B_SPLINE_CURVE(2,(#98562,#98563,#98564),.UNSPECIFIED.,.F.,.F.)
B_SPLINE_CURVE_WITH_KNOTS((3,3),(0.,0.060325206882438),.UNSPECIFIED.)
CURVE()
GEOMETRIC_REPRESENTATION_ITEM()
RATIONAL_B_SPLINE_CURVE((1.,1.00059701757669,1.00061461981927))
REPRESENTATION_ITEM('')
);
#357=(
BOUNDED_CURVE()
B_SPLINE_CURVE(2,(#98566,#98567,#98568),.UNSPECIFIED.,.F.,.F.)
B_SPLINE_CURVE_WITH_KNOTS((3,3),(0.0639904841458312,0.124315691028303),
 .UNSPECIFIED.)
CURVE()
GEOMETRIC_REPRESENTATION_ITEM()
RATIONAL_B_SPLINE_CURVE((1.00061461982088,1.00059701757825,1.))
REPRESENTATION_ITEM('')
);
#358=(
BOUNDED_CURVE()
B_SPLINE_CURVE(2,(#98572,#98573,#98574),.UNSPECIFIED.,.F.,.F.)
B_SPLINE_CURVE_WITH_KNOTS((3,3),(0.,0.0603252068824436),.UNSPECIFIED.)
CURVE()
GEOMETRIC_REPRESENTATION_ITEM()
RATIONAL_B_SPLINE_CURVE((1.,1.00059701757611,1.00061461981868))
REPRESENTATION_ITEM('')
);
#359=(
BOUNDED_CURVE()
B_SPLINE_CURVE(2,(#98576,#98577,#98578),.UNSPECIFIED.,.F.,.F.)
B_SPLINE_CURVE_WITH_KNOTS((3,3),(0.0639904841458248,0.124315691028303),
 .UNSPECIFIED.)
CURVE()
GEOMETRIC_REPRESENTATION_ITEM()
RATIONAL_B_SPLINE_CURVE((1.00061461981152,1.00059701756916,1.))
REPRESENTATION_ITEM('')
);
#360=(
BOUNDED_CURVE()
B_SPLINE_CURVE(2,(#98582,#98583,#98584),.UNSPECIFIED.,.F.,.F.)
B_SPLINE_CURVE_WITH_KNOTS((3,3),(0.,0.060325206882417),.UNSPECIFIED.)
CURVE()
GEOMETRIC_REPRESENTATION_ITEM()
RATIONAL_B_SPLINE_CURVE((1.,1.00059701758071,1.0006146198234))
REPRESENTATION_ITEM('')
);
#361=(
BOUNDED_CURVE()
B_SPLINE_CURVE(2,(#98586,#98587,#98588),.UNSPECIFIED.,.F.,.F.)
B_SPLINE_CURVE_WITH_KNOTS((3,3),(0.063990484145854,0.124315691028302),
 .UNSPECIFIED.)
CURVE()
GEOMETRIC_REPRESENTATION_ITEM()
RATIONAL_B_SPLINE_CURVE((1.00061461982008,1.00059701757748,1.))
REPRESENTATION_ITEM('')
);
#362=(
BOUNDED_CURVE()
B_SPLINE_CURVE(2,(#98592,#98593,#98594),.UNSPECIFIED.,.F.,.F.)
B_SPLINE_CURVE_WITH_KNOTS((3,3),(0.,0.0603252068824378),.UNSPECIFIED.)
CURVE()
GEOMETRIC_REPRESENTATION_ITEM()
RATIONAL_B_SPLINE_CURVE((1.,1.00059701757204,1.00061461981449))
REPRESENTATION_ITEM('')
);
#363=(
BOUNDED_CURVE()
B_SPLINE_CURVE(2,(#98596,#98597,#98598),.UNSPECIFIED.,.F.,.F.)
B_SPLINE_CURVE_WITH_KNOTS((3,3),(0.0639904841458379,0.124315691028302),
 .UNSPECIFIED.)
CURVE()
GEOMETRIC_REPRESENTATION_ITEM()
RATIONAL_B_SPLINE_CURVE((1.00061461981444,1.000597017572,1.))
REPRESENTATION_ITEM('')
);
#364=(
BOUNDED_CURVE()
B_SPLINE_CURVE(2,(#98602,#98603,#98604),.UNSPECIFIED.,.F.,.F.)
B_SPLINE_CURVE_WITH_KNOTS((3,3),(0.,0.0603252068824703),.UNSPECIFIED.)
CURVE()
GEOMETRIC_REPRESENTATION_ITEM()
RATIONAL_B_SPLINE_CURVE((1.,1.00059701757202,1.00061461981446))
REPRESENTATION_ITEM('')
);
#365=(
BOUNDED_CURVE()
B_SPLINE_CURVE(2,(#98606,#98607,#98608),.UNSPECIFIED.,.F.,.F.)
B_SPLINE_CURVE_WITH_KNOTS((3,3),(0.0639904841458564,0.124315691028301),
 .UNSPECIFIED.)
CURVE()
GEOMETRIC_REPRESENTATION_ITEM()
RATIONAL_B_SPLINE_CURVE((1.00061461982062,1.000597017578,1.))
REPRESENTATION_ITEM('')
);
#366=(
BOUNDED_CURVE()
B_SPLINE_CURVE(2,(#98612,#98613,#98614),.UNSPECIFIED.,.F.,.F.)
B_SPLINE_CURVE_WITH_KNOTS((3,3),(0.,0.0603252068824437),.UNSPECIFIED.)
CURVE()
GEOMETRIC_REPRESENTATION_ITEM()
RATIONAL_B_SPLINE_CURVE((1.,1.00059701757562,1.00061461981817))
REPRESENTATION_ITEM('')
);
#367=(
BOUNDED_CURVE()
B_SPLINE_CURVE(2,(#98616,#98617,#98618),.UNSPECIFIED.,.F.,.F.)
B_SPLINE_CURVE_WITH_KNOTS((3,3),(0.0639904841458463,0.124315691028302),
 .UNSPECIFIED.)
CURVE()
GEOMETRIC_REPRESENTATION_ITEM()
RATIONAL_B_SPLINE_CURVE((1.00061461981433,1.0005970175719,1.))
REPRESENTATION_ITEM('')
);
#368=(
BOUNDED_CURVE()
B_SPLINE_CURVE(2,(#98622,#98623,#98624),.UNSPECIFIED.,.F.,.F.)
B_SPLINE_CURVE_WITH_KNOTS((3,3),(0.,0.0603252068824302),.UNSPECIFIED.)
CURVE()
GEOMETRIC_REPRESENTATION_ITEM()
RATIONAL_B_SPLINE_CURVE((1.,1.00059701757328,1.00061461981576))
REPRESENTATION_ITEM('')
);
#369=(
BOUNDED_CURVE()
B_SPLINE_CURVE(2,(#98626,#98627,#98628),.UNSPECIFIED.,.F.,.F.)
B_SPLINE_CURVE_WITH_KNOTS((3,3),(0.06399048414589,0.1243156910283),
 .UNSPECIFIED.)
CURVE()
GEOMETRIC_REPRESENTATION_ITEM()
RATIONAL_B_SPLINE_CURVE((1.00061461981725,1.00059701757473,1.))
REPRESENTATION_ITEM('')
);
#370=(
BOUNDED_CURVE()
B_SPLINE_CURVE(2,(#98631,#98632,#98633),.UNSPECIFIED.,.F.,.F.)
B_SPLINE_CURVE_WITH_KNOTS((3,3),(0.,0.0603252068825018),.UNSPECIFIED.)
CURVE()
GEOMETRIC_REPRESENTATION_ITEM()
RATIONAL_B_SPLINE_CURVE((1.,1.00059701757198,1.00061461981442))
REPRESENTATION_ITEM('')
);
#371=(
BOUNDED_CURVE()
B_SPLINE_CURVE(2,(#102311,#102312,#102313),.UNSPECIFIED.,.F.,.F.)
B_SPLINE_CURVE_WITH_KNOTS((3,3),(0.,0.017254918292991),.UNSPECIFIED.)
CURVE()
GEOMETRIC_REPRESENTATION_ITEM()
RATIONAL_B_SPLINE_CURVE((1.,1.000650607336,1.))
REPRESENTATION_ITEM('')
);
#372=(
BOUNDED_CURVE()
B_SPLINE_CURVE(2,(#102322,#102323,#102324),.UNSPECIFIED.,.F.,.F.)
B_SPLINE_CURVE_WITH_KNOTS((3,3),(0.,0.0163156879194284),.UNSPECIFIED.)
CURVE()
GEOMETRIC_REPRESENTATION_ITEM()
RATIONAL_B_SPLINE_CURVE((1.,1.00054678992472,1.))
REPRESENTATION_ITEM('')
);
#373=(
BOUNDED_CURVE()
B_SPLINE_CURVE(2,(#102497,#102498,#102499),.UNSPECIFIED.,.F.,.F.)
B_SPLINE_CURVE_WITH_KNOTS((3,3),(0.,0.0163156879194291),.UNSPECIFIED.)
CURVE()
GEOMETRIC_REPRESENTATION_ITEM()
RATIONAL_B_SPLINE_CURVE((1.,1.00054678995706,1.))
REPRESENTATION_ITEM('')
);
#374=(
BOUNDED_CURVE()
B_SPLINE_CURVE(2,(#102508,#102509,#102510),.UNSPECIFIED.,.F.,.F.)
B_SPLINE_CURVE_WITH_KNOTS((3,3),(0.,0.0172549182929911),.UNSPECIFIED.)
CURVE()
GEOMETRIC_REPRESENTATION_ITEM()
RATIONAL_B_SPLINE_CURVE((1.,1.0006506073662,1.))
REPRESENTATION_ITEM('')
);
#375=(
BOUNDED_CURVE()
B_SPLINE_CURVE(2,(#102544,#102545,#102546),.UNSPECIFIED.,.F.,.F.)
B_SPLINE_CURVE_WITH_KNOTS((3,3),(0.,0.252982212813465),.UNSPECIFIED.)
CURVE()
GEOMETRIC_REPRESENTATION_ITEM()
RATIONAL_B_SPLINE_CURVE((1.,1.25000000000004,1.))
REPRESENTATION_ITEM('')
);
#376=(
BOUNDED_CURVE()
B_SPLINE_CURVE(2,(#102557,#102558,#102559),.UNSPECIFIED.,.F.,.F.)
B_SPLINE_CURVE_WITH_KNOTS((3,3),(0.,0.252982212813472),.UNSPECIFIED.)
CURVE()
GEOMETRIC_REPRESENTATION_ITEM()
RATIONAL_B_SPLINE_CURVE((1.,1.24999999999997,1.))
REPRESENTATION_ITEM('')
);
#377=(
BOUNDED_CURVE()
B_SPLINE_CURVE(2,(#102574,#102575,#102576),.UNSPECIFIED.,.F.,.F.)
B_SPLINE_CURVE_WITH_KNOTS((3,3),(0.,0.252982212813472),.UNSPECIFIED.)
CURVE()
GEOMETRIC_REPRESENTATION_ITEM()
RATIONAL_B_SPLINE_CURVE((1.,1.24999999999997,1.))
REPRESENTATION_ITEM('')
);
#378=(
BOUNDED_CURVE()
B_SPLINE_CURVE(2,(#102599,#102600,#102601),.UNSPECIFIED.,.F.,.F.)
B_SPLINE_CURVE_WITH_KNOTS((3,3),(0.,0.252982212813465),.UNSPECIFIED.)
CURVE()
GEOMETRIC_REPRESENTATION_ITEM()
RATIONAL_B_SPLINE_CURVE((1.,1.25000000000004,1.))
REPRESENTATION_ITEM('')
);
#379=(
BOUNDED_CURVE()
B_SPLINE_CURVE(2,(#104379,#104380,#104381),.UNSPECIFIED.,.F.,.F.)
B_SPLINE_CURVE_WITH_KNOTS((3,3),(0.,0.0570518843466932),.UNSPECIFIED.)
CURVE()
GEOMETRIC_REPRESENTATION_ITEM()
RATIONAL_B_SPLINE_CURVE((1.,1.00190501274853,1.))
REPRESENTATION_ITEM('')
);
#380=(
BOUNDED_CURVE()
B_SPLINE_CURVE(2,(#104384,#104385,#104386),.UNSPECIFIED.,.F.,.F.)
B_SPLINE_CURVE_WITH_KNOTS((3,3),(0.,0.0570518843466932),.UNSPECIFIED.)
CURVE()
GEOMETRIC_REPRESENTATION_ITEM()
RATIONAL_B_SPLINE_CURVE((1.,1.00190501274853,1.))
REPRESENTATION_ITEM('')
);
#381=(
BOUNDED_CURVE()
B_SPLINE_CURVE(2,(#104392,#104393,#104394),.UNSPECIFIED.,.F.,.F.)
B_SPLINE_CURVE_WITH_KNOTS((3,3),(0.,0.0570518843466932),.UNSPECIFIED.)
CURVE()
GEOMETRIC_REPRESENTATION_ITEM()
RATIONAL_B_SPLINE_CURVE((1.,1.00190501272047,1.))
REPRESENTATION_ITEM('')
);
#382=(
BOUNDED_CURVE()
B_SPLINE_CURVE(2,(#104398,#104399,#104400),.UNSPECIFIED.,.F.,.F.)
B_SPLINE_CURVE_WITH_KNOTS((3,3),(0.,0.0570518843466932),.UNSPECIFIED.)
CURVE()
GEOMETRIC_REPRESENTATION_ITEM()
RATIONAL_B_SPLINE_CURVE((1.,1.00190501272047,1.))
REPRESENTATION_ITEM('')
);
#383=(
BOUNDED_CURVE()
B_SPLINE_CURVE(2,(#105405,#105406,#105407),.UNSPECIFIED.,.F.,.F.)
B_SPLINE_CURVE_WITH_KNOTS((3,3),(0.,0.0136874154102675),.UNSPECIFIED.)
CURVE()
GEOMETRIC_REPRESENTATION_ITEM()
RATIONAL_B_SPLINE_CURVE((1.,1.00669106236177,1.00897713804878))
REPRESENTATION_ITEM('')
);
#384=(
BOUNDED_CURVE()
B_SPLINE_CURVE(2,(#105411,#105412,#105413),.UNSPECIFIED.,.F.,.F.)
B_SPLINE_CURVE_WITH_KNOTS((3,3),(0.0278942541126669,0.0415816695229366),
 .UNSPECIFIED.)
CURVE()
GEOMETRIC_REPRESENTATION_ITEM()
RATIONAL_B_SPLINE_CURVE((1.0089771380491,1.00669106236202,1.))
REPRESENTATION_ITEM('')
);
#385=(
BOUNDED_CURVE()
B_SPLINE_CURVE(2,(#105415,#105416,#105417),.UNSPECIFIED.,.F.,.F.)
B_SPLINE_CURVE_WITH_KNOTS((3,3),(0.,0.013687415410265),.UNSPECIFIED.)
CURVE()
GEOMETRIC_REPRESENTATION_ITEM()
RATIONAL_B_SPLINE_CURVE((1.,1.00669106236252,1.00897713804979))
REPRESENTATION_ITEM('')
);
#386=(
BOUNDED_CURVE()
B_SPLINE_CURVE(2,(#105421,#105422,#105423),.UNSPECIFIED.,.F.,.F.)
B_SPLINE_CURVE_WITH_KNOTS((3,3),(0.02789425411267,0.041581669522935),
 .UNSPECIFIED.)
CURVE()
GEOMETRIC_REPRESENTATION_ITEM()
RATIONAL_B_SPLINE_CURVE((1.00897713804979,1.00669106236252,1.))
REPRESENTATION_ITEM('')
);
#387=(
BOUNDED_CURVE()
B_SPLINE_CURVE(2,(#105425,#105426,#105427),.UNSPECIFIED.,.F.,.F.)
B_SPLINE_CURVE_WITH_KNOTS((3,3),(0.,0.0136874154102697),.UNSPECIFIED.)
CURVE()
GEOMETRIC_REPRESENTATION_ITEM()
RATIONAL_B_SPLINE_CURVE((1.,1.00669106236202,1.0089771380491))
REPRESENTATION_ITEM('')
);
#388=(
BOUNDED_CURVE()
B_SPLINE_CURVE(2,(#105431,#105432,#105433),.UNSPECIFIED.,.F.,.F.)
B_SPLINE_CURVE_WITH_KNOTS((3,3),(0.0278942541126704,0.0415816695229368),
 .UNSPECIFIED.)
CURVE()
GEOMETRIC_REPRESENTATION_ITEM()
RATIONAL_B_SPLINE_CURVE((1.00897713804836,1.00669106236146,1.))
REPRESENTATION_ITEM('')
);
#389=(
BOUNDED_CURVE()
B_SPLINE_CURVE(2,(#105435,#105436,#105437),.UNSPECIFIED.,.F.,.F.)
B_SPLINE_CURVE_WITH_KNOTS((3,3),(0.,0.0136874154102591),.UNSPECIFIED.)
CURVE()
GEOMETRIC_REPRESENTATION_ITEM()
RATIONAL_B_SPLINE_CURVE((1.,1.00669106236259,1.00897713804988))
REPRESENTATION_ITEM('')
);
#390=(
BOUNDED_CURVE()
B_SPLINE_CURVE(2,(#105441,#105442,#105443),.UNSPECIFIED.,.F.,.F.)
B_SPLINE_CURVE_WITH_KNOTS((3,3),(0.0278942541126758,0.0415816695229351),
 .UNSPECIFIED.)
CURVE()
GEOMETRIC_REPRESENTATION_ITEM()
RATIONAL_B_SPLINE_CURVE((1.00897713804987,1.00669106236259,1.))
REPRESENTATION_ITEM('')
);
#391=(
BOUNDED_CURVE()
B_SPLINE_CURVE(2,(#105445,#105446,#105447),.UNSPECIFIED.,.F.,.F.)
B_SPLINE_CURVE_WITH_KNOTS((3,3),(0.,0.0136874154102569),.UNSPECIFIED.)
CURVE()
GEOMETRIC_REPRESENTATION_ITEM()
RATIONAL_B_SPLINE_CURVE((1.,1.00669106236306,1.0089771380505))
REPRESENTATION_ITEM('')
);
#392=(
BOUNDED_CURVE()
B_SPLINE_CURVE(2,(#105451,#105452,#105453),.UNSPECIFIED.,.F.,.F.)
B_SPLINE_CURVE_WITH_KNOTS((3,3),(0.0278942541126783,0.0415816695229351),
 .UNSPECIFIED.)
CURVE()
GEOMETRIC_REPRESENTATION_ITEM()
RATIONAL_B_SPLINE_CURVE((1.0089771380505,1.00669106236306,1.))
REPRESENTATION_ITEM('')
);
#393=(
BOUNDED_CURVE()
B_SPLINE_CURVE(2,(#105455,#105456,#105457),.UNSPECIFIED.,.F.,.F.)
B_SPLINE_CURVE_WITH_KNOTS((3,3),(0.,0.0136874154102613),.UNSPECIFIED.)
CURVE()
GEOMETRIC_REPRESENTATION_ITEM()
RATIONAL_B_SPLINE_CURVE((1.,1.00669106236177,1.00897713804878))
REPRESENTATION_ITEM('')
);
#394=(
BOUNDED_CURVE()
B_SPLINE_CURVE(2,(#105460,#105461,#105462),.UNSPECIFIED.,.F.,.F.)
B_SPLINE_CURVE_WITH_KNOTS((3,3),(0.027894254112673,0.0415816695229326),
 .UNSPECIFIED.)
CURVE()
GEOMETRIC_REPRESENTATION_ITEM()
RATIONAL_B_SPLINE_CURVE((1.00897713804929,1.00669106236215,1.))
REPRESENTATION_ITEM('')
);
#395=(
BOUNDED_CURVE()
B_SPLINE_CURVE(2,(#106350,#106351,#106352),.UNSPECIFIED.,.F.,.F.)
B_SPLINE_CURVE_WITH_KNOTS((3,3),(0.,0.0160544451505013),.UNSPECIFIED.)
CURVE()
GEOMETRIC_REPRESENTATION_ITEM()
RATIONAL_B_SPLINE_CURVE((1.,1.02110226650162,1.02586827095084))
REPRESENTATION_ITEM('')
);
#396=(
BOUNDED_CURVE()
B_SPLINE_CURVE(2,(#106356,#106357,#106358),.UNSPECIFIED.,.F.,.F.)
B_SPLINE_CURVE_WITH_KNOTS((3,3),(0.0254220173370198,0.0414764624875277),
 .UNSPECIFIED.)
CURVE()
GEOMETRIC_REPRESENTATION_ITEM()
RATIONAL_B_SPLINE_CURVE((1.02586827094927,1.02110226650035,1.))
REPRESENTATION_ITEM('')
);
#397=(
BOUNDED_CURVE()
B_SPLINE_CURVE(2,(#106360,#106361,#106362),.UNSPECIFIED.,.F.,.F.)
B_SPLINE_CURVE_WITH_KNOTS((3,3),(0.,0.0160544451505076),.UNSPECIFIED.)
CURVE()
GEOMETRIC_REPRESENTATION_ITEM()
RATIONAL_B_SPLINE_CURVE((1.,1.02110226650074,1.02586827094974))
REPRESENTATION_ITEM('')
);
#398=(
BOUNDED_CURVE()
B_SPLINE_CURVE(2,(#106366,#106367,#106368),.UNSPECIFIED.,.F.,.F.)
B_SPLINE_CURVE_WITH_KNOTS((3,3),(0.0254220173370225,0.0414764624875298),
 .UNSPECIFIED.)
CURVE()
GEOMETRIC_REPRESENTATION_ITEM()
RATIONAL_B_SPLINE_CURVE((1.02586827094974,1.02110226650074,1.))
REPRESENTATION_ITEM('')
);
#399=(
BOUNDED_CURVE()
B_SPLINE_CURVE(2,(#106370,#106371,#106372),.UNSPECIFIED.,.F.,.F.)
B_SPLINE_CURVE_WITH_KNOTS((3,3),(0.,0.0160544451505037),.UNSPECIFIED.)
CURVE()
GEOMETRIC_REPRESENTATION_ITEM()
RATIONAL_B_SPLINE_CURVE((1.,1.02110226650177,1.02586827095102))
REPRESENTATION_ITEM('')
);
#400=(
BOUNDED_CURVE()
B_SPLINE_CURVE(2,(#106376,#106377,#106378),.UNSPECIFIED.,.F.,.F.)
B_SPLINE_CURVE_WITH_KNOTS((3,3),(0.0254220173370244,0.0414764624875264),
 .UNSPECIFIED.)
CURVE()
GEOMETRIC_REPRESENTATION_ITEM()
RATIONAL_B_SPLINE_CURVE((1.02586827094965,1.02110226650066,1.))
REPRESENTATION_ITEM('')
);
#401=(
BOUNDED_CURVE()
B_SPLINE_CURVE(2,(#106380,#106381,#106382),.UNSPECIFIED.,.F.,.F.)
B_SPLINE_CURVE_WITH_KNOTS((3,3),(0.,0.0160544451505027),.UNSPECIFIED.)
CURVE()
GEOMETRIC_REPRESENTATION_ITEM()
RATIONAL_B_SPLINE_CURVE((1.,1.02110226650163,1.02586827095084))
REPRESENTATION_ITEM('')
);
#402=(
BOUNDED_CURVE()
B_SPLINE_CURVE(2,(#106386,#106387,#106388),.UNSPECIFIED.,.F.,.F.)
B_SPLINE_CURVE_WITH_KNOTS((3,3),(0.0254220173370205,0.0414764624875277),
 .UNSPECIFIED.)
CURVE()
GEOMETRIC_REPRESENTATION_ITEM()
RATIONAL_B_SPLINE_CURVE((1.02586827094927,1.02110226650035,1.))
REPRESENTATION_ITEM('')
);
#403=(
BOUNDED_CURVE()
B_SPLINE_CURVE(2,(#106390,#106391,#106392),.UNSPECIFIED.,.F.,.F.)
B_SPLINE_CURVE_WITH_KNOTS((3,3),(0.,0.0160544451505042),.UNSPECIFIED.)
CURVE()
GEOMETRIC_REPRESENTATION_ITEM()
RATIONAL_B_SPLINE_CURVE((1.,1.02110226650138,1.02586827095053))
REPRESENTATION_ITEM('')
);
#404=(
BOUNDED_CURVE()
B_SPLINE_CURVE(2,(#106396,#106397,#106398),.UNSPECIFIED.,.F.,.F.)
B_SPLINE_CURVE_WITH_KNOTS((3,3),(0.0254220173370228,0.0414764624875268),
 .UNSPECIFIED.)
CURVE()
GEOMETRIC_REPRESENTATION_ITEM()
RATIONAL_B_SPLINE_CURVE((1.02586827095053,1.02110226650138,1.))
REPRESENTATION_ITEM('')
);
#405=(
BOUNDED_CURVE()
B_SPLINE_CURVE(2,(#106400,#106401,#106402),.UNSPECIFIED.,.F.,.F.)
B_SPLINE_CURVE_WITH_KNOTS((3,3),(0.,0.0160544451505048),.UNSPECIFIED.)
CURVE()
GEOMETRIC_REPRESENTATION_ITEM()
RATIONAL_B_SPLINE_CURVE((1.,1.02110226650167,1.02586827095089))
REPRESENTATION_ITEM('')
);
#406=(
BOUNDED_CURVE()
B_SPLINE_CURVE(2,(#106405,#106406,#106407),.UNSPECIFIED.,.F.,.F.)
B_SPLINE_CURVE_WITH_KNOTS((3,3),(0.0254220173370243,0.0414764624875262),
 .UNSPECIFIED.)
CURVE()
GEOMETRIC_REPRESENTATION_ITEM()
RATIONAL_B_SPLINE_CURVE((1.02586827094985,1.02110226650082,1.))
REPRESENTATION_ITEM('')
);
#407=(
BOUNDED_CURVE()
B_SPLINE_CURVE(2,(#108240,#108241,#108242),.UNSPECIFIED.,.F.,.F.)
B_SPLINE_CURVE_WITH_KNOTS((3,3),(0.,0.0136874154102654),.UNSPECIFIED.)
CURVE()
GEOMETRIC_REPRESENTATION_ITEM()
RATIONAL_B_SPLINE_CURVE((1.,1.00669106236307,1.00897713805051))
REPRESENTATION_ITEM('')
);
#408=(
BOUNDED_CURVE()
B_SPLINE_CURVE(2,(#108246,#108247,#108248),.UNSPECIFIED.,.F.,.F.)
B_SPLINE_CURVE_WITH_KNOTS((3,3),(0.0278942541126751,0.0415816695229443),
 .UNSPECIFIED.)
CURVE()
GEOMETRIC_REPRESENTATION_ITEM()
RATIONAL_B_SPLINE_CURVE((1.00897713805004,1.00669106236272,1.))
REPRESENTATION_ITEM('')
);
#409=(
BOUNDED_CURVE()
B_SPLINE_CURVE(2,(#108250,#108251,#108252),.UNSPECIFIED.,.F.,.F.)
B_SPLINE_CURVE_WITH_KNOTS((3,3),(0.,0.0136874154102686),.UNSPECIFIED.)
CURVE()
GEOMETRIC_REPRESENTATION_ITEM()
RATIONAL_B_SPLINE_CURVE((1.,1.00669106236263,1.00897713804992))
REPRESENTATION_ITEM('')
);
#410=(
BOUNDED_CURVE()
B_SPLINE_CURVE(2,(#108256,#108257,#108258),.UNSPECIFIED.,.F.,.F.)
B_SPLINE_CURVE_WITH_KNOTS((3,3),(0.0278942541126737,0.04158166952294),
 .UNSPECIFIED.)
CURVE()
GEOMETRIC_REPRESENTATION_ITEM()
RATIONAL_B_SPLINE_CURVE((1.00897713804992,1.00669106236263,1.))
REPRESENTATION_ITEM('')
);
#411=(
BOUNDED_CURVE()
B_SPLINE_CURVE(2,(#108260,#108261,#108262),.UNSPECIFIED.,.F.,.F.)
B_SPLINE_CURVE_WITH_KNOTS((3,3),(0.,0.0136874154102691),.UNSPECIFIED.)
CURVE()
GEOMETRIC_REPRESENTATION_ITEM()
RATIONAL_B_SPLINE_CURVE((1.,1.00669106236264,1.00897713804994))
REPRESENTATION_ITEM('')
);
#412=(
BOUNDED_CURVE()
B_SPLINE_CURVE(2,(#108266,#108267,#108268),.UNSPECIFIED.,.F.,.F.)
B_SPLINE_CURVE_WITH_KNOTS((3,3),(0.0278942541126743,0.0415816695229415),
 .UNSPECIFIED.)
CURVE()
GEOMETRIC_REPRESENTATION_ITEM()
RATIONAL_B_SPLINE_CURVE((1.00897713805037,1.00669106236296,1.))
REPRESENTATION_ITEM('')
);
#413=(
BOUNDED_CURVE()
B_SPLINE_CURVE(2,(#108270,#108271,#108272),.UNSPECIFIED.,.F.,.F.)
B_SPLINE_CURVE_WITH_KNOTS((3,3),(0.,0.0136874154102738),.UNSPECIFIED.)
CURVE()
GEOMETRIC_REPRESENTATION_ITEM()
RATIONAL_B_SPLINE_CURVE((1.,1.00669106236144,1.00897713804833))
REPRESENTATION_ITEM('')
);
#414=(
BOUNDED_CURVE()
B_SPLINE_CURVE(2,(#108276,#108277,#108278),.UNSPECIFIED.,.F.,.F.)
B_SPLINE_CURVE_WITH_KNOTS((3,3),(0.0278942541126704,0.0415816695229415),
 .UNSPECIFIED.)
CURVE()
GEOMETRIC_REPRESENTATION_ITEM()
RATIONAL_B_SPLINE_CURVE((1.00897713804912,1.00669106236203,1.))
REPRESENTATION_ITEM('')
);
#415=(
BOUNDED_CURVE()
B_SPLINE_CURVE(2,(#108280,#108281,#108282),.UNSPECIFIED.,.F.,.F.)
B_SPLINE_CURVE_WITH_KNOTS((3,3),(0.,0.013687415410267),.UNSPECIFIED.)
CURVE()
GEOMETRIC_REPRESENTATION_ITEM()
RATIONAL_B_SPLINE_CURVE((1.,1.0066910623626,1.00897713804988))
REPRESENTATION_ITEM('')
);
#416=(
BOUNDED_CURVE()
B_SPLINE_CURVE(2,(#108286,#108287,#108288),.UNSPECIFIED.,.F.,.F.)
B_SPLINE_CURVE_WITH_KNOTS((3,3),(0.0278942541126708,0.04158166952294),
 .UNSPECIFIED.)
CURVE()
GEOMETRIC_REPRESENTATION_ITEM()
RATIONAL_B_SPLINE_CURVE((1.00897713804988,1.0066910623626,1.))
REPRESENTATION_ITEM('')
);
#417=(
BOUNDED_CURVE()
B_SPLINE_CURVE(2,(#108290,#108291,#108292),.UNSPECIFIED.,.F.,.F.)
B_SPLINE_CURVE_WITH_KNOTS((3,3),(0.,0.0136874154102732),.UNSPECIFIED.)
CURVE()
GEOMETRIC_REPRESENTATION_ITEM()
RATIONAL_B_SPLINE_CURVE((1.,1.00669106236247,1.00897713804971))
REPRESENTATION_ITEM('')
);
#418=(
BOUNDED_CURVE()
B_SPLINE_CURVE(2,(#108295,#108296,#108297),.UNSPECIFIED.,.F.,.F.)
B_SPLINE_CURVE_WITH_KNOTS((3,3),(0.027894254112677,0.0415816695229426),
 .UNSPECIFIED.)
CURVE()
GEOMETRIC_REPRESENTATION_ITEM()
RATIONAL_B_SPLINE_CURVE((1.00897713805068,1.00669106236319,1.))
REPRESENTATION_ITEM('')
);
#419=(
BOUNDED_CURVE()
B_SPLINE_CURVE(2,(#109503,#109504,#109505),.UNSPECIFIED.,.F.,.F.)
B_SPLINE_CURVE_WITH_KNOTS((3,3),(0.,0.0160544451505045),.UNSPECIFIED.)
CURVE()
GEOMETRIC_REPRESENTATION_ITEM()
RATIONAL_B_SPLINE_CURVE((1.,1.02110226650212,1.02586827095145))
REPRESENTATION_ITEM('')
);
#420=(
BOUNDED_CURVE()
B_SPLINE_CURVE(2,(#109509,#109510,#109511),.UNSPECIFIED.,.F.,.F.)
B_SPLINE_CURVE_WITH_KNOTS((3,3),(0.0254220173370218,0.0414764624875315),
 .UNSPECIFIED.)
CURVE()
GEOMETRIC_REPRESENTATION_ITEM()
RATIONAL_B_SPLINE_CURVE((1.02586827095069,1.02110226650151,1.))
REPRESENTATION_ITEM('')
);
#421=(
BOUNDED_CURVE()
B_SPLINE_CURVE(2,(#109513,#109514,#109515),.UNSPECIFIED.,.F.,.F.)
B_SPLINE_CURVE_WITH_KNOTS((3,3),(0.,0.0160544451505064),.UNSPECIFIED.)
CURVE()
GEOMETRIC_REPRESENTATION_ITEM()
RATIONAL_B_SPLINE_CURVE((1.,1.02110226650114,1.02586827095025))
REPRESENTATION_ITEM('')
);
#422=(
BOUNDED_CURVE()
B_SPLINE_CURVE(2,(#109519,#109520,#109521),.UNSPECIFIED.,.F.,.F.)
B_SPLINE_CURVE_WITH_KNOTS((3,3),(0.025422017337023,0.0414764624875296),
 .UNSPECIFIED.)
CURVE()
GEOMETRIC_REPRESENTATION_ITEM()
RATIONAL_B_SPLINE_CURVE((1.02586827095025,1.02110226650115,1.))
REPRESENTATION_ITEM('')
);
#423=(
BOUNDED_CURVE()
B_SPLINE_CURVE(2,(#109523,#109524,#109525),.UNSPECIFIED.,.F.,.F.)
B_SPLINE_CURVE_WITH_KNOTS((3,3),(0.,0.0160544451505046),.UNSPECIFIED.)
CURVE()
GEOMETRIC_REPRESENTATION_ITEM()
RATIONAL_B_SPLINE_CURVE((1.,1.0211022665016,1.02586827095081))
REPRESENTATION_ITEM('')
);
#424=(
BOUNDED_CURVE()
B_SPLINE_CURVE(2,(#109529,#109530,#109531),.UNSPECIFIED.,.F.,.F.)
B_SPLINE_CURVE_WITH_KNOTS((3,3),(0.0254220173370246,0.0414764624875251),
 .UNSPECIFIED.)
CURVE()
GEOMETRIC_REPRESENTATION_ITEM()
RATIONAL_B_SPLINE_CURVE((1.02586827095081,1.0211022665016,1.))
REPRESENTATION_ITEM('')
);
#425=(
BOUNDED_CURVE()
B_SPLINE_CURVE(2,(#109533,#109534,#109535),.UNSPECIFIED.,.F.,.F.)
B_SPLINE_CURVE_WITH_KNOTS((3,3),(0.,0.0160544451505003),.UNSPECIFIED.)
CURVE()
GEOMETRIC_REPRESENTATION_ITEM()
RATIONAL_B_SPLINE_CURVE((1.,1.02110226650136,1.02586827095051))
REPRESENTATION_ITEM('')
);
#426=(
BOUNDED_CURVE()
B_SPLINE_CURVE(2,(#109539,#109540,#109541),.UNSPECIFIED.,.F.,.F.)
B_SPLINE_CURVE_WITH_KNOTS((3,3),(0.0254220173370209,0.0414764624875271),
 .UNSPECIFIED.)
CURVE()
GEOMETRIC_REPRESENTATION_ITEM()
RATIONAL_B_SPLINE_CURVE((1.02586827094991,1.02110226650087,1.))
REPRESENTATION_ITEM('')
);
#427=(
BOUNDED_CURVE()
B_SPLINE_CURVE(2,(#109543,#109544,#109545),.UNSPECIFIED.,.F.,.F.)
B_SPLINE_CURVE_WITH_KNOTS((3,3),(0.,0.0160544451505053),.UNSPECIFIED.)
CURVE()
GEOMETRIC_REPRESENTATION_ITEM()
RATIONAL_B_SPLINE_CURVE((1.,1.02110226650082,1.02586827094985))
REPRESENTATION_ITEM('')
);
#428=(
BOUNDED_CURVE()
B_SPLINE_CURVE(2,(#109549,#109550,#109551),.UNSPECIFIED.,.F.,.F.)
B_SPLINE_CURVE_WITH_KNOTS((3,3),(0.0254220173370217,0.0414764624875263),
 .UNSPECIFIED.)
CURVE()
GEOMETRIC_REPRESENTATION_ITEM()
RATIONAL_B_SPLINE_CURVE((1.02586827094985,1.02110226650082,1.))
REPRESENTATION_ITEM('')
);
#429=(
BOUNDED_CURVE()
B_SPLINE_CURVE(2,(#109553,#109554,#109555),.UNSPECIFIED.,.F.,.F.)
B_SPLINE_CURVE_WITH_KNOTS((3,3),(0.,0.0160544451505048),.UNSPECIFIED.)
CURVE()
GEOMETRIC_REPRESENTATION_ITEM()
RATIONAL_B_SPLINE_CURVE((1.,1.02110226650102,1.02586827095009))
REPRESENTATION_ITEM('')
);
#430=(
BOUNDED_CURVE()
B_SPLINE_CURVE(2,(#109558,#109559,#109560),.UNSPECIFIED.,.F.,.F.)
B_SPLINE_CURVE_WITH_KNOTS((3,3),(0.0254220173370231,0.0414764624875254),
 .UNSPECIFIED.)
CURVE()
GEOMETRIC_REPRESENTATION_ITEM()
RATIONAL_B_SPLINE_CURVE((1.0258682709511,1.02110226650184,1.))
REPRESENTATION_ITEM('')
);
#431=(
BOUNDED_CURVE()
B_SPLINE_CURVE(2,(#112949,#112950,#112951),.UNSPECIFIED.,.F.,.F.)
B_SPLINE_CURVE_WITH_KNOTS((3,3),(0.0227595441420062,0.0437553375522101),
 .UNSPECIFIED.)
CURVE()
GEOMETRIC_REPRESENTATION_ITEM()
RATIONAL_B_SPLINE_CURVE((1.00144169675558,1.00138583461502,1.))
REPRESENTATION_ITEM('')
);
#432=(
BOUNDED_CURVE()
B_SPLINE_CURVE(2,(#112963,#112964,#112965),.UNSPECIFIED.,.F.,.F.)
B_SPLINE_CURVE_WITH_KNOTS((3,3),(0.,0.0209957934101858),.UNSPECIFIED.)
CURVE()
GEOMETRIC_REPRESENTATION_ITEM()
RATIONAL_B_SPLINE_CURVE((1.,1.00138583461543,1.001441696756))
REPRESENTATION_ITEM('')
);
#433=(
BOUNDED_CURVE()
B_SPLINE_CURVE(2,(#113258,#113259,#113260),.UNSPECIFIED.,.F.,.F.)
B_SPLINE_CURVE_WITH_KNOTS((3,3),(0.0227595441420239,0.0437553375522102),
 .UNSPECIFIED.)
CURVE()
GEOMETRIC_REPRESENTATION_ITEM()
RATIONAL_B_SPLINE_CURVE((1.00144169675773,1.00138583461709,1.))
REPRESENTATION_ITEM('')
);
#434=(
BOUNDED_CURVE()
B_SPLINE_CURVE(2,(#113267,#113268,#113269),.UNSPECIFIED.,.F.,.F.)
B_SPLINE_CURVE_WITH_KNOTS((3,3),(0.,0.0209957934101477),.UNSPECIFIED.)
CURVE()
GEOMETRIC_REPRESENTATION_ITEM()
RATIONAL_B_SPLINE_CURVE((1.,1.00138583461455,1.00144169675509))
REPRESENTATION_ITEM('')
);
#435=(
BOUNDED_CURVE()
B_SPLINE_CURVE(2,(#113272,#113273,#113274),.UNSPECIFIED.,.F.,.F.)
B_SPLINE_CURVE_WITH_KNOTS((3,3),(0.0227595441420216,0.04375533755221),
 .UNSPECIFIED.)
CURVE()
GEOMETRIC_REPRESENTATION_ITEM()
RATIONAL_B_SPLINE_CURVE((1.00144169675475,1.00138583461423,1.))
REPRESENTATION_ITEM('')
);
#436=(
BOUNDED_CURVE()
B_SPLINE_CURVE(2,(#113281,#113282,#113283),.UNSPECIFIED.,.F.,.F.)
B_SPLINE_CURVE_WITH_KNOTS((3,3),(0.,0.020995793410179),.UNSPECIFIED.)
CURVE()
GEOMETRIC_REPRESENTATION_ITEM()
RATIONAL_B_SPLINE_CURVE((1.,1.00138583461437,1.0014416967549))
REPRESENTATION_ITEM('')
);
#437=(
BOUNDED_CURVE()
B_SPLINE_CURVE(2,(#113286,#113287,#113288),.UNSPECIFIED.,.F.,.F.)
B_SPLINE_CURVE_WITH_KNOTS((3,3),(0.0227595441420233,0.0437553375522096),
 .UNSPECIFIED.)
CURVE()
GEOMETRIC_REPRESENTATION_ITEM()
RATIONAL_B_SPLINE_CURVE((1.0014416967577,1.00138583461706,1.))
REPRESENTATION_ITEM('')
);
#438=(
BOUNDED_CURVE()
B_SPLINE_CURVE(2,(#113295,#113296,#113297),.UNSPECIFIED.,.F.,.F.)
B_SPLINE_CURVE_WITH_KNOTS((3,3),(0.,0.0209957934101891),.UNSPECIFIED.)
CURVE()
GEOMETRIC_REPRESENTATION_ITEM()
RATIONAL_B_SPLINE_CURVE((1.,1.00138583461396,1.00144169675448))
REPRESENTATION_ITEM('')
);
#439=(
BOUNDED_CURVE()
B_SPLINE_CURVE(2,(#113300,#113301,#113302),.UNSPECIFIED.,.F.,.F.)
B_SPLINE_CURVE_WITH_KNOTS((3,3),(0.0227595441420034,0.04375533755221),
 .UNSPECIFIED.)
CURVE()
GEOMETRIC_REPRESENTATION_ITEM()
RATIONAL_B_SPLINE_CURVE((1.00144169675772,1.00138583461708,1.))
REPRESENTATION_ITEM('')
);
#440=(
BOUNDED_CURVE()
B_SPLINE_CURVE(2,(#113309,#113310,#113311),.UNSPECIFIED.,.F.,.F.)
B_SPLINE_CURVE_WITH_KNOTS((3,3),(0.,0.0209957934101803),.UNSPECIFIED.)
CURVE()
GEOMETRIC_REPRESENTATION_ITEM()
RATIONAL_B_SPLINE_CURVE((1.,1.00138583461545,1.00144169675603))
REPRESENTATION_ITEM('')
);
#441=(
BOUNDED_CURVE()
B_SPLINE_CURVE(2,(#113314,#113315,#113316),.UNSPECIFIED.,.F.,.F.)
B_SPLINE_CURVE_WITH_KNOTS((3,3),(0.0227595441420504,0.0437553375522096),
 .UNSPECIFIED.)
CURVE()
GEOMETRIC_REPRESENTATION_ITEM()
RATIONAL_B_SPLINE_CURVE((1.00144169675773,1.00138583461708,1.))
REPRESENTATION_ITEM('')
);
#442=(
BOUNDED_CURVE()
B_SPLINE_CURVE(2,(#113323,#113324,#113325),.UNSPECIFIED.,.F.,.F.)
B_SPLINE_CURVE_WITH_KNOTS((3,3),(0.,0.0209957934102014),.UNSPECIFIED.)
CURVE()
GEOMETRIC_REPRESENTATION_ITEM()
RATIONAL_B_SPLINE_CURVE((1.,1.00138583461972,1.00144169676047))
REPRESENTATION_ITEM('')
);
#443=(
BOUNDED_CURVE()
B_SPLINE_CURVE(2,(#113328,#113329,#113330),.UNSPECIFIED.,.F.,.F.)
B_SPLINE_CURVE_WITH_KNOTS((3,3),(0.0227595441420253,0.04375533755221),
 .UNSPECIFIED.)
CURVE()
GEOMETRIC_REPRESENTATION_ITEM()
RATIONAL_B_SPLINE_CURVE((1.00144169676086,1.0013858346201,1.))
REPRESENTATION_ITEM('')
);
#444=(
BOUNDED_CURVE()
B_SPLINE_CURVE(2,(#113337,#113338,#113339),.UNSPECIFIED.,.F.,.F.)
B_SPLINE_CURVE_WITH_KNOTS((3,3),(0.,0.0209957934102032),.UNSPECIFIED.)
CURVE()
GEOMETRIC_REPRESENTATION_ITEM()
RATIONAL_B_SPLINE_CURVE((1.,1.00138583461651,1.00144169675713))
REPRESENTATION_ITEM('')
);
#445=(
BOUNDED_CURVE()
B_SPLINE_CURVE(2,(#113342,#113343,#113344),.UNSPECIFIED.,.F.,.F.)
B_SPLINE_CURVE_WITH_KNOTS((3,3),(0.0227595441420214,0.0437553375522101),
 .UNSPECIFIED.)
CURVE()
GEOMETRIC_REPRESENTATION_ITEM()
RATIONAL_B_SPLINE_CURVE((1.00144169675793,1.00138583461728,1.))
REPRESENTATION_ITEM('')
);
#446=(
BOUNDED_CURVE()
B_SPLINE_CURVE(2,(#113351,#113352,#113353),.UNSPECIFIED.,.F.,.F.)
B_SPLINE_CURVE_WITH_KNOTS((3,3),(0.,0.0209957934101777),.UNSPECIFIED.)
CURVE()
GEOMETRIC_REPRESENTATION_ITEM()
RATIONAL_B_SPLINE_CURVE((1.,1.00138583461269,1.00144169675315))
REPRESENTATION_ITEM('')
);
#447=(
BOUNDED_CURVE()
B_SPLINE_CURVE(2,(#113356,#113357,#113358),.UNSPECIFIED.,.F.,.F.)
B_SPLINE_CURVE_WITH_KNOTS((3,3),(0.0227595441419899,0.0437553375522099),
 .UNSPECIFIED.)
CURVE()
GEOMETRIC_REPRESENTATION_ITEM()
RATIONAL_B_SPLINE_CURVE((1.00144169675096,1.00138583461059,1.))
REPRESENTATION_ITEM('')
);
#448=(
BOUNDED_CURVE()
B_SPLINE_CURVE(2,(#113365,#113366,#113367),.UNSPECIFIED.,.F.,.F.)
B_SPLINE_CURVE_WITH_KNOTS((3,3),(0.,0.0209957934101782),.UNSPECIFIED.)
CURVE()
GEOMETRIC_REPRESENTATION_ITEM()
RATIONAL_B_SPLINE_CURVE((1.,1.00138583461646,1.00144169675708))
REPRESENTATION_ITEM('')
);
#449=(
BOUNDED_CURVE()
B_SPLINE_CURVE(2,(#113370,#113371,#113372),.UNSPECIFIED.,.F.,.F.)
B_SPLINE_CURVE_WITH_KNOTS((3,3),(0.0227595441420376,0.0437553375522098),
 .UNSPECIFIED.)
CURVE()
GEOMETRIC_REPRESENTATION_ITEM()
RATIONAL_B_SPLINE_CURVE((1.0014416967547,1.00138583461417,1.))
REPRESENTATION_ITEM('')
);
#450=(
BOUNDED_CURVE()
B_SPLINE_CURVE(2,(#113379,#113380,#113381),.UNSPECIFIED.,.F.,.F.)
B_SPLINE_CURVE_WITH_KNOTS((3,3),(0.,0.020995793410168),.UNSPECIFIED.)
CURVE()
GEOMETRIC_REPRESENTATION_ITEM()
RATIONAL_B_SPLINE_CURVE((1.,1.00138583461699,1.00144169675762))
REPRESENTATION_ITEM('')
);
#451=(
BOUNDED_CURVE()
B_SPLINE_CURVE(2,(#113384,#113385,#113386),.UNSPECIFIED.,.F.,.F.)
B_SPLINE_CURVE_WITH_KNOTS((3,3),(0.0227595441420211,0.0437553375522103),
 .UNSPECIFIED.)
CURVE()
GEOMETRIC_REPRESENTATION_ITEM()
RATIONAL_B_SPLINE_CURVE((1.00144169675723,1.00138583461661,1.))
REPRESENTATION_ITEM('')
);
#452=(
BOUNDED_CURVE()
B_SPLINE_CURVE(2,(#113393,#113394,#113395),.UNSPECIFIED.,.F.,.F.)
B_SPLINE_CURVE_WITH_KNOTS((3,3),(0.,0.0209957934101646),.UNSPECIFIED.)
CURVE()
GEOMETRIC_REPRESENTATION_ITEM()
RATIONAL_B_SPLINE_CURVE((1.,1.00138583461121,1.00144169675162))
REPRESENTATION_ITEM('')
);
#453=(
BOUNDED_CURVE()
B_SPLINE_CURVE(2,(#113398,#113399,#113400),.UNSPECIFIED.,.F.,.F.)
B_SPLINE_CURVE_WITH_KNOTS((3,3),(0.0227595441420204,0.0437553375522103),
 .UNSPECIFIED.)
CURVE()
GEOMETRIC_REPRESENTATION_ITEM()
RATIONAL_B_SPLINE_CURVE((1.0014416967587,1.00138583461803,1.))
REPRESENTATION_ITEM('')
);
#454=(
BOUNDED_CURVE()
B_SPLINE_CURVE(2,(#113407,#113408,#113409),.UNSPECIFIED.,.F.,.F.)
B_SPLINE_CURVE_WITH_KNOTS((3,3),(0.,0.0209957934102059),.UNSPECIFIED.)
CURVE()
GEOMETRIC_REPRESENTATION_ITEM()
RATIONAL_B_SPLINE_CURVE((1.,1.00138583461321,1.00144169675369))
REPRESENTATION_ITEM('')
);
#455=(
BOUNDED_CURVE()
B_SPLINE_CURVE(2,(#113412,#113413,#113414),.UNSPECIFIED.,.F.,.F.)
B_SPLINE_CURVE_WITH_KNOTS((3,3),(0.0227595441420123,0.0437553375522097),
 .UNSPECIFIED.)
CURVE()
GEOMETRIC_REPRESENTATION_ITEM()
RATIONAL_B_SPLINE_CURVE((1.00144169675907,1.00138583461838,1.))
REPRESENTATION_ITEM('')
);
#456=(
BOUNDED_CURVE()
B_SPLINE_CURVE(2,(#113421,#113422,#113423),.UNSPECIFIED.,.F.,.F.)
B_SPLINE_CURVE_WITH_KNOTS((3,3),(0.,0.020995793410209),.UNSPECIFIED.)
CURVE()
GEOMETRIC_REPRESENTATION_ITEM()
RATIONAL_B_SPLINE_CURVE((1.,1.00138583461559,1.00144169675616))
REPRESENTATION_ITEM('')
);
#457=(
BOUNDED_CURVE()
B_SPLINE_CURVE(2,(#113426,#113427,#113428),.UNSPECIFIED.,.F.,.F.)
B_SPLINE_CURVE_WITH_KNOTS((3,3),(0.0227595441420273,0.04375533755221),
 .UNSPECIFIED.)
CURVE()
GEOMETRIC_REPRESENTATION_ITEM()
RATIONAL_B_SPLINE_CURVE((1.00144169675712,1.0013858346165,1.))
REPRESENTATION_ITEM('')
);
#458=(
BOUNDED_CURVE()
B_SPLINE_CURVE(2,(#113435,#113436,#113437),.UNSPECIFIED.,.F.,.F.)
B_SPLINE_CURVE_WITH_KNOTS((3,3),(0.,0.0209957934101636),.UNSPECIFIED.)
CURVE()
GEOMETRIC_REPRESENTATION_ITEM()
RATIONAL_B_SPLINE_CURVE((1.,1.00138583461551,1.00144169675609))
REPRESENTATION_ITEM('')
);
#459=(
BOUNDED_CURVE()
B_SPLINE_CURVE(2,(#113440,#113441,#113442),.UNSPECIFIED.,.F.,.F.)
B_SPLINE_CURVE_WITH_KNOTS((3,3),(0.0227595441420356,0.0437553375522098),
 .UNSPECIFIED.)
CURVE()
GEOMETRIC_REPRESENTATION_ITEM()
RATIONAL_B_SPLINE_CURVE((1.00144169675546,1.00138583461491,1.))
REPRESENTATION_ITEM('')
);
#460=(
BOUNDED_CURVE()
B_SPLINE_CURVE(2,(#113449,#113450,#113451),.UNSPECIFIED.,.F.,.F.)
B_SPLINE_CURVE_WITH_KNOTS((3,3),(0.,0.0209957934102153),.UNSPECIFIED.)
CURVE()
GEOMETRIC_REPRESENTATION_ITEM()
RATIONAL_B_SPLINE_CURVE((1.,1.00138583461812,1.0014416967588))
REPRESENTATION_ITEM('')
);
#461=(
BOUNDED_CURVE()
B_SPLINE_CURVE(2,(#113454,#113455,#113456),.UNSPECIFIED.,.F.,.F.)
B_SPLINE_CURVE_WITH_KNOTS((3,3),(0.0227595441420236,0.0437553375522102),
 .UNSPECIFIED.)
CURVE()
GEOMETRIC_REPRESENTATION_ITEM()
RATIONAL_B_SPLINE_CURVE((1.00144169675374,1.00138583461325,1.))
REPRESENTATION_ITEM('')
);
#462=(
BOUNDED_CURVE()
B_SPLINE_CURVE(2,(#113463,#113464,#113465),.UNSPECIFIED.,.F.,.F.)
B_SPLINE_CURVE_WITH_KNOTS((3,3),(0.,0.0209957934101627),.UNSPECIFIED.)
CURVE()
GEOMETRIC_REPRESENTATION_ITEM()
RATIONAL_B_SPLINE_CURVE((1.,1.00138583461917,1.0014416967599))
REPRESENTATION_ITEM('')
);
#463=(
BOUNDED_CURVE()
B_SPLINE_CURVE(2,(#113468,#113469,#113470),.UNSPECIFIED.,.F.,.F.)
B_SPLINE_CURVE_WITH_KNOTS((3,3),(0.0227595441420239,0.0437553375522098),
 .UNSPECIFIED.)
CURVE()
GEOMETRIC_REPRESENTATION_ITEM()
RATIONAL_B_SPLINE_CURVE((1.00144169675673,1.00138583461613,1.))
REPRESENTATION_ITEM('')
);
#464=(
BOUNDED_CURVE()
B_SPLINE_CURVE(2,(#113477,#113478,#113479),.UNSPECIFIED.,.F.,.F.)
B_SPLINE_CURVE_WITH_KNOTS((3,3),(0.,0.0209957934102122),.UNSPECIFIED.)
CURVE()
GEOMETRIC_REPRESENTATION_ITEM()
RATIONAL_B_SPLINE_CURVE((1.,1.00138583461449,1.00144169675502))
REPRESENTATION_ITEM('')
);
#465=(
BOUNDED_CURVE()
B_SPLINE_CURVE(2,(#113482,#113483,#113484),.UNSPECIFIED.,.F.,.F.)
B_SPLINE_CURVE_WITH_KNOTS((3,3),(0.0227595441420244,0.0437553375522098),
 .UNSPECIFIED.)
CURVE()
GEOMETRIC_REPRESENTATION_ITEM()
RATIONAL_B_SPLINE_CURVE((1.00144169675843,1.00138583461776,1.))
REPRESENTATION_ITEM('')
);
#466=(
BOUNDED_CURVE()
B_SPLINE_CURVE(2,(#113491,#113492,#113493),.UNSPECIFIED.,.F.,.F.)
B_SPLINE_CURVE_WITH_KNOTS((3,3),(0.,0.0209957934102044),.UNSPECIFIED.)
CURVE()
GEOMETRIC_REPRESENTATION_ITEM()
RATIONAL_B_SPLINE_CURVE((1.,1.00138583461816,1.00144169675884))
REPRESENTATION_ITEM('')
);
#467=(
BOUNDED_CURVE()
B_SPLINE_CURVE(2,(#113496,#113497,#113498),.UNSPECIFIED.,.F.,.F.)
B_SPLINE_CURVE_WITH_KNOTS((3,3),(0.0227595441420142,0.0437553375522099),
 .UNSPECIFIED.)
CURVE()
GEOMETRIC_REPRESENTATION_ITEM()
RATIONAL_B_SPLINE_CURVE((1.00144169675525,1.00138583461471,1.))
REPRESENTATION_ITEM('')
);
#468=(
BOUNDED_CURVE()
B_SPLINE_CURVE(2,(#113505,#113506,#113507),.UNSPECIFIED.,.F.,.F.)
B_SPLINE_CURVE_WITH_KNOTS((3,3),(0.,0.0209957934101661),.UNSPECIFIED.)
CURVE()
GEOMETRIC_REPRESENTATION_ITEM()
RATIONAL_B_SPLINE_CURVE((1.,1.00138583461737,1.00144169675803))
REPRESENTATION_ITEM('')
);
#469=(
BOUNDED_CURVE()
B_SPLINE_CURVE(2,(#113510,#113511,#113512),.UNSPECIFIED.,.F.,.F.)
B_SPLINE_CURVE_WITH_KNOTS((3,3),(0.0227595441419954,0.0437553375522101),
 .UNSPECIFIED.)
CURVE()
GEOMETRIC_REPRESENTATION_ITEM()
RATIONAL_B_SPLINE_CURVE((1.00144169675597,1.0013858346154,1.))
REPRESENTATION_ITEM('')
);
#470=(
BOUNDED_CURVE()
B_SPLINE_CURVE(2,(#113519,#113520,#113521),.UNSPECIFIED.,.F.,.F.)
B_SPLINE_CURVE_WITH_KNOTS((3,3),(0.,0.0209957934101572),.UNSPECIFIED.)
CURVE()
GEOMETRIC_REPRESENTATION_ITEM()
RATIONAL_B_SPLINE_CURVE((1.,1.00138583461617,1.00144169675677))
REPRESENTATION_ITEM('')
);
#471=(
BOUNDED_CURVE()
B_SPLINE_CURVE(2,(#113524,#113525,#113526),.UNSPECIFIED.,.F.,.F.)
B_SPLINE_CURVE_WITH_KNOTS((3,3),(0.0227595441420733,0.0437553375522098),
 .UNSPECIFIED.)
CURVE()
GEOMETRIC_REPRESENTATION_ITEM()
RATIONAL_B_SPLINE_CURVE((1.00144169676135,1.00138583462057,1.))
REPRESENTATION_ITEM('')
);
#472=(
BOUNDED_CURVE()
B_SPLINE_CURVE(2,(#113533,#113534,#113535),.UNSPECIFIED.,.F.,.F.)
B_SPLINE_CURVE_WITH_KNOTS((3,3),(0.,0.0209957934101981),.UNSPECIFIED.)
CURVE()
GEOMETRIC_REPRESENTATION_ITEM()
RATIONAL_B_SPLINE_CURVE((1.,1.00138583461495,1.0014416967555))
REPRESENTATION_ITEM('')
);
#473=(
BOUNDED_CURVE()
B_SPLINE_CURVE(2,(#113538,#113539,#113540),.UNSPECIFIED.,.F.,.F.)
B_SPLINE_CURVE_WITH_KNOTS((3,3),(0.022759544142027,0.0437553375522101),
 .UNSPECIFIED.)
CURVE()
GEOMETRIC_REPRESENTATION_ITEM()
RATIONAL_B_SPLINE_CURVE((1.00144169675767,1.00138583461703,1.))
REPRESENTATION_ITEM('')
);
#474=(
BOUNDED_CURVE()
B_SPLINE_CURVE(2,(#113547,#113548,#113549),.UNSPECIFIED.,.F.,.F.)
B_SPLINE_CURVE_WITH_KNOTS((3,3),(0.,0.0209957934102148),.UNSPECIFIED.)
CURVE()
GEOMETRIC_REPRESENTATION_ITEM()
RATIONAL_B_SPLINE_CURVE((1.,1.00138583461343,1.00144169675392))
REPRESENTATION_ITEM('')
);
#475=(
BOUNDED_CURVE()
B_SPLINE_CURVE(2,(#113552,#113553,#113554),.UNSPECIFIED.,.F.,.F.)
B_SPLINE_CURVE_WITH_KNOTS((3,3),(0.0227595441420587,0.04375533755221),
 .UNSPECIFIED.)
CURVE()
GEOMETRIC_REPRESENTATION_ITEM()
RATIONAL_B_SPLINE_CURVE((1.00144169675587,1.0013858346153,1.))
REPRESENTATION_ITEM('')
);
#476=(
BOUNDED_CURVE()
B_SPLINE_CURVE(2,(#113561,#113562,#113563),.UNSPECIFIED.,.F.,.F.)
B_SPLINE_CURVE_WITH_KNOTS((3,3),(0.,0.0209957934101868),.UNSPECIFIED.)
CURVE()
GEOMETRIC_REPRESENTATION_ITEM()
RATIONAL_B_SPLINE_CURVE((1.,1.00138583461518,1.00144169675574))
REPRESENTATION_ITEM('')
);
#477=(
BOUNDED_CURVE()
B_SPLINE_CURVE(2,(#113566,#113567,#113568),.UNSPECIFIED.,.F.,.F.)
B_SPLINE_CURVE_WITH_KNOTS((3,3),(0.0227595441420354,0.0437553375522099),
 .UNSPECIFIED.)
CURVE()
GEOMETRIC_REPRESENTATION_ITEM()
RATIONAL_B_SPLINE_CURVE((1.0014416967583,1.00138583461764,1.))
REPRESENTATION_ITEM('')
);
#478=(
BOUNDED_CURVE()
B_SPLINE_CURVE(2,(#113575,#113576,#113577),.UNSPECIFIED.,.F.,.F.)
B_SPLINE_CURVE_WITH_KNOTS((3,3),(0.,0.0209957934101755),.UNSPECIFIED.)
CURVE()
GEOMETRIC_REPRESENTATION_ITEM()
RATIONAL_B_SPLINE_CURVE((1.,1.00138583461728,1.00144169675792))
REPRESENTATION_ITEM('')
);
#479=(
BOUNDED_CURVE()
B_SPLINE_CURVE(2,(#113580,#113581,#113582),.UNSPECIFIED.,.F.,.F.)
B_SPLINE_CURVE_WITH_KNOTS((3,3),(0.0227595441420414,0.0437553375522097),
 .UNSPECIFIED.)
CURVE()
GEOMETRIC_REPRESENTATION_ITEM()
RATIONAL_B_SPLINE_CURVE((1.00144169676129,1.00138583462051,1.))
REPRESENTATION_ITEM('')
);
#480=(
BOUNDED_CURVE()
B_SPLINE_CURVE(2,(#113589,#113590,#113591),.UNSPECIFIED.,.F.,.F.)
B_SPLINE_CURVE_WITH_KNOTS((3,3),(0.,0.0209957934101856),.UNSPECIFIED.)
CURVE()
GEOMETRIC_REPRESENTATION_ITEM()
RATIONAL_B_SPLINE_CURVE((1.,1.00138583461831,1.001441696759))
REPRESENTATION_ITEM('')
);
#481=(
BOUNDED_CURVE()
B_SPLINE_CURVE(2,(#113594,#113595,#113596),.UNSPECIFIED.,.F.,.F.)
B_SPLINE_CURVE_WITH_KNOTS((3,3),(0.0227595441420472,0.0437553375522097),
 .UNSPECIFIED.)
CURVE()
GEOMETRIC_REPRESENTATION_ITEM()
RATIONAL_B_SPLINE_CURVE((1.00144169675876,1.00138583461808,1.))
REPRESENTATION_ITEM('')
);
#482=(
BOUNDED_CURVE()
B_SPLINE_CURVE(2,(#113603,#113604,#113605),.UNSPECIFIED.,.F.,.F.)
B_SPLINE_CURVE_WITH_KNOTS((3,3),(0.,0.0209957934101722),.UNSPECIFIED.)
CURVE()
GEOMETRIC_REPRESENTATION_ITEM()
RATIONAL_B_SPLINE_CURVE((1.,1.00138583461417,1.0014416967547))
REPRESENTATION_ITEM('')
);
#483=(
BOUNDED_CURVE()
B_SPLINE_CURVE(2,(#113608,#113609,#113610),.UNSPECIFIED.,.F.,.F.)
B_SPLINE_CURVE_WITH_KNOTS((3,3),(0.0227595441420099,0.0437553375522099),
 .UNSPECIFIED.)
CURVE()
GEOMETRIC_REPRESENTATION_ITEM()
RATIONAL_B_SPLINE_CURVE((1.00144169675708,1.00138583461646,1.))
REPRESENTATION_ITEM('')
);
#484=(
BOUNDED_CURVE()
B_SPLINE_CURVE(2,(#113617,#113618,#113619),.UNSPECIFIED.,.F.,.F.)
B_SPLINE_CURVE_WITH_KNOTS((3,3),(0.,0.0209957934101837),.UNSPECIFIED.)
CURVE()
GEOMETRIC_REPRESENTATION_ITEM()
RATIONAL_B_SPLINE_CURVE((1.,1.00138583461363,1.00144169675414))
REPRESENTATION_ITEM('')
);
#485=(
BOUNDED_CURVE()
B_SPLINE_CURVE(2,(#113622,#113623,#113624),.UNSPECIFIED.,.F.,.F.)
B_SPLINE_CURVE_WITH_KNOTS((3,3),(0.0227595441420264,0.0437553375522102),
 .UNSPECIFIED.)
CURVE()
GEOMETRIC_REPRESENTATION_ITEM()
RATIONAL_B_SPLINE_CURVE((1.00144169675219,1.00138583461176,1.))
REPRESENTATION_ITEM('')
);
#486=(
BOUNDED_CURVE()
B_SPLINE_CURVE(2,(#113631,#113632,#113633),.UNSPECIFIED.,.F.,.F.)
B_SPLINE_CURVE_WITH_KNOTS((3,3),(0.,0.0209957934101768),.UNSPECIFIED.)
CURVE()
GEOMETRIC_REPRESENTATION_ITEM()
RATIONAL_B_SPLINE_CURVE((1.,1.00138583461562,1.0014416967562))
REPRESENTATION_ITEM('')
);
#487=(
BOUNDED_CURVE()
B_SPLINE_CURVE(2,(#113636,#113637,#113638),.UNSPECIFIED.,.F.,.F.)
B_SPLINE_CURVE_WITH_KNOTS((3,3),(0.0227595441419788,0.0437553375522102),
 .UNSPECIFIED.)
CURVE()
GEOMETRIC_REPRESENTATION_ITEM()
RATIONAL_B_SPLINE_CURVE((1.00144169675083,1.00138583461046,1.))
REPRESENTATION_ITEM('')
);
#488=(
BOUNDED_CURVE()
B_SPLINE_CURVE(2,(#113645,#113646,#113647),.UNSPECIFIED.,.F.,.F.)
B_SPLINE_CURVE_WITH_KNOTS((3,3),(0.,0.0209957934101946),.UNSPECIFIED.)
CURVE()
GEOMETRIC_REPRESENTATION_ITEM()
RATIONAL_B_SPLINE_CURVE((1.,1.00138583461436,1.00144169675489))
REPRESENTATION_ITEM('')
);
#489=(
BOUNDED_CURVE()
B_SPLINE_CURVE(2,(#113650,#113651,#113652),.UNSPECIFIED.,.F.,.F.)
B_SPLINE_CURVE_WITH_KNOTS((3,3),(0.0227595441420032,0.04375533755221),
 .UNSPECIFIED.)
CURVE()
GEOMETRIC_REPRESENTATION_ITEM()
RATIONAL_B_SPLINE_CURVE((1.00144169675912,1.00138583461843,1.))
REPRESENTATION_ITEM('')
);
#490=(
BOUNDED_CURVE()
B_SPLINE_CURVE(2,(#113659,#113660,#113661),.UNSPECIFIED.,.F.,.F.)
B_SPLINE_CURVE_WITH_KNOTS((3,3),(0.,0.0209957934101575),.UNSPECIFIED.)
CURVE()
GEOMETRIC_REPRESENTATION_ITEM()
RATIONAL_B_SPLINE_CURVE((1.,1.00138583461801,1.00144169675869))
REPRESENTATION_ITEM('')
);
#491=(
BOUNDED_CURVE()
B_SPLINE_CURVE(2,(#113664,#113665,#113666),.UNSPECIFIED.,.F.,.F.)
B_SPLINE_CURVE_WITH_KNOTS((3,3),(0.0227595441420447,0.04375533755221),
 .UNSPECIFIED.)
CURVE()
GEOMETRIC_REPRESENTATION_ITEM()
RATIONAL_B_SPLINE_CURVE((1.00144169676208,1.00138583462127,1.))
REPRESENTATION_ITEM('')
);
#492=(
BOUNDED_CURVE()
B_SPLINE_CURVE(2,(#113673,#113674,#113675),.UNSPECIFIED.,.F.,.F.)
B_SPLINE_CURVE_WITH_KNOTS((3,3),(0.,0.0209957934102153),.UNSPECIFIED.)
CURVE()
GEOMETRIC_REPRESENTATION_ITEM()
RATIONAL_B_SPLINE_CURVE((1.,1.00138583461588,1.00144169675647))
REPRESENTATION_ITEM('')
);
#493=(
BOUNDED_CURVE()
B_SPLINE_CURVE(2,(#113678,#113679,#113680),.UNSPECIFIED.,.F.,.F.)
B_SPLINE_CURVE_WITH_KNOTS((3,3),(0.0227595441420092,0.04375533755221),
 .UNSPECIFIED.)
CURVE()
GEOMETRIC_REPRESENTATION_ITEM()
RATIONAL_B_SPLINE_CURVE((1.00144169675677,1.00138583461617,1.))
REPRESENTATION_ITEM('')
);
#494=(
BOUNDED_CURVE()
B_SPLINE_CURVE(2,(#113687,#113688,#113689),.UNSPECIFIED.,.F.,.F.)
B_SPLINE_CURVE_WITH_KNOTS((3,3),(0.,0.0209957934101552),.UNSPECIFIED.)
CURVE()
GEOMETRIC_REPRESENTATION_ITEM()
RATIONAL_B_SPLINE_CURVE((1.,1.00138583461929,1.00144169676002))
REPRESENTATION_ITEM('')
);
#495=(
BOUNDED_CURVE()
B_SPLINE_CURVE(2,(#113692,#113693,#113694),.UNSPECIFIED.,.F.,.F.)
B_SPLINE_CURVE_WITH_KNOTS((3,3),(0.0227595441419908,0.0437553375522098),
 .UNSPECIFIED.)
CURVE()
GEOMETRIC_REPRESENTATION_ITEM()
RATIONAL_B_SPLINE_CURVE((1.00144169675614,1.00138583461556,1.))
REPRESENTATION_ITEM('')
);
#496=(
BOUNDED_CURVE()
B_SPLINE_CURVE(2,(#113701,#113702,#113703),.UNSPECIFIED.,.F.,.F.)
B_SPLINE_CURVE_WITH_KNOTS((3,3),(0.,0.0209957934101925),.UNSPECIFIED.)
CURVE()
GEOMETRIC_REPRESENTATION_ITEM()
RATIONAL_B_SPLINE_CURVE((1.,1.00138583461381,1.00144169675432))
REPRESENTATION_ITEM('')
);
#497=(
BOUNDED_CURVE()
B_SPLINE_CURVE(2,(#113706,#113707,#113708),.UNSPECIFIED.,.F.,.F.)
B_SPLINE_CURVE_WITH_KNOTS((3,3),(0.0227595441420215,0.0437553375522099),
 .UNSPECIFIED.)
CURVE()
GEOMETRIC_REPRESENTATION_ITEM()
RATIONAL_B_SPLINE_CURVE((1.00144169675677,1.00138583461617,1.))
REPRESENTATION_ITEM('')
);
#498=(
BOUNDED_CURVE()
B_SPLINE_CURVE(2,(#113715,#113716,#113717),.UNSPECIFIED.,.F.,.F.)
B_SPLINE_CURVE_WITH_KNOTS((3,3),(0.,0.0209957934101895),.UNSPECIFIED.)
CURVE()
GEOMETRIC_REPRESENTATION_ITEM()
RATIONAL_B_SPLINE_CURVE((1.,1.00138583461732,1.00144169675797))
REPRESENTATION_ITEM('')
);
#499=(
BOUNDED_CURVE()
B_SPLINE_CURVE(2,(#113720,#113721,#113722),.UNSPECIFIED.,.F.,.F.)
B_SPLINE_CURVE_WITH_KNOTS((3,3),(0.0227595441420421,0.0437553375522098),
 .UNSPECIFIED.)
CURVE()
GEOMETRIC_REPRESENTATION_ITEM()
RATIONAL_B_SPLINE_CURVE((1.00144169675667,1.00138583461607,1.))
REPRESENTATION_ITEM('')
);
#500=(
BOUNDED_CURVE()
B_SPLINE_CURVE(2,(#113729,#113730,#113731),.UNSPECIFIED.,.F.,.F.)
B_SPLINE_CURVE_WITH_KNOTS((3,3),(0.,0.020995793410204),.UNSPECIFIED.)
CURVE()
GEOMETRIC_REPRESENTATION_ITEM()
RATIONAL_B_SPLINE_CURVE((1.,1.00138583461502,1.00144169675558))
REPRESENTATION_ITEM('')
);
#501=(
BOUNDED_CURVE()
B_SPLINE_CURVE(2,(#113734,#113735,#113736),.UNSPECIFIED.,.F.,.F.)
B_SPLINE_CURVE_WITH_KNOTS((3,3),(0.0227595441420457,0.0437553375522097),
 .UNSPECIFIED.)
CURVE()
GEOMETRIC_REPRESENTATION_ITEM()
RATIONAL_B_SPLINE_CURVE((1.00144169675951,1.0013858346188,1.))
REPRESENTATION_ITEM('')
);
#502=(
BOUNDED_CURVE()
B_SPLINE_CURVE(2,(#113743,#113744,#113745),.UNSPECIFIED.,.F.,.F.)
B_SPLINE_CURVE_WITH_KNOTS((3,3),(0.,0.020995793410164),.UNSPECIFIED.)
CURVE()
GEOMETRIC_REPRESENTATION_ITEM()
RATIONAL_B_SPLINE_CURVE((1.,1.0013858346188,1.00144169675951))
REPRESENTATION_ITEM('')
);
#503=(
BOUNDED_CURVE()
B_SPLINE_CURVE(2,(#113759,#113760,#113761),.UNSPECIFIED.,.F.,.F.)
B_SPLINE_CURVE_WITH_KNOTS((3,3),(0.,0.0129989367050987),.UNSPECIFIED.)
CURVE()
GEOMETRIC_REPRESENTATION_ITEM()
RATIONAL_B_SPLINE_CURVE((1.,1.00368858134443,1.0050923555823))
REPRESENTATION_ITEM('')
);
#504=(
BOUNDED_CURVE()
B_SPLINE_CURVE(2,(#113765,#113766,#113767),.UNSPECIFIED.,.F.,.F.)
B_SPLINE_CURVE_WITH_KNOTS((3,3),(0.0289719021373686,0.041970838842468),
 .UNSPECIFIED.)
CURVE()
GEOMETRIC_REPRESENTATION_ITEM()
RATIONAL_B_SPLINE_CURVE((1.00509235558236,1.00368858134447,1.))
REPRESENTATION_ITEM('')
);
#505=(
BOUNDED_CURVE()
B_SPLINE_CURVE(2,(#113769,#113770,#113771),.UNSPECIFIED.,.F.,.F.)
B_SPLINE_CURVE_WITH_KNOTS((3,3),(0.,0.012998936705099),.UNSPECIFIED.)
CURVE()
GEOMETRIC_REPRESENTATION_ITEM()
RATIONAL_B_SPLINE_CURVE((1.,1.0036885813445,1.0050923555824))
REPRESENTATION_ITEM('')
);
#506=(
BOUNDED_CURVE()
B_SPLINE_CURVE(2,(#113775,#113776,#113777),.UNSPECIFIED.,.F.,.F.)
B_SPLINE_CURVE_WITH_KNOTS((3,3),(0.0289719021373694,0.0419708388424683),
 .UNSPECIFIED.)
CURVE()
GEOMETRIC_REPRESENTATION_ITEM()
RATIONAL_B_SPLINE_CURVE((1.0050923555824,1.0036885813445,1.))
REPRESENTATION_ITEM('')
);
#507=(
BOUNDED_CURVE()
B_SPLINE_CURVE(2,(#113779,#113780,#113781),.UNSPECIFIED.,.F.,.F.)
B_SPLINE_CURVE_WITH_KNOTS((3,3),(0.,0.0129989367050987),.UNSPECIFIED.)
CURVE()
GEOMETRIC_REPRESENTATION_ITEM()
RATIONAL_B_SPLINE_CURVE((1.,1.00368858134463,1.00509235558257))
REPRESENTATION_ITEM('')
);
#508=(
BOUNDED_CURVE()
B_SPLINE_CURVE(2,(#113785,#113786,#113787),.UNSPECIFIED.,.F.,.F.)
B_SPLINE_CURVE_WITH_KNOTS((3,3),(0.0289719021373689,0.0419708388424683),
 .UNSPECIFIED.)
CURVE()
GEOMETRIC_REPRESENTATION_ITEM()
RATIONAL_B_SPLINE_CURVE((1.00509235558232,1.00368858134444,1.))
REPRESENTATION_ITEM('')
);
#509=(
BOUNDED_CURVE()
B_SPLINE_CURVE(2,(#113789,#113790,#113791),.UNSPECIFIED.,.F.,.F.)
B_SPLINE_CURVE_WITH_KNOTS((3,3),(0.,0.0129989367050993),.UNSPECIFIED.)
CURVE()
GEOMETRIC_REPRESENTATION_ITEM()
RATIONAL_B_SPLINE_CURVE((1.,1.0036885813444,1.00509235558225))
REPRESENTATION_ITEM('')
);
#510=(
BOUNDED_CURVE()
B_SPLINE_CURVE(2,(#113795,#113796,#113797),.UNSPECIFIED.,.F.,.F.)
B_SPLINE_CURVE_WITH_KNOTS((3,3),(0.0289719021373687,0.041970838842468),
 .UNSPECIFIED.)
CURVE()
GEOMETRIC_REPRESENTATION_ITEM()
RATIONAL_B_SPLINE_CURVE((1.00509235558236,1.00368858134447,1.))
REPRESENTATION_ITEM('')
);
#511=(
BOUNDED_CURVE()
B_SPLINE_CURVE(2,(#113799,#113800,#113801),.UNSPECIFIED.,.F.,.F.)
B_SPLINE_CURVE_WITH_KNOTS((3,3),(0.,0.0129989367050989),.UNSPECIFIED.)
CURVE()
GEOMETRIC_REPRESENTATION_ITEM()
RATIONAL_B_SPLINE_CURVE((1.,1.0036885813445,1.0050923555824))
REPRESENTATION_ITEM('')
);
#512=(
BOUNDED_CURVE()
B_SPLINE_CURVE(2,(#113805,#113806,#113807),.UNSPECIFIED.,.F.,.F.)
B_SPLINE_CURVE_WITH_KNOTS((3,3),(0.0289719021373694,0.0419708388424683),
 .UNSPECIFIED.)
CURVE()
GEOMETRIC_REPRESENTATION_ITEM()
RATIONAL_B_SPLINE_CURVE((1.0050923555824,1.0036885813445,1.))
REPRESENTATION_ITEM('')
);
#513=(
BOUNDED_CURVE()
B_SPLINE_CURVE(2,(#113809,#113810,#113811),.UNSPECIFIED.,.F.,.F.)
B_SPLINE_CURVE_WITH_KNOTS((3,3),(0.,0.0129989367050992),.UNSPECIFIED.)
CURVE()
GEOMETRIC_REPRESENTATION_ITEM()
RATIONAL_B_SPLINE_CURVE((1.,1.00368858134448,1.00509235558236))
REPRESENTATION_ITEM('')
);
#514=(
BOUNDED_CURVE()
B_SPLINE_CURVE(2,(#113814,#113815,#113816),.UNSPECIFIED.,.F.,.F.)
B_SPLINE_CURVE_WITH_KNOTS((3,3),(0.0289719021373676,0.0419708388424684),
 .UNSPECIFIED.)
CURVE()
GEOMETRIC_REPRESENTATION_ITEM()
RATIONAL_B_SPLINE_CURVE((1.00509235558214,1.00368858134432,1.))
REPRESENTATION_ITEM('')
);
#515=SHAPE_REPRESENTATION_RELATIONSHIP('SRR','None',#114052,#533);
#516=SHAPE_REPRESENTATION_RELATIONSHIP('SRR','None',#114053,#534);
#517=SHAPE_REPRESENTATION_RELATIONSHIP('SRR','None',#114054,#535);
#518=SHAPE_REPRESENTATION_RELATIONSHIP('SRR','None',#114055,#536);
#519=SHAPE_REPRESENTATION_RELATIONSHIP('SRR','None',#114056,#537);
#520=SHAPE_REPRESENTATION_RELATIONSHIP('SRR','None',#114057,#538);
#521=SHAPE_REPRESENTATION_RELATIONSHIP('SRR','None',#114058,#539);
#522=SHAPE_REPRESENTATION_RELATIONSHIP('SRR','None',#114059,#540);
#523=SHAPE_REPRESENTATION_RELATIONSHIP('SRR','None',#114060,#541);
#524=SHAPE_REPRESENTATION_RELATIONSHIP('SRR','None',#114061,#542);
#525=SHAPE_REPRESENTATION_RELATIONSHIP('SRR','None',#114062,#543);
#526=SHAPE_REPRESENTATION_RELATIONSHIP('SRR','None',#114063,#544);
#527=SHAPE_REPRESENTATION_RELATIONSHIP('SRR','None',#114064,#545);
#528=SHAPE_REPRESENTATION_RELATIONSHIP('SRR','None',#114065,#546);
#529=SHAPE_REPRESENTATION_RELATIONSHIP('SRR','None',#114066,#547);
#530=SHAPE_REPRESENTATION_RELATIONSHIP('SRR','None',#114067,#548);
#531=SHAPE_REPRESENTATION_RELATIONSHIP('SRR','None',#114068,#549);
#532=SHAPE_REPRESENTATION_RELATIONSHIP('SRR','None',#114069,#550);
#533=ADVANCED_BREP_SHAPE_REPRESENTATION('',(#569),#113966);
#534=ADVANCED_BREP_SHAPE_REPRESENTATION('',(#570),#113967);
#535=ADVANCED_BREP_SHAPE_REPRESENTATION('',(#571),#113968);
#536=ADVANCED_BREP_SHAPE_REPRESENTATION('',(#572),#113969);
#537=ADVANCED_BREP_SHAPE_REPRESENTATION('',(#573),#113970);
#538=ADVANCED_BREP_SHAPE_REPRESENTATION('',(#574),#113971);
#539=ADVANCED_BREP_SHAPE_REPRESENTATION('',(#575),#113972);
#540=ADVANCED_BREP_SHAPE_REPRESENTATION('',(#576),#113973);
#541=ADVANCED_BREP_SHAPE_REPRESENTATION('',(#577),#113974);
#542=ADVANCED_BREP_SHAPE_REPRESENTATION('',(#578),#113975);
#543=ADVANCED_BREP_SHAPE_REPRESENTATION('',(#579),#113976);
#544=ADVANCED_BREP_SHAPE_REPRESENTATION('',(#580),#113977);
#545=ADVANCED_BREP_SHAPE_REPRESENTATION('',(#581),#113978);
#546=ADVANCED_BREP_SHAPE_REPRESENTATION('',(#582),#113979);
#547=ADVANCED_BREP_SHAPE_REPRESENTATION('',(#583),#113980);
#548=ADVANCED_BREP_SHAPE_REPRESENTATION('',(#584),#113981);
#549=ADVANCED_BREP_SHAPE_REPRESENTATION('',(#585),#113982);
#550=ADVANCED_BREP_SHAPE_REPRESENTATION('',(#586),#113983);
#551=STYLED_ITEM('',(#114289),#569);
#552=STYLED_ITEM('',(#114324),#570);
#553=STYLED_ITEM('',(#114324),#571);
#554=STYLED_ITEM('',(#114310),#572);
#555=STYLED_ITEM('',(#114303),#573);
#556=STYLED_ITEM('',(#114324),#574);
#557=STYLED_ITEM('',(#114296),#575);
#558=STYLED_ITEM('',(#114296),#576);
#559=STYLED_ITEM('',(#114289),#577);
#560=STYLED_ITEM('',(#114296),#578);
#561=STYLED_ITEM('',(#114317),#579);
#562=STYLED_ITEM('',(#114317),#580);
#563=STYLED_ITEM('',(#114317),#581);
#564=STYLED_ITEM('',(#114317),#582);
#565=STYLED_ITEM('',(#114317),#583);
#566=STYLED_ITEM('',(#114317),#584);
#567=STYLED_ITEM('',(#114317),#585);
#568=STYLED_ITEM('',(#114310),#586);
#569=MANIFOLD_SOLID_BREP('Cast Iron Dovetail Base Block LWX40 x 220',#60392);
#570=MANIFOLD_SOLID_BREP('Machined Alloy Sliding Carriage 40 x 40',#60393);
#571=MANIFOLD_SOLID_BREP('Adjustable Brass Gib Strip',#60394);
#572=MANIFOLD_SOLID_BREP('Precision Drive Spindle D5 (knob shaft)',#60395);
#573=MANIFOLD_SOLID_BREP('Spur Pinion m0.5 z16 with Hub',#60396);
#574=MANIFOLD_SOLID_BREP('Knurled Adjustment Knob D20',#60397);
#575=MANIFOLD_SOLID_BREP('Sintered Bronze Flanged Bush 5 x 9.6 x 8',#60398);
#576=MANIFOLD_SOLID_BREP('Carriage Drive Gear Rack m0.5 x 6 x 216',#60399);
#577=MANIFOLD_SOLID_BREP('Base Lock Knob Lever (stainless, bent)',#60400);
#578=MANIFOLD_SOLID_BREP('Scale Pointer - Vernier Plate',#60401);
#579=MANIFOLD_SOLID_BREP(
'ISO 1207 - M4 x 8 - 4.8 (Lock Clamp Screw, slotted cheese head)',#60402);
#580=MANIFOLD_SOLID_BREP('ISO 4026 - M3 x 3 - 45H (Knob Set Screw)',#60403);
#581=MANIFOLD_SOLID_BREP('ISO 4026 - M2 x 2 - 45H (Pinion Set Screw)',#60404);
#582=MANIFOLD_SOLID_BREP(
'ISO 4026 - M3 x 6 - 45H (Gib Adjustment Screw)',#60405);
#583=MANIFOLD_SOLID_BREP(
'ISO 4026 - M3 x 4 - 45H (Bush Retaining Screw)',#60406);
#584=MANIFOLD_SOLID_BREP('ISO 10642 - M2 x 4 - 10.9 (Pointer Screw)',#60407);
#585=MANIFOLD_SOLID_BREP('ISO 4762 - M2.5 x 6 - 12.9 (Rack Screw)',#60408);
#586=MANIFOLD_SOLID_BREP(
'ISO 2338 - 2 m6 x 6 - St (Carriage Travel Stop Pin)',#60409);
#587=ELLIPSE('',#61749,0.707106781186562,0.499999999999998);
#588=ELLIPSE('',#61756,0.70710678118656,0.5);
#589=ELLIPSE('',#61760,0.707106781186549,0.499999999999998);
#590=ELLIPSE('',#61761,0.707106781186545,0.499999999999998);
#591=ELLIPSE('',#61762,0.707106781186558,0.499999999999998);
#592=ELLIPSE('',#61770,0.707106781186561,0.5);
#593=ELLIPSE('',#61787,0.707106781186547,0.5);
#594=ELLIPSE('',#61805,0.707106781186548,0.5);
#595=ELLIPSE('',#61838,1.78978583448783,1.54999999999999);
#596=ELLIPSE('',#61844,1.78978583448783,1.54999999999999);
#597=ELLIPSE('',#61849,2.36713610367747,2.05);
#598=ELLIPSE('',#61950,0.692820323027559,0.489897948556646);
#599=ELLIPSE('',#61952,0.692820323027559,0.489897948556646);
#600=ELLIPSE('',#61954,0.692820323027559,0.489897948556646);
#601=ELLIPSE('',#62936,0.751653400711626,0.5);
#602=ELLIPSE('',#62946,0.751653400711626,0.5);
#603=CYLINDRICAL_SURFACE('',#61679,1.);
#604=CYLINDRICAL_SURFACE('',#61681,1.00000000000001);
#605=CYLINDRICAL_SURFACE('',#61686,1.29999999999999);
#606=CYLINDRICAL_SURFACE('',#61693,1.3);
#607=CYLINDRICAL_SURFACE('',#61696,3.00000000000001);
#608=CYLINDRICAL_SURFACE('',#61701,3.);
#609=CYLINDRICAL_SURFACE('',#61706,3.);
#610=CYLINDRICAL_SURFACE('',#61711,3.00000000000001);
#611=CYLINDRICAL_SURFACE('',#61716,3.00000000000001);
#612=CYLINDRICAL_SURFACE('',#61721,3.00000000000001);
#613=CYLINDRICAL_SURFACE('',#61732,2.04999999999998);
#614=CYLINDRICAL_SURFACE('',#61735,2.05);
#615=CYLINDRICAL_SURFACE('',#61738,2.05);
#616=CYLINDRICAL_SURFACE('',#61741,2.05);
#617=CYLINDRICAL_SURFACE('',#61744,2.05);
#618=CYLINDRICAL_SURFACE('',#61747,2.04999999999998);
#619=CYLINDRICAL_SURFACE('',#61759,0.499999999999998);
#620=CYLINDRICAL_SURFACE('',#61809,0.5);
#621=CYLINDRICAL_SURFACE('',#61824,1.05);
#622=CYLINDRICAL_SURFACE('',#61828,1.05);
#623=CYLINDRICAL_SURFACE('',#61837,1.54999999999999);
#624=CYLINDRICAL_SURFACE('',#61843,1.54999999999999);
#625=CYLINDRICAL_SURFACE('',#61848,2.05);
#626=CYLINDRICAL_SURFACE('',#61856,1.05);
#627=CYLINDRICAL_SURFACE('',#61869,1.05);
#628=CYLINDRICAL_SURFACE('',#61875,1.05);
#629=CYLINDRICAL_SURFACE('',#61887,1.54999999999999);
#630=CYLINDRICAL_SURFACE('',#61891,1.54999999999999);
#631=CYLINDRICAL_SURFACE('',#61895,1.54999999999999);
#632=CYLINDRICAL_SURFACE('',#61899,1.54999999999999);
#633=CYLINDRICAL_SURFACE('',#61908,4.8);
#634=CYLINDRICAL_SURFACE('',#61914,2.525);
#635=CYLINDRICAL_SURFACE('',#61984,2.5);
#636=CYLINDRICAL_SURFACE('',#61992,1.05);
#637=CYLINDRICAL_SURFACE('',#61998,4.50000000000305);
#638=CYLINDRICAL_SURFACE('',#62003,3.375);
#639=CYLINDRICAL_SURFACE('',#62039,4.50000000000305);
#640=CYLINDRICAL_SURFACE('',#62045,4.50000000000305);
#641=CYLINDRICAL_SURFACE('',#62051,4.50000000000305);
#642=CYLINDRICAL_SURFACE('',#62057,4.50000000000305);
#643=CYLINDRICAL_SURFACE('',#62063,4.50000000000305);
#644=CYLINDRICAL_SURFACE('',#62069,4.50000000000305);
#645=CYLINDRICAL_SURFACE('',#62075,4.50000000000305);
#646=CYLINDRICAL_SURFACE('',#62081,4.50000000000305);
#647=CYLINDRICAL_SURFACE('',#62087,4.50000000000305);
#648=CYLINDRICAL_SURFACE('',#62093,4.50000000000305);
#649=CYLINDRICAL_SURFACE('',#62099,4.50000000000305);
#650=CYLINDRICAL_SURFACE('',#62105,4.50000000000305);
#651=CYLINDRICAL_SURFACE('',#62111,4.50000000000305);
#652=CYLINDRICAL_SURFACE('',#62117,4.50000000000305);
#653=CYLINDRICAL_SURFACE('',#62122,4.50000000000305);
#654=CYLINDRICAL_SURFACE('',#62127,2.5);
#655=CYLINDRICAL_SURFACE('',#62133,4.49999999999999);
#656=CYLINDRICAL_SURFACE('',#62142,1.54999999999999);
#657=CYLINDRICAL_SURFACE('',#62189,10.);
#658=CYLINDRICAL_SURFACE('',#62191,10.);
#659=CYLINDRICAL_SURFACE('',#62195,10.);
#660=CYLINDRICAL_SURFACE('',#62240,10.);
#661=CYLINDRICAL_SURFACE('',#62241,10.);
#662=CYLINDRICAL_SURFACE('',#62244,10.);
#663=CYLINDRICAL_SURFACE('',#62249,10.);
#664=CYLINDRICAL_SURFACE('',#62250,10.);
#665=CYLINDRICAL_SURFACE('',#62253,10.);
#666=CYLINDRICAL_SURFACE('',#62258,10.);
#667=CYLINDRICAL_SURFACE('',#62259,10.);
#668=CYLINDRICAL_SURFACE('',#62262,10.);
#669=CYLINDRICAL_SURFACE('',#62267,10.);
#670=CYLINDRICAL_SURFACE('',#62268,10.);
#671=CYLINDRICAL_SURFACE('',#62271,10.);
#672=CYLINDRICAL_SURFACE('',#62276,10.);
#673=CYLINDRICAL_SURFACE('',#62277,10.);
#674=CYLINDRICAL_SURFACE('',#62280,10.);
#675=CYLINDRICAL_SURFACE('',#62285,10.);
#676=CYLINDRICAL_SURFACE('',#62286,10.);
#677=CYLINDRICAL_SURFACE('',#62289,10.);
#678=CYLINDRICAL_SURFACE('',#62294,10.);
#679=CYLINDRICAL_SURFACE('',#62295,10.);
#680=CYLINDRICAL_SURFACE('',#62298,10.);
#681=CYLINDRICAL_SURFACE('',#62303,10.);
#682=CYLINDRICAL_SURFACE('',#62304,10.);
#683=CYLINDRICAL_SURFACE('',#62307,10.);
#684=CYLINDRICAL_SURFACE('',#62312,10.);
#685=CYLINDRICAL_SURFACE('',#62313,10.);
#686=CYLINDRICAL_SURFACE('',#62316,10.);
#687=CYLINDRICAL_SURFACE('',#62321,10.);
#688=CYLINDRICAL_SURFACE('',#62322,10.);
#689=CYLINDRICAL_SURFACE('',#62325,10.);
#690=CYLINDRICAL_SURFACE('',#62330,10.);
#691=CYLINDRICAL_SURFACE('',#62331,10.);
#692=CYLINDRICAL_SURFACE('',#62334,10.);
#693=CYLINDRICAL_SURFACE('',#62339,10.);
#694=CYLINDRICAL_SURFACE('',#62340,10.);
#695=CYLINDRICAL_SURFACE('',#62343,10.);
#696=CYLINDRICAL_SURFACE('',#62355,4.);
#697=CYLINDRICAL_SURFACE('',#62361,6.);
#698=CYLINDRICAL_SURFACE('',#62366,10.);
#699=CYLINDRICAL_SURFACE('',#62374,2.51000000000001);
#700=CYLINDRICAL_SURFACE('',#62383,4.8);
#701=CYLINDRICAL_SURFACE('',#62389,6.);
#702=CYLINDRICAL_SURFACE('',#62395,2.51000000000001);
#703=CYLINDRICAL_SURFACE('',#62400,2.5);
#704=CYLINDRICAL_SURFACE('',#62406,2.5);
#705=CYLINDRICAL_SURFACE('',#62413,1.45);
#706=CYLINDRICAL_SURFACE('',#62415,1.45);
#707=CYLINDRICAL_SURFACE('',#62924,0.5);
#708=CYLINDRICAL_SURFACE('',#62927,5.);
#709=CYLINDRICAL_SURFACE('',#62930,0.5);
#710=CYLINDRICAL_SURFACE('',#62934,0.5);
#711=CYLINDRICAL_SURFACE('',#62939,0.5);
#712=CYLINDRICAL_SURFACE('',#62945,0.5);
#713=CYLINDRICAL_SURFACE('',#62953,2.15);
#714=CYLINDRICAL_SURFACE('',#63031,1.09999999999999);
#715=CYLINDRICAL_SURFACE('',#63042,1.09999999999999);
#716=CYLINDRICAL_SURFACE('',#63050,0.800000000000001);
#717=CYLINDRICAL_SURFACE('',#63053,0.800000000000001);
#718=CYLINDRICAL_SURFACE('',#63059,1.954);
#719=CYLINDRICAL_SURFACE('',#63061,1.954);
#720=CYLINDRICAL_SURFACE('',#63062,1.954);
#721=CYLINDRICAL_SURFACE('',#63063,1.954);
#722=CYLINDRICAL_SURFACE('',#63064,1.954);
#723=CYLINDRICAL_SURFACE('',#63065,1.954);
#724=CYLINDRICAL_SURFACE('',#63066,1.954);
#725=CYLINDRICAL_SURFACE('',#63067,1.954);
#726=CYLINDRICAL_SURFACE('',#63068,1.954);
#727=CYLINDRICAL_SURFACE('',#63069,1.954);
#728=CYLINDRICAL_SURFACE('',#63070,1.954);
#729=CYLINDRICAL_SURFACE('',#63071,1.5555);
#730=CYLINDRICAL_SURFACE('',#63073,1.5555);
#731=CYLINDRICAL_SURFACE('',#63074,1.5555);
#732=CYLINDRICAL_SURFACE('',#63075,1.5555);
#733=CYLINDRICAL_SURFACE('',#63076,1.5555);
#734=CYLINDRICAL_SURFACE('',#63077,1.5555);
#735=CYLINDRICAL_SURFACE('',#63078,1.5555);
#736=CYLINDRICAL_SURFACE('',#63079,1.5555);
#737=CYLINDRICAL_SURFACE('',#63080,1.5555);
#738=CYLINDRICAL_SURFACE('',#63081,1.5555);
#739=CYLINDRICAL_SURFACE('',#63089,1.5555);
#740=CYLINDRICAL_SURFACE('',#63095,1.954);
#741=CYLINDRICAL_SURFACE('',#63111,3.5);
#742=CYLINDRICAL_SURFACE('',#63116,1.4635);
#743=CYLINDRICAL_SURFACE('',#63118,1.4635);
#744=CYLINDRICAL_SURFACE('',#63119,1.4635);
#745=CYLINDRICAL_SURFACE('',#63120,1.4635);
#746=CYLINDRICAL_SURFACE('',#63121,1.4635);
#747=CYLINDRICAL_SURFACE('',#63122,1.17775);
#748=CYLINDRICAL_SURFACE('',#63124,1.17775);
#749=CYLINDRICAL_SURFACE('',#63125,1.17775);
#750=CYLINDRICAL_SURFACE('',#63126,1.17775);
#751=CYLINDRICAL_SURFACE('',#63134,1.17775);
#752=CYLINDRICAL_SURFACE('',#63143,0.816025403784444);
#753=CYLINDRICAL_SURFACE('',#63145,0.816025403784444);
#754=CYLINDRICAL_SURFACE('',#63147,0.816025403784444);
#755=CYLINDRICAL_SURFACE('',#63149,0.816025403784444);
#756=CYLINDRICAL_SURFACE('',#63151,0.816025403784444);
#757=CYLINDRICAL_SURFACE('',#63153,0.816025403784444);
#758=CYLINDRICAL_SURFACE('',#63183,1.4635);
#759=CYLINDRICAL_SURFACE('',#63189,0.96675);
#760=CYLINDRICAL_SURFACE('',#63191,0.96675);
#761=CYLINDRICAL_SURFACE('',#63192,0.96675);
#762=CYLINDRICAL_SURFACE('',#63193,0.96675);
#763=CYLINDRICAL_SURFACE('',#63195,0.739000000000001);
#764=CYLINDRICAL_SURFACE('',#63197,0.739000000000001);
#765=CYLINDRICAL_SURFACE('',#63198,0.739000000000001);
#766=CYLINDRICAL_SURFACE('',#63205,0.739000000000001);
#767=CYLINDRICAL_SURFACE('',#63214,0.469615242270667);
#768=CYLINDRICAL_SURFACE('',#63216,0.469615242270667);
#769=CYLINDRICAL_SURFACE('',#63218,0.469615242270667);
#770=CYLINDRICAL_SURFACE('',#63220,0.469615242270667);
#771=CYLINDRICAL_SURFACE('',#63222,0.469615242270667);
#772=CYLINDRICAL_SURFACE('',#63224,0.469615242270667);
#773=CYLINDRICAL_SURFACE('',#63254,0.96675);
#774=CYLINDRICAL_SURFACE('',#63260,1.4635);
#775=CYLINDRICAL_SURFACE('',#63262,1.4635);
#776=CYLINDRICAL_SURFACE('',#63263,1.4635);
#777=CYLINDRICAL_SURFACE('',#63264,1.4635);
#778=CYLINDRICAL_SURFACE('',#63265,1.4635);
#779=CYLINDRICAL_SURFACE('',#63266,1.4635);
#780=CYLINDRICAL_SURFACE('',#63267,1.4635);
#781=CYLINDRICAL_SURFACE('',#63268,1.4635);
#782=CYLINDRICAL_SURFACE('',#63269,1.4635);
#783=CYLINDRICAL_SURFACE('',#63270,1.4635);
#784=CYLINDRICAL_SURFACE('',#63271,1.4635);
#785=CYLINDRICAL_SURFACE('',#63272,1.17775);
#786=CYLINDRICAL_SURFACE('',#63274,1.17775);
#787=CYLINDRICAL_SURFACE('',#63275,1.17775);
#788=CYLINDRICAL_SURFACE('',#63276,1.17775);
#789=CYLINDRICAL_SURFACE('',#63277,1.17775);
#790=CYLINDRICAL_SURFACE('',#63278,1.17775);
#791=CYLINDRICAL_SURFACE('',#63279,1.17775);
#792=CYLINDRICAL_SURFACE('',#63280,1.17775);
#793=CYLINDRICAL_SURFACE('',#63281,1.17775);
#794=CYLINDRICAL_SURFACE('',#63282,1.17775);
#795=CYLINDRICAL_SURFACE('',#63290,1.17775);
#796=CYLINDRICAL_SURFACE('',#63299,0.816025403784426);
#797=CYLINDRICAL_SURFACE('',#63301,0.816025403784426);
#798=CYLINDRICAL_SURFACE('',#63303,0.816025403784426);
#799=CYLINDRICAL_SURFACE('',#63305,0.816025403784426);
#800=CYLINDRICAL_SURFACE('',#63307,0.816025403784426);
#801=CYLINDRICAL_SURFACE('',#63309,0.816025403784426);
#802=CYLINDRICAL_SURFACE('',#63339,1.4635);
#803=CYLINDRICAL_SURFACE('',#63345,0.96675);
#804=CYLINDRICAL_SURFACE('',#63347,0.96675);
#805=CYLINDRICAL_SURFACE('',#63348,0.96675);
#806=CYLINDRICAL_SURFACE('',#63349,0.96675);
#807=CYLINDRICAL_SURFACE('',#63350,0.96675);
#808=CYLINDRICAL_SURFACE('',#63351,0.96675);
#809=CYLINDRICAL_SURFACE('',#63352,0.739000000000001);
#810=CYLINDRICAL_SURFACE('',#63354,0.739000000000001);
#811=CYLINDRICAL_SURFACE('',#63356,0.739000000000001);
#812=CYLINDRICAL_SURFACE('',#63357,0.739000000000001);
#813=CYLINDRICAL_SURFACE('',#63358,0.739000000000001);
#814=CYLINDRICAL_SURFACE('',#63359,0.739000000000001);
#815=CYLINDRICAL_SURFACE('',#63367,0.739000000000001);
#816=CYLINDRICAL_SURFACE('',#63376,0.469615242270667);
#817=CYLINDRICAL_SURFACE('',#63378,0.469615242270667);
#818=CYLINDRICAL_SURFACE('',#63380,0.469615242270667);
#819=CYLINDRICAL_SURFACE('',#63382,0.469615242270667);
#820=CYLINDRICAL_SURFACE('',#63384,0.469615242270667);
#821=CYLINDRICAL_SURFACE('',#63386,0.469615242270667);
#822=CYLINDRICAL_SURFACE('',#63416,0.96675);
#823=CYLINDRICAL_SURFACE('',#63422,0.96675);
#824=CYLINDRICAL_SURFACE('',#63424,0.96675);
#825=CYLINDRICAL_SURFACE('',#63425,0.96675);
#826=CYLINDRICAL_SURFACE('',#63426,0.96675);
#827=CYLINDRICAL_SURFACE('',#63427,0.96675);
#828=CYLINDRICAL_SURFACE('',#63428,0.96675);
#829=CYLINDRICAL_SURFACE('',#63429,0.96675);
#830=CYLINDRICAL_SURFACE('',#63430,0.96675);
#831=CYLINDRICAL_SURFACE('',#63432,0.739000000000001);
#832=CYLINDRICAL_SURFACE('',#63434,0.739000000000001);
#833=CYLINDRICAL_SURFACE('',#63435,0.739000000000001);
#834=CYLINDRICAL_SURFACE('',#63436,0.739000000000001);
#835=CYLINDRICAL_SURFACE('',#63437,0.739000000000001);
#836=CYLINDRICAL_SURFACE('',#63438,0.739000000000001);
#837=CYLINDRICAL_SURFACE('',#63439,0.739000000000001);
#838=CYLINDRICAL_SURFACE('',#63446,0.739000000000001);
#839=CYLINDRICAL_SURFACE('',#63457,0.96675);
#840=CYLINDRICAL_SURFACE('',#63463,1.215);
#841=CYLINDRICAL_SURFACE('',#63465,1.215);
#842=CYLINDRICAL_SURFACE('',#63466,1.215);
#843=CYLINDRICAL_SURFACE('',#63467,1.215);
#844=CYLINDRICAL_SURFACE('',#63468,1.215);
#845=CYLINDRICAL_SURFACE('',#63469,1.215);
#846=CYLINDRICAL_SURFACE('',#63470,1.215);
#847=CYLINDRICAL_SURFACE('',#63471,1.215);
#848=CYLINDRICAL_SURFACE('',#63472,1.215);
#849=CYLINDRICAL_SURFACE('',#63473,1.215);
#850=CYLINDRICAL_SURFACE('',#63474,1.215);
#851=CYLINDRICAL_SURFACE('',#63475,1.215);
#852=CYLINDRICAL_SURFACE('',#63476,1.215);
#853=CYLINDRICAL_SURFACE('',#63477,0.958249999999999);
#854=CYLINDRICAL_SURFACE('',#63479,0.958249999999999);
#855=CYLINDRICAL_SURFACE('',#63480,0.958249999999999);
#856=CYLINDRICAL_SURFACE('',#63481,0.958249999999999);
#857=CYLINDRICAL_SURFACE('',#63482,0.958249999999999);
#858=CYLINDRICAL_SURFACE('',#63483,0.958249999999999);
#859=CYLINDRICAL_SURFACE('',#63484,0.958249999999999);
#860=CYLINDRICAL_SURFACE('',#63485,0.958249999999999);
#861=CYLINDRICAL_SURFACE('',#63486,0.958249999999999);
#862=CYLINDRICAL_SURFACE('',#63487,0.958249999999999);
#863=CYLINDRICAL_SURFACE('',#63488,0.958249999999999);
#864=CYLINDRICAL_SURFACE('',#63489,0.958249999999999);
#865=CYLINDRICAL_SURFACE('',#63497,0.958249999999999);
#866=CYLINDRICAL_SURFACE('',#63501,1.215);
#867=CYLINDRICAL_SURFACE('',#63512,2.25);
#868=CYLINDRICAL_SURFACE('',#63705,1.10470053837925);
#869=CYLINDRICAL_SURFACE('',#63707,1.10470053837925);
#870=CYLINDRICAL_SURFACE('',#63709,1.10470053837925);
#871=CYLINDRICAL_SURFACE('',#63711,1.10470053837925);
#872=CYLINDRICAL_SURFACE('',#63713,1.10470053837925);
#873=CYLINDRICAL_SURFACE('',#63715,1.10470053837925);
#874=CYLINDRICAL_SURFACE('',#63747,1.);
#875=CONICAL_SURFACE('',#61675,0.999999999999979,1.02974425867664);
#876=CONICAL_SURFACE('',#61677,1.,1.02974425867665);
#877=CONICAL_SURFACE('',#61683,1.39999999999999,0.785398163397437);
#878=CONICAL_SURFACE('',#61690,1.30000000000003,1.02974425867666);
#879=CONICAL_SURFACE('',#61691,1.4,0.785398163397448);
#880=CONICAL_SURFACE('',#61695,1.3,1.02974425867665);
#881=CONICAL_SURFACE('',#61726,2.19999999999999,0.785398163397467);
#882=CONICAL_SURFACE('',#61733,2.2,0.785398163397438);
#883=CONICAL_SURFACE('',#61736,2.2,0.785398163397438);
#884=CONICAL_SURFACE('',#61739,2.2,0.785398163397445);
#885=CONICAL_SURFACE('',#61742,2.2,0.785398163397445);
#886=CONICAL_SURFACE('',#61745,2.19999999999999,0.785398163397467);
#887=CONICAL_SURFACE('',#61813,2.2,0.785398163397448);
#888=CONICAL_SURFACE('',#61816,1.12500000000001,0.785398163397478);
#889=CONICAL_SURFACE('',#61826,1.12500000000001,0.785398163397478);
#890=CONICAL_SURFACE('',#61830,0.525000000000002,1.02974425867666);
#891=CONICAL_SURFACE('',#61831,0.525000000000002,1.02974425867665);
#892=CONICAL_SURFACE('',#61832,1.675,0.785398163397455);
#893=CONICAL_SURFACE('',#61839,1.675,0.785398163397455);
#894=CONICAL_SURFACE('',#61845,2.2,0.785398163397448);
#895=CONICAL_SURFACE('',#61851,1.125,0.785398163397434);
#896=CONICAL_SURFACE('',#61860,1.12500000000001,0.785398163397463);
#897=CONICAL_SURFACE('',#61873,1.12500000000001,0.785398163397463);
#898=CONICAL_SURFACE('',#61885,1.675,0.785398163397457);
#899=CONICAL_SURFACE('',#61889,1.675,0.785398163397457);
#900=CONICAL_SURFACE('',#61893,1.675,0.785398163397457);
#901=CONICAL_SURFACE('',#61897,1.675,0.785398163397457);
#902=CONICAL_SURFACE('',#61901,1.54999999999999,1.02974425867665);
#903=CONICAL_SURFACE('',#61902,1.54999999999999,1.02974425867665);
#904=CONICAL_SURFACE('',#61903,1.54999999999999,1.02974425867665);
#905=CONICAL_SURFACE('',#61904,1.54999999999999,1.02974425867665);
#906=CONICAL_SURFACE('',#61905,4.95,0.785398163397434);
#907=CONICAL_SURFACE('',#61912,1.26250000000001,1.02974425867666);
#908=CONICAL_SURFACE('',#61949,1.40000000000001,0.78539816339745);
#909=CONICAL_SURFACE('',#61951,1.40000000000001,0.78539816339745);
#910=CONICAL_SURFACE('',#61953,1.40000000000001,0.78539816339745);
#911=CONICAL_SURFACE('',#61982,2.34999999999999,0.785398163397437);
#912=CONICAL_SURFACE('',#61986,2.34999999999999,0.785398163397448);
#913=CONICAL_SURFACE('',#62135,4.34999999999999,0.785398163397448);
#914=CONICAL_SURFACE('',#62147,9.60000000000001,0.785398163397448);
#915=CONICAL_SURFACE('',#62197,9.60000000000001,0.785398163397448);
#916=CONICAL_SURFACE('',#62348,2.66000000000002,0.785398163397448);
#917=CONICAL_SURFACE('',#62353,3.85000000000002,0.785398163397448);
#918=CONICAL_SURFACE('',#62357,4.20000000000002,0.785398163397459);
#919=CONICAL_SURFACE('',#62363,6.20000000000001,0.785398163397459);
#920=CONICAL_SURFACE('',#62369,7.19999999999999,0.785398163397448);
#921=CONICAL_SURFACE('',#62372,1.25500000000001,1.0321363555003);
#922=CONICAL_SURFACE('',#62376,2.66000000000002,0.785398163397434);
#923=CONICAL_SURFACE('',#62381,4.65,0.785398163397463);
#924=CONICAL_SURFACE('',#62387,5.85000000000001,0.785398163397434);
#925=CONICAL_SURFACE('',#62393,2.66000000000002,0.785398163397434);
#926=CONICAL_SURFACE('',#62397,2.65000000000001,0.785398163397467);
#927=CONICAL_SURFACE('',#62403,2.65,0.785398163397448);
#928=CONICAL_SURFACE('',#63034,1.54999999999999,0.785398163397458);
#929=CONICAL_SURFACE('',#63045,1.54999999999999,0.785398163397448);
#930=CONICAL_SURFACE('',#63103,3.29999999999998,0.78539816339746);
#931=CONICAL_SURFACE('',#63106,3.29999999999998,0.78539816339746);
#932=CONICAL_SURFACE('',#63112,1.75000000000001,0.785398163397437);
#933=CONICAL_SURFACE('',#63135,0.916025403784442,0.785398163397437);
#934=CONICAL_SURFACE('',#63176,0.866025403784434,1.02974425867665);
#935=CONICAL_SURFACE('',#63182,1.35000000000002,0.785398163397434);
#936=CONICAL_SURFACE('',#63185,1.25,0.785398163397457);
#937=CONICAL_SURFACE('',#63206,0.569615242270665,0.785398163397437);
#938=CONICAL_SURFACE('',#63247,0.519615242270657,1.02974425867665);
#939=CONICAL_SURFACE('',#63253,0.88000000000001,0.785398163397439);
#940=CONICAL_SURFACE('',#63256,0.749999999999993,0.785398163397439);
#941=CONICAL_SURFACE('',#63291,0.916025403784424,0.785398163397484);
#942=CONICAL_SURFACE('',#63332,0.866025403784434,1.02974425867665);
#943=CONICAL_SURFACE('',#63338,1.34999999999998,0.785398163397437);
#944=CONICAL_SURFACE('',#63341,1.25,0.785398163397439);
#945=CONICAL_SURFACE('',#63368,0.569615242270665,0.785398163397437);
#946=CONICAL_SURFACE('',#63409,0.519615242270657,1.02974425867665);
#947=CONICAL_SURFACE('',#63415,0.88000000000001,0.78539816339743);
#948=CONICAL_SURFACE('',#63418,0.749999999999993,0.785398163397435);
#949=CONICAL_SURFACE('',#63456,0.899999999999999,0.785398163397426);
#950=CONICAL_SURFACE('',#63459,1.45,0.785398163397448);
#951=CONICAL_SURFACE('',#63505,1.04,0.785398163397448);
#952=CONICAL_SURFACE('',#63694,2.1,0.785398163397448);
#953=CONICAL_SURFACE('',#63698,1.20470053837925,0.785398163397454);
#954=CONICAL_SURFACE('',#63738,1.15470053837925,1.02974425867666);
#955=CONICAL_SURFACE('',#63745,0.85,0.785398163397447);
#956=CONICAL_SURFACE('',#63749,0.85,0.785398163397448);
#957=CIRCLE('',#61666,0.499999999999998);
#958=CIRCLE('',#61667,0.5);
#959=CIRCLE('',#61672,2.34999999999999);
#960=CIRCLE('',#61673,2.35);
#961=CIRCLE('',#61674,2.34999999999999);
#962=CIRCLE('',#61676,1.00000000000001);
#963=CIRCLE('',#61678,1.);
#964=CIRCLE('',#61680,1.);
#965=CIRCLE('',#61682,1.00000000000001);
#966=CIRCLE('',#61684,1.49999999999999);
#967=CIRCLE('',#61685,1.29999999999999);
#968=CIRCLE('',#61687,1.29999999999999);
#969=CIRCLE('',#61689,1.5);
#970=CIRCLE('',#61692,1.3);
#971=CIRCLE('',#61694,1.3);
#972=CIRCLE('',#61697,3.00000000000001);
#973=CIRCLE('',#61698,3.00000000000001);
#974=CIRCLE('',#61700,2.04999999999998);
#975=CIRCLE('',#61702,3.);
#976=CIRCLE('',#61703,3.);
#977=CIRCLE('',#61705,2.05);
#978=CIRCLE('',#61707,3.);
#979=CIRCLE('',#61708,3.);
#980=CIRCLE('',#61710,2.05);
#981=CIRCLE('',#61712,3.00000000000001);
#982=CIRCLE('',#61713,3.00000000000001);
#983=CIRCLE('',#61715,2.05);
#984=CIRCLE('',#61717,3.00000000000001);
#985=CIRCLE('',#61718,3.00000000000001);
#986=CIRCLE('',#61720,2.05);
#987=CIRCLE('',#61722,3.00000000000001);
#988=CIRCLE('',#61723,3.00000000000001);
#989=CIRCLE('',#61725,2.04999999999998);
#990=CIRCLE('',#61727,2.04999999999998);
#991=CIRCLE('',#61729,2.34999999999999);
#992=CIRCLE('',#61730,2.35);
#993=CIRCLE('',#61731,2.34999999999999);
#994=CIRCLE('',#61734,2.05);
#995=CIRCLE('',#61737,2.05);
#996=CIRCLE('',#61740,2.05);
#997=CIRCLE('',#61743,2.05);
#998=CIRCLE('',#61746,2.04999999999998);
#999=CIRCLE('',#61763,0.499999999999998);
#1000=CIRCLE('',#61807,0.5);
#1001=CIRCLE('',#61814,2.35);
#1002=CIRCLE('',#61815,2.05);
#1003=CIRCLE('',#61817,1.20000000000001);
#1004=CIRCLE('',#61818,1.05);
#1005=CIRCLE('',#61819,1.20000000000001);
#1006=CIRCLE('',#61821,1.20000000000001);
#1007=CIRCLE('',#61822,1.20000000000001);
#1008=CIRCLE('',#61823,5.1);
#1009=CIRCLE('',#61825,1.05);
#1010=CIRCLE('',#61827,1.05);
#1011=CIRCLE('',#61829,1.05);
#1012=CIRCLE('',#61833,1.8);
#1013=CIRCLE('',#61834,1.54999999999999);
#1014=CIRCLE('',#61835,1.8);
#1015=CIRCLE('',#61840,1.8);
#1016=CIRCLE('',#61841,1.54999999999999);
#1017=CIRCLE('',#61842,1.8);
#1018=CIRCLE('',#61846,2.05);
#1019=CIRCLE('',#61847,2.35);
#1020=CIRCLE('',#61852,1.2);
#1021=CIRCLE('',#61853,1.05);
#1022=CIRCLE('',#61854,1.2);
#1023=CIRCLE('',#61857,1.05);
#1024=CIRCLE('',#61858,1.05);
#1025=CIRCLE('',#61859,1.05);
#1026=CIRCLE('',#61861,1.20000000000001);
#1027=CIRCLE('',#61862,1.05);
#1028=CIRCLE('',#61864,1.20000000000001);
#1029=CIRCLE('',#61865,1.8);
#1030=CIRCLE('',#61866,1.8);
#1031=CIRCLE('',#61867,1.8);
#1032=CIRCLE('',#61868,1.8);
#1033=CIRCLE('',#61870,1.05);
#1034=CIRCLE('',#61871,1.05);
#1035=CIRCLE('',#61872,1.05);
#1036=CIRCLE('',#61874,1.05);
#1037=CIRCLE('',#61876,1.05);
#1038=CIRCLE('',#61877,1.05);
#1039=CIRCLE('',#61878,1.05);
#1040=CIRCLE('',#61886,1.54999999999999);
#1041=CIRCLE('',#61888,1.54999999999999);
#1042=CIRCLE('',#61890,1.54999999999999);
#1043=CIRCLE('',#61892,1.54999999999999);
#1044=CIRCLE('',#61894,1.54999999999999);
#1045=CIRCLE('',#61896,1.54999999999999);
#1046=CIRCLE('',#61898,1.54999999999999);
#1047=CIRCLE('',#61900,1.54999999999999);
#1048=CIRCLE('',#61906,4.8);
#1049=CIRCLE('',#61907,4.8);
#1050=CIRCLE('',#61909,4.8);
#1051=CIRCLE('',#61910,4.8);
#1052=CIRCLE('',#61911,4.8);
#1053=CIRCLE('',#61913,2.525);
#1054=CIRCLE('',#61915,2.525);
#1055=CIRCLE('',#61971,2.5);
#1056=CIRCLE('',#61973,2.5);
#1057=CIRCLE('',#61976,2.5);
#1058=CIRCLE('',#61978,2.5);
#1059=CIRCLE('',#61981,2.20000000000001);
#1060=CIRCLE('',#61983,2.5);
#1061=CIRCLE('',#61985,2.5);
#1062=CIRCLE('',#61987,2.20000000000001);
#1063=CIRCLE('',#61991,1.05);
#1064=CIRCLE('',#61993,1.05);
#1065=CIRCLE('',#61994,1.05);
#1066=CIRCLE('',#61999,4.50000000000305);
#1067=CIRCLE('',#62000,4.50000000000305);
#1068=CIRCLE('',#62002,3.375);
#1069=CIRCLE('',#62004,3.375);
#1070=CIRCLE('',#62005,3.375);
#1071=CIRCLE('',#62006,3.375);
#1072=CIRCLE('',#62007,3.375);
#1073=CIRCLE('',#62008,3.375);
#1074=CIRCLE('',#62009,3.375);
#1075=CIRCLE('',#62010,3.375);
#1076=CIRCLE('',#62011,3.375);
#1077=CIRCLE('',#62012,3.375);
#1078=CIRCLE('',#62013,3.375);
#1079=CIRCLE('',#62014,3.375);
#1080=CIRCLE('',#62015,3.375);
#1081=CIRCLE('',#62016,3.375);
#1082=CIRCLE('',#62017,3.375);
#1083=CIRCLE('',#62018,3.375);
#1084=CIRCLE('',#62019,3.375);
#1085=CIRCLE('',#62020,3.375);
#1086=CIRCLE('',#62021,3.375);
#1087=CIRCLE('',#62022,3.375);
#1088=CIRCLE('',#62023,3.375);
#1089=CIRCLE('',#62024,3.375);
#1090=CIRCLE('',#62025,3.375);
#1091=CIRCLE('',#62026,3.375);
#1092=CIRCLE('',#62027,3.375);
#1093=CIRCLE('',#62028,3.375);
#1094=CIRCLE('',#62029,3.375);
#1095=CIRCLE('',#62030,3.375);
#1096=CIRCLE('',#62031,3.375);
#1097=CIRCLE('',#62032,3.375);
#1098=CIRCLE('',#62033,3.375);
#1099=CIRCLE('',#62034,3.375);
#1100=CIRCLE('',#62035,3.375);
#1101=CIRCLE('',#62036,3.375);
#1102=CIRCLE('',#62040,4.50000000000305);
#1103=CIRCLE('',#62041,4.50000000000305);
#1104=CIRCLE('',#62046,4.50000000000305);
#1105=CIRCLE('',#62047,4.50000000000305);
#1106=CIRCLE('',#62052,4.50000000000305);
#1107=CIRCLE('',#62053,4.50000000000305);
#1108=CIRCLE('',#62058,4.50000000000305);
#1109=CIRCLE('',#62059,4.50000000000305);
#1110=CIRCLE('',#62064,4.50000000000305);
#1111=CIRCLE('',#62065,4.50000000000305);
#1112=CIRCLE('',#62070,4.50000000000305);
#1113=CIRCLE('',#62071,4.50000000000305);
#1114=CIRCLE('',#62076,4.50000000000305);
#1115=CIRCLE('',#62077,4.50000000000305);
#1116=CIRCLE('',#62082,4.50000000000305);
#1117=CIRCLE('',#62083,4.50000000000305);
#1118=CIRCLE('',#62088,4.50000000000305);
#1119=CIRCLE('',#62089,4.50000000000305);
#1120=CIRCLE('',#62094,4.50000000000305);
#1121=CIRCLE('',#62095,4.50000000000305);
#1122=CIRCLE('',#62100,4.50000000000305);
#1123=CIRCLE('',#62101,4.50000000000305);
#1124=CIRCLE('',#62106,4.50000000000305);
#1125=CIRCLE('',#62107,4.50000000000305);
#1126=CIRCLE('',#62112,4.50000000000305);
#1127=CIRCLE('',#62113,4.50000000000305);
#1128=CIRCLE('',#62118,4.50000000000305);
#1129=CIRCLE('',#62119,4.50000000000305);
#1130=CIRCLE('',#62123,4.50000000000305);
#1131=CIRCLE('',#62124,4.50000000000305);
#1132=CIRCLE('',#62128,2.5);
#1133=CIRCLE('',#62129,2.5);
#1134=CIRCLE('',#62132,4.49999999999999);
#1135=CIRCLE('',#62134,4.49999999999999);
#1136=CIRCLE('',#62136,4.2);
#1137=CIRCLE('',#62140,1.54999999999999);
#1138=CIRCLE('',#62141,1.54999999999999);
#1139=CIRCLE('',#62143,1.54999999999999);
#1140=CIRCLE('',#62148,10.);
#1141=CIRCLE('',#62149,10.);
#1142=CIRCLE('',#62150,10.);
#1143=CIRCLE('',#62151,10.);
#1144=CIRCLE('',#62152,10.);
#1145=CIRCLE('',#62153,10.);
#1146=CIRCLE('',#62154,10.);
#1147=CIRCLE('',#62155,10.);
#1148=CIRCLE('',#62156,10.);
#1149=CIRCLE('',#62157,10.);
#1150=CIRCLE('',#62158,10.);
#1151=CIRCLE('',#62159,10.);
#1152=CIRCLE('',#62160,10.);
#1153=CIRCLE('',#62161,10.);
#1154=CIRCLE('',#62162,10.);
#1155=CIRCLE('',#62163,10.);
#1156=CIRCLE('',#62164,10.);
#1157=CIRCLE('',#62165,10.);
#1158=CIRCLE('',#62166,10.);
#1159=CIRCLE('',#62167,9.2);
#1160=CIRCLE('',#62168,10.);
#1161=CIRCLE('',#62169,10.);
#1162=CIRCLE('',#62170,10.);
#1163=CIRCLE('',#62171,10.);
#1164=CIRCLE('',#62172,10.);
#1165=CIRCLE('',#62173,10.);
#1166=CIRCLE('',#62174,10.);
#1167=CIRCLE('',#62175,10.);
#1168=CIRCLE('',#62176,10.);
#1169=CIRCLE('',#62177,10.);
#1170=CIRCLE('',#62178,10.);
#1171=CIRCLE('',#62179,10.);
#1172=CIRCLE('',#62180,10.);
#1173=CIRCLE('',#62181,10.);
#1174=CIRCLE('',#62182,10.);
#1175=CIRCLE('',#62183,10.);
#1176=CIRCLE('',#62184,10.);
#1177=CIRCLE('',#62185,10.);
#1178=CIRCLE('',#62186,10.);
#1179=CIRCLE('',#62187,10.);
#1180=CIRCLE('',#62188,10.);
#1181=CIRCLE('',#62190,10.);
#1182=CIRCLE('',#62192,10.);
#1183=CIRCLE('',#62196,10.);
#1184=CIRCLE('',#62198,9.2);
#1185=CIRCLE('',#62199,10.);
#1186=CIRCLE('',#62200,10.);
#1187=CIRCLE('',#62201,10.);
#1188=CIRCLE('',#62202,10.);
#1189=CIRCLE('',#62203,10.);
#1190=CIRCLE('',#62204,10.);
#1191=CIRCLE('',#62205,10.);
#1192=CIRCLE('',#62206,10.);
#1193=CIRCLE('',#62207,10.);
#1194=CIRCLE('',#62208,10.);
#1195=CIRCLE('',#62209,10.);
#1196=CIRCLE('',#62210,10.);
#1197=CIRCLE('',#62211,10.);
#1198=CIRCLE('',#62212,10.);
#1199=CIRCLE('',#62213,10.);
#1200=CIRCLE('',#62214,10.);
#1201=CIRCLE('',#62215,10.);
#1202=CIRCLE('',#62216,10.);
#1203=CIRCLE('',#62217,10.);
#1204=CIRCLE('',#62218,10.);
#1205=CIRCLE('',#62219,10.);
#1206=CIRCLE('',#62220,10.);
#1207=CIRCLE('',#62221,10.);
#1208=CIRCLE('',#62222,10.);
#1209=CIRCLE('',#62223,10.);
#1210=CIRCLE('',#62224,10.);
#1211=CIRCLE('',#62225,10.);
#1212=CIRCLE('',#62226,10.);
#1213=CIRCLE('',#62227,10.);
#1214=CIRCLE('',#62228,10.);
#1215=CIRCLE('',#62229,10.);
#1216=CIRCLE('',#62230,10.);
#1217=CIRCLE('',#62231,10.);
#1218=CIRCLE('',#62232,10.);
#1219=CIRCLE('',#62233,10.);
#1220=CIRCLE('',#62234,10.);
#1221=CIRCLE('',#62235,10.);
#1222=CIRCLE('',#62349,2.51000000000001);
#1223=CIRCLE('',#62350,2.81000000000001);
#1224=CIRCLE('',#62352,3.70000000000001);
#1225=CIRCLE('',#62354,4.);
#1226=CIRCLE('',#62356,4.);
#1227=CIRCLE('',#62358,4.40000000000001);
#1228=CIRCLE('',#62360,6.);
#1229=CIRCLE('',#62362,6.);
#1230=CIRCLE('',#62364,6.40000000000001);
#1231=CIRCLE('',#62368,7.4);
#1232=CIRCLE('',#62370,6.99999999999999);
#1233=CIRCLE('',#62373,2.51000000000001);
#1234=CIRCLE('',#62377,2.51000000000001);
#1235=CIRCLE('',#62378,2.81000000000001);
#1236=CIRCLE('',#62380,4.49999999999999);
#1237=CIRCLE('',#62382,4.8);
#1238=CIRCLE('',#62384,4.8);
#1239=CIRCLE('',#62386,5.7);
#1240=CIRCLE('',#62388,6.);
#1241=CIRCLE('',#62390,6.);
#1242=CIRCLE('',#62392,2.81000000000001);
#1243=CIRCLE('',#62394,2.51000000000001);
#1244=CIRCLE('',#62398,2.80000000000001);
#1245=CIRCLE('',#62399,2.5);
#1246=CIRCLE('',#62401,2.5);
#1247=CIRCLE('',#62404,2.8);
#1248=CIRCLE('',#62405,2.5);
#1249=CIRCLE('',#62407,2.5);
#1250=CIRCLE('',#62410,1.45);
#1251=CIRCLE('',#62412,1.45);
#1252=CIRCLE('',#62414,1.45);
#1253=CIRCLE('',#62416,1.45);
#1254=CIRCLE('',#62925,0.5);
#1255=CIRCLE('',#62926,0.5);
#1256=CIRCLE('',#62928,5.);
#1257=CIRCLE('',#62929,5.);
#1258=CIRCLE('',#62931,0.5);
#1259=CIRCLE('',#62932,0.5);
#1260=CIRCLE('',#62935,0.5);
#1261=CIRCLE('',#62940,0.5);
#1262=CIRCLE('',#62941,0.5);
#1263=CIRCLE('',#62943,0.5);
#1264=CIRCLE('',#62944,2.15);
#1265=CIRCLE('',#62954,2.15);
#1266=CIRCLE('',#62993,1.9);
#1267=CIRCLE('',#63025,1.9);
#1268=CIRCLE('',#63027,2.);
#1269=CIRCLE('',#63029,1.99999999999999);
#1270=CIRCLE('',#63032,1.09999999999999);
#1271=CIRCLE('',#63033,1.09999999999999);
#1272=CIRCLE('',#63035,2.);
#1273=CIRCLE('',#63036,2.);
#1274=CIRCLE('',#63037,2.);
#1275=CIRCLE('',#63039,1.99999999999999);
#1276=CIRCLE('',#63041,0.800000000000001);
#1277=CIRCLE('',#63043,1.09999999999999);
#1278=CIRCLE('',#63044,1.09999999999999);
#1279=CIRCLE('',#63046,1.99999999999999);
#1280=CIRCLE('',#63047,1.99999999999999);
#1281=CIRCLE('',#63049,0.800000000000001);
#1282=CIRCLE('',#63051,0.800000000000001);
#1283=CIRCLE('',#63054,0.800000000000001);
#1284=CIRCLE('',#63060,1.954);
#1285=CIRCLE('',#63072,1.5555);
#1286=CIRCLE('',#63083,1.954);
#1287=CIRCLE('',#63084,1.954);
#1288=CIRCLE('',#63086,1.954);
#1289=CIRCLE('',#63087,1.5555);
#1290=CIRCLE('',#63088,1.954);
#1291=CIRCLE('',#63091,2.154);
#1292=CIRCLE('',#63092,0.2);
#1293=CIRCLE('',#63094,3.5);
#1294=CIRCLE('',#63096,1.954);
#1295=CIRCLE('',#63100,3.5);
#1296=CIRCLE('',#63101,3.5);
#1297=CIRCLE('',#63102,3.5);
#1298=CIRCLE('',#63104,3.5);
#1299=CIRCLE('',#63105,3.09999999999999);
#1300=CIRCLE('',#63107,3.09999999999999);
#1301=CIRCLE('',#63108,3.5);
#1302=CIRCLE('',#63113,1.5);
#1303=CIRCLE('',#63117,1.4635);
#1304=CIRCLE('',#63123,1.17775);
#1305=CIRCLE('',#63128,1.4635);
#1306=CIRCLE('',#63129,1.4635);
#1307=CIRCLE('',#63131,1.4635);
#1308=CIRCLE('',#63132,1.4635);
#1309=CIRCLE('',#63133,1.17775);
#1310=CIRCLE('',#63136,1.01602540378444);
#1311=CIRCLE('',#63137,0.816025403784444);
#1312=CIRCLE('',#63138,0.816025403784444);
#1313=CIRCLE('',#63139,0.816025403784444);
#1314=CIRCLE('',#63140,0.816025403784444);
#1315=CIRCLE('',#63141,0.816025403784444);
#1316=CIRCLE('',#63142,0.816025403784444);
#1317=CIRCLE('',#63144,0.816025403784444);
#1318=CIRCLE('',#63146,0.816025403784444);
#1319=CIRCLE('',#63148,0.816025403784444);
#1320=CIRCLE('',#63150,0.816025403784444);
#1321=CIRCLE('',#63152,0.816025403784444);
#1322=CIRCLE('',#63154,0.816025403784444);
#1323=CIRCLE('',#63165,0.866025403784434);
#1324=CIRCLE('',#63167,0.866025403784434);
#1325=CIRCLE('',#63169,0.866025403784434);
#1326=CIRCLE('',#63171,0.866025403784434);
#1327=CIRCLE('',#63173,0.866025403784434);
#1328=CIRCLE('',#63175,0.866025403784434);
#1329=CIRCLE('',#63181,1.20000000000001);
#1330=CIRCLE('',#63184,1.4635);
#1331=CIRCLE('',#63186,0.999999999999996);
#1332=CIRCLE('',#63190,0.96675);
#1333=CIRCLE('',#63194,0.96675);
#1334=CIRCLE('',#63196,0.739000000000001);
#1335=CIRCLE('',#63200,0.96675);
#1336=CIRCLE('',#63202,0.96675);
#1337=CIRCLE('',#63203,0.96675);
#1338=CIRCLE('',#63204,0.739000000000001);
#1339=CIRCLE('',#63207,0.669615242270665);
#1340=CIRCLE('',#63208,0.469615242270667);
#1341=CIRCLE('',#63209,0.469615242270667);
#1342=CIRCLE('',#63210,0.469615242270667);
#1343=CIRCLE('',#63211,0.469615242270667);
#1344=CIRCLE('',#63212,0.469615242270667);
#1345=CIRCLE('',#63213,0.469615242270667);
#1346=CIRCLE('',#63215,0.469615242270667);
#1347=CIRCLE('',#63217,0.469615242270667);
#1348=CIRCLE('',#63219,0.469615242270667);
#1349=CIRCLE('',#63221,0.469615242270667);
#1350=CIRCLE('',#63223,0.469615242270667);
#1351=CIRCLE('',#63225,0.469615242270667);
#1352=CIRCLE('',#63236,0.519615242270657);
#1353=CIRCLE('',#63238,0.519615242270657);
#1354=CIRCLE('',#63240,0.519615242270657);
#1355=CIRCLE('',#63242,0.519615242270657);
#1356=CIRCLE('',#63244,0.519615242270657);
#1357=CIRCLE('',#63246,0.519615242270657);
#1358=CIRCLE('',#63252,0.760000000000005);
#1359=CIRCLE('',#63255,0.96675);
#1360=CIRCLE('',#63257,0.500000000000007);
#1361=CIRCLE('',#63261,1.4635);
#1362=CIRCLE('',#63273,1.17775);
#1363=CIRCLE('',#63284,1.4635);
#1364=CIRCLE('',#63285,1.4635);
#1365=CIRCLE('',#63287,1.4635);
#1366=CIRCLE('',#63288,1.4635);
#1367=CIRCLE('',#63289,1.17775);
#1368=CIRCLE('',#63292,1.01602540378443);
#1369=CIRCLE('',#63293,0.816025403784426);
#1370=CIRCLE('',#63294,0.816025403784426);
#1371=CIRCLE('',#63295,0.816025403784426);
#1372=CIRCLE('',#63296,0.816025403784426);
#1373=CIRCLE('',#63297,0.816025403784426);
#1374=CIRCLE('',#63298,0.816025403784426);
#1375=CIRCLE('',#63300,0.816025403784426);
#1376=CIRCLE('',#63302,0.816025403784426);
#1377=CIRCLE('',#63304,0.816025403784426);
#1378=CIRCLE('',#63306,0.816025403784426);
#1379=CIRCLE('',#63308,0.816025403784426);
#1380=CIRCLE('',#63310,0.816025403784426);
#1381=CIRCLE('',#63321,0.866025403784434);
#1382=CIRCLE('',#63323,0.866025403784434);
#1383=CIRCLE('',#63325,0.866025403784434);
#1384=CIRCLE('',#63327,0.866025403784434);
#1385=CIRCLE('',#63329,0.866025403784434);
#1386=CIRCLE('',#63331,0.866025403784434);
#1387=CIRCLE('',#63337,1.19999999999999);
#1388=CIRCLE('',#63340,1.4635);
#1389=CIRCLE('',#63342,0.999999999999996);
#1390=CIRCLE('',#63346,0.96675);
#1391=CIRCLE('',#63353,0.739000000000001);
#1392=CIRCLE('',#63355,0.739000000000001);
#1393=CIRCLE('',#63361,0.96675);
#1394=CIRCLE('',#63362,0.96675);
#1395=CIRCLE('',#63364,0.96675);
#1396=CIRCLE('',#63365,0.96675);
#1397=CIRCLE('',#63366,0.739000000000001);
#1398=CIRCLE('',#63369,0.669615242270665);
#1399=CIRCLE('',#63370,0.469615242270667);
#1400=CIRCLE('',#63371,0.469615242270667);
#1401=CIRCLE('',#63372,0.469615242270667);
#1402=CIRCLE('',#63373,0.469615242270667);
#1403=CIRCLE('',#63374,0.469615242270667);
#1404=CIRCLE('',#63375,0.469615242270667);
#1405=CIRCLE('',#63377,0.469615242270667);
#1406=CIRCLE('',#63379,0.469615242270667);
#1407=CIRCLE('',#63381,0.469615242270667);
#1408=CIRCLE('',#63383,0.469615242270667);
#1409=CIRCLE('',#63385,0.469615242270667);
#1410=CIRCLE('',#63387,0.469615242270667);
#1411=CIRCLE('',#63398,0.519615242270657);
#1412=CIRCLE('',#63400,0.519615242270657);
#1413=CIRCLE('',#63402,0.519615242270657);
#1414=CIRCLE('',#63404,0.519615242270657);
#1415=CIRCLE('',#63406,0.519615242270657);
#1416=CIRCLE('',#63408,0.519615242270657);
#1417=CIRCLE('',#63414,0.760000000000005);
#1418=CIRCLE('',#63417,0.96675);
#1419=CIRCLE('',#63419,0.500000000000007);
#1420=CIRCLE('',#63423,0.96675);
#1421=CIRCLE('',#63431,0.96675);
#1422=CIRCLE('',#63433,0.739000000000001);
#1423=CIRCLE('',#63441,0.96675);
#1424=CIRCLE('',#63443,0.96675);
#1425=CIRCLE('',#63444,0.96675);
#1426=CIRCLE('',#63445,0.739000000000001);
#1427=CIRCLE('',#63455,0.800000000000001);
#1428=CIRCLE('',#63458,0.96675);
#1429=CIRCLE('',#63460,1.9);
#1430=CIRCLE('',#63464,1.215);
#1431=CIRCLE('',#63478,0.958249999999999);
#1432=CIRCLE('',#63491,1.215);
#1433=CIRCLE('',#63492,1.215);
#1434=CIRCLE('',#63494,1.215);
#1435=CIRCLE('',#63495,0.958249999999999);
#1436=CIRCLE('',#63496,1.215);
#1437=CIRCLE('',#63499,0.1);
#1438=CIRCLE('',#63500,1.315);
#1439=CIRCLE('',#63502,1.215);
#1440=CIRCLE('',#63504,2.05);
#1441=CIRCLE('',#63506,0.865);
#1442=CIRCLE('',#63510,2.25);
#1443=CIRCLE('',#63513,2.25);
#1444=CIRCLE('',#63514,2.25);
#1445=CIRCLE('',#63515,2.25);
#1446=CIRCLE('',#63516,2.25);
#1447=CIRCLE('',#63517,2.25);
#1448=CIRCLE('',#63518,2.25);
#1449=CIRCLE('',#63519,2.25);
#1450=CIRCLE('',#63520,2.25);
#1451=CIRCLE('',#63521,2.25);
#1452=CIRCLE('',#63522,2.25);
#1453=CIRCLE('',#63523,2.25);
#1454=CIRCLE('',#63524,2.25);
#1455=CIRCLE('',#63525,2.25);
#1456=CIRCLE('',#63526,2.25);
#1457=CIRCLE('',#63527,2.25);
#1458=CIRCLE('',#63528,2.25);
#1459=CIRCLE('',#63529,2.25);
#1460=CIRCLE('',#63530,2.25);
#1461=CIRCLE('',#63531,2.25);
#1462=CIRCLE('',#63532,2.25);
#1463=CIRCLE('',#63533,2.25);
#1464=CIRCLE('',#63534,2.25);
#1465=CIRCLE('',#63535,2.25);
#1466=CIRCLE('',#63536,2.25);
#1467=CIRCLE('',#63537,2.25);
#1468=CIRCLE('',#63538,2.25);
#1469=CIRCLE('',#63539,2.25);
#1470=CIRCLE('',#63540,2.25);
#1471=CIRCLE('',#63541,2.25);
#1472=CIRCLE('',#63542,2.25);
#1473=CIRCLE('',#63543,2.25);
#1474=CIRCLE('',#63544,2.25);
#1475=CIRCLE('',#63545,2.25);
#1476=CIRCLE('',#63546,2.25);
#1477=CIRCLE('',#63547,2.25);
#1478=CIRCLE('',#63548,2.25);
#1479=CIRCLE('',#63549,2.25);
#1480=CIRCLE('',#63550,2.25);
#1481=CIRCLE('',#63551,2.25);
#1482=CIRCLE('',#63552,2.25);
#1483=CIRCLE('',#63553,2.25);
#1484=CIRCLE('',#63554,2.25);
#1485=CIRCLE('',#63555,2.25);
#1486=CIRCLE('',#63556,2.25);
#1487=CIRCLE('',#63557,2.25);
#1488=CIRCLE('',#63558,2.25);
#1489=CIRCLE('',#63559,2.25);
#1490=CIRCLE('',#63560,2.25);
#1491=CIRCLE('',#63561,2.25);
#1492=CIRCLE('',#63562,2.25);
#1493=CIRCLE('',#63563,2.25);
#1494=CIRCLE('',#63564,2.25);
#1495=CIRCLE('',#63565,2.25);
#1496=CIRCLE('',#63566,2.25);
#1497=CIRCLE('',#63567,2.25);
#1498=CIRCLE('',#63568,2.25);
#1499=CIRCLE('',#63569,2.25);
#1500=CIRCLE('',#63570,2.25);
#1501=CIRCLE('',#63571,2.25);
#1502=CIRCLE('',#63572,2.25);
#1503=CIRCLE('',#63573,2.25);
#1504=CIRCLE('',#63574,2.25);
#1505=CIRCLE('',#63575,2.25);
#1506=CIRCLE('',#63576,2.25);
#1507=CIRCLE('',#63577,2.25);
#1508=CIRCLE('',#63578,2.25);
#1509=CIRCLE('',#63579,2.25);
#1510=CIRCLE('',#63580,2.25);
#1511=CIRCLE('',#63581,2.25);
#1512=CIRCLE('',#63582,2.25);
#1513=CIRCLE('',#63583,2.25);
#1514=CIRCLE('',#63584,2.25);
#1515=CIRCLE('',#63585,2.25);
#1516=CIRCLE('',#63586,2.25);
#1517=CIRCLE('',#63693,0.2);
#1518=CIRCLE('',#63695,1.95);
#1519=CIRCLE('',#63697,1.30470053837925);
#1520=CIRCLE('',#63699,1.10470053837925);
#1521=CIRCLE('',#63700,1.10470053837925);
#1522=CIRCLE('',#63701,1.10470053837925);
#1523=CIRCLE('',#63702,1.10470053837925);
#1524=CIRCLE('',#63703,1.10470053837925);
#1525=CIRCLE('',#63704,1.10470053837925);
#1526=CIRCLE('',#63706,1.10470053837925);
#1527=CIRCLE('',#63708,1.10470053837925);
#1528=CIRCLE('',#63710,1.10470053837925);
#1529=CIRCLE('',#63712,1.10470053837925);
#1530=CIRCLE('',#63714,1.10470053837925);
#1531=CIRCLE('',#63716,1.10470053837925);
#1532=CIRCLE('',#63727,1.15470053837925);
#1533=CIRCLE('',#63729,1.15470053837925);
#1534=CIRCLE('',#63731,1.15470053837925);
#1535=CIRCLE('',#63733,1.15470053837925);
#1536=CIRCLE('',#63735,1.15470053837925);
#1537=CIRCLE('',#63737,1.15470053837925);
#1538=CIRCLE('',#63744,0.7);
#1539=CIRCLE('',#63746,1.);
#1540=CIRCLE('',#63748,1.);
#1541=CIRCLE('',#63750,0.7);
#1542=FACE_BOUND('',#7313,.T.);
#1543=FACE_BOUND('',#7345,.T.);
#1544=FACE_BOUND('',#7369,.T.);
#1545=FACE_BOUND('',#7404,.T.);
#1546=FACE_BOUND('',#7405,.T.);
#1547=FACE_BOUND('',#7430,.T.);
#1548=FACE_BOUND('',#7465,.T.);
#1549=FACE_BOUND('',#7495,.T.);
#1550=FACE_BOUND('',#7519,.T.);
#1551=FACE_BOUND('',#7565,.T.);
#1552=FACE_BOUND('',#7581,.T.);
#1553=FACE_BOUND('',#7605,.T.);
#1554=FACE_BOUND('',#7659,.T.);
#1555=FACE_BOUND('',#7705,.T.);
#1556=FACE_BOUND('',#7738,.T.);
#1557=FACE_BOUND('',#7761,.T.);
#1558=FACE_BOUND('',#7794,.T.);
#1559=FACE_BOUND('',#7840,.T.);
#1560=FACE_BOUND('',#7894,.T.);
#1561=FACE_BOUND('',#7910,.T.);
#1562=FACE_BOUND('',#7934,.T.);
#1563=FACE_BOUND('',#7980,.T.);
#1564=FACE_BOUND('',#8010,.T.);
#1565=FACE_BOUND('',#8034,.T.);
#1566=FACE_BOUND('',#8069,.T.);
#1567=FACE_BOUND('',#8104,.T.);
#1568=FACE_BOUND('',#8105,.T.);
#1569=FACE_BOUND('',#8130,.T.);
#1570=FACE_BOUND('',#8162,.T.);
#1571=FACE_BOUND('',#9078,.T.);
#1572=FACE_BOUND('',#9079,.T.);
#1573=FACE_BOUND('',#9080,.T.);
#1574=FACE_BOUND('',#9088,.T.);
#1575=FACE_BOUND('',#9089,.T.);
#1576=FACE_BOUND('',#9096,.T.);
#1577=FACE_BOUND('',#9099,.T.);
#1578=FACE_BOUND('',#9102,.T.);
#1579=FACE_BOUND('',#9105,.T.);
#1580=FACE_BOUND('',#9108,.T.);
#1581=FACE_BOUND('',#9111,.T.);
#1582=FACE_BOUND('',#9114,.T.);
#1583=FACE_BOUND('',#9115,.T.);
#1584=FACE_BOUND('',#9116,.T.);
#1585=FACE_BOUND('',#9152,.T.);
#1586=FACE_BOUND('',#9153,.T.);
#1587=FACE_BOUND('',#9154,.T.);
#1588=FACE_BOUND('',#9155,.T.);
#1589=FACE_BOUND('',#9161,.T.);
#1590=FACE_BOUND('',#9162,.T.);
#1591=FACE_BOUND('',#9163,.T.);
#1592=FACE_BOUND('',#9164,.T.);
#1593=FACE_BOUND('',#9165,.T.);
#1594=FACE_BOUND('',#9166,.T.);
#1595=FACE_BOUND('',#9167,.T.);
#1596=FACE_BOUND('',#9168,.T.);
#1597=FACE_BOUND('',#9169,.T.);
#1598=FACE_BOUND('',#9170,.T.);
#1599=FACE_BOUND('',#9171,.T.);
#1600=FACE_BOUND('',#9172,.T.);
#1601=FACE_BOUND('',#9173,.T.);
#1602=FACE_BOUND('',#9174,.T.);
#1603=FACE_BOUND('',#9175,.T.);
#1604=FACE_BOUND('',#9176,.T.);
#1605=FACE_BOUND('',#9177,.T.);
#1606=FACE_BOUND('',#9178,.T.);
#1607=FACE_BOUND('',#9179,.T.);
#1608=FACE_BOUND('',#9180,.T.);
#1609=FACE_BOUND('',#9181,.T.);
#1610=FACE_BOUND('',#9182,.T.);
#1611=FACE_BOUND('',#9183,.T.);
#1612=FACE_BOUND('',#9184,.T.);
#1613=FACE_BOUND('',#9185,.T.);
#1614=FACE_BOUND('',#9186,.T.);
#1615=FACE_BOUND('',#9187,.T.);
#1616=FACE_BOUND('',#9188,.T.);
#1617=FACE_BOUND('',#9189,.T.);
#1618=FACE_BOUND('',#9190,.T.);
#1619=FACE_BOUND('',#9191,.T.);
#1620=FACE_BOUND('',#9192,.T.);
#1621=FACE_BOUND('',#9193,.T.);
#1622=FACE_BOUND('',#9194,.T.);
#1623=FACE_BOUND('',#9195,.T.);
#1624=FACE_BOUND('',#9196,.T.);
#1625=FACE_BOUND('',#9197,.T.);
#1626=FACE_BOUND('',#9198,.T.);
#1627=FACE_BOUND('',#9199,.T.);
#1628=FACE_BOUND('',#9200,.T.);
#1629=FACE_BOUND('',#9201,.T.);
#1630=FACE_BOUND('',#9202,.T.);
#1631=FACE_BOUND('',#9203,.T.);
#1632=FACE_BOUND('',#9204,.T.);
#1633=FACE_BOUND('',#9205,.T.);
#1634=FACE_BOUND('',#9206,.T.);
#1635=FACE_BOUND('',#9207,.T.);
#1636=FACE_BOUND('',#9208,.T.);
#1637=FACE_BOUND('',#9209,.T.);
#1638=FACE_BOUND('',#9210,.T.);
#1639=FACE_BOUND('',#9211,.T.);
#1640=FACE_BOUND('',#9212,.T.);
#1641=FACE_BOUND('',#9213,.T.);
#1642=FACE_BOUND('',#9214,.T.);
#1643=FACE_BOUND('',#9215,.T.);
#1644=FACE_BOUND('',#9216,.T.);
#1645=FACE_BOUND('',#9217,.T.);
#1646=FACE_BOUND('',#9218,.T.);
#1647=FACE_BOUND('',#9219,.T.);
#1648=FACE_BOUND('',#9220,.T.);
#1649=FACE_BOUND('',#9221,.T.);
#1650=FACE_BOUND('',#9222,.T.);
#1651=FACE_BOUND('',#9223,.T.);
#1652=FACE_BOUND('',#9224,.T.);
#1653=FACE_BOUND('',#9225,.T.);
#1654=FACE_BOUND('',#9226,.T.);
#1655=FACE_BOUND('',#9227,.T.);
#1656=FACE_BOUND('',#9228,.T.);
#1657=FACE_BOUND('',#9229,.T.);
#1658=FACE_BOUND('',#9230,.T.);
#1659=FACE_BOUND('',#9231,.T.);
#1660=FACE_BOUND('',#9232,.T.);
#1661=FACE_BOUND('',#9233,.T.);
#1662=FACE_BOUND('',#9234,.T.);
#1663=FACE_BOUND('',#9235,.T.);
#1664=FACE_BOUND('',#9236,.T.);
#1665=FACE_BOUND('',#9237,.T.);
#1666=FACE_BOUND('',#9238,.T.);
#1667=FACE_BOUND('',#9239,.T.);
#1668=FACE_BOUND('',#9240,.T.);
#1669=FACE_BOUND('',#9241,.T.);
#1670=FACE_BOUND('',#9242,.T.);
#1671=FACE_BOUND('',#9243,.T.);
#1672=FACE_BOUND('',#9244,.T.);
#1673=FACE_BOUND('',#9245,.T.);
#1674=FACE_BOUND('',#9246,.T.);
#1675=FACE_BOUND('',#9247,.T.);
#1676=FACE_BOUND('',#9248,.T.);
#1677=FACE_BOUND('',#9249,.T.);
#1678=FACE_BOUND('',#9250,.T.);
#1679=FACE_BOUND('',#9251,.T.);
#1680=FACE_BOUND('',#9252,.T.);
#1681=FACE_BOUND('',#9253,.T.);
#1682=FACE_BOUND('',#9254,.T.);
#1683=FACE_BOUND('',#9255,.T.);
#1684=FACE_BOUND('',#9256,.T.);
#1685=FACE_BOUND('',#9257,.T.);
#1686=FACE_BOUND('',#9258,.T.);
#1687=FACE_BOUND('',#9259,.T.);
#1688=FACE_BOUND('',#9260,.T.);
#1689=FACE_BOUND('',#9261,.T.);
#1690=FACE_BOUND('',#9262,.T.);
#1691=FACE_BOUND('',#9263,.T.);
#1692=FACE_BOUND('',#9264,.T.);
#1693=FACE_BOUND('',#9265,.T.);
#1694=FACE_BOUND('',#9266,.T.);
#1695=FACE_BOUND('',#9267,.T.);
#1696=FACE_BOUND('',#9268,.T.);
#1697=FACE_BOUND('',#9269,.T.);
#1698=FACE_BOUND('',#9270,.T.);
#1699=FACE_BOUND('',#9271,.T.);
#1700=FACE_BOUND('',#9272,.T.);
#1701=FACE_BOUND('',#9273,.T.);
#1702=FACE_BOUND('',#9274,.T.);
#1703=FACE_BOUND('',#9275,.T.);
#1704=FACE_BOUND('',#9276,.T.);
#1705=FACE_BOUND('',#9277,.T.);
#1706=FACE_BOUND('',#9278,.T.);
#1707=FACE_BOUND('',#9279,.T.);
#1708=FACE_BOUND('',#9280,.T.);
#1709=FACE_BOUND('',#9281,.T.);
#1710=FACE_BOUND('',#9282,.T.);
#1711=FACE_BOUND('',#9283,.T.);
#1712=FACE_BOUND('',#9284,.T.);
#1713=FACE_BOUND('',#9285,.T.);
#1714=FACE_BOUND('',#9286,.T.);
#1715=FACE_BOUND('',#9287,.T.);
#1716=FACE_BOUND('',#9288,.T.);
#1717=FACE_BOUND('',#9289,.T.);
#1718=FACE_BOUND('',#9290,.T.);
#1719=FACE_BOUND('',#9291,.T.);
#1720=FACE_BOUND('',#9292,.T.);
#1721=FACE_BOUND('',#9293,.T.);
#1722=FACE_BOUND('',#9294,.T.);
#1723=FACE_BOUND('',#9295,.T.);
#1724=FACE_BOUND('',#9296,.T.);
#1725=FACE_BOUND('',#9297,.T.);
#1726=FACE_BOUND('',#9298,.T.);
#1727=FACE_BOUND('',#9299,.T.);
#1728=FACE_BOUND('',#9300,.T.);
#1729=FACE_BOUND('',#9301,.T.);
#1730=FACE_BOUND('',#9302,.T.);
#1731=FACE_BOUND('',#9303,.T.);
#1732=FACE_BOUND('',#9304,.T.);
#1733=FACE_BOUND('',#9305,.T.);
#1734=FACE_BOUND('',#9306,.T.);
#1735=FACE_BOUND('',#9307,.T.);
#1736=FACE_BOUND('',#9308,.T.);
#1737=FACE_BOUND('',#9309,.T.);
#1738=FACE_BOUND('',#9310,.T.);
#1739=FACE_BOUND('',#9311,.T.);
#1740=FACE_BOUND('',#9312,.T.);
#1741=FACE_BOUND('',#9313,.T.);
#1742=FACE_BOUND('',#9314,.T.);
#1743=FACE_BOUND('',#9315,.T.);
#1744=FACE_BOUND('',#9316,.T.);
#1745=FACE_BOUND('',#9317,.T.);
#1746=FACE_BOUND('',#9318,.T.);
#1747=FACE_BOUND('',#9319,.T.);
#1748=FACE_BOUND('',#9320,.T.);
#1749=FACE_BOUND('',#9321,.T.);
#1750=FACE_BOUND('',#9322,.T.);
#1751=FACE_BOUND('',#9323,.T.);
#1752=FACE_BOUND('',#9324,.T.);
#1753=FACE_BOUND('',#9325,.T.);
#1754=FACE_BOUND('',#9326,.T.);
#1755=FACE_BOUND('',#9327,.T.);
#1756=FACE_BOUND('',#9328,.T.);
#1757=FACE_BOUND('',#9329,.T.);
#1758=FACE_BOUND('',#9330,.T.);
#1759=FACE_BOUND('',#9331,.T.);
#1760=FACE_BOUND('',#9332,.T.);
#1761=FACE_BOUND('',#9333,.T.);
#1762=FACE_BOUND('',#9334,.T.);
#1763=FACE_BOUND('',#9335,.T.);
#1764=FACE_BOUND('',#9336,.T.);
#1765=FACE_BOUND('',#9337,.T.);
#1766=FACE_BOUND('',#9338,.T.);
#1767=FACE_BOUND('',#9339,.T.);
#1768=FACE_BOUND('',#9340,.T.);
#1769=FACE_BOUND('',#9341,.T.);
#1770=FACE_BOUND('',#9342,.T.);
#1771=FACE_BOUND('',#9343,.T.);
#1772=FACE_BOUND('',#9344,.T.);
#1773=FACE_BOUND('',#9345,.T.);
#1774=FACE_BOUND('',#9346,.T.);
#1775=FACE_BOUND('',#9347,.T.);
#1776=FACE_BOUND('',#9348,.T.);
#1777=FACE_BOUND('',#9349,.T.);
#1778=FACE_BOUND('',#9350,.T.);
#1779=FACE_BOUND('',#9351,.T.);
#1780=FACE_BOUND('',#9352,.T.);
#1781=FACE_BOUND('',#9353,.T.);
#1782=FACE_BOUND('',#9354,.T.);
#1783=FACE_BOUND('',#9355,.T.);
#1784=FACE_BOUND('',#9356,.T.);
#1785=FACE_BOUND('',#9357,.T.);
#1786=FACE_BOUND('',#9358,.T.);
#1787=FACE_BOUND('',#9359,.T.);
#1788=FACE_BOUND('',#9360,.T.);
#1789=FACE_BOUND('',#9361,.T.);
#1790=FACE_BOUND('',#9362,.T.);
#1791=FACE_BOUND('',#9363,.T.);
#1792=FACE_BOUND('',#9364,.T.);
#1793=FACE_BOUND('',#9365,.T.);
#1794=FACE_BOUND('',#9366,.T.);
#1795=FACE_BOUND('',#9367,.T.);
#1796=FACE_BOUND('',#9368,.T.);
#1797=FACE_BOUND('',#9369,.T.);
#1798=FACE_BOUND('',#9370,.T.);
#1799=FACE_BOUND('',#9371,.T.);
#1800=FACE_BOUND('',#9372,.T.);
#1801=FACE_BOUND('',#9373,.T.);
#1802=FACE_BOUND('',#9374,.T.);
#1803=FACE_BOUND('',#9375,.T.);
#1804=FACE_BOUND('',#9376,.T.);
#1805=FACE_BOUND('',#9377,.T.);
#1806=FACE_BOUND('',#9378,.T.);
#1807=FACE_BOUND('',#9381,.T.);
#1808=FACE_BOUND('',#9382,.T.);
#1809=FACE_BOUND('',#9383,.T.);
#1810=FACE_BOUND('',#9384,.T.);
#1811=FACE_BOUND('',#9411,.T.);
#1812=FACE_BOUND('',#9430,.T.);
#1813=FACE_BOUND('',#9431,.T.);
#1814=FACE_BOUND('',#9432,.T.);
#1815=FACE_BOUND('',#9433,.T.);
#1816=FACE_BOUND('',#9434,.T.);
#1817=FACE_BOUND('',#9435,.T.);
#1818=FACE_BOUND('',#9462,.T.);
#1819=FACE_BOUND('',#9470,.T.);
#1820=FACE_BOUND('',#9471,.T.);
#1821=FACE_BOUND('',#9472,.T.);
#1822=FACE_BOUND('',#9512,.T.);
#1823=FACE_BOUND('',#9513,.T.);
#1824=FACE_BOUND('',#9514,.T.);
#1825=FACE_BOUND('',#9526,.T.);
#1826=FACE_BOUND('',#9527,.T.);
#1827=FACE_BOUND('',#9631,.T.);
#1828=FACE_BOUND('',#9633,.T.);
#1829=FACE_BOUND('',#9635,.T.);
#1830=FACE_BOUND('',#9637,.T.);
#1831=FACE_BOUND('',#9640,.T.);
#1832=FACE_BOUND('',#9767,.T.);
#1833=FACE_BOUND('',#9772,.T.);
#1834=FACE_BOUND('',#9774,.T.);
#1835=FACE_BOUND('',#9777,.T.);
#1836=FACE_BOUND('',#9780,.T.);
#1837=FACE_BOUND('',#9785,.T.);
#1838=FACE_BOUND('',#9788,.T.);
#1839=FACE_BOUND('',#9792,.T.);
#1840=FACE_BOUND('',#9796,.T.);
#1841=FACE_BOUND('',#9802,.T.);
#1842=FACE_BOUND('',#9806,.T.);
#1843=FACE_BOUND('',#9808,.T.);
#1844=FACE_BOUND('',#9810,.T.);
#1845=FACE_BOUND('',#9816,.T.);
#1846=FACE_BOUND('',#9817,.T.);
#1847=FACE_BOUND('',#10330,.T.);
#1848=FACE_BOUND('',#10341,.T.);
#1849=FACE_BOUND('',#10424,.T.);
#1850=FACE_BOUND('',#10425,.T.);
#1851=FACE_BOUND('',#10454,.T.);
#1852=FACE_BOUND('',#10507,.T.);
#1853=FACE_BOUND('',#10551,.T.);
#1854=FACE_BOUND('',#10609,.T.);
#1855=FACE_BOUND('',#10658,.T.);
#1856=FACE_BOUND('',#10695,.T.);
#1857=FACE_BOUND('',#10729,.T.);
#1858=FACE_BOUND('',#10844,.T.);
#1859=PLANE('',#60611);
#1860=PLANE('',#60612);
#1861=PLANE('',#60613);
#1862=PLANE('',#60614);
#1863=PLANE('',#60615);
#1864=PLANE('',#60616);
#1865=PLANE('',#60617);
#1866=PLANE('',#60618);
#1867=PLANE('',#60619);
#1868=PLANE('',#60620);
#1869=PLANE('',#60621);
#1870=PLANE('',#60622);
#1871=PLANE('',#60623);
#1872=PLANE('',#60624);
#1873=PLANE('',#60625);
#1874=PLANE('',#60626);
#1875=PLANE('',#60627);
#1876=PLANE('',#60628);
#1877=PLANE('',#60629);
#1878=PLANE('',#60630);
#1879=PLANE('',#60631);
#1880=PLANE('',#60632);
#1881=PLANE('',#60633);
#1882=PLANE('',#60634);
#1883=PLANE('',#60635);
#1884=PLANE('',#60636);
#1885=PLANE('',#60637);
#1886=PLANE('',#60638);
#1887=PLANE('',#60639);
#1888=PLANE('',#60640);
#1889=PLANE('',#60641);
#1890=PLANE('',#60642);
#1891=PLANE('',#60643);
#1892=PLANE('',#60644);
#1893=PLANE('',#60645);
#1894=PLANE('',#60646);
#1895=PLANE('',#60647);
#1896=PLANE('',#60648);
#1897=PLANE('',#60649);
#1898=PLANE('',#60650);
#1899=PLANE('',#60651);
#1900=PLANE('',#60652);
#1901=PLANE('',#60653);
#1902=PLANE('',#60654);
#1903=PLANE('',#60655);
#1904=PLANE('',#60656);
#1905=PLANE('',#60657);
#1906=PLANE('',#60658);
#1907=PLANE('',#60659);
#1908=PLANE('',#60660);
#1909=PLANE('',#60661);
#1910=PLANE('',#60662);
#1911=PLANE('',#60663);
#1912=PLANE('',#60664);
#1913=PLANE('',#60665);
#1914=PLANE('',#60666);
#1915=PLANE('',#60667);
#1916=PLANE('',#60668);
#1917=PLANE('',#60669);
#1918=PLANE('',#60670);
#1919=PLANE('',#60671);
#1920=PLANE('',#60672);
#1921=PLANE('',#60673);
#1922=PLANE('',#60674);
#1923=PLANE('',#60675);
#1924=PLANE('',#60676);
#1925=PLANE('',#60677);
#1926=PLANE('',#60678);
#1927=PLANE('',#60679);
#1928=PLANE('',#60680);
#1929=PLANE('',#60681);
#1930=PLANE('',#60682);
#1931=PLANE('',#60683);
#1932=PLANE('',#60684);
#1933=PLANE('',#60685);
#1934=PLANE('',#60686);
#1935=PLANE('',#60687);
#1936=PLANE('',#60688);
#1937=PLANE('',#60689);
#1938=PLANE('',#60690);
#1939=PLANE('',#60691);
#1940=PLANE('',#60692);
#1941=PLANE('',#60693);
#1942=PLANE('',#60694);
#1943=PLANE('',#60695);
#1944=PLANE('',#60696);
#1945=PLANE('',#60697);
#1946=PLANE('',#60698);
#1947=PLANE('',#60699);
#1948=PLANE('',#60700);
#1949=PLANE('',#60701);
#1950=PLANE('',#60702);
#1951=PLANE('',#60703);
#1952=PLANE('',#60704);
#1953=PLANE('',#60705);
#1954=PLANE('',#60706);
#1955=PLANE('',#60707);
#1956=PLANE('',#60708);
#1957=PLANE('',#60709);
#1958=PLANE('',#60710);
#1959=PLANE('',#60711);
#1960=PLANE('',#60712);
#1961=PLANE('',#60713);
#1962=PLANE('',#60714);
#1963=PLANE('',#60715);
#1964=PLANE('',#60716);
#1965=PLANE('',#60717);
#1966=PLANE('',#60718);
#1967=PLANE('',#60719);
#1968=PLANE('',#60720);
#1969=PLANE('',#60721);
#1970=PLANE('',#60722);
#1971=PLANE('',#60723);
#1972=PLANE('',#60724);
#1973=PLANE('',#60725);
#1974=PLANE('',#60726);
#1975=PLANE('',#60727);
#1976=PLANE('',#60728);
#1977=PLANE('',#60729);
#1978=PLANE('',#60730);
#1979=PLANE('',#60731);
#1980=PLANE('',#60732);
#1981=PLANE('',#60733);
#1982=PLANE('',#60734);
#1983=PLANE('',#60735);
#1984=PLANE('',#60736);
#1985=PLANE('',#60737);
#1986=PLANE('',#60738);
#1987=PLANE('',#60739);
#1988=PLANE('',#60740);
#1989=PLANE('',#60741);
#1990=PLANE('',#60742);
#1991=PLANE('',#60743);
#1992=PLANE('',#60744);
#1993=PLANE('',#60745);
#1994=PLANE('',#60746);
#1995=PLANE('',#60747);
#1996=PLANE('',#60748);
#1997=PLANE('',#60749);
#1998=PLANE('',#60750);
#1999=PLANE('',#60751);
#2000=PLANE('',#60752);
#2001=PLANE('',#60753);
#2002=PLANE('',#60754);
#2003=PLANE('',#60755);
#2004=PLANE('',#60756);
#2005=PLANE('',#60757);
#2006=PLANE('',#60758);
#2007=PLANE('',#60759);
#2008=PLANE('',#60760);
#2009=PLANE('',#60761);
#2010=PLANE('',#60762);
#2011=PLANE('',#60763);
#2012=PLANE('',#60764);
#2013=PLANE('',#60765);
#2014=PLANE('',#60766);
#2015=PLANE('',#60767);
#2016=PLANE('',#60768);
#2017=PLANE('',#60769);
#2018=PLANE('',#60770);
#2019=PLANE('',#60771);
#2020=PLANE('',#60772);
#2021=PLANE('',#60773);
#2022=PLANE('',#60774);
#2023=PLANE('',#60775);
#2024=PLANE('',#60776);
#2025=PLANE('',#60777);
#2026=PLANE('',#60778);
#2027=PLANE('',#60779);
#2028=PLANE('',#60780);
#2029=PLANE('',#60781);
#2030=PLANE('',#60782);
#2031=PLANE('',#60783);
#2032=PLANE('',#60784);
#2033=PLANE('',#60785);
#2034=PLANE('',#60786);
#2035=PLANE('',#60787);
#2036=PLANE('',#60788);
#2037=PLANE('',#60789);
#2038=PLANE('',#60790);
#2039=PLANE('',#60791);
#2040=PLANE('',#60792);
#2041=PLANE('',#60793);
#2042=PLANE('',#60794);
#2043=PLANE('',#60795);
#2044=PLANE('',#60796);
#2045=PLANE('',#60797);
#2046=PLANE('',#60798);
#2047=PLANE('',#60799);
#2048=PLANE('',#60800);
#2049=PLANE('',#60801);
#2050=PLANE('',#60802);
#2051=PLANE('',#60803);
#2052=PLANE('',#60804);
#2053=PLANE('',#60805);
#2054=PLANE('',#60806);
#2055=PLANE('',#60807);
#2056=PLANE('',#60808);
#2057=PLANE('',#60809);
#2058=PLANE('',#60810);
#2059=PLANE('',#60811);
#2060=PLANE('',#60812);
#2061=PLANE('',#60813);
#2062=PLANE('',#60814);
#2063=PLANE('',#60815);
#2064=PLANE('',#60816);
#2065=PLANE('',#60817);
#2066=PLANE('',#60818);
#2067=PLANE('',#60819);
#2068=PLANE('',#60820);
#2069=PLANE('',#60821);
#2070=PLANE('',#60822);
#2071=PLANE('',#60823);
#2072=PLANE('',#60824);
#2073=PLANE('',#60825);
#2074=PLANE('',#60826);
#2075=PLANE('',#60827);
#2076=PLANE('',#60828);
#2077=PLANE('',#60829);
#2078=PLANE('',#60830);
#2079=PLANE('',#60831);
#2080=PLANE('',#60832);
#2081=PLANE('',#60833);
#2082=PLANE('',#60834);
#2083=PLANE('',#60835);
#2084=PLANE('',#60836);
#2085=PLANE('',#60837);
#2086=PLANE('',#60838);
#2087=PLANE('',#60839);
#2088=PLANE('',#60840);
#2089=PLANE('',#60841);
#2090=PLANE('',#60842);
#2091=PLANE('',#60843);
#2092=PLANE('',#60844);
#2093=PLANE('',#60845);
#2094=PLANE('',#60846);
#2095=PLANE('',#60847);
#2096=PLANE('',#60848);
#2097=PLANE('',#60849);
#2098=PLANE('',#60850);
#2099=PLANE('',#60851);
#2100=PLANE('',#60852);
#2101=PLANE('',#60853);
#2102=PLANE('',#60854);
#2103=PLANE('',#60855);
#2104=PLANE('',#60856);
#2105=PLANE('',#60857);
#2106=PLANE('',#60858);
#2107=PLANE('',#60859);
#2108=PLANE('',#60860);
#2109=PLANE('',#60861);
#2110=PLANE('',#60862);
#2111=PLANE('',#60863);
#2112=PLANE('',#60864);
#2113=PLANE('',#60865);
#2114=PLANE('',#60866);
#2115=PLANE('',#60867);
#2116=PLANE('',#60868);
#2117=PLANE('',#60869);
#2118=PLANE('',#60870);
#2119=PLANE('',#60871);
#2120=PLANE('',#60872);
#2121=PLANE('',#60873);
#2122=PLANE('',#60874);
#2123=PLANE('',#60875);
#2124=PLANE('',#60876);
#2125=PLANE('',#60877);
#2126=PLANE('',#60878);
#2127=PLANE('',#60879);
#2128=PLANE('',#60880);
#2129=PLANE('',#60881);
#2130=PLANE('',#60882);
#2131=PLANE('',#60883);
#2132=PLANE('',#60884);
#2133=PLANE('',#60885);
#2134=PLANE('',#60886);
#2135=PLANE('',#60887);
#2136=PLANE('',#60888);
#2137=PLANE('',#60889);
#2138=PLANE('',#60890);
#2139=PLANE('',#60891);
#2140=PLANE('',#60892);
#2141=PLANE('',#60893);
#2142=PLANE('',#60894);
#2143=PLANE('',#60895);
#2144=PLANE('',#60896);
#2145=PLANE('',#60897);
#2146=PLANE('',#60898);
#2147=PLANE('',#60899);
#2148=PLANE('',#60900);
#2149=PLANE('',#60901);
#2150=PLANE('',#60902);
#2151=PLANE('',#60903);
#2152=PLANE('',#60904);
#2153=PLANE('',#60905);
#2154=PLANE('',#60906);
#2155=PLANE('',#60907);
#2156=PLANE('',#60908);
#2157=PLANE('',#60909);
#2158=PLANE('',#60910);
#2159=PLANE('',#60911);
#2160=PLANE('',#60912);
#2161=PLANE('',#60913);
#2162=PLANE('',#60914);
#2163=PLANE('',#60915);
#2164=PLANE('',#60916);
#2165=PLANE('',#60917);
#2166=PLANE('',#60918);
#2167=PLANE('',#60919);
#2168=PLANE('',#60920);
#2169=PLANE('',#60921);
#2170=PLANE('',#60922);
#2171=PLANE('',#60923);
#2172=PLANE('',#60924);
#2173=PLANE('',#60925);
#2174=PLANE('',#60926);
#2175=PLANE('',#60927);
#2176=PLANE('',#60928);
#2177=PLANE('',#60929);
#2178=PLANE('',#60930);
#2179=PLANE('',#60931);
#2180=PLANE('',#60932);
#2181=PLANE('',#60933);
#2182=PLANE('',#60934);
#2183=PLANE('',#60935);
#2184=PLANE('',#60936);
#2185=PLANE('',#60937);
#2186=PLANE('',#60938);
#2187=PLANE('',#60939);
#2188=PLANE('',#60940);
#2189=PLANE('',#60941);
#2190=PLANE('',#60942);
#2191=PLANE('',#60943);
#2192=PLANE('',#60944);
#2193=PLANE('',#60945);
#2194=PLANE('',#60946);
#2195=PLANE('',#60947);
#2196=PLANE('',#60948);
#2197=PLANE('',#60949);
#2198=PLANE('',#60950);
#2199=PLANE('',#60951);
#2200=PLANE('',#60952);
#2201=PLANE('',#60953);
#2202=PLANE('',#60954);
#2203=PLANE('',#60955);
#2204=PLANE('',#60956);
#2205=PLANE('',#60957);
#2206=PLANE('',#60958);
#2207=PLANE('',#60959);
#2208=PLANE('',#60960);
#2209=PLANE('',#60961);
#2210=PLANE('',#60962);
#2211=PLANE('',#60963);
#2212=PLANE('',#60964);
#2213=PLANE('',#60965);
#2214=PLANE('',#60966);
#2215=PLANE('',#60967);
#2216=PLANE('',#60968);
#2217=PLANE('',#60969);
#2218=PLANE('',#60970);
#2219=PLANE('',#60971);
#2220=PLANE('',#60972);
#2221=PLANE('',#60973);
#2222=PLANE('',#60974);
#2223=PLANE('',#60975);
#2224=PLANE('',#60976);
#2225=PLANE('',#60977);
#2226=PLANE('',#60978);
#2227=PLANE('',#60979);
#2228=PLANE('',#60980);
#2229=PLANE('',#60981);
#2230=PLANE('',#60982);
#2231=PLANE('',#60983);
#2232=PLANE('',#60984);
#2233=PLANE('',#60985);
#2234=PLANE('',#60986);
#2235=PLANE('',#60987);
#2236=PLANE('',#60988);
#2237=PLANE('',#60989);
#2238=PLANE('',#60990);
#2239=PLANE('',#60991);
#2240=PLANE('',#60992);
#2241=PLANE('',#60993);
#2242=PLANE('',#60994);
#2243=PLANE('',#60995);
#2244=PLANE('',#60996);
#2245=PLANE('',#60997);
#2246=PLANE('',#60998);
#2247=PLANE('',#60999);
#2248=PLANE('',#61000);
#2249=PLANE('',#61001);
#2250=PLANE('',#61002);
#2251=PLANE('',#61003);
#2252=PLANE('',#61004);
#2253=PLANE('',#61005);
#2254=PLANE('',#61006);
#2255=PLANE('',#61007);
#2256=PLANE('',#61008);
#2257=PLANE('',#61009);
#2258=PLANE('',#61010);
#2259=PLANE('',#61011);
#2260=PLANE('',#61012);
#2261=PLANE('',#61013);
#2262=PLANE('',#61014);
#2263=PLANE('',#61015);
#2264=PLANE('',#61016);
#2265=PLANE('',#61017);
#2266=PLANE('',#61018);
#2267=PLANE('',#61019);
#2268=PLANE('',#61020);
#2269=PLANE('',#61021);
#2270=PLANE('',#61022);
#2271=PLANE('',#61023);
#2272=PLANE('',#61024);
#2273=PLANE('',#61025);
#2274=PLANE('',#61026);
#2275=PLANE('',#61027);
#2276=PLANE('',#61028);
#2277=PLANE('',#61029);
#2278=PLANE('',#61030);
#2279=PLANE('',#61031);
#2280=PLANE('',#61032);
#2281=PLANE('',#61033);
#2282=PLANE('',#61034);
#2283=PLANE('',#61035);
#2284=PLANE('',#61036);
#2285=PLANE('',#61037);
#2286=PLANE('',#61038);
#2287=PLANE('',#61039);
#2288=PLANE('',#61040);
#2289=PLANE('',#61041);
#2290=PLANE('',#61042);
#2291=PLANE('',#61043);
#2292=PLANE('',#61044);
#2293=PLANE('',#61045);
#2294=PLANE('',#61046);
#2295=PLANE('',#61047);
#2296=PLANE('',#61048);
#2297=PLANE('',#61049);
#2298=PLANE('',#61050);
#2299=PLANE('',#61051);
#2300=PLANE('',#61052);
#2301=PLANE('',#61053);
#2302=PLANE('',#61054);
#2303=PLANE('',#61055);
#2304=PLANE('',#61056);
#2305=PLANE('',#61057);
#2306=PLANE('',#61058);
#2307=PLANE('',#61059);
#2308=PLANE('',#61060);
#2309=PLANE('',#61061);
#2310=PLANE('',#61062);
#2311=PLANE('',#61063);
#2312=PLANE('',#61064);
#2313=PLANE('',#61065);
#2314=PLANE('',#61066);
#2315=PLANE('',#61067);
#2316=PLANE('',#61068);
#2317=PLANE('',#61069);
#2318=PLANE('',#61070);
#2319=PLANE('',#61071);
#2320=PLANE('',#61072);
#2321=PLANE('',#61073);
#2322=PLANE('',#61074);
#2323=PLANE('',#61075);
#2324=PLANE('',#61076);
#2325=PLANE('',#61077);
#2326=PLANE('',#61078);
#2327=PLANE('',#61079);
#2328=PLANE('',#61080);
#2329=PLANE('',#61081);
#2330=PLANE('',#61082);
#2331=PLANE('',#61083);
#2332=PLANE('',#61084);
#2333=PLANE('',#61085);
#2334=PLANE('',#61086);
#2335=PLANE('',#61087);
#2336=PLANE('',#61088);
#2337=PLANE('',#61089);
#2338=PLANE('',#61090);
#2339=PLANE('',#61091);
#2340=PLANE('',#61092);
#2341=PLANE('',#61093);
#2342=PLANE('',#61094);
#2343=PLANE('',#61095);
#2344=PLANE('',#61096);
#2345=PLANE('',#61097);
#2346=PLANE('',#61098);
#2347=PLANE('',#61099);
#2348=PLANE('',#61100);
#2349=PLANE('',#61101);
#2350=PLANE('',#61102);
#2351=PLANE('',#61103);
#2352=PLANE('',#61104);
#2353=PLANE('',#61105);
#2354=PLANE('',#61106);
#2355=PLANE('',#61107);
#2356=PLANE('',#61108);
#2357=PLANE('',#61109);
#2358=PLANE('',#61110);
#2359=PLANE('',#61111);
#2360=PLANE('',#61112);
#2361=PLANE('',#61113);
#2362=PLANE('',#61114);
#2363=PLANE('',#61115);
#2364=PLANE('',#61116);
#2365=PLANE('',#61117);
#2366=PLANE('',#61118);
#2367=PLANE('',#61119);
#2368=PLANE('',#61120);
#2369=PLANE('',#61121);
#2370=PLANE('',#61122);
#2371=PLANE('',#61123);
#2372=PLANE('',#61124);
#2373=PLANE('',#61125);
#2374=PLANE('',#61126);
#2375=PLANE('',#61127);
#2376=PLANE('',#61128);
#2377=PLANE('',#61129);
#2378=PLANE('',#61130);
#2379=PLANE('',#61131);
#2380=PLANE('',#61132);
#2381=PLANE('',#61133);
#2382=PLANE('',#61134);
#2383=PLANE('',#61135);
#2384=PLANE('',#61136);
#2385=PLANE('',#61137);
#2386=PLANE('',#61138);
#2387=PLANE('',#61139);
#2388=PLANE('',#61140);
#2389=PLANE('',#61141);
#2390=PLANE('',#61142);
#2391=PLANE('',#61143);
#2392=PLANE('',#61144);
#2393=PLANE('',#61145);
#2394=PLANE('',#61146);
#2395=PLANE('',#61147);
#2396=PLANE('',#61148);
#2397=PLANE('',#61149);
#2398=PLANE('',#61150);
#2399=PLANE('',#61151);
#2400=PLANE('',#61152);
#2401=PLANE('',#61153);
#2402=PLANE('',#61154);
#2403=PLANE('',#61155);
#2404=PLANE('',#61156);
#2405=PLANE('',#61157);
#2406=PLANE('',#61158);
#2407=PLANE('',#61159);
#2408=PLANE('',#61160);
#2409=PLANE('',#61161);
#2410=PLANE('',#61162);
#2411=PLANE('',#61163);
#2412=PLANE('',#61164);
#2413=PLANE('',#61165);
#2414=PLANE('',#61166);
#2415=PLANE('',#61167);
#2416=PLANE('',#61168);
#2417=PLANE('',#61169);
#2418=PLANE('',#61170);
#2419=PLANE('',#61171);
#2420=PLANE('',#61172);
#2421=PLANE('',#61173);
#2422=PLANE('',#61174);
#2423=PLANE('',#61175);
#2424=PLANE('',#61176);
#2425=PLANE('',#61177);
#2426=PLANE('',#61178);
#2427=PLANE('',#61179);
#2428=PLANE('',#61180);
#2429=PLANE('',#61181);
#2430=PLANE('',#61182);
#2431=PLANE('',#61183);
#2432=PLANE('',#61184);
#2433=PLANE('',#61185);
#2434=PLANE('',#61186);
#2435=PLANE('',#61187);
#2436=PLANE('',#61188);
#2437=PLANE('',#61189);
#2438=PLANE('',#61190);
#2439=PLANE('',#61191);
#2440=PLANE('',#61192);
#2441=PLANE('',#61193);
#2442=PLANE('',#61194);
#2443=PLANE('',#61195);
#2444=PLANE('',#61196);
#2445=PLANE('',#61197);
#2446=PLANE('',#61198);
#2447=PLANE('',#61199);
#2448=PLANE('',#61200);
#2449=PLANE('',#61201);
#2450=PLANE('',#61202);
#2451=PLANE('',#61203);
#2452=PLANE('',#61204);
#2453=PLANE('',#61205);
#2454=PLANE('',#61206);
#2455=PLANE('',#61207);
#2456=PLANE('',#61208);
#2457=PLANE('',#61209);
#2458=PLANE('',#61210);
#2459=PLANE('',#61211);
#2460=PLANE('',#61212);
#2461=PLANE('',#61213);
#2462=PLANE('',#61214);
#2463=PLANE('',#61215);
#2464=PLANE('',#61216);
#2465=PLANE('',#61217);
#2466=PLANE('',#61218);
#2467=PLANE('',#61219);
#2468=PLANE('',#61220);
#2469=PLANE('',#61221);
#2470=PLANE('',#61222);
#2471=PLANE('',#61223);
#2472=PLANE('',#61224);
#2473=PLANE('',#61225);
#2474=PLANE('',#61226);
#2475=PLANE('',#61227);
#2476=PLANE('',#61228);
#2477=PLANE('',#61229);
#2478=PLANE('',#61230);
#2479=PLANE('',#61231);
#2480=PLANE('',#61232);
#2481=PLANE('',#61233);
#2482=PLANE('',#61234);
#2483=PLANE('',#61235);
#2484=PLANE('',#61236);
#2485=PLANE('',#61237);
#2486=PLANE('',#61238);
#2487=PLANE('',#61239);
#2488=PLANE('',#61240);
#2489=PLANE('',#61241);
#2490=PLANE('',#61242);
#2491=PLANE('',#61243);
#2492=PLANE('',#61244);
#2493=PLANE('',#61245);
#2494=PLANE('',#61246);
#2495=PLANE('',#61247);
#2496=PLANE('',#61248);
#2497=PLANE('',#61249);
#2498=PLANE('',#61250);
#2499=PLANE('',#61251);
#2500=PLANE('',#61252);
#2501=PLANE('',#61253);
#2502=PLANE('',#61254);
#2503=PLANE('',#61255);
#2504=PLANE('',#61256);
#2505=PLANE('',#61257);
#2506=PLANE('',#61258);
#2507=PLANE('',#61259);
#2508=PLANE('',#61260);
#2509=PLANE('',#61261);
#2510=PLANE('',#61262);
#2511=PLANE('',#61263);
#2512=PLANE('',#61264);
#2513=PLANE('',#61265);
#2514=PLANE('',#61266);
#2515=PLANE('',#61267);
#2516=PLANE('',#61268);
#2517=PLANE('',#61269);
#2518=PLANE('',#61270);
#2519=PLANE('',#61271);
#2520=PLANE('',#61272);
#2521=PLANE('',#61273);
#2522=PLANE('',#61274);
#2523=PLANE('',#61275);
#2524=PLANE('',#61276);
#2525=PLANE('',#61277);
#2526=PLANE('',#61278);
#2527=PLANE('',#61279);
#2528=PLANE('',#61280);
#2529=PLANE('',#61281);
#2530=PLANE('',#61282);
#2531=PLANE('',#61283);
#2532=PLANE('',#61284);
#2533=PLANE('',#61285);
#2534=PLANE('',#61286);
#2535=PLANE('',#61287);
#2536=PLANE('',#61288);
#2537=PLANE('',#61289);
#2538=PLANE('',#61290);
#2539=PLANE('',#61291);
#2540=PLANE('',#61292);
#2541=PLANE('',#61293);
#2542=PLANE('',#61294);
#2543=PLANE('',#61295);
#2544=PLANE('',#61296);
#2545=PLANE('',#61297);
#2546=PLANE('',#61298);
#2547=PLANE('',#61299);
#2548=PLANE('',#61300);
#2549=PLANE('',#61301);
#2550=PLANE('',#61302);
#2551=PLANE('',#61303);
#2552=PLANE('',#61304);
#2553=PLANE('',#61305);
#2554=PLANE('',#61306);
#2555=PLANE('',#61307);
#2556=PLANE('',#61308);
#2557=PLANE('',#61309);
#2558=PLANE('',#61310);
#2559=PLANE('',#61311);
#2560=PLANE('',#61312);
#2561=PLANE('',#61313);
#2562=PLANE('',#61314);
#2563=PLANE('',#61315);
#2564=PLANE('',#61316);
#2565=PLANE('',#61317);
#2566=PLANE('',#61318);
#2567=PLANE('',#61319);
#2568=PLANE('',#61320);
#2569=PLANE('',#61321);
#2570=PLANE('',#61322);
#2571=PLANE('',#61323);
#2572=PLANE('',#61324);
#2573=PLANE('',#61325);
#2574=PLANE('',#61326);
#2575=PLANE('',#61327);
#2576=PLANE('',#61328);
#2577=PLANE('',#61329);
#2578=PLANE('',#61330);
#2579=PLANE('',#61331);
#2580=PLANE('',#61332);
#2581=PLANE('',#61333);
#2582=PLANE('',#61334);
#2583=PLANE('',#61335);
#2584=PLANE('',#61336);
#2585=PLANE('',#61337);
#2586=PLANE('',#61338);
#2587=PLANE('',#61339);
#2588=PLANE('',#61340);
#2589=PLANE('',#61341);
#2590=PLANE('',#61342);
#2591=PLANE('',#61343);
#2592=PLANE('',#61344);
#2593=PLANE('',#61345);
#2594=PLANE('',#61346);
#2595=PLANE('',#61347);
#2596=PLANE('',#61348);
#2597=PLANE('',#61349);
#2598=PLANE('',#61350);
#2599=PLANE('',#61351);
#2600=PLANE('',#61352);
#2601=PLANE('',#61353);
#2602=PLANE('',#61354);
#2603=PLANE('',#61355);
#2604=PLANE('',#61356);
#2605=PLANE('',#61357);
#2606=PLANE('',#61358);
#2607=PLANE('',#61359);
#2608=PLANE('',#61360);
#2609=PLANE('',#61361);
#2610=PLANE('',#61362);
#2611=PLANE('',#61363);
#2612=PLANE('',#61364);
#2613=PLANE('',#61365);
#2614=PLANE('',#61366);
#2615=PLANE('',#61367);
#2616=PLANE('',#61368);
#2617=PLANE('',#61369);
#2618=PLANE('',#61370);
#2619=PLANE('',#61371);
#2620=PLANE('',#61372);
#2621=PLANE('',#61373);
#2622=PLANE('',#61374);
#2623=PLANE('',#61375);
#2624=PLANE('',#61376);
#2625=PLANE('',#61377);
#2626=PLANE('',#61378);
#2627=PLANE('',#61379);
#2628=PLANE('',#61380);
#2629=PLANE('',#61381);
#2630=PLANE('',#61382);
#2631=PLANE('',#61383);
#2632=PLANE('',#61384);
#2633=PLANE('',#61385);
#2634=PLANE('',#61386);
#2635=PLANE('',#61387);
#2636=PLANE('',#61388);
#2637=PLANE('',#61389);
#2638=PLANE('',#61390);
#2639=PLANE('',#61391);
#2640=PLANE('',#61392);
#2641=PLANE('',#61393);
#2642=PLANE('',#61394);
#2643=PLANE('',#61395);
#2644=PLANE('',#61396);
#2645=PLANE('',#61397);
#2646=PLANE('',#61398);
#2647=PLANE('',#61399);
#2648=PLANE('',#61400);
#2649=PLANE('',#61401);
#2650=PLANE('',#61402);
#2651=PLANE('',#61403);
#2652=PLANE('',#61404);
#2653=PLANE('',#61405);
#2654=PLANE('',#61406);
#2655=PLANE('',#61407);
#2656=PLANE('',#61408);
#2657=PLANE('',#61409);
#2658=PLANE('',#61410);
#2659=PLANE('',#61411);
#2660=PLANE('',#61412);
#2661=PLANE('',#61413);
#2662=PLANE('',#61414);
#2663=PLANE('',#61415);
#2664=PLANE('',#61416);
#2665=PLANE('',#61417);
#2666=PLANE('',#61418);
#2667=PLANE('',#61419);
#2668=PLANE('',#61420);
#2669=PLANE('',#61421);
#2670=PLANE('',#61422);
#2671=PLANE('',#61423);
#2672=PLANE('',#61424);
#2673=PLANE('',#61425);
#2674=PLANE('',#61426);
#2675=PLANE('',#61427);
#2676=PLANE('',#61428);
#2677=PLANE('',#61429);
#2678=PLANE('',#61430);
#2679=PLANE('',#61431);
#2680=PLANE('',#61432);
#2681=PLANE('',#61433);
#2682=PLANE('',#61434);
#2683=PLANE('',#61435);
#2684=PLANE('',#61436);
#2685=PLANE('',#61437);
#2686=PLANE('',#61438);
#2687=PLANE('',#61439);
#2688=PLANE('',#61440);
#2689=PLANE('',#61441);
#2690=PLANE('',#61442);
#2691=PLANE('',#61443);
#2692=PLANE('',#61444);
#2693=PLANE('',#61445);
#2694=PLANE('',#61446);
#2695=PLANE('',#61447);
#2696=PLANE('',#61448);
#2697=PLANE('',#61449);
#2698=PLANE('',#61450);
#2699=PLANE('',#61451);
#2700=PLANE('',#61452);
#2701=PLANE('',#61453);
#2702=PLANE('',#61454);
#2703=PLANE('',#61455);
#2704=PLANE('',#61456);
#2705=PLANE('',#61457);
#2706=PLANE('',#61458);
#2707=PLANE('',#61459);
#2708=PLANE('',#61460);
#2709=PLANE('',#61461);
#2710=PLANE('',#61462);
#2711=PLANE('',#61463);
#2712=PLANE('',#61464);
#2713=PLANE('',#61465);
#2714=PLANE('',#61466);
#2715=PLANE('',#61467);
#2716=PLANE('',#61468);
#2717=PLANE('',#61469);
#2718=PLANE('',#61470);
#2719=PLANE('',#61471);
#2720=PLANE('',#61472);
#2721=PLANE('',#61473);
#2722=PLANE('',#61474);
#2723=PLANE('',#61475);
#2724=PLANE('',#61476);
#2725=PLANE('',#61477);
#2726=PLANE('',#61478);
#2727=PLANE('',#61479);
#2728=PLANE('',#61480);
#2729=PLANE('',#61481);
#2730=PLANE('',#61482);
#2731=PLANE('',#61483);
#2732=PLANE('',#61484);
#2733=PLANE('',#61485);
#2734=PLANE('',#61486);
#2735=PLANE('',#61487);
#2736=PLANE('',#61488);
#2737=PLANE('',#61489);
#2738=PLANE('',#61490);
#2739=PLANE('',#61491);
#2740=PLANE('',#61492);
#2741=PLANE('',#61493);
#2742=PLANE('',#61494);
#2743=PLANE('',#61495);
#2744=PLANE('',#61496);
#2745=PLANE('',#61497);
#2746=PLANE('',#61498);
#2747=PLANE('',#61499);
#2748=PLANE('',#61500);
#2749=PLANE('',#61501);
#2750=PLANE('',#61502);
#2751=PLANE('',#61503);
#2752=PLANE('',#61504);
#2753=PLANE('',#61505);
#2754=PLANE('',#61506);
#2755=PLANE('',#61507);
#2756=PLANE('',#61508);
#2757=PLANE('',#61509);
#2758=PLANE('',#61510);
#2759=PLANE('',#61511);
#2760=PLANE('',#61512);
#2761=PLANE('',#61513);
#2762=PLANE('',#61514);
#2763=PLANE('',#61515);
#2764=PLANE('',#61516);
#2765=PLANE('',#61517);
#2766=PLANE('',#61518);
#2767=PLANE('',#61519);
#2768=PLANE('',#61520);
#2769=PLANE('',#61521);
#2770=PLANE('',#61522);
#2771=PLANE('',#61523);
#2772=PLANE('',#61524);
#2773=PLANE('',#61525);
#2774=PLANE('',#61526);
#2775=PLANE('',#61527);
#2776=PLANE('',#61528);
#2777=PLANE('',#61529);
#2778=PLANE('',#61530);
#2779=PLANE('',#61531);
#2780=PLANE('',#61532);
#2781=PLANE('',#61533);
#2782=PLANE('',#61534);
#2783=PLANE('',#61535);
#2784=PLANE('',#61536);
#2785=PLANE('',#61537);
#2786=PLANE('',#61538);
#2787=PLANE('',#61539);
#2788=PLANE('',#61540);
#2789=PLANE('',#61541);
#2790=PLANE('',#61542);
#2791=PLANE('',#61543);
#2792=PLANE('',#61544);
#2793=PLANE('',#61545);
#2794=PLANE('',#61546);
#2795=PLANE('',#61547);
#2796=PLANE('',#61548);
#2797=PLANE('',#61549);
#2798=PLANE('',#61550);
#2799=PLANE('',#61551);
#2800=PLANE('',#61552);
#2801=PLANE('',#61553);
#2802=PLANE('',#61554);
#2803=PLANE('',#61555);
#2804=PLANE('',#61556);
#2805=PLANE('',#61557);
#2806=PLANE('',#61558);
#2807=PLANE('',#61559);
#2808=PLANE('',#61560);
#2809=PLANE('',#61561);
#2810=PLANE('',#61562);
#2811=PLANE('',#61563);
#2812=PLANE('',#61564);
#2813=PLANE('',#61565);
#2814=PLANE('',#61566);
#2815=PLANE('',#61567);
#2816=PLANE('',#61568);
#2817=PLANE('',#61569);
#2818=PLANE('',#61570);
#2819=PLANE('',#61571);
#2820=PLANE('',#61572);
#2821=PLANE('',#61573);
#2822=PLANE('',#61574);
#2823=PLANE('',#61575);
#2824=PLANE('',#61576);
#2825=PLANE('',#61577);
#2826=PLANE('',#61578);
#2827=PLANE('',#61579);
#2828=PLANE('',#61580);
#2829=PLANE('',#61581);
#2830=PLANE('',#61582);
#2831=PLANE('',#61583);
#2832=PLANE('',#61584);
#2833=PLANE('',#61585);
#2834=PLANE('',#61586);
#2835=PLANE('',#61587);
#2836=PLANE('',#61588);
#2837=PLANE('',#61589);
#2838=PLANE('',#61590);
#2839=PLANE('',#61591);
#2840=PLANE('',#61592);
#2841=PLANE('',#61593);
#2842=PLANE('',#61594);
#2843=PLANE('',#61595);
#2844=PLANE('',#61596);
#2845=PLANE('',#61597);
#2846=PLANE('',#61598);
#2847=PLANE('',#61599);
#2848=PLANE('',#61600);
#2849=PLANE('',#61601);
#2850=PLANE('',#61602);
#2851=PLANE('',#61603);
#2852=PLANE('',#61604);
#2853=PLANE('',#61605);
#2854=PLANE('',#61606);
#2855=PLANE('',#61607);
#2856=PLANE('',#61608);
#2857=PLANE('',#61609);
#2858=PLANE('',#61610);
#2859=PLANE('',#61611);
#2860=PLANE('',#61612);
#2861=PLANE('',#61613);
#2862=PLANE('',#61614);
#2863=PLANE('',#61615);
#2864=PLANE('',#61616);
#2865=PLANE('',#61617);
#2866=PLANE('',#61618);
#2867=PLANE('',#61619);
#2868=PLANE('',#61620);
#2869=PLANE('',#61621);
#2870=PLANE('',#61622);
#2871=PLANE('',#61623);
#2872=PLANE('',#61624);
#2873=PLANE('',#61625);
#2874=PLANE('',#61626);
#2875=PLANE('',#61627);
#2876=PLANE('',#61628);
#2877=PLANE('',#61629);
#2878=PLANE('',#61630);
#2879=PLANE('',#61631);
#2880=PLANE('',#61632);
#2881=PLANE('',#61633);
#2882=PLANE('',#61634);
#2883=PLANE('',#61635);
#2884=PLANE('',#61636);
#2885=PLANE('',#61637);
#2886=PLANE('',#61638);
#2887=PLANE('',#61639);
#2888=PLANE('',#61640);
#2889=PLANE('',#61641);
#2890=PLANE('',#61642);
#2891=PLANE('',#61643);
#2892=PLANE('',#61644);
#2893=PLANE('',#61645);
#2894=PLANE('',#61646);
#2895=PLANE('',#61647);
#2896=PLANE('',#61648);
#2897=PLANE('',#61649);
#2898=PLANE('',#61650);
#2899=PLANE('',#61651);
#2900=PLANE('',#61652);
#2901=PLANE('',#61653);
#2902=PLANE('',#61654);
#2903=PLANE('',#61655);
#2904=PLANE('',#61656);
#2905=PLANE('',#61657);
#2906=PLANE('',#61658);
#2907=PLANE('',#61659);
#2908=PLANE('',#61660);
#2909=PLANE('',#61661);
#2910=PLANE('',#61662);
#2911=PLANE('',#61663);
#2912=PLANE('',#61664);
#2913=PLANE('',#61665);
#2914=PLANE('',#61668);
#2915=PLANE('',#61669);
#2916=PLANE('',#61670);
#2917=PLANE('',#61671);
#2918=PLANE('',#61688);
#2919=PLANE('',#61699);
#2920=PLANE('',#61704);
#2921=PLANE('',#61709);
#2922=PLANE('',#61714);
#2923=PLANE('',#61719);
#2924=PLANE('',#61724);
#2925=PLANE('',#61728);
#2926=PLANE('',#61748);
#2927=PLANE('',#61750);
#2928=PLANE('',#61751);
#2929=PLANE('',#61752);
#2930=PLANE('',#61753);
#2931=PLANE('',#61754);
#2932=PLANE('',#61755);
#2933=PLANE('',#61757);
#2934=PLANE('',#61758);
#2935=PLANE('',#61764);
#2936=PLANE('',#61765);
#2937=PLANE('',#61766);
#2938=PLANE('',#61767);
#2939=PLANE('',#61768);
#2940=PLANE('',#61769);
#2941=PLANE('',#61771);
#2942=PLANE('',#61772);
#2943=PLANE('',#61773);
#2944=PLANE('',#61774);
#2945=PLANE('',#61775);
#2946=PLANE('',#61776);
#2947=PLANE('',#61777);
#2948=PLANE('',#61778);
#2949=PLANE('',#61779);
#2950=PLANE('',#61780);
#2951=PLANE('',#61781);
#2952=PLANE('',#61782);
#2953=PLANE('',#61783);
#2954=PLANE('',#61784);
#2955=PLANE('',#61785);
#2956=PLANE('',#61786);
#2957=PLANE('',#61788);
#2958=PLANE('',#61789);
#2959=PLANE('',#61790);
#2960=PLANE('',#61791);
#2961=PLANE('',#61792);
#2962=PLANE('',#61793);
#2963=PLANE('',#61794);
#2964=PLANE('',#61795);
#2965=PLANE('',#61796);
#2966=PLANE('',#61797);
#2967=PLANE('',#61798);
#2968=PLANE('',#61799);
#2969=PLANE('',#61800);
#2970=PLANE('',#61801);
#2971=PLANE('',#61802);
#2972=PLANE('',#61803);
#2973=PLANE('',#61804);
#2974=PLANE('',#61806);
#2975=PLANE('',#61808);
#2976=PLANE('',#61810);
#2977=PLANE('',#61811);
#2978=PLANE('',#61820);
#2979=PLANE('',#61836);
#2980=PLANE('',#61850);
#2981=PLANE('',#61855);
#2982=PLANE('',#61863);
#2983=PLANE('',#61879);
#2984=PLANE('',#61880);
#2985=PLANE('',#61881);
#2986=PLANE('',#61882);
#2987=PLANE('',#61883);
#2988=PLANE('',#61884);
#2989=PLANE('',#61916);
#2990=PLANE('',#61917);
#2991=PLANE('',#61918);
#2992=PLANE('',#61919);
#2993=PLANE('',#61920);
#2994=PLANE('',#61921);
#2995=PLANE('',#61922);
#2996=PLANE('',#61923);
#2997=PLANE('',#61924);
#2998=PLANE('',#61925);
#2999=PLANE('',#61926);
#3000=PLANE('',#61927);
#3001=PLANE('',#61928);
#3002=PLANE('',#61929);
#3003=PLANE('',#61930);
#3004=PLANE('',#61931);
#3005=PLANE('',#61932);
#3006=PLANE('',#61933);
#3007=PLANE('',#61934);
#3008=PLANE('',#61935);
#3009=PLANE('',#61936);
#3010=PLANE('',#61937);
#3011=PLANE('',#61938);
#3012=PLANE('',#61939);
#3013=PLANE('',#61940);
#3014=PLANE('',#61941);
#3015=PLANE('',#61942);
#3016=PLANE('',#61943);
#3017=PLANE('',#61944);
#3018=PLANE('',#61945);
#3019=PLANE('',#61946);
#3020=PLANE('',#61947);
#3021=PLANE('',#61955);
#3022=PLANE('',#61956);
#3023=PLANE('',#61957);
#3024=PLANE('',#61958);
#3025=PLANE('',#61959);
#3026=PLANE('',#61960);
#3027=PLANE('',#61961);
#3028=PLANE('',#61962);
#3029=PLANE('',#61963);
#3030=PLANE('',#61964);
#3031=PLANE('',#61965);
#3032=PLANE('',#61966);
#3033=PLANE('',#61967);
#3034=PLANE('',#61968);
#3035=PLANE('',#61970);
#3036=PLANE('',#61972);
#3037=PLANE('',#61974);
#3038=PLANE('',#61975);
#3039=PLANE('',#61977);
#3040=PLANE('',#61979);
#3041=PLANE('',#61980);
#3042=PLANE('',#61988);
#3043=PLANE('',#61990);
#3044=PLANE('',#61995);
#3045=PLANE('',#61996);
#3046=PLANE('',#61997);
#3047=PLANE('',#62001);
#3048=PLANE('',#62037);
#3049=PLANE('',#62038);
#3050=PLANE('',#62042);
#3051=PLANE('',#62043);
#3052=PLANE('',#62044);
#3053=PLANE('',#62048);
#3054=PLANE('',#62049);
#3055=PLANE('',#62050);
#3056=PLANE('',#62054);
#3057=PLANE('',#62055);
#3058=PLANE('',#62056);
#3059=PLANE('',#62060);
#3060=PLANE('',#62061);
#3061=PLANE('',#62062);
#3062=PLANE('',#62066);
#3063=PLANE('',#62067);
#3064=PLANE('',#62068);
#3065=PLANE('',#62072);
#3066=PLANE('',#62073);
#3067=PLANE('',#62074);
#3068=PLANE('',#62078);
#3069=PLANE('',#62079);
#3070=PLANE('',#62080);
#3071=PLANE('',#62084);
#3072=PLANE('',#62085);
#3073=PLANE('',#62086);
#3074=PLANE('',#62090);
#3075=PLANE('',#62091);
#3076=PLANE('',#62092);
#3077=PLANE('',#62096);
#3078=PLANE('',#62097);
#3079=PLANE('',#62098);
#3080=PLANE('',#62102);
#3081=PLANE('',#62103);
#3082=PLANE('',#62104);
#3083=PLANE('',#62108);
#3084=PLANE('',#62109);
#3085=PLANE('',#62110);
#3086=PLANE('',#62114);
#3087=PLANE('',#62115);
#3088=PLANE('',#62116);
#3089=PLANE('',#62120);
#3090=PLANE('',#62121);
#3091=PLANE('',#62125);
#3092=PLANE('',#62126);
#3093=PLANE('',#62130);
#3094=PLANE('',#62131);
#3095=PLANE('',#62137);
#3096=PLANE('',#62139);
#3097=PLANE('',#62144);
#3098=PLANE('',#62145);
#3099=PLANE('',#62146);
#3100=PLANE('',#62193);
#3101=PLANE('',#62194);
#3102=PLANE('',#62236);
#3103=PLANE('',#62237);
#3104=PLANE('',#62238);
#3105=PLANE('',#62239);
#3106=PLANE('',#62242);
#3107=PLANE('',#62243);
#3108=PLANE('',#62245);
#3109=PLANE('',#62246);
#3110=PLANE('',#62247);
#3111=PLANE('',#62248);
#3112=PLANE('',#62251);
#3113=PLANE('',#62252);
#3114=PLANE('',#62254);
#3115=PLANE('',#62255);
#3116=PLANE('',#62256);
#3117=PLANE('',#62257);
#3118=PLANE('',#62260);
#3119=PLANE('',#62261);
#3120=PLANE('',#62263);
#3121=PLANE('',#62264);
#3122=PLANE('',#62265);
#3123=PLANE('',#62266);
#3124=PLANE('',#62269);
#3125=PLANE('',#62270);
#3126=PLANE('',#62272);
#3127=PLANE('',#62273);
#3128=PLANE('',#62274);
#3129=PLANE('',#62275);
#3130=PLANE('',#62278);
#3131=PLANE('',#62279);
#3132=PLANE('',#62281);
#3133=PLANE('',#62282);
#3134=PLANE('',#62283);
#3135=PLANE('',#62284);
#3136=PLANE('',#62287);
#3137=PLANE('',#62288);
#3138=PLANE('',#62290);
#3139=PLANE('',#62291);
#3140=PLANE('',#62292);
#3141=PLANE('',#62293);
#3142=PLANE('',#62296);
#3143=PLANE('',#62297);
#3144=PLANE('',#62299);
#3145=PLANE('',#62300);
#3146=PLANE('',#62301);
#3147=PLANE('',#62302);
#3148=PLANE('',#62305);
#3149=PLANE('',#62306);
#3150=PLANE('',#62308);
#3151=PLANE('',#62309);
#3152=PLANE('',#62310);
#3153=PLANE('',#62311);
#3154=PLANE('',#62314);
#3155=PLANE('',#62315);
#3156=PLANE('',#62317);
#3157=PLANE('',#62318);
#3158=PLANE('',#62319);
#3159=PLANE('',#62320);
#3160=PLANE('',#62323);
#3161=PLANE('',#62324);
#3162=PLANE('',#62326);
#3163=PLANE('',#62327);
#3164=PLANE('',#62328);
#3165=PLANE('',#62329);
#3166=PLANE('',#62332);
#3167=PLANE('',#62333);
#3168=PLANE('',#62335);
#3169=PLANE('',#62336);
#3170=PLANE('',#62337);
#3171=PLANE('',#62338);
#3172=PLANE('',#62341);
#3173=PLANE('',#62342);
#3174=PLANE('',#62344);
#3175=PLANE('',#62345);
#3176=PLANE('',#62346);
#3177=PLANE('',#62347);
#3178=PLANE('',#62351);
#3179=PLANE('',#62359);
#3180=PLANE('',#62365);
#3181=PLANE('',#62367);
#3182=PLANE('',#62371);
#3183=PLANE('',#62379);
#3184=PLANE('',#62385);
#3185=PLANE('',#62391);
#3186=PLANE('',#62402);
#3187=PLANE('',#62408);
#3188=PLANE('',#62409);
#3189=PLANE('',#62411);
#3190=PLANE('',#62417);
#3191=PLANE('',#62418);
#3192=PLANE('',#62419);
#3193=PLANE('',#62420);
#3194=PLANE('',#62421);
#3195=PLANE('',#62422);
#3196=PLANE('',#62423);
#3197=PLANE('',#62424);
#3198=PLANE('',#62425);
#3199=PLANE('',#62426);
#3200=PLANE('',#62427);
#3201=PLANE('',#62428);
#3202=PLANE('',#62429);
#3203=PLANE('',#62430);
#3204=PLANE('',#62431);
#3205=PLANE('',#62432);
#3206=PLANE('',#62433);
#3207=PLANE('',#62434);
#3208=PLANE('',#62435);
#3209=PLANE('',#62436);
#3210=PLANE('',#62437);
#3211=PLANE('',#62438);
#3212=PLANE('',#62439);
#3213=PLANE('',#62440);
#3214=PLANE('',#62441);
#3215=PLANE('',#62442);
#3216=PLANE('',#62443);
#3217=PLANE('',#62444);
#3218=PLANE('',#62445);
#3219=PLANE('',#62446);
#3220=PLANE('',#62447);
#3221=PLANE('',#62448);
#3222=PLANE('',#62449);
#3223=PLANE('',#62450);
#3224=PLANE('',#62451);
#3225=PLANE('',#62452);
#3226=PLANE('',#62453);
#3227=PLANE('',#62454);
#3228=PLANE('',#62455);
#3229=PLANE('',#62456);
#3230=PLANE('',#62457);
#3231=PLANE('',#62458);
#3232=PLANE('',#62459);
#3233=PLANE('',#62460);
#3234=PLANE('',#62461);
#3235=PLANE('',#62462);
#3236=PLANE('',#62463);
#3237=PLANE('',#62464);
#3238=PLANE('',#62465);
#3239=PLANE('',#62466);
#3240=PLANE('',#62467);
#3241=PLANE('',#62468);
#3242=PLANE('',#62469);
#3243=PLANE('',#62470);
#3244=PLANE('',#62471);
#3245=PLANE('',#62472);
#3246=PLANE('',#62473);
#3247=PLANE('',#62474);
#3248=PLANE('',#62475);
#3249=PLANE('',#62476);
#3250=PLANE('',#62477);
#3251=PLANE('',#62478);
#3252=PLANE('',#62479);
#3253=PLANE('',#62480);
#3254=PLANE('',#62481);
#3255=PLANE('',#62482);
#3256=PLANE('',#62483);
#3257=PLANE('',#62484);
#3258=PLANE('',#62485);
#3259=PLANE('',#62486);
#3260=PLANE('',#62487);
#3261=PLANE('',#62488);
#3262=PLANE('',#62489);
#3263=PLANE('',#62490);
#3264=PLANE('',#62491);
#3265=PLANE('',#62492);
#3266=PLANE('',#62493);
#3267=PLANE('',#62494);
#3268=PLANE('',#62495);
#3269=PLANE('',#62496);
#3270=PLANE('',#62497);
#3271=PLANE('',#62498);
#3272=PLANE('',#62499);
#3273=PLANE('',#62500);
#3274=PLANE('',#62501);
#3275=PLANE('',#62502);
#3276=PLANE('',#62503);
#3277=PLANE('',#62504);
#3278=PLANE('',#62505);
#3279=PLANE('',#62506);
#3280=PLANE('',#62507);
#3281=PLANE('',#62508);
#3282=PLANE('',#62509);
#3283=PLANE('',#62510);
#3284=PLANE('',#62511);
#3285=PLANE('',#62512);
#3286=PLANE('',#62513);
#3287=PLANE('',#62514);
#3288=PLANE('',#62515);
#3289=PLANE('',#62516);
#3290=PLANE('',#62517);
#3291=PLANE('',#62518);
#3292=PLANE('',#62519);
#3293=PLANE('',#62520);
#3294=PLANE('',#62521);
#3295=PLANE('',#62522);
#3296=PLANE('',#62523);
#3297=PLANE('',#62524);
#3298=PLANE('',#62525);
#3299=PLANE('',#62526);
#3300=PLANE('',#62527);
#3301=PLANE('',#62528);
#3302=PLANE('',#62529);
#3303=PLANE('',#62530);
#3304=PLANE('',#62531);
#3305=PLANE('',#62532);
#3306=PLANE('',#62533);
#3307=PLANE('',#62534);
#3308=PLANE('',#62535);
#3309=PLANE('',#62536);
#3310=PLANE('',#62537);
#3311=PLANE('',#62538);
#3312=PLANE('',#62539);
#3313=PLANE('',#62540);
#3314=PLANE('',#62541);
#3315=PLANE('',#62542);
#3316=PLANE('',#62543);
#3317=PLANE('',#62544);
#3318=PLANE('',#62545);
#3319=PLANE('',#62546);
#3320=PLANE('',#62547);
#3321=PLANE('',#62548);
#3322=PLANE('',#62549);
#3323=PLANE('',#62550);
#3324=PLANE('',#62551);
#3325=PLANE('',#62552);
#3326=PLANE('',#62553);
#3327=PLANE('',#62554);
#3328=PLANE('',#62555);
#3329=PLANE('',#62556);
#3330=PLANE('',#62557);
#3331=PLANE('',#62558);
#3332=PLANE('',#62559);
#3333=PLANE('',#62560);
#3334=PLANE('',#62561);
#3335=PLANE('',#62562);
#3336=PLANE('',#62563);
#3337=PLANE('',#62564);
#3338=PLANE('',#62565);
#3339=PLANE('',#62566);
#3340=PLANE('',#62567);
#3341=PLANE('',#62568);
#3342=PLANE('',#62569);
#3343=PLANE('',#62570);
#3344=PLANE('',#62571);
#3345=PLANE('',#62572);
#3346=PLANE('',#62573);
#3347=PLANE('',#62574);
#3348=PLANE('',#62575);
#3349=PLANE('',#62576);
#3350=PLANE('',#62577);
#3351=PLANE('',#62578);
#3352=PLANE('',#62579);
#3353=PLANE('',#62580);
#3354=PLANE('',#62581);
#3355=PLANE('',#62582);
#3356=PLANE('',#62583);
#3357=PLANE('',#62584);
#3358=PLANE('',#62585);
#3359=PLANE('',#62586);
#3360=PLANE('',#62587);
#3361=PLANE('',#62588);
#3362=PLANE('',#62589);
#3363=PLANE('',#62590);
#3364=PLANE('',#62591);
#3365=PLANE('',#62592);
#3366=PLANE('',#62593);
#3367=PLANE('',#62594);
#3368=PLANE('',#62595);
#3369=PLANE('',#62596);
#3370=PLANE('',#62597);
#3371=PLANE('',#62598);
#3372=PLANE('',#62599);
#3373=PLANE('',#62600);
#3374=PLANE('',#62601);
#3375=PLANE('',#62602);
#3376=PLANE('',#62603);
#3377=PLANE('',#62604);
#3378=PLANE('',#62605);
#3379=PLANE('',#62606);
#3380=PLANE('',#62607);
#3381=PLANE('',#62608);
#3382=PLANE('',#62609);
#3383=PLANE('',#62610);
#3384=PLANE('',#62611);
#3385=PLANE('',#62612);
#3386=PLANE('',#62613);
#3387=PLANE('',#62614);
#3388=PLANE('',#62615);
#3389=PLANE('',#62616);
#3390=PLANE('',#62617);
#3391=PLANE('',#62618);
#3392=PLANE('',#62619);
#3393=PLANE('',#62620);
#3394=PLANE('',#62621);
#3395=PLANE('',#62622);
#3396=PLANE('',#62623);
#3397=PLANE('',#62624);
#3398=PLANE('',#62625);
#3399=PLANE('',#62626);
#3400=PLANE('',#62627);
#3401=PLANE('',#62628);
#3402=PLANE('',#62629);
#3403=PLANE('',#62630);
#3404=PLANE('',#62631);
#3405=PLANE('',#62632);
#3406=PLANE('',#62633);
#3407=PLANE('',#62634);
#3408=PLANE('',#62635);
#3409=PLANE('',#62636);
#3410=PLANE('',#62637);
#3411=PLANE('',#62638);
#3412=PLANE('',#62639);
#3413=PLANE('',#62640);
#3414=PLANE('',#62641);
#3415=PLANE('',#62642);
#3416=PLANE('',#62643);
#3417=PLANE('',#62644);
#3418=PLANE('',#62645);
#3419=PLANE('',#62646);
#3420=PLANE('',#62647);
#3421=PLANE('',#62648);
#3422=PLANE('',#62649);
#3423=PLANE('',#62650);
#3424=PLANE('',#62651);
#3425=PLANE('',#62652);
#3426=PLANE('',#62653);
#3427=PLANE('',#62654);
#3428=PLANE('',#62655);
#3429=PLANE('',#62656);
#3430=PLANE('',#62657);
#3431=PLANE('',#62658);
#3432=PLANE('',#62659);
#3433=PLANE('',#62660);
#3434=PLANE('',#62661);
#3435=PLANE('',#62662);
#3436=PLANE('',#62663);
#3437=PLANE('',#62664);
#3438=PLANE('',#62665);
#3439=PLANE('',#62666);
#3440=PLANE('',#62667);
#3441=PLANE('',#62668);
#3442=PLANE('',#62669);
#3443=PLANE('',#62670);
#3444=PLANE('',#62671);
#3445=PLANE('',#62672);
#3446=PLANE('',#62673);
#3447=PLANE('',#62674);
#3448=PLANE('',#62675);
#3449=PLANE('',#62676);
#3450=PLANE('',#62677);
#3451=PLANE('',#62678);
#3452=PLANE('',#62679);
#3453=PLANE('',#62680);
#3454=PLANE('',#62681);
#3455=PLANE('',#62682);
#3456=PLANE('',#62683);
#3457=PLANE('',#62684);
#3458=PLANE('',#62685);
#3459=PLANE('',#62686);
#3460=PLANE('',#62687);
#3461=PLANE('',#62688);
#3462=PLANE('',#62689);
#3463=PLANE('',#62690);
#3464=PLANE('',#62691);
#3465=PLANE('',#62692);
#3466=PLANE('',#62693);
#3467=PLANE('',#62694);
#3468=PLANE('',#62695);
#3469=PLANE('',#62696);
#3470=PLANE('',#62697);
#3471=PLANE('',#62698);
#3472=PLANE('',#62699);
#3473=PLANE('',#62700);
#3474=PLANE('',#62701);
#3475=PLANE('',#62702);
#3476=PLANE('',#62703);
#3477=PLANE('',#62704);
#3478=PLANE('',#62705);
#3479=PLANE('',#62706);
#3480=PLANE('',#62707);
#3481=PLANE('',#62708);
#3482=PLANE('',#62709);
#3483=PLANE('',#62710);
#3484=PLANE('',#62711);
#3485=PLANE('',#62712);
#3486=PLANE('',#62713);
#3487=PLANE('',#62714);
#3488=PLANE('',#62715);
#3489=PLANE('',#62716);
#3490=PLANE('',#62717);
#3491=PLANE('',#62718);
#3492=PLANE('',#62719);
#3493=PLANE('',#62720);
#3494=PLANE('',#62721);
#3495=PLANE('',#62722);
#3496=PLANE('',#62723);
#3497=PLANE('',#62724);
#3498=PLANE('',#62725);
#3499=PLANE('',#62726);
#3500=PLANE('',#62727);
#3501=PLANE('',#62728);
#3502=PLANE('',#62729);
#3503=PLANE('',#62730);
#3504=PLANE('',#62731);
#3505=PLANE('',#62732);
#3506=PLANE('',#62733);
#3507=PLANE('',#62734);
#3508=PLANE('',#62735);
#3509=PLANE('',#62736);
#3510=PLANE('',#62737);
#3511=PLANE('',#62738);
#3512=PLANE('',#62739);
#3513=PLANE('',#62740);
#3514=PLANE('',#62741);
#3515=PLANE('',#62742);
#3516=PLANE('',#62743);
#3517=PLANE('',#62744);
#3518=PLANE('',#62745);
#3519=PLANE('',#62746);
#3520=PLANE('',#62747);
#3521=PLANE('',#62748);
#3522=PLANE('',#62749);
#3523=PLANE('',#62750);
#3524=PLANE('',#62751);
#3525=PLANE('',#62752);
#3526=PLANE('',#62753);
#3527=PLANE('',#62754);
#3528=PLANE('',#62755);
#3529=PLANE('',#62756);
#3530=PLANE('',#62757);
#3531=PLANE('',#62758);
#3532=PLANE('',#62759);
#3533=PLANE('',#62760);
#3534=PLANE('',#62761);
#3535=PLANE('',#62762);
#3536=PLANE('',#62763);
#3537=PLANE('',#62764);
#3538=PLANE('',#62765);
#3539=PLANE('',#62766);
#3540=PLANE('',#62767);
#3541=PLANE('',#62768);
#3542=PLANE('',#62769);
#3543=PLANE('',#62770);
#3544=PLANE('',#62771);
#3545=PLANE('',#62772);
#3546=PLANE('',#62773);
#3547=PLANE('',#62774);
#3548=PLANE('',#62775);
#3549=PLANE('',#62776);
#3550=PLANE('',#62777);
#3551=PLANE('',#62778);
#3552=PLANE('',#62779);
#3553=PLANE('',#62780);
#3554=PLANE('',#62781);
#3555=PLANE('',#62782);
#3556=PLANE('',#62783);
#3557=PLANE('',#62784);
#3558=PLANE('',#62785);
#3559=PLANE('',#62786);
#3560=PLANE('',#62787);
#3561=PLANE('',#62788);
#3562=PLANE('',#62789);
#3563=PLANE('',#62790);
#3564=PLANE('',#62791);
#3565=PLANE('',#62792);
#3566=PLANE('',#62793);
#3567=PLANE('',#62794);
#3568=PLANE('',#62795);
#3569=PLANE('',#62796);
#3570=PLANE('',#62797);
#3571=PLANE('',#62798);
#3572=PLANE('',#62799);
#3573=PLANE('',#62800);
#3574=PLANE('',#62801);
#3575=PLANE('',#62802);
#3576=PLANE('',#62803);
#3577=PLANE('',#62804);
#3578=PLANE('',#62805);
#3579=PLANE('',#62806);
#3580=PLANE('',#62807);
#3581=PLANE('',#62808);
#3582=PLANE('',#62809);
#3583=PLANE('',#62810);
#3584=PLANE('',#62811);
#3585=PLANE('',#62812);
#3586=PLANE('',#62813);
#3587=PLANE('',#62814);
#3588=PLANE('',#62815);
#3589=PLANE('',#62816);
#3590=PLANE('',#62817);
#3591=PLANE('',#62818);
#3592=PLANE('',#62819);
#3593=PLANE('',#62820);
#3594=PLANE('',#62821);
#3595=PLANE('',#62822);
#3596=PLANE('',#62823);
#3597=PLANE('',#62824);
#3598=PLANE('',#62825);
#3599=PLANE('',#62826);
#3600=PLANE('',#62827);
#3601=PLANE('',#62828);
#3602=PLANE('',#62829);
#3603=PLANE('',#62830);
#3604=PLANE('',#62831);
#3605=PLANE('',#62832);
#3606=PLANE('',#62833);
#3607=PLANE('',#62834);
#3608=PLANE('',#62835);
#3609=PLANE('',#62836);
#3610=PLANE('',#62837);
#3611=PLANE('',#62838);
#3612=PLANE('',#62839);
#3613=PLANE('',#62840);
#3614=PLANE('',#62841);
#3615=PLANE('',#62842);
#3616=PLANE('',#62843);
#3617=PLANE('',#62844);
#3618=PLANE('',#62845);
#3619=PLANE('',#62846);
#3620=PLANE('',#62847);
#3621=PLANE('',#62848);
#3622=PLANE('',#62849);
#3623=PLANE('',#62850);
#3624=PLANE('',#62851);
#3625=PLANE('',#62852);
#3626=PLANE('',#62853);
#3627=PLANE('',#62854);
#3628=PLANE('',#62855);
#3629=PLANE('',#62856);
#3630=PLANE('',#62857);
#3631=PLANE('',#62858);
#3632=PLANE('',#62859);
#3633=PLANE('',#62860);
#3634=PLANE('',#62861);
#3635=PLANE('',#62862);
#3636=PLANE('',#62863);
#3637=PLANE('',#62864);
#3638=PLANE('',#62865);
#3639=PLANE('',#62866);
#3640=PLANE('',#62867);
#3641=PLANE('',#62868);
#3642=PLANE('',#62869);
#3643=PLANE('',#62870);
#3644=PLANE('',#62871);
#3645=PLANE('',#62872);
#3646=PLANE('',#62873);
#3647=PLANE('',#62874);
#3648=PLANE('',#62875);
#3649=PLANE('',#62876);
#3650=PLANE('',#62877);
#3651=PLANE('',#62878);
#3652=PLANE('',#62879);
#3653=PLANE('',#62880);
#3654=PLANE('',#62881);
#3655=PLANE('',#62882);
#3656=PLANE('',#62883);
#3657=PLANE('',#62884);
#3658=PLANE('',#62885);
#3659=PLANE('',#62886);
#3660=PLANE('',#62887);
#3661=PLANE('',#62888);
#3662=PLANE('',#62889);
#3663=PLANE('',#62890);
#3664=PLANE('',#62891);
#3665=PLANE('',#62892);
#3666=PLANE('',#62893);
#3667=PLANE('',#62894);
#3668=PLANE('',#62895);
#3669=PLANE('',#62896);
#3670=PLANE('',#62897);
#3671=PLANE('',#62898);
#3672=PLANE('',#62899);
#3673=PLANE('',#62900);
#3674=PLANE('',#62901);
#3675=PLANE('',#62902);
#3676=PLANE('',#62903);
#3677=PLANE('',#62904);
#3678=PLANE('',#62905);
#3679=PLANE('',#62906);
#3680=PLANE('',#62907);
#3681=PLANE('',#62908);
#3682=PLANE('',#62909);
#3683=PLANE('',#62910);
#3684=PLANE('',#62911);
#3685=PLANE('',#62912);
#3686=PLANE('',#62913);
#3687=PLANE('',#62914);
#3688=PLANE('',#62915);
#3689=PLANE('',#62916);
#3690=PLANE('',#62917);
#3691=PLANE('',#62918);
#3692=PLANE('',#62919);
#3693=PLANE('',#62920);
#3694=PLANE('',#62921);
#3695=PLANE('',#62922);
#3696=PLANE('',#62933);
#3697=PLANE('',#62937);
#3698=PLANE('',#62938);
#3699=PLANE('',#62942);
#3700=PLANE('',#62947);
#3701=PLANE('',#62948);
#3702=PLANE('',#62949);
#3703=PLANE('',#62950);
#3704=PLANE('',#62951);
#3705=PLANE('',#62952);
#3706=PLANE('',#62955);
#3707=PLANE('',#62956);
#3708=PLANE('',#62958);
#3709=PLANE('',#62959);
#3710=PLANE('',#62960);
#3711=PLANE('',#62961);
#3712=PLANE('',#62962);
#3713=PLANE('',#62963);
#3714=PLANE('',#62964);
#3715=PLANE('',#62965);
#3716=PLANE('',#62966);
#3717=PLANE('',#62967);
#3718=PLANE('',#62968);
#3719=PLANE('',#62969);
#3720=PLANE('',#62970);
#3721=PLANE('',#62971);
#3722=PLANE('',#62972);
#3723=PLANE('',#62973);
#3724=PLANE('',#62974);
#3725=PLANE('',#62975);
#3726=PLANE('',#62976);
#3727=PLANE('',#62977);
#3728=PLANE('',#62978);
#3729=PLANE('',#62979);
#3730=PLANE('',#62980);
#3731=PLANE('',#62981);
#3732=PLANE('',#62982);
#3733=PLANE('',#62983);
#3734=PLANE('',#62984);
#3735=PLANE('',#62985);
#3736=PLANE('',#62986);
#3737=PLANE('',#62987);
#3738=PLANE('',#62988);
#3739=PLANE('',#62989);
#3740=PLANE('',#62990);
#3741=PLANE('',#62991);
#3742=PLANE('',#62992);
#3743=PLANE('',#62994);
#3744=PLANE('',#62995);
#3745=PLANE('',#62996);
#3746=PLANE('',#62997);
#3747=PLANE('',#62998);
#3748=PLANE('',#62999);
#3749=PLANE('',#63000);
#3750=PLANE('',#63001);
#3751=PLANE('',#63002);
#3752=PLANE('',#63003);
#3753=PLANE('',#63004);
#3754=PLANE('',#63005);
#3755=PLANE('',#63006);
#3756=PLANE('',#63007);
#3757=PLANE('',#63008);
#3758=PLANE('',#63009);
#3759=PLANE('',#63010);
#3760=PLANE('',#63011);
#3761=PLANE('',#63012);
#3762=PLANE('',#63013);
#3763=PLANE('',#63014);
#3764=PLANE('',#63015);
#3765=PLANE('',#63016);
#3766=PLANE('',#63017);
#3767=PLANE('',#63018);
#3768=PLANE('',#63019);
#3769=PLANE('',#63020);
#3770=PLANE('',#63021);
#3771=PLANE('',#63022);
#3772=PLANE('',#63023);
#3773=PLANE('',#63024);
#3774=PLANE('',#63026);
#3775=PLANE('',#63028);
#3776=PLANE('',#63030);
#3777=PLANE('',#63038);
#3778=PLANE('',#63040);
#3779=PLANE('',#63048);
#3780=PLANE('',#63052);
#3781=PLANE('',#63055);
#3782=PLANE('',#63056);
#3783=PLANE('',#63057);
#3784=PLANE('',#63082);
#3785=PLANE('',#63085);
#3786=PLANE('',#63093);
#3787=PLANE('',#63097);
#3788=PLANE('',#63098);
#3789=PLANE('',#63099);
#3790=PLANE('',#63109);
#3791=PLANE('',#63110);
#3792=PLANE('',#63114);
#3793=PLANE('',#63127);
#3794=PLANE('',#63130);
#3795=PLANE('',#63155);
#3796=PLANE('',#63156);
#3797=PLANE('',#63157);
#3798=PLANE('',#63158);
#3799=PLANE('',#63159);
#3800=PLANE('',#63160);
#3801=PLANE('',#63161);
#3802=PLANE('',#63162);
#3803=PLANE('',#63163);
#3804=PLANE('',#63164);
#3805=PLANE('',#63166);
#3806=PLANE('',#63168);
#3807=PLANE('',#63170);
#3808=PLANE('',#63172);
#3809=PLANE('',#63174);
#3810=PLANE('',#63177);
#3811=PLANE('',#63178);
#3812=PLANE('',#63179);
#3813=PLANE('',#63180);
#3814=PLANE('',#63187);
#3815=PLANE('',#63199);
#3816=PLANE('',#63201);
#3817=PLANE('',#63226);
#3818=PLANE('',#63227);
#3819=PLANE('',#63228);
#3820=PLANE('',#63229);
#3821=PLANE('',#63230);
#3822=PLANE('',#63231);
#3823=PLANE('',#63232);
#3824=PLANE('',#63233);
#3825=PLANE('',#63234);
#3826=PLANE('',#63235);
#3827=PLANE('',#63237);
#3828=PLANE('',#63239);
#3829=PLANE('',#63241);
#3830=PLANE('',#63243);
#3831=PLANE('',#63245);
#3832=PLANE('',#63248);
#3833=PLANE('',#63249);
#3834=PLANE('',#63250);
#3835=PLANE('',#63251);
#3836=PLANE('',#63258);
#3837=PLANE('',#63283);
#3838=PLANE('',#63286);
#3839=PLANE('',#63311);
#3840=PLANE('',#63312);
#3841=PLANE('',#63313);
#3842=PLANE('',#63314);
#3843=PLANE('',#63315);
#3844=PLANE('',#63316);
#3845=PLANE('',#63317);
#3846=PLANE('',#63318);
#3847=PLANE('',#63319);
#3848=PLANE('',#63320);
#3849=PLANE('',#63322);
#3850=PLANE('',#63324);
#3851=PLANE('',#63326);
#3852=PLANE('',#63328);
#3853=PLANE('',#63330);
#3854=PLANE('',#63333);
#3855=PLANE('',#63334);
#3856=PLANE('',#63335);
#3857=PLANE('',#63336);
#3858=PLANE('',#63343);
#3859=PLANE('',#63360);
#3860=PLANE('',#63363);
#3861=PLANE('',#63388);
#3862=PLANE('',#63389);
#3863=PLANE('',#63390);
#3864=PLANE('',#63391);
#3865=PLANE('',#63392);
#3866=PLANE('',#63393);
#3867=PLANE('',#63394);
#3868=PLANE('',#63395);
#3869=PLANE('',#63396);
#3870=PLANE('',#63397);
#3871=PLANE('',#63399);
#3872=PLANE('',#63401);
#3873=PLANE('',#63403);
#3874=PLANE('',#63405);
#3875=PLANE('',#63407);
#3876=PLANE('',#63410);
#3877=PLANE('',#63411);
#3878=PLANE('',#63412);
#3879=PLANE('',#63413);
#3880=PLANE('',#63420);
#3881=PLANE('',#63440);
#3882=PLANE('',#63442);
#3883=PLANE('',#63447);
#3884=PLANE('',#63448);
#3885=PLANE('',#63449);
#3886=PLANE('',#63450);
#3887=PLANE('',#63451);
#3888=PLANE('',#63452);
#3889=PLANE('',#63453);
#3890=PLANE('',#63454);
#3891=PLANE('',#63461);
#3892=PLANE('',#63490);
#3893=PLANE('',#63493);
#3894=PLANE('',#63503);
#3895=PLANE('',#63507);
#3896=PLANE('',#63508);
#3897=PLANE('',#63509);
#3898=PLANE('',#63511);
#3899=PLANE('',#63587);
#3900=PLANE('',#63588);
#3901=PLANE('',#63589);
#3902=PLANE('',#63590);
#3903=PLANE('',#63591);
#3904=PLANE('',#63592);
#3905=PLANE('',#63593);
#3906=PLANE('',#63594);
#3907=PLANE('',#63595);
#3908=PLANE('',#63596);
#3909=PLANE('',#63597);
#3910=PLANE('',#63598);
#3911=PLANE('',#63599);
#3912=PLANE('',#63600);
#3913=PLANE('',#63601);
#3914=PLANE('',#63602);
#3915=PLANE('',#63603);
#3916=PLANE('',#63604);
#3917=PLANE('',#63605);
#3918=PLANE('',#63606);
#3919=PLANE('',#63607);
#3920=PLANE('',#63608);
#3921=PLANE('',#63609);
#3922=PLANE('',#63610);
#3923=PLANE('',#63611);
#3924=PLANE('',#63612);
#3925=PLANE('',#63613);
#3926=PLANE('',#63614);
#3927=PLANE('',#63615);
#3928=PLANE('',#63616);
#3929=PLANE('',#63617);
#3930=PLANE('',#63618);
#3931=PLANE('',#63619);
#3932=PLANE('',#63620);
#3933=PLANE('',#63621);
#3934=PLANE('',#63622);
#3935=PLANE('',#63623);
#3936=PLANE('',#63624);
#3937=PLANE('',#63625);
#3938=PLANE('',#63626);
#3939=PLANE('',#63627);
#3940=PLANE('',#63628);
#3941=PLANE('',#63629);
#3942=PLANE('',#63630);
#3943=PLANE('',#63631);
#3944=PLANE('',#63632);
#3945=PLANE('',#63633);
#3946=PLANE('',#63634);
#3947=PLANE('',#63635);
#3948=PLANE('',#63636);
#3949=PLANE('',#63637);
#3950=PLANE('',#63638);
#3951=PLANE('',#63639);
#3952=PLANE('',#63640);
#3953=PLANE('',#63641);
#3954=PLANE('',#63642);
#3955=PLANE('',#63643);
#3956=PLANE('',#63644);
#3957=PLANE('',#63645);
#3958=PLANE('',#63646);
#3959=PLANE('',#63647);
#3960=PLANE('',#63648);
#3961=PLANE('',#63649);
#3962=PLANE('',#63650);
#3963=PLANE('',#63651);
#3964=PLANE('',#63652);
#3965=PLANE('',#63653);
#3966=PLANE('',#63654);
#3967=PLANE('',#63655);
#3968=PLANE('',#63656);
#3969=PLANE('',#63657);
#3970=PLANE('',#63658);
#3971=PLANE('',#63659);
#3972=PLANE('',#63660);
#3973=PLANE('',#63661);
#3974=PLANE('',#63662);
#3975=PLANE('',#63663);
#3976=PLANE('',#63664);
#3977=PLANE('',#63665);
#3978=PLANE('',#63666);
#3979=PLANE('',#63667);
#3980=PLANE('',#63668);
#3981=PLANE('',#63669);
#3982=PLANE('',#63670);
#3983=PLANE('',#63671);
#3984=PLANE('',#63672);
#3985=PLANE('',#63673);
#3986=PLANE('',#63674);
#3987=PLANE('',#63675);
#3988=PLANE('',#63676);
#3989=PLANE('',#63677);
#3990=PLANE('',#63678);
#3991=PLANE('',#63679);
#3992=PLANE('',#63680);
#3993=PLANE('',#63681);
#3994=PLANE('',#63682);
#3995=PLANE('',#63683);
#3996=PLANE('',#63684);
#3997=PLANE('',#63685);
#3998=PLANE('',#63686);
#3999=PLANE('',#63687);
#4000=PLANE('',#63688);
#4001=PLANE('',#63689);
#4002=PLANE('',#63690);
#4003=PLANE('',#63691);
#4004=PLANE('',#63696);
#4005=PLANE('',#63717);
#4006=PLANE('',#63718);
#4007=PLANE('',#63719);
#4008=PLANE('',#63720);
#4009=PLANE('',#63721);
#4010=PLANE('',#63722);
#4011=PLANE('',#63723);
#4012=PLANE('',#63724);
#4013=PLANE('',#63725);
#4014=PLANE('',#63726);
#4015=PLANE('',#63728);
#4016=PLANE('',#63730);
#4017=PLANE('',#63732);
#4018=PLANE('',#63734);
#4019=PLANE('',#63736);
#4020=PLANE('',#63739);
#4021=PLANE('',#63740);
#4022=PLANE('',#63741);
#4023=PLANE('',#63743);
#4024=PLANE('',#63751);
#4025=FACE_OUTER_BOUND('',#7292,.T.);
#4026=FACE_OUTER_BOUND('',#7293,.T.);
#4027=FACE_OUTER_BOUND('',#7294,.T.);
#4028=FACE_OUTER_BOUND('',#7295,.T.);
#4029=FACE_OUTER_BOUND('',#7296,.T.);
#4030=FACE_OUTER_BOUND('',#7297,.T.);
#4031=FACE_OUTER_BOUND('',#7298,.T.);
#4032=FACE_OUTER_BOUND('',#7299,.T.);
#4033=FACE_OUTER_BOUND('',#7300,.T.);
#4034=FACE_OUTER_BOUND('',#7301,.T.);
#4035=FACE_OUTER_BOUND('',#7302,.T.);
#4036=FACE_OUTER_BOUND('',#7303,.T.);
#4037=FACE_OUTER_BOUND('',#7304,.T.);
#4038=FACE_OUTER_BOUND('',#7305,.T.);
#4039=FACE_OUTER_BOUND('',#7306,.T.);
#4040=FACE_OUTER_BOUND('',#7307,.T.);
#4041=FACE_OUTER_BOUND('',#7308,.T.);
#4042=FACE_OUTER_BOUND('',#7309,.T.);
#4043=FACE_OUTER_BOUND('',#7310,.T.);
#4044=FACE_OUTER_BOUND('',#7311,.T.);
#4045=FACE_OUTER_BOUND('',#7312,.T.);
#4046=FACE_OUTER_BOUND('',#7314,.T.);
#4047=FACE_OUTER_BOUND('',#7315,.T.);
#4048=FACE_OUTER_BOUND('',#7316,.T.);
#4049=FACE_OUTER_BOUND('',#7317,.T.);
#4050=FACE_OUTER_BOUND('',#7318,.T.);
#4051=FACE_OUTER_BOUND('',#7319,.T.);
#4052=FACE_OUTER_BOUND('',#7320,.T.);
#4053=FACE_OUTER_BOUND('',#7321,.T.);
#4054=FACE_OUTER_BOUND('',#7322,.T.);
#4055=FACE_OUTER_BOUND('',#7323,.T.);
#4056=FACE_OUTER_BOUND('',#7324,.T.);
#4057=FACE_OUTER_BOUND('',#7325,.T.);
#4058=FACE_OUTER_BOUND('',#7326,.T.);
#4059=FACE_OUTER_BOUND('',#7327,.T.);
#4060=FACE_OUTER_BOUND('',#7328,.T.);
#4061=FACE_OUTER_BOUND('',#7329,.T.);
#4062=FACE_OUTER_BOUND('',#7330,.T.);
#4063=FACE_OUTER_BOUND('',#7331,.T.);
#4064=FACE_OUTER_BOUND('',#7332,.T.);
#4065=FACE_OUTER_BOUND('',#7333,.T.);
#4066=FACE_OUTER_BOUND('',#7334,.T.);
#4067=FACE_OUTER_BOUND('',#7335,.T.);
#4068=FACE_OUTER_BOUND('',#7336,.T.);
#4069=FACE_OUTER_BOUND('',#7337,.T.);
#4070=FACE_OUTER_BOUND('',#7338,.T.);
#4071=FACE_OUTER_BOUND('',#7339,.T.);
#4072=FACE_OUTER_BOUND('',#7340,.T.);
#4073=FACE_OUTER_BOUND('',#7341,.T.);
#4074=FACE_OUTER_BOUND('',#7342,.T.);
#4075=FACE_OUTER_BOUND('',#7343,.T.);
#4076=FACE_OUTER_BOUND('',#7344,.T.);
#4077=FACE_OUTER_BOUND('',#7346,.T.);
#4078=FACE_OUTER_BOUND('',#7347,.T.);
#4079=FACE_OUTER_BOUND('',#7348,.T.);
#4080=FACE_OUTER_BOUND('',#7349,.T.);
#4081=FACE_OUTER_BOUND('',#7350,.T.);
#4082=FACE_OUTER_BOUND('',#7351,.T.);
#4083=FACE_OUTER_BOUND('',#7352,.T.);
#4084=FACE_OUTER_BOUND('',#7353,.T.);
#4085=FACE_OUTER_BOUND('',#7354,.T.);
#4086=FACE_OUTER_BOUND('',#7355,.T.);
#4087=FACE_OUTER_BOUND('',#7356,.T.);
#4088=FACE_OUTER_BOUND('',#7357,.T.);
#4089=FACE_OUTER_BOUND('',#7358,.T.);
#4090=FACE_OUTER_BOUND('',#7359,.T.);
#4091=FACE_OUTER_BOUND('',#7360,.T.);
#4092=FACE_OUTER_BOUND('',#7361,.T.);
#4093=FACE_OUTER_BOUND('',#7362,.T.);
#4094=FACE_OUTER_BOUND('',#7363,.T.);
#4095=FACE_OUTER_BOUND('',#7364,.T.);
#4096=FACE_OUTER_BOUND('',#7365,.T.);
#4097=FACE_OUTER_BOUND('',#7366,.T.);
#4098=FACE_OUTER_BOUND('',#7367,.T.);
#4099=FACE_OUTER_BOUND('',#7368,.T.);
#4100=FACE_OUTER_BOUND('',#7370,.T.);
#4101=FACE_OUTER_BOUND('',#7371,.T.);
#4102=FACE_OUTER_BOUND('',#7372,.T.);
#4103=FACE_OUTER_BOUND('',#7373,.T.);
#4104=FACE_OUTER_BOUND('',#7374,.T.);
#4105=FACE_OUTER_BOUND('',#7375,.T.);
#4106=FACE_OUTER_BOUND('',#7376,.T.);
#4107=FACE_OUTER_BOUND('',#7377,.T.);
#4108=FACE_OUTER_BOUND('',#7378,.T.);
#4109=FACE_OUTER_BOUND('',#7379,.T.);
#4110=FACE_OUTER_BOUND('',#7380,.T.);
#4111=FACE_OUTER_BOUND('',#7381,.T.);
#4112=FACE_OUTER_BOUND('',#7382,.T.);
#4113=FACE_OUTER_BOUND('',#7383,.T.);
#4114=FACE_OUTER_BOUND('',#7384,.T.);
#4115=FACE_OUTER_BOUND('',#7385,.T.);
#4116=FACE_OUTER_BOUND('',#7386,.T.);
#4117=FACE_OUTER_BOUND('',#7387,.T.);
#4118=FACE_OUTER_BOUND('',#7388,.T.);
#4119=FACE_OUTER_BOUND('',#7389,.T.);
#4120=FACE_OUTER_BOUND('',#7390,.T.);
#4121=FACE_OUTER_BOUND('',#7391,.T.);
#4122=FACE_OUTER_BOUND('',#7392,.T.);
#4123=FACE_OUTER_BOUND('',#7393,.T.);
#4124=FACE_OUTER_BOUND('',#7394,.T.);
#4125=FACE_OUTER_BOUND('',#7395,.T.);
#4126=FACE_OUTER_BOUND('',#7396,.T.);
#4127=FACE_OUTER_BOUND('',#7397,.T.);
#4128=FACE_OUTER_BOUND('',#7398,.T.);
#4129=FACE_OUTER_BOUND('',#7399,.T.);
#4130=FACE_OUTER_BOUND('',#7400,.T.);
#4131=FACE_OUTER_BOUND('',#7401,.T.);
#4132=FACE_OUTER_BOUND('',#7402,.T.);
#4133=FACE_OUTER_BOUND('',#7403,.T.);
#4134=FACE_OUTER_BOUND('',#7406,.T.);
#4135=FACE_OUTER_BOUND('',#7407,.T.);
#4136=FACE_OUTER_BOUND('',#7408,.T.);
#4137=FACE_OUTER_BOUND('',#7409,.T.);
#4138=FACE_OUTER_BOUND('',#7410,.T.);
#4139=FACE_OUTER_BOUND('',#7411,.T.);
#4140=FACE_OUTER_BOUND('',#7412,.T.);
#4141=FACE_OUTER_BOUND('',#7413,.T.);
#4142=FACE_OUTER_BOUND('',#7414,.T.);
#4143=FACE_OUTER_BOUND('',#7415,.T.);
#4144=FACE_OUTER_BOUND('',#7416,.T.);
#4145=FACE_OUTER_BOUND('',#7417,.T.);
#4146=FACE_OUTER_BOUND('',#7418,.T.);
#4147=FACE_OUTER_BOUND('',#7419,.T.);
#4148=FACE_OUTER_BOUND('',#7420,.T.);
#4149=FACE_OUTER_BOUND('',#7421,.T.);
#4150=FACE_OUTER_BOUND('',#7422,.T.);
#4151=FACE_OUTER_BOUND('',#7423,.T.);
#4152=FACE_OUTER_BOUND('',#7424,.T.);
#4153=FACE_OUTER_BOUND('',#7425,.T.);
#4154=FACE_OUTER_BOUND('',#7426,.T.);
#4155=FACE_OUTER_BOUND('',#7427,.T.);
#4156=FACE_OUTER_BOUND('',#7428,.T.);
#4157=FACE_OUTER_BOUND('',#7429,.T.);
#4158=FACE_OUTER_BOUND('',#7431,.T.);
#4159=FACE_OUTER_BOUND('',#7432,.T.);
#4160=FACE_OUTER_BOUND('',#7433,.T.);
#4161=FACE_OUTER_BOUND('',#7434,.T.);
#4162=FACE_OUTER_BOUND('',#7435,.T.);
#4163=FACE_OUTER_BOUND('',#7436,.T.);
#4164=FACE_OUTER_BOUND('',#7437,.T.);
#4165=FACE_OUTER_BOUND('',#7438,.T.);
#4166=FACE_OUTER_BOUND('',#7439,.T.);
#4167=FACE_OUTER_BOUND('',#7440,.T.);
#4168=FACE_OUTER_BOUND('',#7441,.T.);
#4169=FACE_OUTER_BOUND('',#7442,.T.);
#4170=FACE_OUTER_BOUND('',#7443,.T.);
#4171=FACE_OUTER_BOUND('',#7444,.T.);
#4172=FACE_OUTER_BOUND('',#7445,.T.);
#4173=FACE_OUTER_BOUND('',#7446,.T.);
#4174=FACE_OUTER_BOUND('',#7447,.T.);
#4175=FACE_OUTER_BOUND('',#7448,.T.);
#4176=FACE_OUTER_BOUND('',#7449,.T.);
#4177=FACE_OUTER_BOUND('',#7450,.T.);
#4178=FACE_OUTER_BOUND('',#7451,.T.);
#4179=FACE_OUTER_BOUND('',#7452,.T.);
#4180=FACE_OUTER_BOUND('',#7453,.T.);
#4181=FACE_OUTER_BOUND('',#7454,.T.);
#4182=FACE_OUTER_BOUND('',#7455,.T.);
#4183=FACE_OUTER_BOUND('',#7456,.T.);
#4184=FACE_OUTER_BOUND('',#7457,.T.);
#4185=FACE_OUTER_BOUND('',#7458,.T.);
#4186=FACE_OUTER_BOUND('',#7459,.T.);
#4187=FACE_OUTER_BOUND('',#7460,.T.);
#4188=FACE_OUTER_BOUND('',#7461,.T.);
#4189=FACE_OUTER_BOUND('',#7462,.T.);
#4190=FACE_OUTER_BOUND('',#7463,.T.);
#4191=FACE_OUTER_BOUND('',#7464,.T.);
#4192=FACE_OUTER_BOUND('',#7466,.T.);
#4193=FACE_OUTER_BOUND('',#7467,.T.);
#4194=FACE_OUTER_BOUND('',#7468,.T.);
#4195=FACE_OUTER_BOUND('',#7469,.T.);
#4196=FACE_OUTER_BOUND('',#7470,.T.);
#4197=FACE_OUTER_BOUND('',#7471,.T.);
#4198=FACE_OUTER_BOUND('',#7472,.T.);
#4199=FACE_OUTER_BOUND('',#7473,.T.);
#4200=FACE_OUTER_BOUND('',#7474,.T.);
#4201=FACE_OUTER_BOUND('',#7475,.T.);
#4202=FACE_OUTER_BOUND('',#7476,.T.);
#4203=FACE_OUTER_BOUND('',#7477,.T.);
#4204=FACE_OUTER_BOUND('',#7478,.T.);
#4205=FACE_OUTER_BOUND('',#7479,.T.);
#4206=FACE_OUTER_BOUND('',#7480,.T.);
#4207=FACE_OUTER_BOUND('',#7481,.T.);
#4208=FACE_OUTER_BOUND('',#7482,.T.);
#4209=FACE_OUTER_BOUND('',#7483,.T.);
#4210=FACE_OUTER_BOUND('',#7484,.T.);
#4211=FACE_OUTER_BOUND('',#7485,.T.);
#4212=FACE_OUTER_BOUND('',#7486,.T.);
#4213=FACE_OUTER_BOUND('',#7487,.T.);
#4214=FACE_OUTER_BOUND('',#7488,.T.);
#4215=FACE_OUTER_BOUND('',#7489,.T.);
#4216=FACE_OUTER_BOUND('',#7490,.T.);
#4217=FACE_OUTER_BOUND('',#7491,.T.);
#4218=FACE_OUTER_BOUND('',#7492,.T.);
#4219=FACE_OUTER_BOUND('',#7493,.T.);
#4220=FACE_OUTER_BOUND('',#7494,.T.);
#4221=FACE_OUTER_BOUND('',#7496,.T.);
#4222=FACE_OUTER_BOUND('',#7497,.T.);
#4223=FACE_OUTER_BOUND('',#7498,.T.);
#4224=FACE_OUTER_BOUND('',#7499,.T.);
#4225=FACE_OUTER_BOUND('',#7500,.T.);
#4226=FACE_OUTER_BOUND('',#7501,.T.);
#4227=FACE_OUTER_BOUND('',#7502,.T.);
#4228=FACE_OUTER_BOUND('',#7503,.T.);
#4229=FACE_OUTER_BOUND('',#7504,.T.);
#4230=FACE_OUTER_BOUND('',#7505,.T.);
#4231=FACE_OUTER_BOUND('',#7506,.T.);
#4232=FACE_OUTER_BOUND('',#7507,.T.);
#4233=FACE_OUTER_BOUND('',#7508,.T.);
#4234=FACE_OUTER_BOUND('',#7509,.T.);
#4235=FACE_OUTER_BOUND('',#7510,.T.);
#4236=FACE_OUTER_BOUND('',#7511,.T.);
#4237=FACE_OUTER_BOUND('',#7512,.T.);
#4238=FACE_OUTER_BOUND('',#7513,.T.);
#4239=FACE_OUTER_BOUND('',#7514,.T.);
#4240=FACE_OUTER_BOUND('',#7515,.T.);
#4241=FACE_OUTER_BOUND('',#7516,.T.);
#4242=FACE_OUTER_BOUND('',#7517,.T.);
#4243=FACE_OUTER_BOUND('',#7518,.T.);
#4244=FACE_OUTER_BOUND('',#7520,.T.);
#4245=FACE_OUTER_BOUND('',#7521,.T.);
#4246=FACE_OUTER_BOUND('',#7522,.T.);
#4247=FACE_OUTER_BOUND('',#7523,.T.);
#4248=FACE_OUTER_BOUND('',#7524,.T.);
#4249=FACE_OUTER_BOUND('',#7525,.T.);
#4250=FACE_OUTER_BOUND('',#7526,.T.);
#4251=FACE_OUTER_BOUND('',#7527,.T.);
#4252=FACE_OUTER_BOUND('',#7528,.T.);
#4253=FACE_OUTER_BOUND('',#7529,.T.);
#4254=FACE_OUTER_BOUND('',#7530,.T.);
#4255=FACE_OUTER_BOUND('',#7531,.T.);
#4256=FACE_OUTER_BOUND('',#7532,.T.);
#4257=FACE_OUTER_BOUND('',#7533,.T.);
#4258=FACE_OUTER_BOUND('',#7534,.T.);
#4259=FACE_OUTER_BOUND('',#7535,.T.);
#4260=FACE_OUTER_BOUND('',#7536,.T.);
#4261=FACE_OUTER_BOUND('',#7537,.T.);
#4262=FACE_OUTER_BOUND('',#7538,.T.);
#4263=FACE_OUTER_BOUND('',#7539,.T.);
#4264=FACE_OUTER_BOUND('',#7540,.T.);
#4265=FACE_OUTER_BOUND('',#7541,.T.);
#4266=FACE_OUTER_BOUND('',#7542,.T.);
#4267=FACE_OUTER_BOUND('',#7543,.T.);
#4268=FACE_OUTER_BOUND('',#7544,.T.);
#4269=FACE_OUTER_BOUND('',#7545,.T.);
#4270=FACE_OUTER_BOUND('',#7546,.T.);
#4271=FACE_OUTER_BOUND('',#7547,.T.);
#4272=FACE_OUTER_BOUND('',#7548,.T.);
#4273=FACE_OUTER_BOUND('',#7549,.T.);
#4274=FACE_OUTER_BOUND('',#7550,.T.);
#4275=FACE_OUTER_BOUND('',#7551,.T.);
#4276=FACE_OUTER_BOUND('',#7552,.T.);
#4277=FACE_OUTER_BOUND('',#7553,.T.);
#4278=FACE_OUTER_BOUND('',#7554,.T.);
#4279=FACE_OUTER_BOUND('',#7555,.T.);
#4280=FACE_OUTER_BOUND('',#7556,.T.);
#4281=FACE_OUTER_BOUND('',#7557,.T.);
#4282=FACE_OUTER_BOUND('',#7558,.T.);
#4283=FACE_OUTER_BOUND('',#7559,.T.);
#4284=FACE_OUTER_BOUND('',#7560,.T.);
#4285=FACE_OUTER_BOUND('',#7561,.T.);
#4286=FACE_OUTER_BOUND('',#7562,.T.);
#4287=FACE_OUTER_BOUND('',#7563,.T.);
#4288=FACE_OUTER_BOUND('',#7564,.T.);
#4289=FACE_OUTER_BOUND('',#7566,.T.);
#4290=FACE_OUTER_BOUND('',#7567,.T.);
#4291=FACE_OUTER_BOUND('',#7568,.T.);
#4292=FACE_OUTER_BOUND('',#7569,.T.);
#4293=FACE_OUTER_BOUND('',#7570,.T.);
#4294=FACE_OUTER_BOUND('',#7571,.T.);
#4295=FACE_OUTER_BOUND('',#7572,.T.);
#4296=FACE_OUTER_BOUND('',#7573,.T.);
#4297=FACE_OUTER_BOUND('',#7574,.T.);
#4298=FACE_OUTER_BOUND('',#7575,.T.);
#4299=FACE_OUTER_BOUND('',#7576,.T.);
#4300=FACE_OUTER_BOUND('',#7577,.T.);
#4301=FACE_OUTER_BOUND('',#7578,.T.);
#4302=FACE_OUTER_BOUND('',#7579,.T.);
#4303=FACE_OUTER_BOUND('',#7580,.T.);
#4304=FACE_OUTER_BOUND('',#7582,.T.);
#4305=FACE_OUTER_BOUND('',#7583,.T.);
#4306=FACE_OUTER_BOUND('',#7584,.T.);
#4307=FACE_OUTER_BOUND('',#7585,.T.);
#4308=FACE_OUTER_BOUND('',#7586,.T.);
#4309=FACE_OUTER_BOUND('',#7587,.T.);
#4310=FACE_OUTER_BOUND('',#7588,.T.);
#4311=FACE_OUTER_BOUND('',#7589,.T.);
#4312=FACE_OUTER_BOUND('',#7590,.T.);
#4313=FACE_OUTER_BOUND('',#7591,.T.);
#4314=FACE_OUTER_BOUND('',#7592,.T.);
#4315=FACE_OUTER_BOUND('',#7593,.T.);
#4316=FACE_OUTER_BOUND('',#7594,.T.);
#4317=FACE_OUTER_BOUND('',#7595,.T.);
#4318=FACE_OUTER_BOUND('',#7596,.T.);
#4319=FACE_OUTER_BOUND('',#7597,.T.);
#4320=FACE_OUTER_BOUND('',#7598,.T.);
#4321=FACE_OUTER_BOUND('',#7599,.T.);
#4322=FACE_OUTER_BOUND('',#7600,.T.);
#4323=FACE_OUTER_BOUND('',#7601,.T.);
#4324=FACE_OUTER_BOUND('',#7602,.T.);
#4325=FACE_OUTER_BOUND('',#7603,.T.);
#4326=FACE_OUTER_BOUND('',#7604,.T.);
#4327=FACE_OUTER_BOUND('',#7606,.T.);
#4328=FACE_OUTER_BOUND('',#7607,.T.);
#4329=FACE_OUTER_BOUND('',#7608,.T.);
#4330=FACE_OUTER_BOUND('',#7609,.T.);
#4331=FACE_OUTER_BOUND('',#7610,.T.);
#4332=FACE_OUTER_BOUND('',#7611,.T.);
#4333=FACE_OUTER_BOUND('',#7612,.T.);
#4334=FACE_OUTER_BOUND('',#7613,.T.);
#4335=FACE_OUTER_BOUND('',#7614,.T.);
#4336=FACE_OUTER_BOUND('',#7615,.T.);
#4337=FACE_OUTER_BOUND('',#7616,.T.);
#4338=FACE_OUTER_BOUND('',#7617,.T.);
#4339=FACE_OUTER_BOUND('',#7618,.T.);
#4340=FACE_OUTER_BOUND('',#7619,.T.);
#4341=FACE_OUTER_BOUND('',#7620,.T.);
#4342=FACE_OUTER_BOUND('',#7621,.T.);
#4343=FACE_OUTER_BOUND('',#7622,.T.);
#4344=FACE_OUTER_BOUND('',#7623,.T.);
#4345=FACE_OUTER_BOUND('',#7624,.T.);
#4346=FACE_OUTER_BOUND('',#7625,.T.);
#4347=FACE_OUTER_BOUND('',#7626,.T.);
#4348=FACE_OUTER_BOUND('',#7627,.T.);
#4349=FACE_OUTER_BOUND('',#7628,.T.);
#4350=FACE_OUTER_BOUND('',#7629,.T.);
#4351=FACE_OUTER_BOUND('',#7630,.T.);
#4352=FACE_OUTER_BOUND('',#7631,.T.);
#4353=FACE_OUTER_BOUND('',#7632,.T.);
#4354=FACE_OUTER_BOUND('',#7633,.T.);
#4355=FACE_OUTER_BOUND('',#7634,.T.);
#4356=FACE_OUTER_BOUND('',#7635,.T.);
#4357=FACE_OUTER_BOUND('',#7636,.T.);
#4358=FACE_OUTER_BOUND('',#7637,.T.);
#4359=FACE_OUTER_BOUND('',#7638,.T.);
#4360=FACE_OUTER_BOUND('',#7639,.T.);
#4361=FACE_OUTER_BOUND('',#7640,.T.);
#4362=FACE_OUTER_BOUND('',#7641,.T.);
#4363=FACE_OUTER_BOUND('',#7642,.T.);
#4364=FACE_OUTER_BOUND('',#7643,.T.);
#4365=FACE_OUTER_BOUND('',#7644,.T.);
#4366=FACE_OUTER_BOUND('',#7645,.T.);
#4367=FACE_OUTER_BOUND('',#7646,.T.);
#4368=FACE_OUTER_BOUND('',#7647,.T.);
#4369=FACE_OUTER_BOUND('',#7648,.T.);
#4370=FACE_OUTER_BOUND('',#7649,.T.);
#4371=FACE_OUTER_BOUND('',#7650,.T.);
#4372=FACE_OUTER_BOUND('',#7651,.T.);
#4373=FACE_OUTER_BOUND('',#7652,.T.);
#4374=FACE_OUTER_BOUND('',#7653,.T.);
#4375=FACE_OUTER_BOUND('',#7654,.T.);
#4376=FACE_OUTER_BOUND('',#7655,.T.);
#4377=FACE_OUTER_BOUND('',#7656,.T.);
#4378=FACE_OUTER_BOUND('',#7657,.T.);
#4379=FACE_OUTER_BOUND('',#7658,.T.);
#4380=FACE_OUTER_BOUND('',#7660,.T.);
#4381=FACE_OUTER_BOUND('',#7661,.T.);
#4382=FACE_OUTER_BOUND('',#7662,.T.);
#4383=FACE_OUTER_BOUND('',#7663,.T.);
#4384=FACE_OUTER_BOUND('',#7664,.T.);
#4385=FACE_OUTER_BOUND('',#7665,.T.);
#4386=FACE_OUTER_BOUND('',#7666,.T.);
#4387=FACE_OUTER_BOUND('',#7667,.T.);
#4388=FACE_OUTER_BOUND('',#7668,.T.);
#4389=FACE_OUTER_BOUND('',#7669,.T.);
#4390=FACE_OUTER_BOUND('',#7670,.T.);
#4391=FACE_OUTER_BOUND('',#7671,.T.);
#4392=FACE_OUTER_BOUND('',#7672,.T.);
#4393=FACE_OUTER_BOUND('',#7673,.T.);
#4394=FACE_OUTER_BOUND('',#7674,.T.);
#4395=FACE_OUTER_BOUND('',#7675,.T.);
#4396=FACE_OUTER_BOUND('',#7676,.T.);
#4397=FACE_OUTER_BOUND('',#7677,.T.);
#4398=FACE_OUTER_BOUND('',#7678,.T.);
#4399=FACE_OUTER_BOUND('',#7679,.T.);
#4400=FACE_OUTER_BOUND('',#7680,.T.);
#4401=FACE_OUTER_BOUND('',#7681,.T.);
#4402=FACE_OUTER_BOUND('',#7682,.T.);
#4403=FACE_OUTER_BOUND('',#7683,.T.);
#4404=FACE_OUTER_BOUND('',#7684,.T.);
#4405=FACE_OUTER_BOUND('',#7685,.T.);
#4406=FACE_OUTER_BOUND('',#7686,.T.);
#4407=FACE_OUTER_BOUND('',#7687,.T.);
#4408=FACE_OUTER_BOUND('',#7688,.T.);
#4409=FACE_OUTER_BOUND('',#7689,.T.);
#4410=FACE_OUTER_BOUND('',#7690,.T.);
#4411=FACE_OUTER_BOUND('',#7691,.T.);
#4412=FACE_OUTER_BOUND('',#7692,.T.);
#4413=FACE_OUTER_BOUND('',#7693,.T.);
#4414=FACE_OUTER_BOUND('',#7694,.T.);
#4415=FACE_OUTER_BOUND('',#7695,.T.);
#4416=FACE_OUTER_BOUND('',#7696,.T.);
#4417=FACE_OUTER_BOUND('',#7697,.T.);
#4418=FACE_OUTER_BOUND('',#7698,.T.);
#4419=FACE_OUTER_BOUND('',#7699,.T.);
#4420=FACE_OUTER_BOUND('',#7700,.T.);
#4421=FACE_OUTER_BOUND('',#7701,.T.);
#4422=FACE_OUTER_BOUND('',#7702,.T.);
#4423=FACE_OUTER_BOUND('',#7703,.T.);
#4424=FACE_OUTER_BOUND('',#7704,.T.);
#4425=FACE_OUTER_BOUND('',#7706,.T.);
#4426=FACE_OUTER_BOUND('',#7707,.T.);
#4427=FACE_OUTER_BOUND('',#7708,.T.);
#4428=FACE_OUTER_BOUND('',#7709,.T.);
#4429=FACE_OUTER_BOUND('',#7710,.T.);
#4430=FACE_OUTER_BOUND('',#7711,.T.);
#4431=FACE_OUTER_BOUND('',#7712,.T.);
#4432=FACE_OUTER_BOUND('',#7713,.T.);
#4433=FACE_OUTER_BOUND('',#7714,.T.);
#4434=FACE_OUTER_BOUND('',#7715,.T.);
#4435=FACE_OUTER_BOUND('',#7716,.T.);
#4436=FACE_OUTER_BOUND('',#7717,.T.);
#4437=FACE_OUTER_BOUND('',#7718,.T.);
#4438=FACE_OUTER_BOUND('',#7719,.T.);
#4439=FACE_OUTER_BOUND('',#7720,.T.);
#4440=FACE_OUTER_BOUND('',#7721,.T.);
#4441=FACE_OUTER_BOUND('',#7722,.T.);
#4442=FACE_OUTER_BOUND('',#7723,.T.);
#4443=FACE_OUTER_BOUND('',#7724,.T.);
#4444=FACE_OUTER_BOUND('',#7725,.T.);
#4445=FACE_OUTER_BOUND('',#7726,.T.);
#4446=FACE_OUTER_BOUND('',#7727,.T.);
#4447=FACE_OUTER_BOUND('',#7728,.T.);
#4448=FACE_OUTER_BOUND('',#7729,.T.);
#4449=FACE_OUTER_BOUND('',#7730,.T.);
#4450=FACE_OUTER_BOUND('',#7731,.T.);
#4451=FACE_OUTER_BOUND('',#7732,.T.);
#4452=FACE_OUTER_BOUND('',#7733,.T.);
#4453=FACE_OUTER_BOUND('',#7734,.T.);
#4454=FACE_OUTER_BOUND('',#7735,.T.);
#4455=FACE_OUTER_BOUND('',#7736,.T.);
#4456=FACE_OUTER_BOUND('',#7737,.T.);
#4457=FACE_OUTER_BOUND('',#7739,.T.);
#4458=FACE_OUTER_BOUND('',#7740,.T.);
#4459=FACE_OUTER_BOUND('',#7741,.T.);
#4460=FACE_OUTER_BOUND('',#7742,.T.);
#4461=FACE_OUTER_BOUND('',#7743,.T.);
#4462=FACE_OUTER_BOUND('',#7744,.T.);
#4463=FACE_OUTER_BOUND('',#7745,.T.);
#4464=FACE_OUTER_BOUND('',#7746,.T.);
#4465=FACE_OUTER_BOUND('',#7747,.T.);
#4466=FACE_OUTER_BOUND('',#7748,.T.);
#4467=FACE_OUTER_BOUND('',#7749,.T.);
#4468=FACE_OUTER_BOUND('',#7750,.T.);
#4469=FACE_OUTER_BOUND('',#7751,.T.);
#4470=FACE_OUTER_BOUND('',#7752,.T.);
#4471=FACE_OUTER_BOUND('',#7753,.T.);
#4472=FACE_OUTER_BOUND('',#7754,.T.);
#4473=FACE_OUTER_BOUND('',#7755,.T.);
#4474=FACE_OUTER_BOUND('',#7756,.T.);
#4475=FACE_OUTER_BOUND('',#7757,.T.);
#4476=FACE_OUTER_BOUND('',#7758,.T.);
#4477=FACE_OUTER_BOUND('',#7759,.T.);
#4478=FACE_OUTER_BOUND('',#7760,.T.);
#4479=FACE_OUTER_BOUND('',#7762,.T.);
#4480=FACE_OUTER_BOUND('',#7763,.T.);
#4481=FACE_OUTER_BOUND('',#7764,.T.);
#4482=FACE_OUTER_BOUND('',#7765,.T.);
#4483=FACE_OUTER_BOUND('',#7766,.T.);
#4484=FACE_OUTER_BOUND('',#7767,.T.);
#4485=FACE_OUTER_BOUND('',#7768,.T.);
#4486=FACE_OUTER_BOUND('',#7769,.T.);
#4487=FACE_OUTER_BOUND('',#7770,.T.);
#4488=FACE_OUTER_BOUND('',#7771,.T.);
#4489=FACE_OUTER_BOUND('',#7772,.T.);
#4490=FACE_OUTER_BOUND('',#7773,.T.);
#4491=FACE_OUTER_BOUND('',#7774,.T.);
#4492=FACE_OUTER_BOUND('',#7775,.T.);
#4493=FACE_OUTER_BOUND('',#7776,.T.);
#4494=FACE_OUTER_BOUND('',#7777,.T.);
#4495=FACE_OUTER_BOUND('',#7778,.T.);
#4496=FACE_OUTER_BOUND('',#7779,.T.);
#4497=FACE_OUTER_BOUND('',#7780,.T.);
#4498=FACE_OUTER_BOUND('',#7781,.T.);
#4499=FACE_OUTER_BOUND('',#7782,.T.);
#4500=FACE_OUTER_BOUND('',#7783,.T.);
#4501=FACE_OUTER_BOUND('',#7784,.T.);
#4502=FACE_OUTER_BOUND('',#7785,.T.);
#4503=FACE_OUTER_BOUND('',#7786,.T.);
#4504=FACE_OUTER_BOUND('',#7787,.T.);
#4505=FACE_OUTER_BOUND('',#7788,.T.);
#4506=FACE_OUTER_BOUND('',#7789,.T.);
#4507=FACE_OUTER_BOUND('',#7790,.T.);
#4508=FACE_OUTER_BOUND('',#7791,.T.);
#4509=FACE_OUTER_BOUND('',#7792,.T.);
#4510=FACE_OUTER_BOUND('',#7793,.T.);
#4511=FACE_OUTER_BOUND('',#7795,.T.);
#4512=FACE_OUTER_BOUND('',#7796,.T.);
#4513=FACE_OUTER_BOUND('',#7797,.T.);
#4514=FACE_OUTER_BOUND('',#7798,.T.);
#4515=FACE_OUTER_BOUND('',#7799,.T.);
#4516=FACE_OUTER_BOUND('',#7800,.T.);
#4517=FACE_OUTER_BOUND('',#7801,.T.);
#4518=FACE_OUTER_BOUND('',#7802,.T.);
#4519=FACE_OUTER_BOUND('',#7803,.T.);
#4520=FACE_OUTER_BOUND('',#7804,.T.);
#4521=FACE_OUTER_BOUND('',#7805,.T.);
#4522=FACE_OUTER_BOUND('',#7806,.T.);
#4523=FACE_OUTER_BOUND('',#7807,.T.);
#4524=FACE_OUTER_BOUND('',#7808,.T.);
#4525=FACE_OUTER_BOUND('',#7809,.T.);
#4526=FACE_OUTER_BOUND('',#7810,.T.);
#4527=FACE_OUTER_BOUND('',#7811,.T.);
#4528=FACE_OUTER_BOUND('',#7812,.T.);
#4529=FACE_OUTER_BOUND('',#7813,.T.);
#4530=FACE_OUTER_BOUND('',#7814,.T.);
#4531=FACE_OUTER_BOUND('',#7815,.T.);
#4532=FACE_OUTER_BOUND('',#7816,.T.);
#4533=FACE_OUTER_BOUND('',#7817,.T.);
#4534=FACE_OUTER_BOUND('',#7818,.T.);
#4535=FACE_OUTER_BOUND('',#7819,.T.);
#4536=FACE_OUTER_BOUND('',#7820,.T.);
#4537=FACE_OUTER_BOUND('',#7821,.T.);
#4538=FACE_OUTER_BOUND('',#7822,.T.);
#4539=FACE_OUTER_BOUND('',#7823,.T.);
#4540=FACE_OUTER_BOUND('',#7824,.T.);
#4541=FACE_OUTER_BOUND('',#7825,.T.);
#4542=FACE_OUTER_BOUND('',#7826,.T.);
#4543=FACE_OUTER_BOUND('',#7827,.T.);
#4544=FACE_OUTER_BOUND('',#7828,.T.);
#4545=FACE_OUTER_BOUND('',#7829,.T.);
#4546=FACE_OUTER_BOUND('',#7830,.T.);
#4547=FACE_OUTER_BOUND('',#7831,.T.);
#4548=FACE_OUTER_BOUND('',#7832,.T.);
#4549=FACE_OUTER_BOUND('',#7833,.T.);
#4550=FACE_OUTER_BOUND('',#7834,.T.);
#4551=FACE_OUTER_BOUND('',#7835,.T.);
#4552=FACE_OUTER_BOUND('',#7836,.T.);
#4553=FACE_OUTER_BOUND('',#7837,.T.);
#4554=FACE_OUTER_BOUND('',#7838,.T.);
#4555=FACE_OUTER_BOUND('',#7839,.T.);
#4556=FACE_OUTER_BOUND('',#7841,.T.);
#4557=FACE_OUTER_BOUND('',#7842,.T.);
#4558=FACE_OUTER_BOUND('',#7843,.T.);
#4559=FACE_OUTER_BOUND('',#7844,.T.);
#4560=FACE_OUTER_BOUND('',#7845,.T.);
#4561=FACE_OUTER_BOUND('',#7846,.T.);
#4562=FACE_OUTER_BOUND('',#7847,.T.);
#4563=FACE_OUTER_BOUND('',#7848,.T.);
#4564=FACE_OUTER_BOUND('',#7849,.T.);
#4565=FACE_OUTER_BOUND('',#7850,.T.);
#4566=FACE_OUTER_BOUND('',#7851,.T.);
#4567=FACE_OUTER_BOUND('',#7852,.T.);
#4568=FACE_OUTER_BOUND('',#7853,.T.);
#4569=FACE_OUTER_BOUND('',#7854,.T.);
#4570=FACE_OUTER_BOUND('',#7855,.T.);
#4571=FACE_OUTER_BOUND('',#7856,.T.);
#4572=FACE_OUTER_BOUND('',#7857,.T.);
#4573=FACE_OUTER_BOUND('',#7858,.T.);
#4574=FACE_OUTER_BOUND('',#7859,.T.);
#4575=FACE_OUTER_BOUND('',#7860,.T.);
#4576=FACE_OUTER_BOUND('',#7861,.T.);
#4577=FACE_OUTER_BOUND('',#7862,.T.);
#4578=FACE_OUTER_BOUND('',#7863,.T.);
#4579=FACE_OUTER_BOUND('',#7864,.T.);
#4580=FACE_OUTER_BOUND('',#7865,.T.);
#4581=FACE_OUTER_BOUND('',#7866,.T.);
#4582=FACE_OUTER_BOUND('',#7867,.T.);
#4583=FACE_OUTER_BOUND('',#7868,.T.);
#4584=FACE_OUTER_BOUND('',#7869,.T.);
#4585=FACE_OUTER_BOUND('',#7870,.T.);
#4586=FACE_OUTER_BOUND('',#7871,.T.);
#4587=FACE_OUTER_BOUND('',#7872,.T.);
#4588=FACE_OUTER_BOUND('',#7873,.T.);
#4589=FACE_OUTER_BOUND('',#7874,.T.);
#4590=FACE_OUTER_BOUND('',#7875,.T.);
#4591=FACE_OUTER_BOUND('',#7876,.T.);
#4592=FACE_OUTER_BOUND('',#7877,.T.);
#4593=FACE_OUTER_BOUND('',#7878,.T.);
#4594=FACE_OUTER_BOUND('',#7879,.T.);
#4595=FACE_OUTER_BOUND('',#7880,.T.);
#4596=FACE_OUTER_BOUND('',#7881,.T.);
#4597=FACE_OUTER_BOUND('',#7882,.T.);
#4598=FACE_OUTER_BOUND('',#7883,.T.);
#4599=FACE_OUTER_BOUND('',#7884,.T.);
#4600=FACE_OUTER_BOUND('',#7885,.T.);
#4601=FACE_OUTER_BOUND('',#7886,.T.);
#4602=FACE_OUTER_BOUND('',#7887,.T.);
#4603=FACE_OUTER_BOUND('',#7888,.T.);
#4604=FACE_OUTER_BOUND('',#7889,.T.);
#4605=FACE_OUTER_BOUND('',#7890,.T.);
#4606=FACE_OUTER_BOUND('',#7891,.T.);
#4607=FACE_OUTER_BOUND('',#7892,.T.);
#4608=FACE_OUTER_BOUND('',#7893,.T.);
#4609=FACE_OUTER_BOUND('',#7895,.T.);
#4610=FACE_OUTER_BOUND('',#7896,.T.);
#4611=FACE_OUTER_BOUND('',#7897,.T.);
#4612=FACE_OUTER_BOUND('',#7898,.T.);
#4613=FACE_OUTER_BOUND('',#7899,.T.);
#4614=FACE_OUTER_BOUND('',#7900,.T.);
#4615=FACE_OUTER_BOUND('',#7901,.T.);
#4616=FACE_OUTER_BOUND('',#7902,.T.);
#4617=FACE_OUTER_BOUND('',#7903,.T.);
#4618=FACE_OUTER_BOUND('',#7904,.T.);
#4619=FACE_OUTER_BOUND('',#7905,.T.);
#4620=FACE_OUTER_BOUND('',#7906,.T.);
#4621=FACE_OUTER_BOUND('',#7907,.T.);
#4622=FACE_OUTER_BOUND('',#7908,.T.);
#4623=FACE_OUTER_BOUND('',#7909,.T.);
#4624=FACE_OUTER_BOUND('',#7911,.T.);
#4625=FACE_OUTER_BOUND('',#7912,.T.);
#4626=FACE_OUTER_BOUND('',#7913,.T.);
#4627=FACE_OUTER_BOUND('',#7914,.T.);
#4628=FACE_OUTER_BOUND('',#7915,.T.);
#4629=FACE_OUTER_BOUND('',#7916,.T.);
#4630=FACE_OUTER_BOUND('',#7917,.T.);
#4631=FACE_OUTER_BOUND('',#7918,.T.);
#4632=FACE_OUTER_BOUND('',#7919,.T.);
#4633=FACE_OUTER_BOUND('',#7920,.T.);
#4634=FACE_OUTER_BOUND('',#7921,.T.);
#4635=FACE_OUTER_BOUND('',#7922,.T.);
#4636=FACE_OUTER_BOUND('',#7923,.T.);
#4637=FACE_OUTER_BOUND('',#7924,.T.);
#4638=FACE_OUTER_BOUND('',#7925,.T.);
#4639=FACE_OUTER_BOUND('',#7926,.T.);
#4640=FACE_OUTER_BOUND('',#7927,.T.);
#4641=FACE_OUTER_BOUND('',#7928,.T.);
#4642=FACE_OUTER_BOUND('',#7929,.T.);
#4643=FACE_OUTER_BOUND('',#7930,.T.);
#4644=FACE_OUTER_BOUND('',#7931,.T.);
#4645=FACE_OUTER_BOUND('',#7932,.T.);
#4646=FACE_OUTER_BOUND('',#7933,.T.);
#4647=FACE_OUTER_BOUND('',#7935,.T.);
#4648=FACE_OUTER_BOUND('',#7936,.T.);
#4649=FACE_OUTER_BOUND('',#7937,.T.);
#4650=FACE_OUTER_BOUND('',#7938,.T.);
#4651=FACE_OUTER_BOUND('',#7939,.T.);
#4652=FACE_OUTER_BOUND('',#7940,.T.);
#4653=FACE_OUTER_BOUND('',#7941,.T.);
#4654=FACE_OUTER_BOUND('',#7942,.T.);
#4655=FACE_OUTER_BOUND('',#7943,.T.);
#4656=FACE_OUTER_BOUND('',#7944,.T.);
#4657=FACE_OUTER_BOUND('',#7945,.T.);
#4658=FACE_OUTER_BOUND('',#7946,.T.);
#4659=FACE_OUTER_BOUND('',#7947,.T.);
#4660=FACE_OUTER_BOUND('',#7948,.T.);
#4661=FACE_OUTER_BOUND('',#7949,.T.);
#4662=FACE_OUTER_BOUND('',#7950,.T.);
#4663=FACE_OUTER_BOUND('',#7951,.T.);
#4664=FACE_OUTER_BOUND('',#7952,.T.);
#4665=FACE_OUTER_BOUND('',#7953,.T.);
#4666=FACE_OUTER_BOUND('',#7954,.T.);
#4667=FACE_OUTER_BOUND('',#7955,.T.);
#4668=FACE_OUTER_BOUND('',#7956,.T.);
#4669=FACE_OUTER_BOUND('',#7957,.T.);
#4670=FACE_OUTER_BOUND('',#7958,.T.);
#4671=FACE_OUTER_BOUND('',#7959,.T.);
#4672=FACE_OUTER_BOUND('',#7960,.T.);
#4673=FACE_OUTER_BOUND('',#7961,.T.);
#4674=FACE_OUTER_BOUND('',#7962,.T.);
#4675=FACE_OUTER_BOUND('',#7963,.T.);
#4676=FACE_OUTER_BOUND('',#7964,.T.);
#4677=FACE_OUTER_BOUND('',#7965,.T.);
#4678=FACE_OUTER_BOUND('',#7966,.T.);
#4679=FACE_OUTER_BOUND('',#7967,.T.);
#4680=FACE_OUTER_BOUND('',#7968,.T.);
#4681=FACE_OUTER_BOUND('',#7969,.T.);
#4682=FACE_OUTER_BOUND('',#7970,.T.);
#4683=FACE_OUTER_BOUND('',#7971,.T.);
#4684=FACE_OUTER_BOUND('',#7972,.T.);
#4685=FACE_OUTER_BOUND('',#7973,.T.);
#4686=FACE_OUTER_BOUND('',#7974,.T.);
#4687=FACE_OUTER_BOUND('',#7975,.T.);
#4688=FACE_OUTER_BOUND('',#7976,.T.);
#4689=FACE_OUTER_BOUND('',#7977,.T.);
#4690=FACE_OUTER_BOUND('',#7978,.T.);
#4691=FACE_OUTER_BOUND('',#7979,.T.);
#4692=FACE_OUTER_BOUND('',#7981,.T.);
#4693=FACE_OUTER_BOUND('',#7982,.T.);
#4694=FACE_OUTER_BOUND('',#7983,.T.);
#4695=FACE_OUTER_BOUND('',#7984,.T.);
#4696=FACE_OUTER_BOUND('',#7985,.T.);
#4697=FACE_OUTER_BOUND('',#7986,.T.);
#4698=FACE_OUTER_BOUND('',#7987,.T.);
#4699=FACE_OUTER_BOUND('',#7988,.T.);
#4700=FACE_OUTER_BOUND('',#7989,.T.);
#4701=FACE_OUTER_BOUND('',#7990,.T.);
#4702=FACE_OUTER_BOUND('',#7991,.T.);
#4703=FACE_OUTER_BOUND('',#7992,.T.);
#4704=FACE_OUTER_BOUND('',#7993,.T.);
#4705=FACE_OUTER_BOUND('',#7994,.T.);
#4706=FACE_OUTER_BOUND('',#7995,.T.);
#4707=FACE_OUTER_BOUND('',#7996,.T.);
#4708=FACE_OUTER_BOUND('',#7997,.T.);
#4709=FACE_OUTER_BOUND('',#7998,.T.);
#4710=FACE_OUTER_BOUND('',#7999,.T.);
#4711=FACE_OUTER_BOUND('',#8000,.T.);
#4712=FACE_OUTER_BOUND('',#8001,.T.);
#4713=FACE_OUTER_BOUND('',#8002,.T.);
#4714=FACE_OUTER_BOUND('',#8003,.T.);
#4715=FACE_OUTER_BOUND('',#8004,.T.);
#4716=FACE_OUTER_BOUND('',#8005,.T.);
#4717=FACE_OUTER_BOUND('',#8006,.T.);
#4718=FACE_OUTER_BOUND('',#8007,.T.);
#4719=FACE_OUTER_BOUND('',#8008,.T.);
#4720=FACE_OUTER_BOUND('',#8009,.T.);
#4721=FACE_OUTER_BOUND('',#8011,.T.);
#4722=FACE_OUTER_BOUND('',#8012,.T.);
#4723=FACE_OUTER_BOUND('',#8013,.T.);
#4724=FACE_OUTER_BOUND('',#8014,.T.);
#4725=FACE_OUTER_BOUND('',#8015,.T.);
#4726=FACE_OUTER_BOUND('',#8016,.T.);
#4727=FACE_OUTER_BOUND('',#8017,.T.);
#4728=FACE_OUTER_BOUND('',#8018,.T.);
#4729=FACE_OUTER_BOUND('',#8019,.T.);
#4730=FACE_OUTER_BOUND('',#8020,.T.);
#4731=FACE_OUTER_BOUND('',#8021,.T.);
#4732=FACE_OUTER_BOUND('',#8022,.T.);
#4733=FACE_OUTER_BOUND('',#8023,.T.);
#4734=FACE_OUTER_BOUND('',#8024,.T.);
#4735=FACE_OUTER_BOUND('',#8025,.T.);
#4736=FACE_OUTER_BOUND('',#8026,.T.);
#4737=FACE_OUTER_BOUND('',#8027,.T.);
#4738=FACE_OUTER_BOUND('',#8028,.T.);
#4739=FACE_OUTER_BOUND('',#8029,.T.);
#4740=FACE_OUTER_BOUND('',#8030,.T.);
#4741=FACE_OUTER_BOUND('',#8031,.T.);
#4742=FACE_OUTER_BOUND('',#8032,.T.);
#4743=FACE_OUTER_BOUND('',#8033,.T.);
#4744=FACE_OUTER_BOUND('',#8035,.T.);
#4745=FACE_OUTER_BOUND('',#8036,.T.);
#4746=FACE_OUTER_BOUND('',#8037,.T.);
#4747=FACE_OUTER_BOUND('',#8038,.T.);
#4748=FACE_OUTER_BOUND('',#8039,.T.);
#4749=FACE_OUTER_BOUND('',#8040,.T.);
#4750=FACE_OUTER_BOUND('',#8041,.T.);
#4751=FACE_OUTER_BOUND('',#8042,.T.);
#4752=FACE_OUTER_BOUND('',#8043,.T.);
#4753=FACE_OUTER_BOUND('',#8044,.T.);
#4754=FACE_OUTER_BOUND('',#8045,.T.);
#4755=FACE_OUTER_BOUND('',#8046,.T.);
#4756=FACE_OUTER_BOUND('',#8047,.T.);
#4757=FACE_OUTER_BOUND('',#8048,.T.);
#4758=FACE_OUTER_BOUND('',#8049,.T.);
#4759=FACE_OUTER_BOUND('',#8050,.T.);
#4760=FACE_OUTER_BOUND('',#8051,.T.);
#4761=FACE_OUTER_BOUND('',#8052,.T.);
#4762=FACE_OUTER_BOUND('',#8053,.T.);
#4763=FACE_OUTER_BOUND('',#8054,.T.);
#4764=FACE_OUTER_BOUND('',#8055,.T.);
#4765=FACE_OUTER_BOUND('',#8056,.T.);
#4766=FACE_OUTER_BOUND('',#8057,.T.);
#4767=FACE_OUTER_BOUND('',#8058,.T.);
#4768=FACE_OUTER_BOUND('',#8059,.T.);
#4769=FACE_OUTER_BOUND('',#8060,.T.);
#4770=FACE_OUTER_BOUND('',#8061,.T.);
#4771=FACE_OUTER_BOUND('',#8062,.T.);
#4772=FACE_OUTER_BOUND('',#8063,.T.);
#4773=FACE_OUTER_BOUND('',#8064,.T.);
#4774=FACE_OUTER_BOUND('',#8065,.T.);
#4775=FACE_OUTER_BOUND('',#8066,.T.);
#4776=FACE_OUTER_BOUND('',#8067,.T.);
#4777=FACE_OUTER_BOUND('',#8068,.T.);
#4778=FACE_OUTER_BOUND('',#8070,.T.);
#4779=FACE_OUTER_BOUND('',#8071,.T.);
#4780=FACE_OUTER_BOUND('',#8072,.T.);
#4781=FACE_OUTER_BOUND('',#8073,.T.);
#4782=FACE_OUTER_BOUND('',#8074,.T.);
#4783=FACE_OUTER_BOUND('',#8075,.T.);
#4784=FACE_OUTER_BOUND('',#8076,.T.);
#4785=FACE_OUTER_BOUND('',#8077,.T.);
#4786=FACE_OUTER_BOUND('',#8078,.T.);
#4787=FACE_OUTER_BOUND('',#8079,.T.);
#4788=FACE_OUTER_BOUND('',#8080,.T.);
#4789=FACE_OUTER_BOUND('',#8081,.T.);
#4790=FACE_OUTER_BOUND('',#8082,.T.);
#4791=FACE_OUTER_BOUND('',#8083,.T.);
#4792=FACE_OUTER_BOUND('',#8084,.T.);
#4793=FACE_OUTER_BOUND('',#8085,.T.);
#4794=FACE_OUTER_BOUND('',#8086,.T.);
#4795=FACE_OUTER_BOUND('',#8087,.T.);
#4796=FACE_OUTER_BOUND('',#8088,.T.);
#4797=FACE_OUTER_BOUND('',#8089,.T.);
#4798=FACE_OUTER_BOUND('',#8090,.T.);
#4799=FACE_OUTER_BOUND('',#8091,.T.);
#4800=FACE_OUTER_BOUND('',#8092,.T.);
#4801=FACE_OUTER_BOUND('',#8093,.T.);
#4802=FACE_OUTER_BOUND('',#8094,.T.);
#4803=FACE_OUTER_BOUND('',#8095,.T.);
#4804=FACE_OUTER_BOUND('',#8096,.T.);
#4805=FACE_OUTER_BOUND('',#8097,.T.);
#4806=FACE_OUTER_BOUND('',#8098,.T.);
#4807=FACE_OUTER_BOUND('',#8099,.T.);
#4808=FACE_OUTER_BOUND('',#8100,.T.);
#4809=FACE_OUTER_BOUND('',#8101,.T.);
#4810=FACE_OUTER_BOUND('',#8102,.T.);
#4811=FACE_OUTER_BOUND('',#8103,.T.);
#4812=FACE_OUTER_BOUND('',#8106,.T.);
#4813=FACE_OUTER_BOUND('',#8107,.T.);
#4814=FACE_OUTER_BOUND('',#8108,.T.);
#4815=FACE_OUTER_BOUND('',#8109,.T.);
#4816=FACE_OUTER_BOUND('',#8110,.T.);
#4817=FACE_OUTER_BOUND('',#8111,.T.);
#4818=FACE_OUTER_BOUND('',#8112,.T.);
#4819=FACE_OUTER_BOUND('',#8113,.T.);
#4820=FACE_OUTER_BOUND('',#8114,.T.);
#4821=FACE_OUTER_BOUND('',#8115,.T.);
#4822=FACE_OUTER_BOUND('',#8116,.T.);
#4823=FACE_OUTER_BOUND('',#8117,.T.);
#4824=FACE_OUTER_BOUND('',#8118,.T.);
#4825=FACE_OUTER_BOUND('',#8119,.T.);
#4826=FACE_OUTER_BOUND('',#8120,.T.);
#4827=FACE_OUTER_BOUND('',#8121,.T.);
#4828=FACE_OUTER_BOUND('',#8122,.T.);
#4829=FACE_OUTER_BOUND('',#8123,.T.);
#4830=FACE_OUTER_BOUND('',#8124,.T.);
#4831=FACE_OUTER_BOUND('',#8125,.T.);
#4832=FACE_OUTER_BOUND('',#8126,.T.);
#4833=FACE_OUTER_BOUND('',#8127,.T.);
#4834=FACE_OUTER_BOUND('',#8128,.T.);
#4835=FACE_OUTER_BOUND('',#8129,.T.);
#4836=FACE_OUTER_BOUND('',#8131,.T.);
#4837=FACE_OUTER_BOUND('',#8132,.T.);
#4838=FACE_OUTER_BOUND('',#8133,.T.);
#4839=FACE_OUTER_BOUND('',#8134,.T.);
#4840=FACE_OUTER_BOUND('',#8135,.T.);
#4841=FACE_OUTER_BOUND('',#8136,.T.);
#4842=FACE_OUTER_BOUND('',#8137,.T.);
#4843=FACE_OUTER_BOUND('',#8138,.T.);
#4844=FACE_OUTER_BOUND('',#8139,.T.);
#4845=FACE_OUTER_BOUND('',#8140,.T.);
#4846=FACE_OUTER_BOUND('',#8141,.T.);
#4847=FACE_OUTER_BOUND('',#8142,.T.);
#4848=FACE_OUTER_BOUND('',#8143,.T.);
#4849=FACE_OUTER_BOUND('',#8144,.T.);
#4850=FACE_OUTER_BOUND('',#8145,.T.);
#4851=FACE_OUTER_BOUND('',#8146,.T.);
#4852=FACE_OUTER_BOUND('',#8147,.T.);
#4853=FACE_OUTER_BOUND('',#8148,.T.);
#4854=FACE_OUTER_BOUND('',#8149,.T.);
#4855=FACE_OUTER_BOUND('',#8150,.T.);
#4856=FACE_OUTER_BOUND('',#8151,.T.);
#4857=FACE_OUTER_BOUND('',#8152,.T.);
#4858=FACE_OUTER_BOUND('',#8153,.T.);
#4859=FACE_OUTER_BOUND('',#8154,.T.);
#4860=FACE_OUTER_BOUND('',#8155,.T.);
#4861=FACE_OUTER_BOUND('',#8156,.T.);
#4862=FACE_OUTER_BOUND('',#8157,.T.);
#4863=FACE_OUTER_BOUND('',#8158,.T.);
#4864=FACE_OUTER_BOUND('',#8159,.T.);
#4865=FACE_OUTER_BOUND('',#8160,.T.);
#4866=FACE_OUTER_BOUND('',#8161,.T.);
#4867=FACE_OUTER_BOUND('',#8163,.T.);
#4868=FACE_OUTER_BOUND('',#8164,.T.);
#4869=FACE_OUTER_BOUND('',#8165,.T.);
#4870=FACE_OUTER_BOUND('',#8166,.T.);
#4871=FACE_OUTER_BOUND('',#8167,.T.);
#4872=FACE_OUTER_BOUND('',#8168,.T.);
#4873=FACE_OUTER_BOUND('',#8169,.T.);
#4874=FACE_OUTER_BOUND('',#8170,.T.);
#4875=FACE_OUTER_BOUND('',#8171,.T.);
#4876=FACE_OUTER_BOUND('',#8172,.T.);
#4877=FACE_OUTER_BOUND('',#8173,.T.);
#4878=FACE_OUTER_BOUND('',#8174,.T.);
#4879=FACE_OUTER_BOUND('',#8175,.T.);
#4880=FACE_OUTER_BOUND('',#8176,.T.);
#4881=FACE_OUTER_BOUND('',#8177,.T.);
#4882=FACE_OUTER_BOUND('',#8178,.T.);
#4883=FACE_OUTER_BOUND('',#8179,.T.);
#4884=FACE_OUTER_BOUND('',#8180,.T.);
#4885=FACE_OUTER_BOUND('',#8181,.T.);
#4886=FACE_OUTER_BOUND('',#8182,.T.);
#4887=FACE_OUTER_BOUND('',#8183,.T.);
#4888=FACE_OUTER_BOUND('',#8184,.T.);
#4889=FACE_OUTER_BOUND('',#8185,.T.);
#4890=FACE_OUTER_BOUND('',#8186,.T.);
#4891=FACE_OUTER_BOUND('',#8187,.T.);
#4892=FACE_OUTER_BOUND('',#8188,.T.);
#4893=FACE_OUTER_BOUND('',#8189,.T.);
#4894=FACE_OUTER_BOUND('',#8190,.T.);
#4895=FACE_OUTER_BOUND('',#8191,.T.);
#4896=FACE_OUTER_BOUND('',#8192,.T.);
#4897=FACE_OUTER_BOUND('',#8193,.T.);
#4898=FACE_OUTER_BOUND('',#8194,.T.);
#4899=FACE_OUTER_BOUND('',#8195,.T.);
#4900=FACE_OUTER_BOUND('',#8196,.T.);
#4901=FACE_OUTER_BOUND('',#8197,.T.);
#4902=FACE_OUTER_BOUND('',#8198,.T.);
#4903=FACE_OUTER_BOUND('',#8199,.T.);
#4904=FACE_OUTER_BOUND('',#8200,.T.);
#4905=FACE_OUTER_BOUND('',#8201,.T.);
#4906=FACE_OUTER_BOUND('',#8202,.T.);
#4907=FACE_OUTER_BOUND('',#8203,.T.);
#4908=FACE_OUTER_BOUND('',#8204,.T.);
#4909=FACE_OUTER_BOUND('',#8205,.T.);
#4910=FACE_OUTER_BOUND('',#8206,.T.);
#4911=FACE_OUTER_BOUND('',#8207,.T.);
#4912=FACE_OUTER_BOUND('',#8208,.T.);
#4913=FACE_OUTER_BOUND('',#8209,.T.);
#4914=FACE_OUTER_BOUND('',#8210,.T.);
#4915=FACE_OUTER_BOUND('',#8211,.T.);
#4916=FACE_OUTER_BOUND('',#8212,.T.);
#4917=FACE_OUTER_BOUND('',#8213,.T.);
#4918=FACE_OUTER_BOUND('',#8214,.T.);
#4919=FACE_OUTER_BOUND('',#8215,.T.);
#4920=FACE_OUTER_BOUND('',#8216,.T.);
#4921=FACE_OUTER_BOUND('',#8217,.T.);
#4922=FACE_OUTER_BOUND('',#8218,.T.);
#4923=FACE_OUTER_BOUND('',#8219,.T.);
#4924=FACE_OUTER_BOUND('',#8220,.T.);
#4925=FACE_OUTER_BOUND('',#8221,.T.);
#4926=FACE_OUTER_BOUND('',#8222,.T.);
#4927=FACE_OUTER_BOUND('',#8223,.T.);
#4928=FACE_OUTER_BOUND('',#8224,.T.);
#4929=FACE_OUTER_BOUND('',#8225,.T.);
#4930=FACE_OUTER_BOUND('',#8226,.T.);
#4931=FACE_OUTER_BOUND('',#8227,.T.);
#4932=FACE_OUTER_BOUND('',#8228,.T.);
#4933=FACE_OUTER_BOUND('',#8229,.T.);
#4934=FACE_OUTER_BOUND('',#8230,.T.);
#4935=FACE_OUTER_BOUND('',#8231,.T.);
#4936=FACE_OUTER_BOUND('',#8232,.T.);
#4937=FACE_OUTER_BOUND('',#8233,.T.);
#4938=FACE_OUTER_BOUND('',#8234,.T.);
#4939=FACE_OUTER_BOUND('',#8235,.T.);
#4940=FACE_OUTER_BOUND('',#8236,.T.);
#4941=FACE_OUTER_BOUND('',#8237,.T.);
#4942=FACE_OUTER_BOUND('',#8238,.T.);
#4943=FACE_OUTER_BOUND('',#8239,.T.);
#4944=FACE_OUTER_BOUND('',#8240,.T.);
#4945=FACE_OUTER_BOUND('',#8241,.T.);
#4946=FACE_OUTER_BOUND('',#8242,.T.);
#4947=FACE_OUTER_BOUND('',#8243,.T.);
#4948=FACE_OUTER_BOUND('',#8244,.T.);
#4949=FACE_OUTER_BOUND('',#8245,.T.);
#4950=FACE_OUTER_BOUND('',#8246,.T.);
#4951=FACE_OUTER_BOUND('',#8247,.T.);
#4952=FACE_OUTER_BOUND('',#8248,.T.);
#4953=FACE_OUTER_BOUND('',#8249,.T.);
#4954=FACE_OUTER_BOUND('',#8250,.T.);
#4955=FACE_OUTER_BOUND('',#8251,.T.);
#4956=FACE_OUTER_BOUND('',#8252,.T.);
#4957=FACE_OUTER_BOUND('',#8253,.T.);
#4958=FACE_OUTER_BOUND('',#8254,.T.);
#4959=FACE_OUTER_BOUND('',#8255,.T.);
#4960=FACE_OUTER_BOUND('',#8256,.T.);
#4961=FACE_OUTER_BOUND('',#8257,.T.);
#4962=FACE_OUTER_BOUND('',#8258,.T.);
#4963=FACE_OUTER_BOUND('',#8259,.T.);
#4964=FACE_OUTER_BOUND('',#8260,.T.);
#4965=FACE_OUTER_BOUND('',#8261,.T.);
#4966=FACE_OUTER_BOUND('',#8262,.T.);
#4967=FACE_OUTER_BOUND('',#8263,.T.);
#4968=FACE_OUTER_BOUND('',#8264,.T.);
#4969=FACE_OUTER_BOUND('',#8265,.T.);
#4970=FACE_OUTER_BOUND('',#8266,.T.);
#4971=FACE_OUTER_BOUND('',#8267,.T.);
#4972=FACE_OUTER_BOUND('',#8268,.T.);
#4973=FACE_OUTER_BOUND('',#8269,.T.);
#4974=FACE_OUTER_BOUND('',#8270,.T.);
#4975=FACE_OUTER_BOUND('',#8271,.T.);
#4976=FACE_OUTER_BOUND('',#8272,.T.);
#4977=FACE_OUTER_BOUND('',#8273,.T.);
#4978=FACE_OUTER_BOUND('',#8274,.T.);
#4979=FACE_OUTER_BOUND('',#8275,.T.);
#4980=FACE_OUTER_BOUND('',#8276,.T.);
#4981=FACE_OUTER_BOUND('',#8277,.T.);
#4982=FACE_OUTER_BOUND('',#8278,.T.);
#4983=FACE_OUTER_BOUND('',#8279,.T.);
#4984=FACE_OUTER_BOUND('',#8280,.T.);
#4985=FACE_OUTER_BOUND('',#8281,.T.);
#4986=FACE_OUTER_BOUND('',#8282,.T.);
#4987=FACE_OUTER_BOUND('',#8283,.T.);
#4988=FACE_OUTER_BOUND('',#8284,.T.);
#4989=FACE_OUTER_BOUND('',#8285,.T.);
#4990=FACE_OUTER_BOUND('',#8286,.T.);
#4991=FACE_OUTER_BOUND('',#8287,.T.);
#4992=FACE_OUTER_BOUND('',#8288,.T.);
#4993=FACE_OUTER_BOUND('',#8289,.T.);
#4994=FACE_OUTER_BOUND('',#8290,.T.);
#4995=FACE_OUTER_BOUND('',#8291,.T.);
#4996=FACE_OUTER_BOUND('',#8292,.T.);
#4997=FACE_OUTER_BOUND('',#8293,.T.);
#4998=FACE_OUTER_BOUND('',#8294,.T.);
#4999=FACE_OUTER_BOUND('',#8295,.T.);
#5000=FACE_OUTER_BOUND('',#8296,.T.);
#5001=FACE_OUTER_BOUND('',#8297,.T.);
#5002=FACE_OUTER_BOUND('',#8298,.T.);
#5003=FACE_OUTER_BOUND('',#8299,.T.);
#5004=FACE_OUTER_BOUND('',#8300,.T.);
#5005=FACE_OUTER_BOUND('',#8301,.T.);
#5006=FACE_OUTER_BOUND('',#8302,.T.);
#5007=FACE_OUTER_BOUND('',#8303,.T.);
#5008=FACE_OUTER_BOUND('',#8304,.T.);
#5009=FACE_OUTER_BOUND('',#8305,.T.);
#5010=FACE_OUTER_BOUND('',#8306,.T.);
#5011=FACE_OUTER_BOUND('',#8307,.T.);
#5012=FACE_OUTER_BOUND('',#8308,.T.);
#5013=FACE_OUTER_BOUND('',#8309,.T.);
#5014=FACE_OUTER_BOUND('',#8310,.T.);
#5015=FACE_OUTER_BOUND('',#8311,.T.);
#5016=FACE_OUTER_BOUND('',#8312,.T.);
#5017=FACE_OUTER_BOUND('',#8313,.T.);
#5018=FACE_OUTER_BOUND('',#8314,.T.);
#5019=FACE_OUTER_BOUND('',#8315,.T.);
#5020=FACE_OUTER_BOUND('',#8316,.T.);
#5021=FACE_OUTER_BOUND('',#8317,.T.);
#5022=FACE_OUTER_BOUND('',#8318,.T.);
#5023=FACE_OUTER_BOUND('',#8319,.T.);
#5024=FACE_OUTER_BOUND('',#8320,.T.);
#5025=FACE_OUTER_BOUND('',#8321,.T.);
#5026=FACE_OUTER_BOUND('',#8322,.T.);
#5027=FACE_OUTER_BOUND('',#8323,.T.);
#5028=FACE_OUTER_BOUND('',#8324,.T.);
#5029=FACE_OUTER_BOUND('',#8325,.T.);
#5030=FACE_OUTER_BOUND('',#8326,.T.);
#5031=FACE_OUTER_BOUND('',#8327,.T.);
#5032=FACE_OUTER_BOUND('',#8328,.T.);
#5033=FACE_OUTER_BOUND('',#8329,.T.);
#5034=FACE_OUTER_BOUND('',#8330,.T.);
#5035=FACE_OUTER_BOUND('',#8331,.T.);
#5036=FACE_OUTER_BOUND('',#8332,.T.);
#5037=FACE_OUTER_BOUND('',#8333,.T.);
#5038=FACE_OUTER_BOUND('',#8334,.T.);
#5039=FACE_OUTER_BOUND('',#8335,.T.);
#5040=FACE_OUTER_BOUND('',#8336,.T.);
#5041=FACE_OUTER_BOUND('',#8337,.T.);
#5042=FACE_OUTER_BOUND('',#8338,.T.);
#5043=FACE_OUTER_BOUND('',#8339,.T.);
#5044=FACE_OUTER_BOUND('',#8340,.T.);
#5045=FACE_OUTER_BOUND('',#8341,.T.);
#5046=FACE_OUTER_BOUND('',#8342,.T.);
#5047=FACE_OUTER_BOUND('',#8343,.T.);
#5048=FACE_OUTER_BOUND('',#8344,.T.);
#5049=FACE_OUTER_BOUND('',#8345,.T.);
#5050=FACE_OUTER_BOUND('',#8346,.T.);
#5051=FACE_OUTER_BOUND('',#8347,.T.);
#5052=FACE_OUTER_BOUND('',#8348,.T.);
#5053=FACE_OUTER_BOUND('',#8349,.T.);
#5054=FACE_OUTER_BOUND('',#8350,.T.);
#5055=FACE_OUTER_BOUND('',#8351,.T.);
#5056=FACE_OUTER_BOUND('',#8352,.T.);
#5057=FACE_OUTER_BOUND('',#8353,.T.);
#5058=FACE_OUTER_BOUND('',#8354,.T.);
#5059=FACE_OUTER_BOUND('',#8355,.T.);
#5060=FACE_OUTER_BOUND('',#8356,.T.);
#5061=FACE_OUTER_BOUND('',#8357,.T.);
#5062=FACE_OUTER_BOUND('',#8358,.T.);
#5063=FACE_OUTER_BOUND('',#8359,.T.);
#5064=FACE_OUTER_BOUND('',#8360,.T.);
#5065=FACE_OUTER_BOUND('',#8361,.T.);
#5066=FACE_OUTER_BOUND('',#8362,.T.);
#5067=FACE_OUTER_BOUND('',#8363,.T.);
#5068=FACE_OUTER_BOUND('',#8364,.T.);
#5069=FACE_OUTER_BOUND('',#8365,.T.);
#5070=FACE_OUTER_BOUND('',#8366,.T.);
#5071=FACE_OUTER_BOUND('',#8367,.T.);
#5072=FACE_OUTER_BOUND('',#8368,.T.);
#5073=FACE_OUTER_BOUND('',#8369,.T.);
#5074=FACE_OUTER_BOUND('',#8370,.T.);
#5075=FACE_OUTER_BOUND('',#8371,.T.);
#5076=FACE_OUTER_BOUND('',#8372,.T.);
#5077=FACE_OUTER_BOUND('',#8373,.T.);
#5078=FACE_OUTER_BOUND('',#8374,.T.);
#5079=FACE_OUTER_BOUND('',#8375,.T.);
#5080=FACE_OUTER_BOUND('',#8376,.T.);
#5081=FACE_OUTER_BOUND('',#8377,.T.);
#5082=FACE_OUTER_BOUND('',#8378,.T.);
#5083=FACE_OUTER_BOUND('',#8379,.T.);
#5084=FACE_OUTER_BOUND('',#8380,.T.);
#5085=FACE_OUTER_BOUND('',#8381,.T.);
#5086=FACE_OUTER_BOUND('',#8382,.T.);
#5087=FACE_OUTER_BOUND('',#8383,.T.);
#5088=FACE_OUTER_BOUND('',#8384,.T.);
#5089=FACE_OUTER_BOUND('',#8385,.T.);
#5090=FACE_OUTER_BOUND('',#8386,.T.);
#5091=FACE_OUTER_BOUND('',#8387,.T.);
#5092=FACE_OUTER_BOUND('',#8388,.T.);
#5093=FACE_OUTER_BOUND('',#8389,.T.);
#5094=FACE_OUTER_BOUND('',#8390,.T.);
#5095=FACE_OUTER_BOUND('',#8391,.T.);
#5096=FACE_OUTER_BOUND('',#8392,.T.);
#5097=FACE_OUTER_BOUND('',#8393,.T.);
#5098=FACE_OUTER_BOUND('',#8394,.T.);
#5099=FACE_OUTER_BOUND('',#8395,.T.);
#5100=FACE_OUTER_BOUND('',#8396,.T.);
#5101=FACE_OUTER_BOUND('',#8397,.T.);
#5102=FACE_OUTER_BOUND('',#8398,.T.);
#5103=FACE_OUTER_BOUND('',#8399,.T.);
#5104=FACE_OUTER_BOUND('',#8400,.T.);
#5105=FACE_OUTER_BOUND('',#8401,.T.);
#5106=FACE_OUTER_BOUND('',#8402,.T.);
#5107=FACE_OUTER_BOUND('',#8403,.T.);
#5108=FACE_OUTER_BOUND('',#8404,.T.);
#5109=FACE_OUTER_BOUND('',#8405,.T.);
#5110=FACE_OUTER_BOUND('',#8406,.T.);
#5111=FACE_OUTER_BOUND('',#8407,.T.);
#5112=FACE_OUTER_BOUND('',#8408,.T.);
#5113=FACE_OUTER_BOUND('',#8409,.T.);
#5114=FACE_OUTER_BOUND('',#8410,.T.);
#5115=FACE_OUTER_BOUND('',#8411,.T.);
#5116=FACE_OUTER_BOUND('',#8412,.T.);
#5117=FACE_OUTER_BOUND('',#8413,.T.);
#5118=FACE_OUTER_BOUND('',#8414,.T.);
#5119=FACE_OUTER_BOUND('',#8415,.T.);
#5120=FACE_OUTER_BOUND('',#8416,.T.);
#5121=FACE_OUTER_BOUND('',#8417,.T.);
#5122=FACE_OUTER_BOUND('',#8418,.T.);
#5123=FACE_OUTER_BOUND('',#8419,.T.);
#5124=FACE_OUTER_BOUND('',#8420,.T.);
#5125=FACE_OUTER_BOUND('',#8421,.T.);
#5126=FACE_OUTER_BOUND('',#8422,.T.);
#5127=FACE_OUTER_BOUND('',#8423,.T.);
#5128=FACE_OUTER_BOUND('',#8424,.T.);
#5129=FACE_OUTER_BOUND('',#8425,.T.);
#5130=FACE_OUTER_BOUND('',#8426,.T.);
#5131=FACE_OUTER_BOUND('',#8427,.T.);
#5132=FACE_OUTER_BOUND('',#8428,.T.);
#5133=FACE_OUTER_BOUND('',#8429,.T.);
#5134=FACE_OUTER_BOUND('',#8430,.T.);
#5135=FACE_OUTER_BOUND('',#8431,.T.);
#5136=FACE_OUTER_BOUND('',#8432,.T.);
#5137=FACE_OUTER_BOUND('',#8433,.T.);
#5138=FACE_OUTER_BOUND('',#8434,.T.);
#5139=FACE_OUTER_BOUND('',#8435,.T.);
#5140=FACE_OUTER_BOUND('',#8436,.T.);
#5141=FACE_OUTER_BOUND('',#8437,.T.);
#5142=FACE_OUTER_BOUND('',#8438,.T.);
#5143=FACE_OUTER_BOUND('',#8439,.T.);
#5144=FACE_OUTER_BOUND('',#8440,.T.);
#5145=FACE_OUTER_BOUND('',#8441,.T.);
#5146=FACE_OUTER_BOUND('',#8442,.T.);
#5147=FACE_OUTER_BOUND('',#8443,.T.);
#5148=FACE_OUTER_BOUND('',#8444,.T.);
#5149=FACE_OUTER_BOUND('',#8445,.T.);
#5150=FACE_OUTER_BOUND('',#8446,.T.);
#5151=FACE_OUTER_BOUND('',#8447,.T.);
#5152=FACE_OUTER_BOUND('',#8448,.T.);
#5153=FACE_OUTER_BOUND('',#8449,.T.);
#5154=FACE_OUTER_BOUND('',#8450,.T.);
#5155=FACE_OUTER_BOUND('',#8451,.T.);
#5156=FACE_OUTER_BOUND('',#8452,.T.);
#5157=FACE_OUTER_BOUND('',#8453,.T.);
#5158=FACE_OUTER_BOUND('',#8454,.T.);
#5159=FACE_OUTER_BOUND('',#8455,.T.);
#5160=FACE_OUTER_BOUND('',#8456,.T.);
#5161=FACE_OUTER_BOUND('',#8457,.T.);
#5162=FACE_OUTER_BOUND('',#8458,.T.);
#5163=FACE_OUTER_BOUND('',#8459,.T.);
#5164=FACE_OUTER_BOUND('',#8460,.T.);
#5165=FACE_OUTER_BOUND('',#8461,.T.);
#5166=FACE_OUTER_BOUND('',#8462,.T.);
#5167=FACE_OUTER_BOUND('',#8463,.T.);
#5168=FACE_OUTER_BOUND('',#8464,.T.);
#5169=FACE_OUTER_BOUND('',#8465,.T.);
#5170=FACE_OUTER_BOUND('',#8466,.T.);
#5171=FACE_OUTER_BOUND('',#8467,.T.);
#5172=FACE_OUTER_BOUND('',#8468,.T.);
#5173=FACE_OUTER_BOUND('',#8469,.T.);
#5174=FACE_OUTER_BOUND('',#8470,.T.);
#5175=FACE_OUTER_BOUND('',#8471,.T.);
#5176=FACE_OUTER_BOUND('',#8472,.T.);
#5177=FACE_OUTER_BOUND('',#8473,.T.);
#5178=FACE_OUTER_BOUND('',#8474,.T.);
#5179=FACE_OUTER_BOUND('',#8475,.T.);
#5180=FACE_OUTER_BOUND('',#8476,.T.);
#5181=FACE_OUTER_BOUND('',#8477,.T.);
#5182=FACE_OUTER_BOUND('',#8478,.T.);
#5183=FACE_OUTER_BOUND('',#8479,.T.);
#5184=FACE_OUTER_BOUND('',#8480,.T.);
#5185=FACE_OUTER_BOUND('',#8481,.T.);
#5186=FACE_OUTER_BOUND('',#8482,.T.);
#5187=FACE_OUTER_BOUND('',#8483,.T.);
#5188=FACE_OUTER_BOUND('',#8484,.T.);
#5189=FACE_OUTER_BOUND('',#8485,.T.);
#5190=FACE_OUTER_BOUND('',#8486,.T.);
#5191=FACE_OUTER_BOUND('',#8487,.T.);
#5192=FACE_OUTER_BOUND('',#8488,.T.);
#5193=FACE_OUTER_BOUND('',#8489,.T.);
#5194=FACE_OUTER_BOUND('',#8490,.T.);
#5195=FACE_OUTER_BOUND('',#8491,.T.);
#5196=FACE_OUTER_BOUND('',#8492,.T.);
#5197=FACE_OUTER_BOUND('',#8493,.T.);
#5198=FACE_OUTER_BOUND('',#8494,.T.);
#5199=FACE_OUTER_BOUND('',#8495,.T.);
#5200=FACE_OUTER_BOUND('',#8496,.T.);
#5201=FACE_OUTER_BOUND('',#8497,.T.);
#5202=FACE_OUTER_BOUND('',#8498,.T.);
#5203=FACE_OUTER_BOUND('',#8499,.T.);
#5204=FACE_OUTER_BOUND('',#8500,.T.);
#5205=FACE_OUTER_BOUND('',#8501,.T.);
#5206=FACE_OUTER_BOUND('',#8502,.T.);
#5207=FACE_OUTER_BOUND('',#8503,.T.);
#5208=FACE_OUTER_BOUND('',#8504,.T.);
#5209=FACE_OUTER_BOUND('',#8505,.T.);
#5210=FACE_OUTER_BOUND('',#8506,.T.);
#5211=FACE_OUTER_BOUND('',#8507,.T.);
#5212=FACE_OUTER_BOUND('',#8508,.T.);
#5213=FACE_OUTER_BOUND('',#8509,.T.);
#5214=FACE_OUTER_BOUND('',#8510,.T.);
#5215=FACE_OUTER_BOUND('',#8511,.T.);
#5216=FACE_OUTER_BOUND('',#8512,.T.);
#5217=FACE_OUTER_BOUND('',#8513,.T.);
#5218=FACE_OUTER_BOUND('',#8514,.T.);
#5219=FACE_OUTER_BOUND('',#8515,.T.);
#5220=FACE_OUTER_BOUND('',#8516,.T.);
#5221=FACE_OUTER_BOUND('',#8517,.T.);
#5222=FACE_OUTER_BOUND('',#8518,.T.);
#5223=FACE_OUTER_BOUND('',#8519,.T.);
#5224=FACE_OUTER_BOUND('',#8520,.T.);
#5225=FACE_OUTER_BOUND('',#8521,.T.);
#5226=FACE_OUTER_BOUND('',#8522,.T.);
#5227=FACE_OUTER_BOUND('',#8523,.T.);
#5228=FACE_OUTER_BOUND('',#8524,.T.);
#5229=FACE_OUTER_BOUND('',#8525,.T.);
#5230=FACE_OUTER_BOUND('',#8526,.T.);
#5231=FACE_OUTER_BOUND('',#8527,.T.);
#5232=FACE_OUTER_BOUND('',#8528,.T.);
#5233=FACE_OUTER_BOUND('',#8529,.T.);
#5234=FACE_OUTER_BOUND('',#8530,.T.);
#5235=FACE_OUTER_BOUND('',#8531,.T.);
#5236=FACE_OUTER_BOUND('',#8532,.T.);
#5237=FACE_OUTER_BOUND('',#8533,.T.);
#5238=FACE_OUTER_BOUND('',#8534,.T.);
#5239=FACE_OUTER_BOUND('',#8535,.T.);
#5240=FACE_OUTER_BOUND('',#8536,.T.);
#5241=FACE_OUTER_BOUND('',#8537,.T.);
#5242=FACE_OUTER_BOUND('',#8538,.T.);
#5243=FACE_OUTER_BOUND('',#8539,.T.);
#5244=FACE_OUTER_BOUND('',#8540,.T.);
#5245=FACE_OUTER_BOUND('',#8541,.T.);
#5246=FACE_OUTER_BOUND('',#8542,.T.);
#5247=FACE_OUTER_BOUND('',#8543,.T.);
#5248=FACE_OUTER_BOUND('',#8544,.T.);
#5249=FACE_OUTER_BOUND('',#8545,.T.);
#5250=FACE_OUTER_BOUND('',#8546,.T.);
#5251=FACE_OUTER_BOUND('',#8547,.T.);
#5252=FACE_OUTER_BOUND('',#8548,.T.);
#5253=FACE_OUTER_BOUND('',#8549,.T.);
#5254=FACE_OUTER_BOUND('',#8550,.T.);
#5255=FACE_OUTER_BOUND('',#8551,.T.);
#5256=FACE_OUTER_BOUND('',#8552,.T.);
#5257=FACE_OUTER_BOUND('',#8553,.T.);
#5258=FACE_OUTER_BOUND('',#8554,.T.);
#5259=FACE_OUTER_BOUND('',#8555,.T.);
#5260=FACE_OUTER_BOUND('',#8556,.T.);
#5261=FACE_OUTER_BOUND('',#8557,.T.);
#5262=FACE_OUTER_BOUND('',#8558,.T.);
#5263=FACE_OUTER_BOUND('',#8559,.T.);
#5264=FACE_OUTER_BOUND('',#8560,.T.);
#5265=FACE_OUTER_BOUND('',#8561,.T.);
#5266=FACE_OUTER_BOUND('',#8562,.T.);
#5267=FACE_OUTER_BOUND('',#8563,.T.);
#5268=FACE_OUTER_BOUND('',#8564,.T.);
#5269=FACE_OUTER_BOUND('',#8565,.T.);
#5270=FACE_OUTER_BOUND('',#8566,.T.);
#5271=FACE_OUTER_BOUND('',#8567,.T.);
#5272=FACE_OUTER_BOUND('',#8568,.T.);
#5273=FACE_OUTER_BOUND('',#8569,.T.);
#5274=FACE_OUTER_BOUND('',#8570,.T.);
#5275=FACE_OUTER_BOUND('',#8571,.T.);
#5276=FACE_OUTER_BOUND('',#8572,.T.);
#5277=FACE_OUTER_BOUND('',#8573,.T.);
#5278=FACE_OUTER_BOUND('',#8574,.T.);
#5279=FACE_OUTER_BOUND('',#8575,.T.);
#5280=FACE_OUTER_BOUND('',#8576,.T.);
#5281=FACE_OUTER_BOUND('',#8577,.T.);
#5282=FACE_OUTER_BOUND('',#8578,.T.);
#5283=FACE_OUTER_BOUND('',#8579,.T.);
#5284=FACE_OUTER_BOUND('',#8580,.T.);
#5285=FACE_OUTER_BOUND('',#8581,.T.);
#5286=FACE_OUTER_BOUND('',#8582,.T.);
#5287=FACE_OUTER_BOUND('',#8583,.T.);
#5288=FACE_OUTER_BOUND('',#8584,.T.);
#5289=FACE_OUTER_BOUND('',#8585,.T.);
#5290=FACE_OUTER_BOUND('',#8586,.T.);
#5291=FACE_OUTER_BOUND('',#8587,.T.);
#5292=FACE_OUTER_BOUND('',#8588,.T.);
#5293=FACE_OUTER_BOUND('',#8589,.T.);
#5294=FACE_OUTER_BOUND('',#8590,.T.);
#5295=FACE_OUTER_BOUND('',#8591,.T.);
#5296=FACE_OUTER_BOUND('',#8592,.T.);
#5297=FACE_OUTER_BOUND('',#8593,.T.);
#5298=FACE_OUTER_BOUND('',#8594,.T.);
#5299=FACE_OUTER_BOUND('',#8595,.T.);
#5300=FACE_OUTER_BOUND('',#8596,.T.);
#5301=FACE_OUTER_BOUND('',#8597,.T.);
#5302=FACE_OUTER_BOUND('',#8598,.T.);
#5303=FACE_OUTER_BOUND('',#8599,.T.);
#5304=FACE_OUTER_BOUND('',#8600,.T.);
#5305=FACE_OUTER_BOUND('',#8601,.T.);
#5306=FACE_OUTER_BOUND('',#8602,.T.);
#5307=FACE_OUTER_BOUND('',#8603,.T.);
#5308=FACE_OUTER_BOUND('',#8604,.T.);
#5309=FACE_OUTER_BOUND('',#8605,.T.);
#5310=FACE_OUTER_BOUND('',#8606,.T.);
#5311=FACE_OUTER_BOUND('',#8607,.T.);
#5312=FACE_OUTER_BOUND('',#8608,.T.);
#5313=FACE_OUTER_BOUND('',#8609,.T.);
#5314=FACE_OUTER_BOUND('',#8610,.T.);
#5315=FACE_OUTER_BOUND('',#8611,.T.);
#5316=FACE_OUTER_BOUND('',#8612,.T.);
#5317=FACE_OUTER_BOUND('',#8613,.T.);
#5318=FACE_OUTER_BOUND('',#8614,.T.);
#5319=FACE_OUTER_BOUND('',#8615,.T.);
#5320=FACE_OUTER_BOUND('',#8616,.T.);
#5321=FACE_OUTER_BOUND('',#8617,.T.);
#5322=FACE_OUTER_BOUND('',#8618,.T.);
#5323=FACE_OUTER_BOUND('',#8619,.T.);
#5324=FACE_OUTER_BOUND('',#8620,.T.);
#5325=FACE_OUTER_BOUND('',#8621,.T.);
#5326=FACE_OUTER_BOUND('',#8622,.T.);
#5327=FACE_OUTER_BOUND('',#8623,.T.);
#5328=FACE_OUTER_BOUND('',#8624,.T.);
#5329=FACE_OUTER_BOUND('',#8625,.T.);
#5330=FACE_OUTER_BOUND('',#8626,.T.);
#5331=FACE_OUTER_BOUND('',#8627,.T.);
#5332=FACE_OUTER_BOUND('',#8628,.T.);
#5333=FACE_OUTER_BOUND('',#8629,.T.);
#5334=FACE_OUTER_BOUND('',#8630,.T.);
#5335=FACE_OUTER_BOUND('',#8631,.T.);
#5336=FACE_OUTER_BOUND('',#8632,.T.);
#5337=FACE_OUTER_BOUND('',#8633,.T.);
#5338=FACE_OUTER_BOUND('',#8634,.T.);
#5339=FACE_OUTER_BOUND('',#8635,.T.);
#5340=FACE_OUTER_BOUND('',#8636,.T.);
#5341=FACE_OUTER_BOUND('',#8637,.T.);
#5342=FACE_OUTER_BOUND('',#8638,.T.);
#5343=FACE_OUTER_BOUND('',#8639,.T.);
#5344=FACE_OUTER_BOUND('',#8640,.T.);
#5345=FACE_OUTER_BOUND('',#8641,.T.);
#5346=FACE_OUTER_BOUND('',#8642,.T.);
#5347=FACE_OUTER_BOUND('',#8643,.T.);
#5348=FACE_OUTER_BOUND('',#8644,.T.);
#5349=FACE_OUTER_BOUND('',#8645,.T.);
#5350=FACE_OUTER_BOUND('',#8646,.T.);
#5351=FACE_OUTER_BOUND('',#8647,.T.);
#5352=FACE_OUTER_BOUND('',#8648,.T.);
#5353=FACE_OUTER_BOUND('',#8649,.T.);
#5354=FACE_OUTER_BOUND('',#8650,.T.);
#5355=FACE_OUTER_BOUND('',#8651,.T.);
#5356=FACE_OUTER_BOUND('',#8652,.T.);
#5357=FACE_OUTER_BOUND('',#8653,.T.);
#5358=FACE_OUTER_BOUND('',#8654,.T.);
#5359=FACE_OUTER_BOUND('',#8655,.T.);
#5360=FACE_OUTER_BOUND('',#8656,.T.);
#5361=FACE_OUTER_BOUND('',#8657,.T.);
#5362=FACE_OUTER_BOUND('',#8658,.T.);
#5363=FACE_OUTER_BOUND('',#8659,.T.);
#5364=FACE_OUTER_BOUND('',#8660,.T.);
#5365=FACE_OUTER_BOUND('',#8661,.T.);
#5366=FACE_OUTER_BOUND('',#8662,.T.);
#5367=FACE_OUTER_BOUND('',#8663,.T.);
#5368=FACE_OUTER_BOUND('',#8664,.T.);
#5369=FACE_OUTER_BOUND('',#8665,.T.);
#5370=FACE_OUTER_BOUND('',#8666,.T.);
#5371=FACE_OUTER_BOUND('',#8667,.T.);
#5372=FACE_OUTER_BOUND('',#8668,.T.);
#5373=FACE_OUTER_BOUND('',#8669,.T.);
#5374=FACE_OUTER_BOUND('',#8670,.T.);
#5375=FACE_OUTER_BOUND('',#8671,.T.);
#5376=FACE_OUTER_BOUND('',#8672,.T.);
#5377=FACE_OUTER_BOUND('',#8673,.T.);
#5378=FACE_OUTER_BOUND('',#8674,.T.);
#5379=FACE_OUTER_BOUND('',#8675,.T.);
#5380=FACE_OUTER_BOUND('',#8676,.T.);
#5381=FACE_OUTER_BOUND('',#8677,.T.);
#5382=FACE_OUTER_BOUND('',#8678,.T.);
#5383=FACE_OUTER_BOUND('',#8679,.T.);
#5384=FACE_OUTER_BOUND('',#8680,.T.);
#5385=FACE_OUTER_BOUND('',#8681,.T.);
#5386=FACE_OUTER_BOUND('',#8682,.T.);
#5387=FACE_OUTER_BOUND('',#8683,.T.);
#5388=FACE_OUTER_BOUND('',#8684,.T.);
#5389=FACE_OUTER_BOUND('',#8685,.T.);
#5390=FACE_OUTER_BOUND('',#8686,.T.);
#5391=FACE_OUTER_BOUND('',#8687,.T.);
#5392=FACE_OUTER_BOUND('',#8688,.T.);
#5393=FACE_OUTER_BOUND('',#8689,.T.);
#5394=FACE_OUTER_BOUND('',#8690,.T.);
#5395=FACE_OUTER_BOUND('',#8691,.T.);
#5396=FACE_OUTER_BOUND('',#8692,.T.);
#5397=FACE_OUTER_BOUND('',#8693,.T.);
#5398=FACE_OUTER_BOUND('',#8694,.T.);
#5399=FACE_OUTER_BOUND('',#8695,.T.);
#5400=FACE_OUTER_BOUND('',#8696,.T.);
#5401=FACE_OUTER_BOUND('',#8697,.T.);
#5402=FACE_OUTER_BOUND('',#8698,.T.);
#5403=FACE_OUTER_BOUND('',#8699,.T.);
#5404=FACE_OUTER_BOUND('',#8700,.T.);
#5405=FACE_OUTER_BOUND('',#8701,.T.);
#5406=FACE_OUTER_BOUND('',#8702,.T.);
#5407=FACE_OUTER_BOUND('',#8703,.T.);
#5408=FACE_OUTER_BOUND('',#8704,.T.);
#5409=FACE_OUTER_BOUND('',#8705,.T.);
#5410=FACE_OUTER_BOUND('',#8706,.T.);
#5411=FACE_OUTER_BOUND('',#8707,.T.);
#5412=FACE_OUTER_BOUND('',#8708,.T.);
#5413=FACE_OUTER_BOUND('',#8709,.T.);
#5414=FACE_OUTER_BOUND('',#8710,.T.);
#5415=FACE_OUTER_BOUND('',#8711,.T.);
#5416=FACE_OUTER_BOUND('',#8712,.T.);
#5417=FACE_OUTER_BOUND('',#8713,.T.);
#5418=FACE_OUTER_BOUND('',#8714,.T.);
#5419=FACE_OUTER_BOUND('',#8715,.T.);
#5420=FACE_OUTER_BOUND('',#8716,.T.);
#5421=FACE_OUTER_BOUND('',#8717,.T.);
#5422=FACE_OUTER_BOUND('',#8718,.T.);
#5423=FACE_OUTER_BOUND('',#8719,.T.);
#5424=FACE_OUTER_BOUND('',#8720,.T.);
#5425=FACE_OUTER_BOUND('',#8721,.T.);
#5426=FACE_OUTER_BOUND('',#8722,.T.);
#5427=FACE_OUTER_BOUND('',#8723,.T.);
#5428=FACE_OUTER_BOUND('',#8724,.T.);
#5429=FACE_OUTER_BOUND('',#8725,.T.);
#5430=FACE_OUTER_BOUND('',#8726,.T.);
#5431=FACE_OUTER_BOUND('',#8727,.T.);
#5432=FACE_OUTER_BOUND('',#8728,.T.);
#5433=FACE_OUTER_BOUND('',#8729,.T.);
#5434=FACE_OUTER_BOUND('',#8730,.T.);
#5435=FACE_OUTER_BOUND('',#8731,.T.);
#5436=FACE_OUTER_BOUND('',#8732,.T.);
#5437=FACE_OUTER_BOUND('',#8733,.T.);
#5438=FACE_OUTER_BOUND('',#8734,.T.);
#5439=FACE_OUTER_BOUND('',#8735,.T.);
#5440=FACE_OUTER_BOUND('',#8736,.T.);
#5441=FACE_OUTER_BOUND('',#8737,.T.);
#5442=FACE_OUTER_BOUND('',#8738,.T.);
#5443=FACE_OUTER_BOUND('',#8739,.T.);
#5444=FACE_OUTER_BOUND('',#8740,.T.);
#5445=FACE_OUTER_BOUND('',#8741,.T.);
#5446=FACE_OUTER_BOUND('',#8742,.T.);
#5447=FACE_OUTER_BOUND('',#8743,.T.);
#5448=FACE_OUTER_BOUND('',#8744,.T.);
#5449=FACE_OUTER_BOUND('',#8745,.T.);
#5450=FACE_OUTER_BOUND('',#8746,.T.);
#5451=FACE_OUTER_BOUND('',#8747,.T.);
#5452=FACE_OUTER_BOUND('',#8748,.T.);
#5453=FACE_OUTER_BOUND('',#8749,.T.);
#5454=FACE_OUTER_BOUND('',#8750,.T.);
#5455=FACE_OUTER_BOUND('',#8751,.T.);
#5456=FACE_OUTER_BOUND('',#8752,.T.);
#5457=FACE_OUTER_BOUND('',#8753,.T.);
#5458=FACE_OUTER_BOUND('',#8754,.T.);
#5459=FACE_OUTER_BOUND('',#8755,.T.);
#5460=FACE_OUTER_BOUND('',#8756,.T.);
#5461=FACE_OUTER_BOUND('',#8757,.T.);
#5462=FACE_OUTER_BOUND('',#8758,.T.);
#5463=FACE_OUTER_BOUND('',#8759,.T.);
#5464=FACE_OUTER_BOUND('',#8760,.T.);
#5465=FACE_OUTER_BOUND('',#8761,.T.);
#5466=FACE_OUTER_BOUND('',#8762,.T.);
#5467=FACE_OUTER_BOUND('',#8763,.T.);
#5468=FACE_OUTER_BOUND('',#8764,.T.);
#5469=FACE_OUTER_BOUND('',#8765,.T.);
#5470=FACE_OUTER_BOUND('',#8766,.T.);
#5471=FACE_OUTER_BOUND('',#8767,.T.);
#5472=FACE_OUTER_BOUND('',#8768,.T.);
#5473=FACE_OUTER_BOUND('',#8769,.T.);
#5474=FACE_OUTER_BOUND('',#8770,.T.);
#5475=FACE_OUTER_BOUND('',#8771,.T.);
#5476=FACE_OUTER_BOUND('',#8772,.T.);
#5477=FACE_OUTER_BOUND('',#8773,.T.);
#5478=FACE_OUTER_BOUND('',#8774,.T.);
#5479=FACE_OUTER_BOUND('',#8775,.T.);
#5480=FACE_OUTER_BOUND('',#8776,.T.);
#5481=FACE_OUTER_BOUND('',#8777,.T.);
#5482=FACE_OUTER_BOUND('',#8778,.T.);
#5483=FACE_OUTER_BOUND('',#8779,.T.);
#5484=FACE_OUTER_BOUND('',#8780,.T.);
#5485=FACE_OUTER_BOUND('',#8781,.T.);
#5486=FACE_OUTER_BOUND('',#8782,.T.);
#5487=FACE_OUTER_BOUND('',#8783,.T.);
#5488=FACE_OUTER_BOUND('',#8784,.T.);
#5489=FACE_OUTER_BOUND('',#8785,.T.);
#5490=FACE_OUTER_BOUND('',#8786,.T.);
#5491=FACE_OUTER_BOUND('',#8787,.T.);
#5492=FACE_OUTER_BOUND('',#8788,.T.);
#5493=FACE_OUTER_BOUND('',#8789,.T.);
#5494=FACE_OUTER_BOUND('',#8790,.T.);
#5495=FACE_OUTER_BOUND('',#8791,.T.);
#5496=FACE_OUTER_BOUND('',#8792,.T.);
#5497=FACE_OUTER_BOUND('',#8793,.T.);
#5498=FACE_OUTER_BOUND('',#8794,.T.);
#5499=FACE_OUTER_BOUND('',#8795,.T.);
#5500=FACE_OUTER_BOUND('',#8796,.T.);
#5501=FACE_OUTER_BOUND('',#8797,.T.);
#5502=FACE_OUTER_BOUND('',#8798,.T.);
#5503=FACE_OUTER_BOUND('',#8799,.T.);
#5504=FACE_OUTER_BOUND('',#8800,.T.);
#5505=FACE_OUTER_BOUND('',#8801,.T.);
#5506=FACE_OUTER_BOUND('',#8802,.T.);
#5507=FACE_OUTER_BOUND('',#8803,.T.);
#5508=FACE_OUTER_BOUND('',#8804,.T.);
#5509=FACE_OUTER_BOUND('',#8805,.T.);
#5510=FACE_OUTER_BOUND('',#8806,.T.);
#5511=FACE_OUTER_BOUND('',#8807,.T.);
#5512=FACE_OUTER_BOUND('',#8808,.T.);
#5513=FACE_OUTER_BOUND('',#8809,.T.);
#5514=FACE_OUTER_BOUND('',#8810,.T.);
#5515=FACE_OUTER_BOUND('',#8811,.T.);
#5516=FACE_OUTER_BOUND('',#8812,.T.);
#5517=FACE_OUTER_BOUND('',#8813,.T.);
#5518=FACE_OUTER_BOUND('',#8814,.T.);
#5519=FACE_OUTER_BOUND('',#8815,.T.);
#5520=FACE_OUTER_BOUND('',#8816,.T.);
#5521=FACE_OUTER_BOUND('',#8817,.T.);
#5522=FACE_OUTER_BOUND('',#8818,.T.);
#5523=FACE_OUTER_BOUND('',#8819,.T.);
#5524=FACE_OUTER_BOUND('',#8820,.T.);
#5525=FACE_OUTER_BOUND('',#8821,.T.);
#5526=FACE_OUTER_BOUND('',#8822,.T.);
#5527=FACE_OUTER_BOUND('',#8823,.T.);
#5528=FACE_OUTER_BOUND('',#8824,.T.);
#5529=FACE_OUTER_BOUND('',#8825,.T.);
#5530=FACE_OUTER_BOUND('',#8826,.T.);
#5531=FACE_OUTER_BOUND('',#8827,.T.);
#5532=FACE_OUTER_BOUND('',#8828,.T.);
#5533=FACE_OUTER_BOUND('',#8829,.T.);
#5534=FACE_OUTER_BOUND('',#8830,.T.);
#5535=FACE_OUTER_BOUND('',#8831,.T.);
#5536=FACE_OUTER_BOUND('',#8832,.T.);
#5537=FACE_OUTER_BOUND('',#8833,.T.);
#5538=FACE_OUTER_BOUND('',#8834,.T.);
#5539=FACE_OUTER_BOUND('',#8835,.T.);
#5540=FACE_OUTER_BOUND('',#8836,.T.);
#5541=FACE_OUTER_BOUND('',#8837,.T.);
#5542=FACE_OUTER_BOUND('',#8838,.T.);
#5543=FACE_OUTER_BOUND('',#8839,.T.);
#5544=FACE_OUTER_BOUND('',#8840,.T.);
#5545=FACE_OUTER_BOUND('',#8841,.T.);
#5546=FACE_OUTER_BOUND('',#8842,.T.);
#5547=FACE_OUTER_BOUND('',#8843,.T.);
#5548=FACE_OUTER_BOUND('',#8844,.T.);
#5549=FACE_OUTER_BOUND('',#8845,.T.);
#5550=FACE_OUTER_BOUND('',#8846,.T.);
#5551=FACE_OUTER_BOUND('',#8847,.T.);
#5552=FACE_OUTER_BOUND('',#8848,.T.);
#5553=FACE_OUTER_BOUND('',#8849,.T.);
#5554=FACE_OUTER_BOUND('',#8850,.T.);
#5555=FACE_OUTER_BOUND('',#8851,.T.);
#5556=FACE_OUTER_BOUND('',#8852,.T.);
#5557=FACE_OUTER_BOUND('',#8853,.T.);
#5558=FACE_OUTER_BOUND('',#8854,.T.);
#5559=FACE_OUTER_BOUND('',#8855,.T.);
#5560=FACE_OUTER_BOUND('',#8856,.T.);
#5561=FACE_OUTER_BOUND('',#8857,.T.);
#5562=FACE_OUTER_BOUND('',#8858,.T.);
#5563=FACE_OUTER_BOUND('',#8859,.T.);
#5564=FACE_OUTER_BOUND('',#8860,.T.);
#5565=FACE_OUTER_BOUND('',#8861,.T.);
#5566=FACE_OUTER_BOUND('',#8862,.T.);
#5567=FACE_OUTER_BOUND('',#8863,.T.);
#5568=FACE_OUTER_BOUND('',#8864,.T.);
#5569=FACE_OUTER_BOUND('',#8865,.T.);
#5570=FACE_OUTER_BOUND('',#8866,.T.);
#5571=FACE_OUTER_BOUND('',#8867,.T.);
#5572=FACE_OUTER_BOUND('',#8868,.T.);
#5573=FACE_OUTER_BOUND('',#8869,.T.);
#5574=FACE_OUTER_BOUND('',#8870,.T.);
#5575=FACE_OUTER_BOUND('',#8871,.T.);
#5576=FACE_OUTER_BOUND('',#8872,.T.);
#5577=FACE_OUTER_BOUND('',#8873,.T.);
#5578=FACE_OUTER_BOUND('',#8874,.T.);
#5579=FACE_OUTER_BOUND('',#8875,.T.);
#5580=FACE_OUTER_BOUND('',#8876,.T.);
#5581=FACE_OUTER_BOUND('',#8877,.T.);
#5582=FACE_OUTER_BOUND('',#8878,.T.);
#5583=FACE_OUTER_BOUND('',#8879,.T.);
#5584=FACE_OUTER_BOUND('',#8880,.T.);
#5585=FACE_OUTER_BOUND('',#8881,.T.);
#5586=FACE_OUTER_BOUND('',#8882,.T.);
#5587=FACE_OUTER_BOUND('',#8883,.T.);
#5588=FACE_OUTER_BOUND('',#8884,.T.);
#5589=FACE_OUTER_BOUND('',#8885,.T.);
#5590=FACE_OUTER_BOUND('',#8886,.T.);
#5591=FACE_OUTER_BOUND('',#8887,.T.);
#5592=FACE_OUTER_BOUND('',#8888,.T.);
#5593=FACE_OUTER_BOUND('',#8889,.T.);
#5594=FACE_OUTER_BOUND('',#8890,.T.);
#5595=FACE_OUTER_BOUND('',#8891,.T.);
#5596=FACE_OUTER_BOUND('',#8892,.T.);
#5597=FACE_OUTER_BOUND('',#8893,.T.);
#5598=FACE_OUTER_BOUND('',#8894,.T.);
#5599=FACE_OUTER_BOUND('',#8895,.T.);
#5600=FACE_OUTER_BOUND('',#8896,.T.);
#5601=FACE_OUTER_BOUND('',#8897,.T.);
#5602=FACE_OUTER_BOUND('',#8898,.T.);
#5603=FACE_OUTER_BOUND('',#8899,.T.);
#5604=FACE_OUTER_BOUND('',#8900,.T.);
#5605=FACE_OUTER_BOUND('',#8901,.T.);
#5606=FACE_OUTER_BOUND('',#8902,.T.);
#5607=FACE_OUTER_BOUND('',#8903,.T.);
#5608=FACE_OUTER_BOUND('',#8904,.T.);
#5609=FACE_OUTER_BOUND('',#8905,.T.);
#5610=FACE_OUTER_BOUND('',#8906,.T.);
#5611=FACE_OUTER_BOUND('',#8907,.T.);
#5612=FACE_OUTER_BOUND('',#8908,.T.);
#5613=FACE_OUTER_BOUND('',#8909,.T.);
#5614=FACE_OUTER_BOUND('',#8910,.T.);
#5615=FACE_OUTER_BOUND('',#8911,.T.);
#5616=FACE_OUTER_BOUND('',#8912,.T.);
#5617=FACE_OUTER_BOUND('',#8913,.T.);
#5618=FACE_OUTER_BOUND('',#8914,.T.);
#5619=FACE_OUTER_BOUND('',#8915,.T.);
#5620=FACE_OUTER_BOUND('',#8916,.T.);
#5621=FACE_OUTER_BOUND('',#8917,.T.);
#5622=FACE_OUTER_BOUND('',#8918,.T.);
#5623=FACE_OUTER_BOUND('',#8919,.T.);
#5624=FACE_OUTER_BOUND('',#8920,.T.);
#5625=FACE_OUTER_BOUND('',#8921,.T.);
#5626=FACE_OUTER_BOUND('',#8922,.T.);
#5627=FACE_OUTER_BOUND('',#8923,.T.);
#5628=FACE_OUTER_BOUND('',#8924,.T.);
#5629=FACE_OUTER_BOUND('',#8925,.T.);
#5630=FACE_OUTER_BOUND('',#8926,.T.);
#5631=FACE_OUTER_BOUND('',#8927,.T.);
#5632=FACE_OUTER_BOUND('',#8928,.T.);
#5633=FACE_OUTER_BOUND('',#8929,.T.);
#5634=FACE_OUTER_BOUND('',#8930,.T.);
#5635=FACE_OUTER_BOUND('',#8931,.T.);
#5636=FACE_OUTER_BOUND('',#8932,.T.);
#5637=FACE_OUTER_BOUND('',#8933,.T.);
#5638=FACE_OUTER_BOUND('',#8934,.T.);
#5639=FACE_OUTER_BOUND('',#8935,.T.);
#5640=FACE_OUTER_BOUND('',#8936,.T.);
#5641=FACE_OUTER_BOUND('',#8937,.T.);
#5642=FACE_OUTER_BOUND('',#8938,.T.);
#5643=FACE_OUTER_BOUND('',#8939,.T.);
#5644=FACE_OUTER_BOUND('',#8940,.T.);
#5645=FACE_OUTER_BOUND('',#8941,.T.);
#5646=FACE_OUTER_BOUND('',#8942,.T.);
#5647=FACE_OUTER_BOUND('',#8943,.T.);
#5648=FACE_OUTER_BOUND('',#8944,.T.);
#5649=FACE_OUTER_BOUND('',#8945,.T.);
#5650=FACE_OUTER_BOUND('',#8946,.T.);
#5651=FACE_OUTER_BOUND('',#8947,.T.);
#5652=FACE_OUTER_BOUND('',#8948,.T.);
#5653=FACE_OUTER_BOUND('',#8949,.T.);
#5654=FACE_OUTER_BOUND('',#8950,.T.);
#5655=FACE_OUTER_BOUND('',#8951,.T.);
#5656=FACE_OUTER_BOUND('',#8952,.T.);
#5657=FACE_OUTER_BOUND('',#8953,.T.);
#5658=FACE_OUTER_BOUND('',#8954,.T.);
#5659=FACE_OUTER_BOUND('',#8955,.T.);
#5660=FACE_OUTER_BOUND('',#8956,.T.);
#5661=FACE_OUTER_BOUND('',#8957,.T.);
#5662=FACE_OUTER_BOUND('',#8958,.T.);
#5663=FACE_OUTER_BOUND('',#8959,.T.);
#5664=FACE_OUTER_BOUND('',#8960,.T.);
#5665=FACE_OUTER_BOUND('',#8961,.T.);
#5666=FACE_OUTER_BOUND('',#8962,.T.);
#5667=FACE_OUTER_BOUND('',#8963,.T.);
#5668=FACE_OUTER_BOUND('',#8964,.T.);
#5669=FACE_OUTER_BOUND('',#8965,.T.);
#5670=FACE_OUTER_BOUND('',#8966,.T.);
#5671=FACE_OUTER_BOUND('',#8967,.T.);
#5672=FACE_OUTER_BOUND('',#8968,.T.);
#5673=FACE_OUTER_BOUND('',#8969,.T.);
#5674=FACE_OUTER_BOUND('',#8970,.T.);
#5675=FACE_OUTER_BOUND('',#8971,.T.);
#5676=FACE_OUTER_BOUND('',#8972,.T.);
#5677=FACE_OUTER_BOUND('',#8973,.T.);
#5678=FACE_OUTER_BOUND('',#8974,.T.);
#5679=FACE_OUTER_BOUND('',#8975,.T.);
#5680=FACE_OUTER_BOUND('',#8976,.T.);
#5681=FACE_OUTER_BOUND('',#8977,.T.);
#5682=FACE_OUTER_BOUND('',#8978,.T.);
#5683=FACE_OUTER_BOUND('',#8979,.T.);
#5684=FACE_OUTER_BOUND('',#8980,.T.);
#5685=FACE_OUTER_BOUND('',#8981,.T.);
#5686=FACE_OUTER_BOUND('',#8982,.T.);
#5687=FACE_OUTER_BOUND('',#8983,.T.);
#5688=FACE_OUTER_BOUND('',#8984,.T.);
#5689=FACE_OUTER_BOUND('',#8985,.T.);
#5690=FACE_OUTER_BOUND('',#8986,.T.);
#5691=FACE_OUTER_BOUND('',#8987,.T.);
#5692=FACE_OUTER_BOUND('',#8988,.T.);
#5693=FACE_OUTER_BOUND('',#8989,.T.);
#5694=FACE_OUTER_BOUND('',#8990,.T.);
#5695=FACE_OUTER_BOUND('',#8991,.T.);
#5696=FACE_OUTER_BOUND('',#8992,.T.);
#5697=FACE_OUTER_BOUND('',#8993,.T.);
#5698=FACE_OUTER_BOUND('',#8994,.T.);
#5699=FACE_OUTER_BOUND('',#8995,.T.);
#5700=FACE_OUTER_BOUND('',#8996,.T.);
#5701=FACE_OUTER_BOUND('',#8997,.T.);
#5702=FACE_OUTER_BOUND('',#8998,.T.);
#5703=FACE_OUTER_BOUND('',#8999,.T.);
#5704=FACE_OUTER_BOUND('',#9000,.T.);
#5705=FACE_OUTER_BOUND('',#9001,.T.);
#5706=FACE_OUTER_BOUND('',#9002,.T.);
#5707=FACE_OUTER_BOUND('',#9003,.T.);
#5708=FACE_OUTER_BOUND('',#9004,.T.);
#5709=FACE_OUTER_BOUND('',#9005,.T.);
#5710=FACE_OUTER_BOUND('',#9006,.T.);
#5711=FACE_OUTER_BOUND('',#9007,.T.);
#5712=FACE_OUTER_BOUND('',#9008,.T.);
#5713=FACE_OUTER_BOUND('',#9009,.T.);
#5714=FACE_OUTER_BOUND('',#9010,.T.);
#5715=FACE_OUTER_BOUND('',#9011,.T.);
#5716=FACE_OUTER_BOUND('',#9012,.T.);
#5717=FACE_OUTER_BOUND('',#9013,.T.);
#5718=FACE_OUTER_BOUND('',#9014,.T.);
#5719=FACE_OUTER_BOUND('',#9015,.T.);
#5720=FACE_OUTER_BOUND('',#9016,.T.);
#5721=FACE_OUTER_BOUND('',#9017,.T.);
#5722=FACE_OUTER_BOUND('',#9018,.T.);
#5723=FACE_OUTER_BOUND('',#9019,.T.);
#5724=FACE_OUTER_BOUND('',#9020,.T.);
#5725=FACE_OUTER_BOUND('',#9021,.T.);
#5726=FACE_OUTER_BOUND('',#9022,.T.);
#5727=FACE_OUTER_BOUND('',#9023,.T.);
#5728=FACE_OUTER_BOUND('',#9024,.T.);
#5729=FACE_OUTER_BOUND('',#9025,.T.);
#5730=FACE_OUTER_BOUND('',#9026,.T.);
#5731=FACE_OUTER_BOUND('',#9027,.T.);
#5732=FACE_OUTER_BOUND('',#9028,.T.);
#5733=FACE_OUTER_BOUND('',#9029,.T.);
#5734=FACE_OUTER_BOUND('',#9030,.T.);
#5735=FACE_OUTER_BOUND('',#9031,.T.);
#5736=FACE_OUTER_BOUND('',#9032,.T.);
#5737=FACE_OUTER_BOUND('',#9033,.T.);
#5738=FACE_OUTER_BOUND('',#9034,.T.);
#5739=FACE_OUTER_BOUND('',#9035,.T.);
#5740=FACE_OUTER_BOUND('',#9036,.T.);
#5741=FACE_OUTER_BOUND('',#9037,.T.);
#5742=FACE_OUTER_BOUND('',#9038,.T.);
#5743=FACE_OUTER_BOUND('',#9039,.T.);
#5744=FACE_OUTER_BOUND('',#9040,.T.);
#5745=FACE_OUTER_BOUND('',#9041,.T.);
#5746=FACE_OUTER_BOUND('',#9042,.T.);
#5747=FACE_OUTER_BOUND('',#9043,.T.);
#5748=FACE_OUTER_BOUND('',#9044,.T.);
#5749=FACE_OUTER_BOUND('',#9045,.T.);
#5750=FACE_OUTER_BOUND('',#9046,.T.);
#5751=FACE_OUTER_BOUND('',#9047,.T.);
#5752=FACE_OUTER_BOUND('',#9048,.T.);
#5753=FACE_OUTER_BOUND('',#9049,.T.);
#5754=FACE_OUTER_BOUND('',#9050,.T.);
#5755=FACE_OUTER_BOUND('',#9051,.T.);
#5756=FACE_OUTER_BOUND('',#9052,.T.);
#5757=FACE_OUTER_BOUND('',#9053,.T.);
#5758=FACE_OUTER_BOUND('',#9054,.T.);
#5759=FACE_OUTER_BOUND('',#9055,.T.);
#5760=FACE_OUTER_BOUND('',#9056,.T.);
#5761=FACE_OUTER_BOUND('',#9057,.T.);
#5762=FACE_OUTER_BOUND('',#9058,.T.);
#5763=FACE_OUTER_BOUND('',#9059,.T.);
#5764=FACE_OUTER_BOUND('',#9060,.T.);
#5765=FACE_OUTER_BOUND('',#9061,.T.);
#5766=FACE_OUTER_BOUND('',#9062,.T.);
#5767=FACE_OUTER_BOUND('',#9063,.T.);
#5768=FACE_OUTER_BOUND('',#9064,.T.);
#5769=FACE_OUTER_BOUND('',#9065,.T.);
#5770=FACE_OUTER_BOUND('',#9066,.T.);
#5771=FACE_OUTER_BOUND('',#9067,.T.);
#5772=FACE_OUTER_BOUND('',#9068,.T.);
#5773=FACE_OUTER_BOUND('',#9069,.T.);
#5774=FACE_OUTER_BOUND('',#9070,.T.);
#5775=FACE_OUTER_BOUND('',#9071,.T.);
#5776=FACE_OUTER_BOUND('',#9072,.T.);
#5777=FACE_OUTER_BOUND('',#9073,.T.);
#5778=FACE_OUTER_BOUND('',#9074,.T.);
#5779=FACE_OUTER_BOUND('',#9075,.T.);
#5780=FACE_OUTER_BOUND('',#9076,.T.);
#5781=FACE_OUTER_BOUND('',#9077,.T.);
#5782=FACE_OUTER_BOUND('',#9081,.T.);
#5783=FACE_OUTER_BOUND('',#9082,.T.);
#5784=FACE_OUTER_BOUND('',#9083,.T.);
#5785=FACE_OUTER_BOUND('',#9084,.T.);
#5786=FACE_OUTER_BOUND('',#9085,.T.);
#5787=FACE_OUTER_BOUND('',#9086,.T.);
#5788=FACE_OUTER_BOUND('',#9087,.T.);
#5789=FACE_OUTER_BOUND('',#9090,.T.);
#5790=FACE_OUTER_BOUND('',#9091,.T.);
#5791=FACE_OUTER_BOUND('',#9092,.T.);
#5792=FACE_OUTER_BOUND('',#9093,.T.);
#5793=FACE_OUTER_BOUND('',#9094,.T.);
#5794=FACE_OUTER_BOUND('',#9095,.T.);
#5795=FACE_OUTER_BOUND('',#9097,.T.);
#5796=FACE_OUTER_BOUND('',#9098,.T.);
#5797=FACE_OUTER_BOUND('',#9100,.T.);
#5798=FACE_OUTER_BOUND('',#9101,.T.);
#5799=FACE_OUTER_BOUND('',#9103,.T.);
#5800=FACE_OUTER_BOUND('',#9104,.T.);
#5801=FACE_OUTER_BOUND('',#9106,.T.);
#5802=FACE_OUTER_BOUND('',#9107,.T.);
#5803=FACE_OUTER_BOUND('',#9109,.T.);
#5804=FACE_OUTER_BOUND('',#9110,.T.);
#5805=FACE_OUTER_BOUND('',#9112,.T.);
#5806=FACE_OUTER_BOUND('',#9113,.T.);
#5807=FACE_OUTER_BOUND('',#9117,.T.);
#5808=FACE_OUTER_BOUND('',#9118,.T.);
#5809=FACE_OUTER_BOUND('',#9119,.T.);
#5810=FACE_OUTER_BOUND('',#9120,.T.);
#5811=FACE_OUTER_BOUND('',#9121,.T.);
#5812=FACE_OUTER_BOUND('',#9122,.T.);
#5813=FACE_OUTER_BOUND('',#9123,.T.);
#5814=FACE_OUTER_BOUND('',#9124,.T.);
#5815=FACE_OUTER_BOUND('',#9125,.T.);
#5816=FACE_OUTER_BOUND('',#9126,.T.);
#5817=FACE_OUTER_BOUND('',#9127,.T.);
#5818=FACE_OUTER_BOUND('',#9128,.T.);
#5819=FACE_OUTER_BOUND('',#9129,.T.);
#5820=FACE_OUTER_BOUND('',#9130,.T.);
#5821=FACE_OUTER_BOUND('',#9131,.T.);
#5822=FACE_OUTER_BOUND('',#9132,.T.);
#5823=FACE_OUTER_BOUND('',#9133,.T.);
#5824=FACE_OUTER_BOUND('',#9134,.T.);
#5825=FACE_OUTER_BOUND('',#9135,.T.);
#5826=FACE_OUTER_BOUND('',#9136,.T.);
#5827=FACE_OUTER_BOUND('',#9137,.T.);
#5828=FACE_OUTER_BOUND('',#9138,.T.);
#5829=FACE_OUTER_BOUND('',#9139,.T.);
#5830=FACE_OUTER_BOUND('',#9140,.T.);
#5831=FACE_OUTER_BOUND('',#9141,.T.);
#5832=FACE_OUTER_BOUND('',#9142,.T.);
#5833=FACE_OUTER_BOUND('',#9143,.T.);
#5834=FACE_OUTER_BOUND('',#9144,.T.);
#5835=FACE_OUTER_BOUND('',#9145,.T.);
#5836=FACE_OUTER_BOUND('',#9146,.T.);
#5837=FACE_OUTER_BOUND('',#9147,.T.);
#5838=FACE_OUTER_BOUND('',#9148,.T.);
#5839=FACE_OUTER_BOUND('',#9149,.T.);
#5840=FACE_OUTER_BOUND('',#9150,.T.);
#5841=FACE_OUTER_BOUND('',#9151,.T.);
#5842=FACE_OUTER_BOUND('',#9156,.T.);
#5843=FACE_OUTER_BOUND('',#9157,.T.);
#5844=FACE_OUTER_BOUND('',#9158,.T.);
#5845=FACE_OUTER_BOUND('',#9159,.T.);
#5846=FACE_OUTER_BOUND('',#9160,.T.);
#5847=FACE_OUTER_BOUND('',#9379,.T.);
#5848=FACE_OUTER_BOUND('',#9380,.T.);
#5849=FACE_OUTER_BOUND('',#9385,.T.);
#5850=FACE_OUTER_BOUND('',#9386,.T.);
#5851=FACE_OUTER_BOUND('',#9387,.T.);
#5852=FACE_OUTER_BOUND('',#9388,.T.);
#5853=FACE_OUTER_BOUND('',#9389,.T.);
#5854=FACE_OUTER_BOUND('',#9390,.T.);
#5855=FACE_OUTER_BOUND('',#9391,.T.);
#5856=FACE_OUTER_BOUND('',#9392,.T.);
#5857=FACE_OUTER_BOUND('',#9393,.T.);
#5858=FACE_OUTER_BOUND('',#9394,.T.);
#5859=FACE_OUTER_BOUND('',#9395,.T.);
#5860=FACE_OUTER_BOUND('',#9396,.T.);
#5861=FACE_OUTER_BOUND('',#9397,.T.);
#5862=FACE_OUTER_BOUND('',#9398,.T.);
#5863=FACE_OUTER_BOUND('',#9399,.T.);
#5864=FACE_OUTER_BOUND('',#9400,.T.);
#5865=FACE_OUTER_BOUND('',#9401,.T.);
#5866=FACE_OUTER_BOUND('',#9402,.T.);
#5867=FACE_OUTER_BOUND('',#9403,.T.);
#5868=FACE_OUTER_BOUND('',#9404,.T.);
#5869=FACE_OUTER_BOUND('',#9405,.T.);
#5870=FACE_OUTER_BOUND('',#9406,.T.);
#5871=FACE_OUTER_BOUND('',#9407,.T.);
#5872=FACE_OUTER_BOUND('',#9408,.T.);
#5873=FACE_OUTER_BOUND('',#9409,.T.);
#5874=FACE_OUTER_BOUND('',#9410,.T.);
#5875=FACE_OUTER_BOUND('',#9412,.T.);
#5876=FACE_OUTER_BOUND('',#9413,.T.);
#5877=FACE_OUTER_BOUND('',#9414,.T.);
#5878=FACE_OUTER_BOUND('',#9415,.T.);
#5879=FACE_OUTER_BOUND('',#9416,.T.);
#5880=FACE_OUTER_BOUND('',#9417,.T.);
#5881=FACE_OUTER_BOUND('',#9418,.T.);
#5882=FACE_OUTER_BOUND('',#9419,.T.);
#5883=FACE_OUTER_BOUND('',#9420,.T.);
#5884=FACE_OUTER_BOUND('',#9421,.T.);
#5885=FACE_OUTER_BOUND('',#9422,.T.);
#5886=FACE_OUTER_BOUND('',#9423,.T.);
#5887=FACE_OUTER_BOUND('',#9424,.T.);
#5888=FACE_OUTER_BOUND('',#9425,.T.);
#5889=FACE_OUTER_BOUND('',#9426,.T.);
#5890=FACE_OUTER_BOUND('',#9427,.T.);
#5891=FACE_OUTER_BOUND('',#9428,.T.);
#5892=FACE_OUTER_BOUND('',#9429,.T.);
#5893=FACE_OUTER_BOUND('',#9436,.T.);
#5894=FACE_OUTER_BOUND('',#9437,.T.);
#5895=FACE_OUTER_BOUND('',#9438,.T.);
#5896=FACE_OUTER_BOUND('',#9439,.T.);
#5897=FACE_OUTER_BOUND('',#9440,.T.);
#5898=FACE_OUTER_BOUND('',#9441,.T.);
#5899=FACE_OUTER_BOUND('',#9442,.T.);
#5900=FACE_OUTER_BOUND('',#9443,.T.);
#5901=FACE_OUTER_BOUND('',#9444,.T.);
#5902=FACE_OUTER_BOUND('',#9445,.T.);
#5903=FACE_OUTER_BOUND('',#9446,.T.);
#5904=FACE_OUTER_BOUND('',#9447,.T.);
#5905=FACE_OUTER_BOUND('',#9448,.T.);
#5906=FACE_OUTER_BOUND('',#9449,.T.);
#5907=FACE_OUTER_BOUND('',#9450,.T.);
#5908=FACE_OUTER_BOUND('',#9451,.T.);
#5909=FACE_OUTER_BOUND('',#9452,.T.);
#5910=FACE_OUTER_BOUND('',#9453,.T.);
#5911=FACE_OUTER_BOUND('',#9454,.T.);
#5912=FACE_OUTER_BOUND('',#9455,.T.);
#5913=FACE_OUTER_BOUND('',#9456,.T.);
#5914=FACE_OUTER_BOUND('',#9457,.T.);
#5915=FACE_OUTER_BOUND('',#9458,.T.);
#5916=FACE_OUTER_BOUND('',#9459,.T.);
#5917=FACE_OUTER_BOUND('',#9460,.T.);
#5918=FACE_OUTER_BOUND('',#9461,.T.);
#5919=FACE_OUTER_BOUND('',#9463,.T.);
#5920=FACE_OUTER_BOUND('',#9464,.T.);
#5921=FACE_OUTER_BOUND('',#9465,.T.);
#5922=FACE_OUTER_BOUND('',#9466,.T.);
#5923=FACE_OUTER_BOUND('',#9467,.T.);
#5924=FACE_OUTER_BOUND('',#9468,.T.);
#5925=FACE_OUTER_BOUND('',#9469,.T.);
#5926=FACE_OUTER_BOUND('',#9473,.T.);
#5927=FACE_OUTER_BOUND('',#9474,.T.);
#5928=FACE_OUTER_BOUND('',#9475,.T.);
#5929=FACE_OUTER_BOUND('',#9476,.T.);
#5930=FACE_OUTER_BOUND('',#9477,.T.);
#5931=FACE_OUTER_BOUND('',#9478,.T.);
#5932=FACE_OUTER_BOUND('',#9479,.T.);
#5933=FACE_OUTER_BOUND('',#9480,.T.);
#5934=FACE_OUTER_BOUND('',#9481,.T.);
#5935=FACE_OUTER_BOUND('',#9482,.T.);
#5936=FACE_OUTER_BOUND('',#9483,.T.);
#5937=FACE_OUTER_BOUND('',#9484,.T.);
#5938=FACE_OUTER_BOUND('',#9485,.T.);
#5939=FACE_OUTER_BOUND('',#9486,.T.);
#5940=FACE_OUTER_BOUND('',#9487,.T.);
#5941=FACE_OUTER_BOUND('',#9488,.T.);
#5942=FACE_OUTER_BOUND('',#9489,.T.);
#5943=FACE_OUTER_BOUND('',#9490,.T.);
#5944=FACE_OUTER_BOUND('',#9491,.T.);
#5945=FACE_OUTER_BOUND('',#9492,.T.);
#5946=FACE_OUTER_BOUND('',#9493,.T.);
#5947=FACE_OUTER_BOUND('',#9494,.T.);
#5948=FACE_OUTER_BOUND('',#9495,.T.);
#5949=FACE_OUTER_BOUND('',#9496,.T.);
#5950=FACE_OUTER_BOUND('',#9497,.T.);
#5951=FACE_OUTER_BOUND('',#9498,.T.);
#5952=FACE_OUTER_BOUND('',#9499,.T.);
#5953=FACE_OUTER_BOUND('',#9500,.T.);
#5954=FACE_OUTER_BOUND('',#9501,.T.);
#5955=FACE_OUTER_BOUND('',#9502,.T.);
#5956=FACE_OUTER_BOUND('',#9503,.T.);
#5957=FACE_OUTER_BOUND('',#9504,.T.);
#5958=FACE_OUTER_BOUND('',#9505,.T.);
#5959=FACE_OUTER_BOUND('',#9506,.T.);
#5960=FACE_OUTER_BOUND('',#9507,.T.);
#5961=FACE_OUTER_BOUND('',#9508,.T.);
#5962=FACE_OUTER_BOUND('',#9509,.T.);
#5963=FACE_OUTER_BOUND('',#9510,.T.);
#5964=FACE_OUTER_BOUND('',#9511,.T.);
#5965=FACE_OUTER_BOUND('',#9515,.T.);
#5966=FACE_OUTER_BOUND('',#9516,.T.);
#5967=FACE_OUTER_BOUND('',#9517,.T.);
#5968=FACE_OUTER_BOUND('',#9518,.T.);
#5969=FACE_OUTER_BOUND('',#9519,.T.);
#5970=FACE_OUTER_BOUND('',#9520,.T.);
#5971=FACE_OUTER_BOUND('',#9521,.T.);
#5972=FACE_OUTER_BOUND('',#9522,.T.);
#5973=FACE_OUTER_BOUND('',#9523,.T.);
#5974=FACE_OUTER_BOUND('',#9524,.T.);
#5975=FACE_OUTER_BOUND('',#9525,.T.);
#5976=FACE_OUTER_BOUND('',#9528,.T.);
#5977=FACE_OUTER_BOUND('',#9529,.T.);
#5978=FACE_OUTER_BOUND('',#9530,.T.);
#5979=FACE_OUTER_BOUND('',#9531,.T.);
#5980=FACE_OUTER_BOUND('',#9532,.T.);
#5981=FACE_OUTER_BOUND('',#9533,.T.);
#5982=FACE_OUTER_BOUND('',#9534,.T.);
#5983=FACE_OUTER_BOUND('',#9535,.T.);
#5984=FACE_OUTER_BOUND('',#9536,.T.);
#5985=FACE_OUTER_BOUND('',#9537,.T.);
#5986=FACE_OUTER_BOUND('',#9538,.T.);
#5987=FACE_OUTER_BOUND('',#9539,.T.);
#5988=FACE_OUTER_BOUND('',#9540,.T.);
#5989=FACE_OUTER_BOUND('',#9541,.T.);
#5990=FACE_OUTER_BOUND('',#9542,.T.);
#5991=FACE_OUTER_BOUND('',#9543,.T.);
#5992=FACE_OUTER_BOUND('',#9544,.T.);
#5993=FACE_OUTER_BOUND('',#9545,.T.);
#5994=FACE_OUTER_BOUND('',#9546,.T.);
#5995=FACE_OUTER_BOUND('',#9547,.T.);
#5996=FACE_OUTER_BOUND('',#9548,.T.);
#5997=FACE_OUTER_BOUND('',#9549,.T.);
#5998=FACE_OUTER_BOUND('',#9550,.T.);
#5999=FACE_OUTER_BOUND('',#9551,.T.);
#6000=FACE_OUTER_BOUND('',#9552,.T.);
#6001=FACE_OUTER_BOUND('',#9553,.T.);
#6002=FACE_OUTER_BOUND('',#9554,.T.);
#6003=FACE_OUTER_BOUND('',#9555,.T.);
#6004=FACE_OUTER_BOUND('',#9556,.T.);
#6005=FACE_OUTER_BOUND('',#9557,.T.);
#6006=FACE_OUTER_BOUND('',#9558,.T.);
#6007=FACE_OUTER_BOUND('',#9559,.T.);
#6008=FACE_OUTER_BOUND('',#9560,.T.);
#6009=FACE_OUTER_BOUND('',#9561,.T.);
#6010=FACE_OUTER_BOUND('',#9562,.T.);
#6011=FACE_OUTER_BOUND('',#9563,.T.);
#6012=FACE_OUTER_BOUND('',#9564,.T.);
#6013=FACE_OUTER_BOUND('',#9565,.T.);
#6014=FACE_OUTER_BOUND('',#9566,.T.);
#6015=FACE_OUTER_BOUND('',#9567,.T.);
#6016=FACE_OUTER_BOUND('',#9568,.T.);
#6017=FACE_OUTER_BOUND('',#9569,.T.);
#6018=FACE_OUTER_BOUND('',#9570,.T.);
#6019=FACE_OUTER_BOUND('',#9571,.T.);
#6020=FACE_OUTER_BOUND('',#9572,.T.);
#6021=FACE_OUTER_BOUND('',#9573,.T.);
#6022=FACE_OUTER_BOUND('',#9574,.T.);
#6023=FACE_OUTER_BOUND('',#9575,.T.);
#6024=FACE_OUTER_BOUND('',#9576,.T.);
#6025=FACE_OUTER_BOUND('',#9577,.T.);
#6026=FACE_OUTER_BOUND('',#9578,.T.);
#6027=FACE_OUTER_BOUND('',#9579,.T.);
#6028=FACE_OUTER_BOUND('',#9580,.T.);
#6029=FACE_OUTER_BOUND('',#9581,.T.);
#6030=FACE_OUTER_BOUND('',#9582,.T.);
#6031=FACE_OUTER_BOUND('',#9583,.T.);
#6032=FACE_OUTER_BOUND('',#9584,.T.);
#6033=FACE_OUTER_BOUND('',#9585,.T.);
#6034=FACE_OUTER_BOUND('',#9586,.T.);
#6035=FACE_OUTER_BOUND('',#9587,.T.);
#6036=FACE_OUTER_BOUND('',#9588,.T.);
#6037=FACE_OUTER_BOUND('',#9589,.T.);
#6038=FACE_OUTER_BOUND('',#9590,.T.);
#6039=FACE_OUTER_BOUND('',#9591,.T.);
#6040=FACE_OUTER_BOUND('',#9592,.T.);
#6041=FACE_OUTER_BOUND('',#9593,.T.);
#6042=FACE_OUTER_BOUND('',#9594,.T.);
#6043=FACE_OUTER_BOUND('',#9595,.T.);
#6044=FACE_OUTER_BOUND('',#9596,.T.);
#6045=FACE_OUTER_BOUND('',#9597,.T.);
#6046=FACE_OUTER_BOUND('',#9598,.T.);
#6047=FACE_OUTER_BOUND('',#9599,.T.);
#6048=FACE_OUTER_BOUND('',#9600,.T.);
#6049=FACE_OUTER_BOUND('',#9601,.T.);
#6050=FACE_OUTER_BOUND('',#9602,.T.);
#6051=FACE_OUTER_BOUND('',#9603,.T.);
#6052=FACE_OUTER_BOUND('',#9604,.T.);
#6053=FACE_OUTER_BOUND('',#9605,.T.);
#6054=FACE_OUTER_BOUND('',#9606,.T.);
#6055=FACE_OUTER_BOUND('',#9607,.T.);
#6056=FACE_OUTER_BOUND('',#9608,.T.);
#6057=FACE_OUTER_BOUND('',#9609,.T.);
#6058=FACE_OUTER_BOUND('',#9610,.T.);
#6059=FACE_OUTER_BOUND('',#9611,.T.);
#6060=FACE_OUTER_BOUND('',#9612,.T.);
#6061=FACE_OUTER_BOUND('',#9613,.T.);
#6062=FACE_OUTER_BOUND('',#9614,.T.);
#6063=FACE_OUTER_BOUND('',#9615,.T.);
#6064=FACE_OUTER_BOUND('',#9616,.T.);
#6065=FACE_OUTER_BOUND('',#9617,.T.);
#6066=FACE_OUTER_BOUND('',#9618,.T.);
#6067=FACE_OUTER_BOUND('',#9619,.T.);
#6068=FACE_OUTER_BOUND('',#9620,.T.);
#6069=FACE_OUTER_BOUND('',#9621,.T.);
#6070=FACE_OUTER_BOUND('',#9622,.T.);
#6071=FACE_OUTER_BOUND('',#9623,.T.);
#6072=FACE_OUTER_BOUND('',#9624,.T.);
#6073=FACE_OUTER_BOUND('',#9625,.T.);
#6074=FACE_OUTER_BOUND('',#9626,.T.);
#6075=FACE_OUTER_BOUND('',#9627,.T.);
#6076=FACE_OUTER_BOUND('',#9628,.T.);
#6077=FACE_OUTER_BOUND('',#9629,.T.);
#6078=FACE_OUTER_BOUND('',#9630,.T.);
#6079=FACE_OUTER_BOUND('',#9632,.T.);
#6080=FACE_OUTER_BOUND('',#9634,.T.);
#6081=FACE_OUTER_BOUND('',#9636,.T.);
#6082=FACE_OUTER_BOUND('',#9638,.T.);
#6083=FACE_OUTER_BOUND('',#9639,.T.);
#6084=FACE_OUTER_BOUND('',#9641,.T.);
#6085=FACE_OUTER_BOUND('',#9642,.T.);
#6086=FACE_OUTER_BOUND('',#9643,.T.);
#6087=FACE_OUTER_BOUND('',#9644,.T.);
#6088=FACE_OUTER_BOUND('',#9645,.T.);
#6089=FACE_OUTER_BOUND('',#9646,.T.);
#6090=FACE_OUTER_BOUND('',#9647,.T.);
#6091=FACE_OUTER_BOUND('',#9648,.T.);
#6092=FACE_OUTER_BOUND('',#9649,.T.);
#6093=FACE_OUTER_BOUND('',#9650,.T.);
#6094=FACE_OUTER_BOUND('',#9651,.T.);
#6095=FACE_OUTER_BOUND('',#9652,.T.);
#6096=FACE_OUTER_BOUND('',#9653,.T.);
#6097=FACE_OUTER_BOUND('',#9654,.T.);
#6098=FACE_OUTER_BOUND('',#9655,.T.);
#6099=FACE_OUTER_BOUND('',#9656,.T.);
#6100=FACE_OUTER_BOUND('',#9657,.T.);
#6101=FACE_OUTER_BOUND('',#9658,.T.);
#6102=FACE_OUTER_BOUND('',#9659,.T.);
#6103=FACE_OUTER_BOUND('',#9660,.T.);
#6104=FACE_OUTER_BOUND('',#9661,.T.);
#6105=FACE_OUTER_BOUND('',#9662,.T.);
#6106=FACE_OUTER_BOUND('',#9663,.T.);
#6107=FACE_OUTER_BOUND('',#9664,.T.);
#6108=FACE_OUTER_BOUND('',#9665,.T.);
#6109=FACE_OUTER_BOUND('',#9666,.T.);
#6110=FACE_OUTER_BOUND('',#9667,.T.);
#6111=FACE_OUTER_BOUND('',#9668,.T.);
#6112=FACE_OUTER_BOUND('',#9669,.T.);
#6113=FACE_OUTER_BOUND('',#9670,.T.);
#6114=FACE_OUTER_BOUND('',#9671,.T.);
#6115=FACE_OUTER_BOUND('',#9672,.T.);
#6116=FACE_OUTER_BOUND('',#9673,.T.);
#6117=FACE_OUTER_BOUND('',#9674,.T.);
#6118=FACE_OUTER_BOUND('',#9675,.T.);
#6119=FACE_OUTER_BOUND('',#9676,.T.);
#6120=FACE_OUTER_BOUND('',#9677,.T.);
#6121=FACE_OUTER_BOUND('',#9678,.T.);
#6122=FACE_OUTER_BOUND('',#9679,.T.);
#6123=FACE_OUTER_BOUND('',#9680,.T.);
#6124=FACE_OUTER_BOUND('',#9681,.T.);
#6125=FACE_OUTER_BOUND('',#9682,.T.);
#6126=FACE_OUTER_BOUND('',#9683,.T.);
#6127=FACE_OUTER_BOUND('',#9684,.T.);
#6128=FACE_OUTER_BOUND('',#9685,.T.);
#6129=FACE_OUTER_BOUND('',#9686,.T.);
#6130=FACE_OUTER_BOUND('',#9687,.T.);
#6131=FACE_OUTER_BOUND('',#9688,.T.);
#6132=FACE_OUTER_BOUND('',#9689,.T.);
#6133=FACE_OUTER_BOUND('',#9690,.T.);
#6134=FACE_OUTER_BOUND('',#9691,.T.);
#6135=FACE_OUTER_BOUND('',#9692,.T.);
#6136=FACE_OUTER_BOUND('',#9693,.T.);
#6137=FACE_OUTER_BOUND('',#9694,.T.);
#6138=FACE_OUTER_BOUND('',#9695,.T.);
#6139=FACE_OUTER_BOUND('',#9696,.T.);
#6140=FACE_OUTER_BOUND('',#9697,.T.);
#6141=FACE_OUTER_BOUND('',#9698,.T.);
#6142=FACE_OUTER_BOUND('',#9699,.T.);
#6143=FACE_OUTER_BOUND('',#9700,.T.);
#6144=FACE_OUTER_BOUND('',#9701,.T.);
#6145=FACE_OUTER_BOUND('',#9702,.T.);
#6146=FACE_OUTER_BOUND('',#9703,.T.);
#6147=FACE_OUTER_BOUND('',#9704,.T.);
#6148=FACE_OUTER_BOUND('',#9705,.T.);
#6149=FACE_OUTER_BOUND('',#9706,.T.);
#6150=FACE_OUTER_BOUND('',#9707,.T.);
#6151=FACE_OUTER_BOUND('',#9708,.T.);
#6152=FACE_OUTER_BOUND('',#9709,.T.);
#6153=FACE_OUTER_BOUND('',#9710,.T.);
#6154=FACE_OUTER_BOUND('',#9711,.T.);
#6155=FACE_OUTER_BOUND('',#9712,.T.);
#6156=FACE_OUTER_BOUND('',#9713,.T.);
#6157=FACE_OUTER_BOUND('',#9714,.T.);
#6158=FACE_OUTER_BOUND('',#9715,.T.);
#6159=FACE_OUTER_BOUND('',#9716,.T.);
#6160=FACE_OUTER_BOUND('',#9717,.T.);
#6161=FACE_OUTER_BOUND('',#9718,.T.);
#6162=FACE_OUTER_BOUND('',#9719,.T.);
#6163=FACE_OUTER_BOUND('',#9720,.T.);
#6164=FACE_OUTER_BOUND('',#9721,.T.);
#6165=FACE_OUTER_BOUND('',#9722,.T.);
#6166=FACE_OUTER_BOUND('',#9723,.T.);
#6167=FACE_OUTER_BOUND('',#9724,.T.);
#6168=FACE_OUTER_BOUND('',#9725,.T.);
#6169=FACE_OUTER_BOUND('',#9726,.T.);
#6170=FACE_OUTER_BOUND('',#9727,.T.);
#6171=FACE_OUTER_BOUND('',#9728,.T.);
#6172=FACE_OUTER_BOUND('',#9729,.T.);
#6173=FACE_OUTER_BOUND('',#9730,.T.);
#6174=FACE_OUTER_BOUND('',#9731,.T.);
#6175=FACE_OUTER_BOUND('',#9732,.T.);
#6176=FACE_OUTER_BOUND('',#9733,.T.);
#6177=FACE_OUTER_BOUND('',#9734,.T.);
#6178=FACE_OUTER_BOUND('',#9735,.T.);
#6179=FACE_OUTER_BOUND('',#9736,.T.);
#6180=FACE_OUTER_BOUND('',#9737,.T.);
#6181=FACE_OUTER_BOUND('',#9738,.T.);
#6182=FACE_OUTER_BOUND('',#9739,.T.);
#6183=FACE_OUTER_BOUND('',#9740,.T.);
#6184=FACE_OUTER_BOUND('',#9741,.T.);
#6185=FACE_OUTER_BOUND('',#9742,.T.);
#6186=FACE_OUTER_BOUND('',#9743,.T.);
#6187=FACE_OUTER_BOUND('',#9744,.T.);
#6188=FACE_OUTER_BOUND('',#9745,.T.);
#6189=FACE_OUTER_BOUND('',#9746,.T.);
#6190=FACE_OUTER_BOUND('',#9747,.T.);
#6191=FACE_OUTER_BOUND('',#9748,.T.);
#6192=FACE_OUTER_BOUND('',#9749,.T.);
#6193=FACE_OUTER_BOUND('',#9750,.T.);
#6194=FACE_OUTER_BOUND('',#9751,.T.);
#6195=FACE_OUTER_BOUND('',#9752,.T.);
#6196=FACE_OUTER_BOUND('',#9753,.T.);
#6197=FACE_OUTER_BOUND('',#9754,.T.);
#6198=FACE_OUTER_BOUND('',#9755,.T.);
#6199=FACE_OUTER_BOUND('',#9756,.T.);
#6200=FACE_OUTER_BOUND('',#9757,.T.);
#6201=FACE_OUTER_BOUND('',#9758,.T.);
#6202=FACE_OUTER_BOUND('',#9759,.T.);
#6203=FACE_OUTER_BOUND('',#9760,.T.);
#6204=FACE_OUTER_BOUND('',#9761,.T.);
#6205=FACE_OUTER_BOUND('',#9762,.T.);
#6206=FACE_OUTER_BOUND('',#9763,.T.);
#6207=FACE_OUTER_BOUND('',#9764,.T.);
#6208=FACE_OUTER_BOUND('',#9765,.T.);
#6209=FACE_OUTER_BOUND('',#9766,.T.);
#6210=FACE_OUTER_BOUND('',#9768,.T.);
#6211=FACE_OUTER_BOUND('',#9769,.T.);
#6212=FACE_OUTER_BOUND('',#9770,.T.);
#6213=FACE_OUTER_BOUND('',#9771,.T.);
#6214=FACE_OUTER_BOUND('',#9773,.T.);
#6215=FACE_OUTER_BOUND('',#9775,.T.);
#6216=FACE_OUTER_BOUND('',#9776,.T.);
#6217=FACE_OUTER_BOUND('',#9778,.T.);
#6218=FACE_OUTER_BOUND('',#9779,.T.);
#6219=FACE_OUTER_BOUND('',#9781,.T.);
#6220=FACE_OUTER_BOUND('',#9782,.T.);
#6221=FACE_OUTER_BOUND('',#9783,.T.);
#6222=FACE_OUTER_BOUND('',#9784,.T.);
#6223=FACE_OUTER_BOUND('',#9786,.T.);
#6224=FACE_OUTER_BOUND('',#9787,.T.);
#6225=FACE_OUTER_BOUND('',#9789,.T.);
#6226=FACE_OUTER_BOUND('',#9790,.T.);
#6227=FACE_OUTER_BOUND('',#9791,.T.);
#6228=FACE_OUTER_BOUND('',#9793,.T.);
#6229=FACE_OUTER_BOUND('',#9794,.T.);
#6230=FACE_OUTER_BOUND('',#9795,.T.);
#6231=FACE_OUTER_BOUND('',#9797,.T.);
#6232=FACE_OUTER_BOUND('',#9798,.T.);
#6233=FACE_OUTER_BOUND('',#9799,.T.);
#6234=FACE_OUTER_BOUND('',#9800,.T.);
#6235=FACE_OUTER_BOUND('',#9801,.T.);
#6236=FACE_OUTER_BOUND('',#9803,.T.);
#6237=FACE_OUTER_BOUND('',#9804,.T.);
#6238=FACE_OUTER_BOUND('',#9805,.T.);
#6239=FACE_OUTER_BOUND('',#9807,.T.);
#6240=FACE_OUTER_BOUND('',#9809,.T.);
#6241=FACE_OUTER_BOUND('',#9811,.T.);
#6242=FACE_OUTER_BOUND('',#9812,.T.);
#6243=FACE_OUTER_BOUND('',#9813,.T.);
#6244=FACE_OUTER_BOUND('',#9814,.T.);
#6245=FACE_OUTER_BOUND('',#9815,.T.);
#6246=FACE_OUTER_BOUND('',#9818,.T.);
#6247=FACE_OUTER_BOUND('',#9819,.T.);
#6248=FACE_OUTER_BOUND('',#9820,.T.);
#6249=FACE_OUTER_BOUND('',#9821,.T.);
#6250=FACE_OUTER_BOUND('',#9822,.T.);
#6251=FACE_OUTER_BOUND('',#9823,.T.);
#6252=FACE_OUTER_BOUND('',#9824,.T.);
#6253=FACE_OUTER_BOUND('',#9825,.T.);
#6254=FACE_OUTER_BOUND('',#9826,.T.);
#6255=FACE_OUTER_BOUND('',#9827,.T.);
#6256=FACE_OUTER_BOUND('',#9828,.T.);
#6257=FACE_OUTER_BOUND('',#9829,.T.);
#6258=FACE_OUTER_BOUND('',#9830,.T.);
#6259=FACE_OUTER_BOUND('',#9831,.T.);
#6260=FACE_OUTER_BOUND('',#9832,.T.);
#6261=FACE_OUTER_BOUND('',#9833,.T.);
#6262=FACE_OUTER_BOUND('',#9834,.T.);
#6263=FACE_OUTER_BOUND('',#9835,.T.);
#6264=FACE_OUTER_BOUND('',#9836,.T.);
#6265=FACE_OUTER_BOUND('',#9837,.T.);
#6266=FACE_OUTER_BOUND('',#9838,.T.);
#6267=FACE_OUTER_BOUND('',#9839,.T.);
#6268=FACE_OUTER_BOUND('',#9840,.T.);
#6269=FACE_OUTER_BOUND('',#9841,.T.);
#6270=FACE_OUTER_BOUND('',#9842,.T.);
#6271=FACE_OUTER_BOUND('',#9843,.T.);
#6272=FACE_OUTER_BOUND('',#9844,.T.);
#6273=FACE_OUTER_BOUND('',#9845,.T.);
#6274=FACE_OUTER_BOUND('',#9846,.T.);
#6275=FACE_OUTER_BOUND('',#9847,.T.);
#6276=FACE_OUTER_BOUND('',#9848,.T.);
#6277=FACE_OUTER_BOUND('',#9849,.T.);
#6278=FACE_OUTER_BOUND('',#9850,.T.);
#6279=FACE_OUTER_BOUND('',#9851,.T.);
#6280=FACE_OUTER_BOUND('',#9852,.T.);
#6281=FACE_OUTER_BOUND('',#9853,.T.);
#6282=FACE_OUTER_BOUND('',#9854,.T.);
#6283=FACE_OUTER_BOUND('',#9855,.T.);
#6284=FACE_OUTER_BOUND('',#9856,.T.);
#6285=FACE_OUTER_BOUND('',#9857,.T.);
#6286=FACE_OUTER_BOUND('',#9858,.T.);
#6287=FACE_OUTER_BOUND('',#9859,.T.);
#6288=FACE_OUTER_BOUND('',#9860,.T.);
#6289=FACE_OUTER_BOUND('',#9861,.T.);
#6290=FACE_OUTER_BOUND('',#9862,.T.);
#6291=FACE_OUTER_BOUND('',#9863,.T.);
#6292=FACE_OUTER_BOUND('',#9864,.T.);
#6293=FACE_OUTER_BOUND('',#9865,.T.);
#6294=FACE_OUTER_BOUND('',#9866,.T.);
#6295=FACE_OUTER_BOUND('',#9867,.T.);
#6296=FACE_OUTER_BOUND('',#9868,.T.);
#6297=FACE_OUTER_BOUND('',#9869,.T.);
#6298=FACE_OUTER_BOUND('',#9870,.T.);
#6299=FACE_OUTER_BOUND('',#9871,.T.);
#6300=FACE_OUTER_BOUND('',#9872,.T.);
#6301=FACE_OUTER_BOUND('',#9873,.T.);
#6302=FACE_OUTER_BOUND('',#9874,.T.);
#6303=FACE_OUTER_BOUND('',#9875,.T.);
#6304=FACE_OUTER_BOUND('',#9876,.T.);
#6305=FACE_OUTER_BOUND('',#9877,.T.);
#6306=FACE_OUTER_BOUND('',#9878,.T.);
#6307=FACE_OUTER_BOUND('',#9879,.T.);
#6308=FACE_OUTER_BOUND('',#9880,.T.);
#6309=FACE_OUTER_BOUND('',#9881,.T.);
#6310=FACE_OUTER_BOUND('',#9882,.T.);
#6311=FACE_OUTER_BOUND('',#9883,.T.);
#6312=FACE_OUTER_BOUND('',#9884,.T.);
#6313=FACE_OUTER_BOUND('',#9885,.T.);
#6314=FACE_OUTER_BOUND('',#9886,.T.);
#6315=FACE_OUTER_BOUND('',#9887,.T.);
#6316=FACE_OUTER_BOUND('',#9888,.T.);
#6317=FACE_OUTER_BOUND('',#9889,.T.);
#6318=FACE_OUTER_BOUND('',#9890,.T.);
#6319=FACE_OUTER_BOUND('',#9891,.T.);
#6320=FACE_OUTER_BOUND('',#9892,.T.);
#6321=FACE_OUTER_BOUND('',#9893,.T.);
#6322=FACE_OUTER_BOUND('',#9894,.T.);
#6323=FACE_OUTER_BOUND('',#9895,.T.);
#6324=FACE_OUTER_BOUND('',#9896,.T.);
#6325=FACE_OUTER_BOUND('',#9897,.T.);
#6326=FACE_OUTER_BOUND('',#9898,.T.);
#6327=FACE_OUTER_BOUND('',#9899,.T.);
#6328=FACE_OUTER_BOUND('',#9900,.T.);
#6329=FACE_OUTER_BOUND('',#9901,.T.);
#6330=FACE_OUTER_BOUND('',#9902,.T.);
#6331=FACE_OUTER_BOUND('',#9903,.T.);
#6332=FACE_OUTER_BOUND('',#9904,.T.);
#6333=FACE_OUTER_BOUND('',#9905,.T.);
#6334=FACE_OUTER_BOUND('',#9906,.T.);
#6335=FACE_OUTER_BOUND('',#9907,.T.);
#6336=FACE_OUTER_BOUND('',#9908,.T.);
#6337=FACE_OUTER_BOUND('',#9909,.T.);
#6338=FACE_OUTER_BOUND('',#9910,.T.);
#6339=FACE_OUTER_BOUND('',#9911,.T.);
#6340=FACE_OUTER_BOUND('',#9912,.T.);
#6341=FACE_OUTER_BOUND('',#9913,.T.);
#6342=FACE_OUTER_BOUND('',#9914,.T.);
#6343=FACE_OUTER_BOUND('',#9915,.T.);
#6344=FACE_OUTER_BOUND('',#9916,.T.);
#6345=FACE_OUTER_BOUND('',#9917,.T.);
#6346=FACE_OUTER_BOUND('',#9918,.T.);
#6347=FACE_OUTER_BOUND('',#9919,.T.);
#6348=FACE_OUTER_BOUND('',#9920,.T.);
#6349=FACE_OUTER_BOUND('',#9921,.T.);
#6350=FACE_OUTER_BOUND('',#9922,.T.);
#6351=FACE_OUTER_BOUND('',#9923,.T.);
#6352=FACE_OUTER_BOUND('',#9924,.T.);
#6353=FACE_OUTER_BOUND('',#9925,.T.);
#6354=FACE_OUTER_BOUND('',#9926,.T.);
#6355=FACE_OUTER_BOUND('',#9927,.T.);
#6356=FACE_OUTER_BOUND('',#9928,.T.);
#6357=FACE_OUTER_BOUND('',#9929,.T.);
#6358=FACE_OUTER_BOUND('',#9930,.T.);
#6359=FACE_OUTER_BOUND('',#9931,.T.);
#6360=FACE_OUTER_BOUND('',#9932,.T.);
#6361=FACE_OUTER_BOUND('',#9933,.T.);
#6362=FACE_OUTER_BOUND('',#9934,.T.);
#6363=FACE_OUTER_BOUND('',#9935,.T.);
#6364=FACE_OUTER_BOUND('',#9936,.T.);
#6365=FACE_OUTER_BOUND('',#9937,.T.);
#6366=FACE_OUTER_BOUND('',#9938,.T.);
#6367=FACE_OUTER_BOUND('',#9939,.T.);
#6368=FACE_OUTER_BOUND('',#9940,.T.);
#6369=FACE_OUTER_BOUND('',#9941,.T.);
#6370=FACE_OUTER_BOUND('',#9942,.T.);
#6371=FACE_OUTER_BOUND('',#9943,.T.);
#6372=FACE_OUTER_BOUND('',#9944,.T.);
#6373=FACE_OUTER_BOUND('',#9945,.T.);
#6374=FACE_OUTER_BOUND('',#9946,.T.);
#6375=FACE_OUTER_BOUND('',#9947,.T.);
#6376=FACE_OUTER_BOUND('',#9948,.T.);
#6377=FACE_OUTER_BOUND('',#9949,.T.);
#6378=FACE_OUTER_BOUND('',#9950,.T.);
#6379=FACE_OUTER_BOUND('',#9951,.T.);
#6380=FACE_OUTER_BOUND('',#9952,.T.);
#6381=FACE_OUTER_BOUND('',#9953,.T.);
#6382=FACE_OUTER_BOUND('',#9954,.T.);
#6383=FACE_OUTER_BOUND('',#9955,.T.);
#6384=FACE_OUTER_BOUND('',#9956,.T.);
#6385=FACE_OUTER_BOUND('',#9957,.T.);
#6386=FACE_OUTER_BOUND('',#9958,.T.);
#6387=FACE_OUTER_BOUND('',#9959,.T.);
#6388=FACE_OUTER_BOUND('',#9960,.T.);
#6389=FACE_OUTER_BOUND('',#9961,.T.);
#6390=FACE_OUTER_BOUND('',#9962,.T.);
#6391=FACE_OUTER_BOUND('',#9963,.T.);
#6392=FACE_OUTER_BOUND('',#9964,.T.);
#6393=FACE_OUTER_BOUND('',#9965,.T.);
#6394=FACE_OUTER_BOUND('',#9966,.T.);
#6395=FACE_OUTER_BOUND('',#9967,.T.);
#6396=FACE_OUTER_BOUND('',#9968,.T.);
#6397=FACE_OUTER_BOUND('',#9969,.T.);
#6398=FACE_OUTER_BOUND('',#9970,.T.);
#6399=FACE_OUTER_BOUND('',#9971,.T.);
#6400=FACE_OUTER_BOUND('',#9972,.T.);
#6401=FACE_OUTER_BOUND('',#9973,.T.);
#6402=FACE_OUTER_BOUND('',#9974,.T.);
#6403=FACE_OUTER_BOUND('',#9975,.T.);
#6404=FACE_OUTER_BOUND('',#9976,.T.);
#6405=FACE_OUTER_BOUND('',#9977,.T.);
#6406=FACE_OUTER_BOUND('',#9978,.T.);
#6407=FACE_OUTER_BOUND('',#9979,.T.);
#6408=FACE_OUTER_BOUND('',#9980,.T.);
#6409=FACE_OUTER_BOUND('',#9981,.T.);
#6410=FACE_OUTER_BOUND('',#9982,.T.);
#6411=FACE_OUTER_BOUND('',#9983,.T.);
#6412=FACE_OUTER_BOUND('',#9984,.T.);
#6413=FACE_OUTER_BOUND('',#9985,.T.);
#6414=FACE_OUTER_BOUND('',#9986,.T.);
#6415=FACE_OUTER_BOUND('',#9987,.T.);
#6416=FACE_OUTER_BOUND('',#9988,.T.);
#6417=FACE_OUTER_BOUND('',#9989,.T.);
#6418=FACE_OUTER_BOUND('',#9990,.T.);
#6419=FACE_OUTER_BOUND('',#9991,.T.);
#6420=FACE_OUTER_BOUND('',#9992,.T.);
#6421=FACE_OUTER_BOUND('',#9993,.T.);
#6422=FACE_OUTER_BOUND('',#9994,.T.);
#6423=FACE_OUTER_BOUND('',#9995,.T.);
#6424=FACE_OUTER_BOUND('',#9996,.T.);
#6425=FACE_OUTER_BOUND('',#9997,.T.);
#6426=FACE_OUTER_BOUND('',#9998,.T.);
#6427=FACE_OUTER_BOUND('',#9999,.T.);
#6428=FACE_OUTER_BOUND('',#10000,.T.);
#6429=FACE_OUTER_BOUND('',#10001,.T.);
#6430=FACE_OUTER_BOUND('',#10002,.T.);
#6431=FACE_OUTER_BOUND('',#10003,.T.);
#6432=FACE_OUTER_BOUND('',#10004,.T.);
#6433=FACE_OUTER_BOUND('',#10005,.T.);
#6434=FACE_OUTER_BOUND('',#10006,.T.);
#6435=FACE_OUTER_BOUND('',#10007,.T.);
#6436=FACE_OUTER_BOUND('',#10008,.T.);
#6437=FACE_OUTER_BOUND('',#10009,.T.);
#6438=FACE_OUTER_BOUND('',#10010,.T.);
#6439=FACE_OUTER_BOUND('',#10011,.T.);
#6440=FACE_OUTER_BOUND('',#10012,.T.);
#6441=FACE_OUTER_BOUND('',#10013,.T.);
#6442=FACE_OUTER_BOUND('',#10014,.T.);
#6443=FACE_OUTER_BOUND('',#10015,.T.);
#6444=FACE_OUTER_BOUND('',#10016,.T.);
#6445=FACE_OUTER_BOUND('',#10017,.T.);
#6446=FACE_OUTER_BOUND('',#10018,.T.);
#6447=FACE_OUTER_BOUND('',#10019,.T.);
#6448=FACE_OUTER_BOUND('',#10020,.T.);
#6449=FACE_OUTER_BOUND('',#10021,.T.);
#6450=FACE_OUTER_BOUND('',#10022,.T.);
#6451=FACE_OUTER_BOUND('',#10023,.T.);
#6452=FACE_OUTER_BOUND('',#10024,.T.);
#6453=FACE_OUTER_BOUND('',#10025,.T.);
#6454=FACE_OUTER_BOUND('',#10026,.T.);
#6455=FACE_OUTER_BOUND('',#10027,.T.);
#6456=FACE_OUTER_BOUND('',#10028,.T.);
#6457=FACE_OUTER_BOUND('',#10029,.T.);
#6458=FACE_OUTER_BOUND('',#10030,.T.);
#6459=FACE_OUTER_BOUND('',#10031,.T.);
#6460=FACE_OUTER_BOUND('',#10032,.T.);
#6461=FACE_OUTER_BOUND('',#10033,.T.);
#6462=FACE_OUTER_BOUND('',#10034,.T.);
#6463=FACE_OUTER_BOUND('',#10035,.T.);
#6464=FACE_OUTER_BOUND('',#10036,.T.);
#6465=FACE_OUTER_BOUND('',#10037,.T.);
#6466=FACE_OUTER_BOUND('',#10038,.T.);
#6467=FACE_OUTER_BOUND('',#10039,.T.);
#6468=FACE_OUTER_BOUND('',#10040,.T.);
#6469=FACE_OUTER_BOUND('',#10041,.T.);
#6470=FACE_OUTER_BOUND('',#10042,.T.);
#6471=FACE_OUTER_BOUND('',#10043,.T.);
#6472=FACE_OUTER_BOUND('',#10044,.T.);
#6473=FACE_OUTER_BOUND('',#10045,.T.);
#6474=FACE_OUTER_BOUND('',#10046,.T.);
#6475=FACE_OUTER_BOUND('',#10047,.T.);
#6476=FACE_OUTER_BOUND('',#10048,.T.);
#6477=FACE_OUTER_BOUND('',#10049,.T.);
#6478=FACE_OUTER_BOUND('',#10050,.T.);
#6479=FACE_OUTER_BOUND('',#10051,.T.);
#6480=FACE_OUTER_BOUND('',#10052,.T.);
#6481=FACE_OUTER_BOUND('',#10053,.T.);
#6482=FACE_OUTER_BOUND('',#10054,.T.);
#6483=FACE_OUTER_BOUND('',#10055,.T.);
#6484=FACE_OUTER_BOUND('',#10056,.T.);
#6485=FACE_OUTER_BOUND('',#10057,.T.);
#6486=FACE_OUTER_BOUND('',#10058,.T.);
#6487=FACE_OUTER_BOUND('',#10059,.T.);
#6488=FACE_OUTER_BOUND('',#10060,.T.);
#6489=FACE_OUTER_BOUND('',#10061,.T.);
#6490=FACE_OUTER_BOUND('',#10062,.T.);
#6491=FACE_OUTER_BOUND('',#10063,.T.);
#6492=FACE_OUTER_BOUND('',#10064,.T.);
#6493=FACE_OUTER_BOUND('',#10065,.T.);
#6494=FACE_OUTER_BOUND('',#10066,.T.);
#6495=FACE_OUTER_BOUND('',#10067,.T.);
#6496=FACE_OUTER_BOUND('',#10068,.T.);
#6497=FACE_OUTER_BOUND('',#10069,.T.);
#6498=FACE_OUTER_BOUND('',#10070,.T.);
#6499=FACE_OUTER_BOUND('',#10071,.T.);
#6500=FACE_OUTER_BOUND('',#10072,.T.);
#6501=FACE_OUTER_BOUND('',#10073,.T.);
#6502=FACE_OUTER_BOUND('',#10074,.T.);
#6503=FACE_OUTER_BOUND('',#10075,.T.);
#6504=FACE_OUTER_BOUND('',#10076,.T.);
#6505=FACE_OUTER_BOUND('',#10077,.T.);
#6506=FACE_OUTER_BOUND('',#10078,.T.);
#6507=FACE_OUTER_BOUND('',#10079,.T.);
#6508=FACE_OUTER_BOUND('',#10080,.T.);
#6509=FACE_OUTER_BOUND('',#10081,.T.);
#6510=FACE_OUTER_BOUND('',#10082,.T.);
#6511=FACE_OUTER_BOUND('',#10083,.T.);
#6512=FACE_OUTER_BOUND('',#10084,.T.);
#6513=FACE_OUTER_BOUND('',#10085,.T.);
#6514=FACE_OUTER_BOUND('',#10086,.T.);
#6515=FACE_OUTER_BOUND('',#10087,.T.);
#6516=FACE_OUTER_BOUND('',#10088,.T.);
#6517=FACE_OUTER_BOUND('',#10089,.T.);
#6518=FACE_OUTER_BOUND('',#10090,.T.);
#6519=FACE_OUTER_BOUND('',#10091,.T.);
#6520=FACE_OUTER_BOUND('',#10092,.T.);
#6521=FACE_OUTER_BOUND('',#10093,.T.);
#6522=FACE_OUTER_BOUND('',#10094,.T.);
#6523=FACE_OUTER_BOUND('',#10095,.T.);
#6524=FACE_OUTER_BOUND('',#10096,.T.);
#6525=FACE_OUTER_BOUND('',#10097,.T.);
#6526=FACE_OUTER_BOUND('',#10098,.T.);
#6527=FACE_OUTER_BOUND('',#10099,.T.);
#6528=FACE_OUTER_BOUND('',#10100,.T.);
#6529=FACE_OUTER_BOUND('',#10101,.T.);
#6530=FACE_OUTER_BOUND('',#10102,.T.);
#6531=FACE_OUTER_BOUND('',#10103,.T.);
#6532=FACE_OUTER_BOUND('',#10104,.T.);
#6533=FACE_OUTER_BOUND('',#10105,.T.);
#6534=FACE_OUTER_BOUND('',#10106,.T.);
#6535=FACE_OUTER_BOUND('',#10107,.T.);
#6536=FACE_OUTER_BOUND('',#10108,.T.);
#6537=FACE_OUTER_BOUND('',#10109,.T.);
#6538=FACE_OUTER_BOUND('',#10110,.T.);
#6539=FACE_OUTER_BOUND('',#10111,.T.);
#6540=FACE_OUTER_BOUND('',#10112,.T.);
#6541=FACE_OUTER_BOUND('',#10113,.T.);
#6542=FACE_OUTER_BOUND('',#10114,.T.);
#6543=FACE_OUTER_BOUND('',#10115,.T.);
#6544=FACE_OUTER_BOUND('',#10116,.T.);
#6545=FACE_OUTER_BOUND('',#10117,.T.);
#6546=FACE_OUTER_BOUND('',#10118,.T.);
#6547=FACE_OUTER_BOUND('',#10119,.T.);
#6548=FACE_OUTER_BOUND('',#10120,.T.);
#6549=FACE_OUTER_BOUND('',#10121,.T.);
#6550=FACE_OUTER_BOUND('',#10122,.T.);
#6551=FACE_OUTER_BOUND('',#10123,.T.);
#6552=FACE_OUTER_BOUND('',#10124,.T.);
#6553=FACE_OUTER_BOUND('',#10125,.T.);
#6554=FACE_OUTER_BOUND('',#10126,.T.);
#6555=FACE_OUTER_BOUND('',#10127,.T.);
#6556=FACE_OUTER_BOUND('',#10128,.T.);
#6557=FACE_OUTER_BOUND('',#10129,.T.);
#6558=FACE_OUTER_BOUND('',#10130,.T.);
#6559=FACE_OUTER_BOUND('',#10131,.T.);
#6560=FACE_OUTER_BOUND('',#10132,.T.);
#6561=FACE_OUTER_BOUND('',#10133,.T.);
#6562=FACE_OUTER_BOUND('',#10134,.T.);
#6563=FACE_OUTER_BOUND('',#10135,.T.);
#6564=FACE_OUTER_BOUND('',#10136,.T.);
#6565=FACE_OUTER_BOUND('',#10137,.T.);
#6566=FACE_OUTER_BOUND('',#10138,.T.);
#6567=FACE_OUTER_BOUND('',#10139,.T.);
#6568=FACE_OUTER_BOUND('',#10140,.T.);
#6569=FACE_OUTER_BOUND('',#10141,.T.);
#6570=FACE_OUTER_BOUND('',#10142,.T.);
#6571=FACE_OUTER_BOUND('',#10143,.T.);
#6572=FACE_OUTER_BOUND('',#10144,.T.);
#6573=FACE_OUTER_BOUND('',#10145,.T.);
#6574=FACE_OUTER_BOUND('',#10146,.T.);
#6575=FACE_OUTER_BOUND('',#10147,.T.);
#6576=FACE_OUTER_BOUND('',#10148,.T.);
#6577=FACE_OUTER_BOUND('',#10149,.T.);
#6578=FACE_OUTER_BOUND('',#10150,.T.);
#6579=FACE_OUTER_BOUND('',#10151,.T.);
#6580=FACE_OUTER_BOUND('',#10152,.T.);
#6581=FACE_OUTER_BOUND('',#10153,.T.);
#6582=FACE_OUTER_BOUND('',#10154,.T.);
#6583=FACE_OUTER_BOUND('',#10155,.T.);
#6584=FACE_OUTER_BOUND('',#10156,.T.);
#6585=FACE_OUTER_BOUND('',#10157,.T.);
#6586=FACE_OUTER_BOUND('',#10158,.T.);
#6587=FACE_OUTER_BOUND('',#10159,.T.);
#6588=FACE_OUTER_BOUND('',#10160,.T.);
#6589=FACE_OUTER_BOUND('',#10161,.T.);
#6590=FACE_OUTER_BOUND('',#10162,.T.);
#6591=FACE_OUTER_BOUND('',#10163,.T.);
#6592=FACE_OUTER_BOUND('',#10164,.T.);
#6593=FACE_OUTER_BOUND('',#10165,.T.);
#6594=FACE_OUTER_BOUND('',#10166,.T.);
#6595=FACE_OUTER_BOUND('',#10167,.T.);
#6596=FACE_OUTER_BOUND('',#10168,.T.);
#6597=FACE_OUTER_BOUND('',#10169,.T.);
#6598=FACE_OUTER_BOUND('',#10170,.T.);
#6599=FACE_OUTER_BOUND('',#10171,.T.);
#6600=FACE_OUTER_BOUND('',#10172,.T.);
#6601=FACE_OUTER_BOUND('',#10173,.T.);
#6602=FACE_OUTER_BOUND('',#10174,.T.);
#6603=FACE_OUTER_BOUND('',#10175,.T.);
#6604=FACE_OUTER_BOUND('',#10176,.T.);
#6605=FACE_OUTER_BOUND('',#10177,.T.);
#6606=FACE_OUTER_BOUND('',#10178,.T.);
#6607=FACE_OUTER_BOUND('',#10179,.T.);
#6608=FACE_OUTER_BOUND('',#10180,.T.);
#6609=FACE_OUTER_BOUND('',#10181,.T.);
#6610=FACE_OUTER_BOUND('',#10182,.T.);
#6611=FACE_OUTER_BOUND('',#10183,.T.);
#6612=FACE_OUTER_BOUND('',#10184,.T.);
#6613=FACE_OUTER_BOUND('',#10185,.T.);
#6614=FACE_OUTER_BOUND('',#10186,.T.);
#6615=FACE_OUTER_BOUND('',#10187,.T.);
#6616=FACE_OUTER_BOUND('',#10188,.T.);
#6617=FACE_OUTER_BOUND('',#10189,.T.);
#6618=FACE_OUTER_BOUND('',#10190,.T.);
#6619=FACE_OUTER_BOUND('',#10191,.T.);
#6620=FACE_OUTER_BOUND('',#10192,.T.);
#6621=FACE_OUTER_BOUND('',#10193,.T.);
#6622=FACE_OUTER_BOUND('',#10194,.T.);
#6623=FACE_OUTER_BOUND('',#10195,.T.);
#6624=FACE_OUTER_BOUND('',#10196,.T.);
#6625=FACE_OUTER_BOUND('',#10197,.T.);
#6626=FACE_OUTER_BOUND('',#10198,.T.);
#6627=FACE_OUTER_BOUND('',#10199,.T.);
#6628=FACE_OUTER_BOUND('',#10200,.T.);
#6629=FACE_OUTER_BOUND('',#10201,.T.);
#6630=FACE_OUTER_BOUND('',#10202,.T.);
#6631=FACE_OUTER_BOUND('',#10203,.T.);
#6632=FACE_OUTER_BOUND('',#10204,.T.);
#6633=FACE_OUTER_BOUND('',#10205,.T.);
#6634=FACE_OUTER_BOUND('',#10206,.T.);
#6635=FACE_OUTER_BOUND('',#10207,.T.);
#6636=FACE_OUTER_BOUND('',#10208,.T.);
#6637=FACE_OUTER_BOUND('',#10209,.T.);
#6638=FACE_OUTER_BOUND('',#10210,.T.);
#6639=FACE_OUTER_BOUND('',#10211,.T.);
#6640=FACE_OUTER_BOUND('',#10212,.T.);
#6641=FACE_OUTER_BOUND('',#10213,.T.);
#6642=FACE_OUTER_BOUND('',#10214,.T.);
#6643=FACE_OUTER_BOUND('',#10215,.T.);
#6644=FACE_OUTER_BOUND('',#10216,.T.);
#6645=FACE_OUTER_BOUND('',#10217,.T.);
#6646=FACE_OUTER_BOUND('',#10218,.T.);
#6647=FACE_OUTER_BOUND('',#10219,.T.);
#6648=FACE_OUTER_BOUND('',#10220,.T.);
#6649=FACE_OUTER_BOUND('',#10221,.T.);
#6650=FACE_OUTER_BOUND('',#10222,.T.);
#6651=FACE_OUTER_BOUND('',#10223,.T.);
#6652=FACE_OUTER_BOUND('',#10224,.T.);
#6653=FACE_OUTER_BOUND('',#10225,.T.);
#6654=FACE_OUTER_BOUND('',#10226,.T.);
#6655=FACE_OUTER_BOUND('',#10227,.T.);
#6656=FACE_OUTER_BOUND('',#10228,.T.);
#6657=FACE_OUTER_BOUND('',#10229,.T.);
#6658=FACE_OUTER_BOUND('',#10230,.T.);
#6659=FACE_OUTER_BOUND('',#10231,.T.);
#6660=FACE_OUTER_BOUND('',#10232,.T.);
#6661=FACE_OUTER_BOUND('',#10233,.T.);
#6662=FACE_OUTER_BOUND('',#10234,.T.);
#6663=FACE_OUTER_BOUND('',#10235,.T.);
#6664=FACE_OUTER_BOUND('',#10236,.T.);
#6665=FACE_OUTER_BOUND('',#10237,.T.);
#6666=FACE_OUTER_BOUND('',#10238,.T.);
#6667=FACE_OUTER_BOUND('',#10239,.T.);
#6668=FACE_OUTER_BOUND('',#10240,.T.);
#6669=FACE_OUTER_BOUND('',#10241,.T.);
#6670=FACE_OUTER_BOUND('',#10242,.T.);
#6671=FACE_OUTER_BOUND('',#10243,.T.);
#6672=FACE_OUTER_BOUND('',#10244,.T.);
#6673=FACE_OUTER_BOUND('',#10245,.T.);
#6674=FACE_OUTER_BOUND('',#10246,.T.);
#6675=FACE_OUTER_BOUND('',#10247,.T.);
#6676=FACE_OUTER_BOUND('',#10248,.T.);
#6677=FACE_OUTER_BOUND('',#10249,.T.);
#6678=FACE_OUTER_BOUND('',#10250,.T.);
#6679=FACE_OUTER_BOUND('',#10251,.T.);
#6680=FACE_OUTER_BOUND('',#10252,.T.);
#6681=FACE_OUTER_BOUND('',#10253,.T.);
#6682=FACE_OUTER_BOUND('',#10254,.T.);
#6683=FACE_OUTER_BOUND('',#10255,.T.);
#6684=FACE_OUTER_BOUND('',#10256,.T.);
#6685=FACE_OUTER_BOUND('',#10257,.T.);
#6686=FACE_OUTER_BOUND('',#10258,.T.);
#6687=FACE_OUTER_BOUND('',#10259,.T.);
#6688=FACE_OUTER_BOUND('',#10260,.T.);
#6689=FACE_OUTER_BOUND('',#10261,.T.);
#6690=FACE_OUTER_BOUND('',#10262,.T.);
#6691=FACE_OUTER_BOUND('',#10263,.T.);
#6692=FACE_OUTER_BOUND('',#10264,.T.);
#6693=FACE_OUTER_BOUND('',#10265,.T.);
#6694=FACE_OUTER_BOUND('',#10266,.T.);
#6695=FACE_OUTER_BOUND('',#10267,.T.);
#6696=FACE_OUTER_BOUND('',#10268,.T.);
#6697=FACE_OUTER_BOUND('',#10269,.T.);
#6698=FACE_OUTER_BOUND('',#10270,.T.);
#6699=FACE_OUTER_BOUND('',#10271,.T.);
#6700=FACE_OUTER_BOUND('',#10272,.T.);
#6701=FACE_OUTER_BOUND('',#10273,.T.);
#6702=FACE_OUTER_BOUND('',#10274,.T.);
#6703=FACE_OUTER_BOUND('',#10275,.T.);
#6704=FACE_OUTER_BOUND('',#10276,.T.);
#6705=FACE_OUTER_BOUND('',#10277,.T.);
#6706=FACE_OUTER_BOUND('',#10278,.T.);
#6707=FACE_OUTER_BOUND('',#10279,.T.);
#6708=FACE_OUTER_BOUND('',#10280,.T.);
#6709=FACE_OUTER_BOUND('',#10281,.T.);
#6710=FACE_OUTER_BOUND('',#10282,.T.);
#6711=FACE_OUTER_BOUND('',#10283,.T.);
#6712=FACE_OUTER_BOUND('',#10284,.T.);
#6713=FACE_OUTER_BOUND('',#10285,.T.);
#6714=FACE_OUTER_BOUND('',#10286,.T.);
#6715=FACE_OUTER_BOUND('',#10287,.T.);
#6716=FACE_OUTER_BOUND('',#10288,.T.);
#6717=FACE_OUTER_BOUND('',#10289,.T.);
#6718=FACE_OUTER_BOUND('',#10290,.T.);
#6719=FACE_OUTER_BOUND('',#10291,.T.);
#6720=FACE_OUTER_BOUND('',#10292,.T.);
#6721=FACE_OUTER_BOUND('',#10293,.T.);
#6722=FACE_OUTER_BOUND('',#10294,.T.);
#6723=FACE_OUTER_BOUND('',#10295,.T.);
#6724=FACE_OUTER_BOUND('',#10296,.T.);
#6725=FACE_OUTER_BOUND('',#10297,.T.);
#6726=FACE_OUTER_BOUND('',#10298,.T.);
#6727=FACE_OUTER_BOUND('',#10299,.T.);
#6728=FACE_OUTER_BOUND('',#10300,.T.);
#6729=FACE_OUTER_BOUND('',#10301,.T.);
#6730=FACE_OUTER_BOUND('',#10302,.T.);
#6731=FACE_OUTER_BOUND('',#10303,.T.);
#6732=FACE_OUTER_BOUND('',#10304,.T.);
#6733=FACE_OUTER_BOUND('',#10305,.T.);
#6734=FACE_OUTER_BOUND('',#10306,.T.);
#6735=FACE_OUTER_BOUND('',#10307,.T.);
#6736=FACE_OUTER_BOUND('',#10308,.T.);
#6737=FACE_OUTER_BOUND('',#10309,.T.);
#6738=FACE_OUTER_BOUND('',#10310,.T.);
#6739=FACE_OUTER_BOUND('',#10311,.T.);
#6740=FACE_OUTER_BOUND('',#10312,.T.);
#6741=FACE_OUTER_BOUND('',#10313,.T.);
#6742=FACE_OUTER_BOUND('',#10314,.T.);
#6743=FACE_OUTER_BOUND('',#10315,.T.);
#6744=FACE_OUTER_BOUND('',#10316,.T.);
#6745=FACE_OUTER_BOUND('',#10317,.T.);
#6746=FACE_OUTER_BOUND('',#10318,.T.);
#6747=FACE_OUTER_BOUND('',#10319,.T.);
#6748=FACE_OUTER_BOUND('',#10320,.T.);
#6749=FACE_OUTER_BOUND('',#10321,.T.);
#6750=FACE_OUTER_BOUND('',#10322,.T.);
#6751=FACE_OUTER_BOUND('',#10323,.T.);
#6752=FACE_OUTER_BOUND('',#10324,.T.);
#6753=FACE_OUTER_BOUND('',#10325,.T.);
#6754=FACE_OUTER_BOUND('',#10326,.T.);
#6755=FACE_OUTER_BOUND('',#10327,.T.);
#6756=FACE_OUTER_BOUND('',#10328,.T.);
#6757=FACE_OUTER_BOUND('',#10329,.T.);
#6758=FACE_OUTER_BOUND('',#10331,.T.);
#6759=FACE_OUTER_BOUND('',#10332,.T.);
#6760=FACE_OUTER_BOUND('',#10333,.T.);
#6761=FACE_OUTER_BOUND('',#10334,.T.);
#6762=FACE_OUTER_BOUND('',#10335,.T.);
#6763=FACE_OUTER_BOUND('',#10336,.T.);
#6764=FACE_OUTER_BOUND('',#10337,.T.);
#6765=FACE_OUTER_BOUND('',#10338,.T.);
#6766=FACE_OUTER_BOUND('',#10339,.T.);
#6767=FACE_OUTER_BOUND('',#10340,.T.);
#6768=FACE_OUTER_BOUND('',#10342,.T.);
#6769=FACE_OUTER_BOUND('',#10343,.T.);
#6770=FACE_OUTER_BOUND('',#10344,.T.);
#6771=FACE_OUTER_BOUND('',#10345,.T.);
#6772=FACE_OUTER_BOUND('',#10346,.T.);
#6773=FACE_OUTER_BOUND('',#10347,.T.);
#6774=FACE_OUTER_BOUND('',#10348,.T.);
#6775=FACE_OUTER_BOUND('',#10349,.T.);
#6776=FACE_OUTER_BOUND('',#10350,.T.);
#6777=FACE_OUTER_BOUND('',#10351,.T.);
#6778=FACE_OUTER_BOUND('',#10352,.T.);
#6779=FACE_OUTER_BOUND('',#10353,.T.);
#6780=FACE_OUTER_BOUND('',#10354,.T.);
#6781=FACE_OUTER_BOUND('',#10355,.T.);
#6782=FACE_OUTER_BOUND('',#10356,.T.);
#6783=FACE_OUTER_BOUND('',#10357,.T.);
#6784=FACE_OUTER_BOUND('',#10358,.T.);
#6785=FACE_OUTER_BOUND('',#10359,.T.);
#6786=FACE_OUTER_BOUND('',#10360,.T.);
#6787=FACE_OUTER_BOUND('',#10361,.T.);
#6788=FACE_OUTER_BOUND('',#10362,.T.);
#6789=FACE_OUTER_BOUND('',#10363,.T.);
#6790=FACE_OUTER_BOUND('',#10364,.T.);
#6791=FACE_OUTER_BOUND('',#10365,.T.);
#6792=FACE_OUTER_BOUND('',#10366,.T.);
#6793=FACE_OUTER_BOUND('',#10367,.T.);
#6794=FACE_OUTER_BOUND('',#10368,.T.);
#6795=FACE_OUTER_BOUND('',#10369,.T.);
#6796=FACE_OUTER_BOUND('',#10370,.T.);
#6797=FACE_OUTER_BOUND('',#10371,.T.);
#6798=FACE_OUTER_BOUND('',#10372,.T.);
#6799=FACE_OUTER_BOUND('',#10373,.T.);
#6800=FACE_OUTER_BOUND('',#10374,.T.);
#6801=FACE_OUTER_BOUND('',#10375,.T.);
#6802=FACE_OUTER_BOUND('',#10376,.T.);
#6803=FACE_OUTER_BOUND('',#10377,.T.);
#6804=FACE_OUTER_BOUND('',#10378,.T.);
#6805=FACE_OUTER_BOUND('',#10379,.T.);
#6806=FACE_OUTER_BOUND('',#10380,.T.);
#6807=FACE_OUTER_BOUND('',#10381,.T.);
#6808=FACE_OUTER_BOUND('',#10382,.T.);
#6809=FACE_OUTER_BOUND('',#10383,.T.);
#6810=FACE_OUTER_BOUND('',#10384,.T.);
#6811=FACE_OUTER_BOUND('',#10385,.T.);
#6812=FACE_OUTER_BOUND('',#10386,.T.);
#6813=FACE_OUTER_BOUND('',#10387,.T.);
#6814=FACE_OUTER_BOUND('',#10388,.T.);
#6815=FACE_OUTER_BOUND('',#10389,.T.);
#6816=FACE_OUTER_BOUND('',#10390,.T.);
#6817=FACE_OUTER_BOUND('',#10391,.T.);
#6818=FACE_OUTER_BOUND('',#10392,.T.);
#6819=FACE_OUTER_BOUND('',#10393,.T.);
#6820=FACE_OUTER_BOUND('',#10394,.T.);
#6821=FACE_OUTER_BOUND('',#10395,.T.);
#6822=FACE_OUTER_BOUND('',#10396,.T.);
#6823=FACE_OUTER_BOUND('',#10397,.T.);
#6824=FACE_OUTER_BOUND('',#10398,.T.);
#6825=FACE_OUTER_BOUND('',#10399,.T.);
#6826=FACE_OUTER_BOUND('',#10400,.T.);
#6827=FACE_OUTER_BOUND('',#10401,.T.);
#6828=FACE_OUTER_BOUND('',#10402,.T.);
#6829=FACE_OUTER_BOUND('',#10403,.T.);
#6830=FACE_OUTER_BOUND('',#10404,.T.);
#6831=FACE_OUTER_BOUND('',#10405,.T.);
#6832=FACE_OUTER_BOUND('',#10406,.T.);
#6833=FACE_OUTER_BOUND('',#10407,.T.);
#6834=FACE_OUTER_BOUND('',#10408,.T.);
#6835=FACE_OUTER_BOUND('',#10409,.T.);
#6836=FACE_OUTER_BOUND('',#10410,.T.);
#6837=FACE_OUTER_BOUND('',#10411,.T.);
#6838=FACE_OUTER_BOUND('',#10412,.T.);
#6839=FACE_OUTER_BOUND('',#10413,.T.);
#6840=FACE_OUTER_BOUND('',#10414,.T.);
#6841=FACE_OUTER_BOUND('',#10415,.T.);
#6842=FACE_OUTER_BOUND('',#10416,.T.);
#6843=FACE_OUTER_BOUND('',#10417,.T.);
#6844=FACE_OUTER_BOUND('',#10418,.T.);
#6845=FACE_OUTER_BOUND('',#10419,.T.);
#6846=FACE_OUTER_BOUND('',#10420,.T.);
#6847=FACE_OUTER_BOUND('',#10421,.T.);
#6848=FACE_OUTER_BOUND('',#10422,.T.);
#6849=FACE_OUTER_BOUND('',#10423,.T.);
#6850=FACE_OUTER_BOUND('',#10426,.T.);
#6851=FACE_OUTER_BOUND('',#10427,.T.);
#6852=FACE_OUTER_BOUND('',#10428,.T.);
#6853=FACE_OUTER_BOUND('',#10429,.T.);
#6854=FACE_OUTER_BOUND('',#10430,.T.);
#6855=FACE_OUTER_BOUND('',#10431,.T.);
#6856=FACE_OUTER_BOUND('',#10432,.T.);
#6857=FACE_OUTER_BOUND('',#10433,.T.);
#6858=FACE_OUTER_BOUND('',#10434,.T.);
#6859=FACE_OUTER_BOUND('',#10435,.T.);
#6860=FACE_OUTER_BOUND('',#10436,.T.);
#6861=FACE_OUTER_BOUND('',#10437,.T.);
#6862=FACE_OUTER_BOUND('',#10438,.T.);
#6863=FACE_OUTER_BOUND('',#10439,.T.);
#6864=FACE_OUTER_BOUND('',#10440,.T.);
#6865=FACE_OUTER_BOUND('',#10441,.T.);
#6866=FACE_OUTER_BOUND('',#10442,.T.);
#6867=FACE_OUTER_BOUND('',#10443,.T.);
#6868=FACE_OUTER_BOUND('',#10444,.T.);
#6869=FACE_OUTER_BOUND('',#10445,.T.);
#6870=FACE_OUTER_BOUND('',#10446,.T.);
#6871=FACE_OUTER_BOUND('',#10447,.T.);
#6872=FACE_OUTER_BOUND('',#10448,.T.);
#6873=FACE_OUTER_BOUND('',#10449,.T.);
#6874=FACE_OUTER_BOUND('',#10450,.T.);
#6875=FACE_OUTER_BOUND('',#10451,.T.);
#6876=FACE_OUTER_BOUND('',#10452,.T.);
#6877=FACE_OUTER_BOUND('',#10453,.T.);
#6878=FACE_OUTER_BOUND('',#10455,.T.);
#6879=FACE_OUTER_BOUND('',#10456,.T.);
#6880=FACE_OUTER_BOUND('',#10457,.T.);
#6881=FACE_OUTER_BOUND('',#10458,.T.);
#6882=FACE_OUTER_BOUND('',#10459,.T.);
#6883=FACE_OUTER_BOUND('',#10460,.T.);
#6884=FACE_OUTER_BOUND('',#10461,.T.);
#6885=FACE_OUTER_BOUND('',#10462,.T.);
#6886=FACE_OUTER_BOUND('',#10463,.T.);
#6887=FACE_OUTER_BOUND('',#10464,.T.);
#6888=FACE_OUTER_BOUND('',#10465,.T.);
#6889=FACE_OUTER_BOUND('',#10466,.T.);
#6890=FACE_OUTER_BOUND('',#10467,.T.);
#6891=FACE_OUTER_BOUND('',#10468,.T.);
#6892=FACE_OUTER_BOUND('',#10469,.T.);
#6893=FACE_OUTER_BOUND('',#10470,.T.);
#6894=FACE_OUTER_BOUND('',#10471,.T.);
#6895=FACE_OUTER_BOUND('',#10472,.T.);
#6896=FACE_OUTER_BOUND('',#10473,.T.);
#6897=FACE_OUTER_BOUND('',#10474,.T.);
#6898=FACE_OUTER_BOUND('',#10475,.T.);
#6899=FACE_OUTER_BOUND('',#10476,.T.);
#6900=FACE_OUTER_BOUND('',#10477,.T.);
#6901=FACE_OUTER_BOUND('',#10478,.T.);
#6902=FACE_OUTER_BOUND('',#10479,.T.);
#6903=FACE_OUTER_BOUND('',#10480,.T.);
#6904=FACE_OUTER_BOUND('',#10481,.T.);
#6905=FACE_OUTER_BOUND('',#10482,.T.);
#6906=FACE_OUTER_BOUND('',#10483,.T.);
#6907=FACE_OUTER_BOUND('',#10484,.T.);
#6908=FACE_OUTER_BOUND('',#10485,.T.);
#6909=FACE_OUTER_BOUND('',#10486,.T.);
#6910=FACE_OUTER_BOUND('',#10487,.T.);
#6911=FACE_OUTER_BOUND('',#10488,.T.);
#6912=FACE_OUTER_BOUND('',#10489,.T.);
#6913=FACE_OUTER_BOUND('',#10490,.T.);
#6914=FACE_OUTER_BOUND('',#10491,.T.);
#6915=FACE_OUTER_BOUND('',#10492,.T.);
#6916=FACE_OUTER_BOUND('',#10493,.T.);
#6917=FACE_OUTER_BOUND('',#10494,.T.);
#6918=FACE_OUTER_BOUND('',#10495,.T.);
#6919=FACE_OUTER_BOUND('',#10496,.T.);
#6920=FACE_OUTER_BOUND('',#10497,.T.);
#6921=FACE_OUTER_BOUND('',#10498,.T.);
#6922=FACE_OUTER_BOUND('',#10499,.T.);
#6923=FACE_OUTER_BOUND('',#10500,.T.);
#6924=FACE_OUTER_BOUND('',#10501,.T.);
#6925=FACE_OUTER_BOUND('',#10502,.T.);
#6926=FACE_OUTER_BOUND('',#10503,.T.);
#6927=FACE_OUTER_BOUND('',#10504,.T.);
#6928=FACE_OUTER_BOUND('',#10505,.T.);
#6929=FACE_OUTER_BOUND('',#10506,.T.);
#6930=FACE_OUTER_BOUND('',#10508,.T.);
#6931=FACE_OUTER_BOUND('',#10509,.T.);
#6932=FACE_OUTER_BOUND('',#10510,.T.);
#6933=FACE_OUTER_BOUND('',#10511,.T.);
#6934=FACE_OUTER_BOUND('',#10512,.T.);
#6935=FACE_OUTER_BOUND('',#10513,.T.);
#6936=FACE_OUTER_BOUND('',#10514,.T.);
#6937=FACE_OUTER_BOUND('',#10515,.T.);
#6938=FACE_OUTER_BOUND('',#10516,.T.);
#6939=FACE_OUTER_BOUND('',#10517,.T.);
#6940=FACE_OUTER_BOUND('',#10518,.T.);
#6941=FACE_OUTER_BOUND('',#10519,.T.);
#6942=FACE_OUTER_BOUND('',#10520,.T.);
#6943=FACE_OUTER_BOUND('',#10521,.T.);
#6944=FACE_OUTER_BOUND('',#10522,.T.);
#6945=FACE_OUTER_BOUND('',#10523,.T.);
#6946=FACE_OUTER_BOUND('',#10524,.T.);
#6947=FACE_OUTER_BOUND('',#10525,.T.);
#6948=FACE_OUTER_BOUND('',#10526,.T.);
#6949=FACE_OUTER_BOUND('',#10527,.T.);
#6950=FACE_OUTER_BOUND('',#10528,.T.);
#6951=FACE_OUTER_BOUND('',#10529,.T.);
#6952=FACE_OUTER_BOUND('',#10530,.T.);
#6953=FACE_OUTER_BOUND('',#10531,.T.);
#6954=FACE_OUTER_BOUND('',#10532,.T.);
#6955=FACE_OUTER_BOUND('',#10533,.T.);
#6956=FACE_OUTER_BOUND('',#10534,.T.);
#6957=FACE_OUTER_BOUND('',#10535,.T.);
#6958=FACE_OUTER_BOUND('',#10536,.T.);
#6959=FACE_OUTER_BOUND('',#10537,.T.);
#6960=FACE_OUTER_BOUND('',#10538,.T.);
#6961=FACE_OUTER_BOUND('',#10539,.T.);
#6962=FACE_OUTER_BOUND('',#10540,.T.);
#6963=FACE_OUTER_BOUND('',#10541,.T.);
#6964=FACE_OUTER_BOUND('',#10542,.T.);
#6965=FACE_OUTER_BOUND('',#10543,.T.);
#6966=FACE_OUTER_BOUND('',#10544,.T.);
#6967=FACE_OUTER_BOUND('',#10545,.T.);
#6968=FACE_OUTER_BOUND('',#10546,.T.);
#6969=FACE_OUTER_BOUND('',#10547,.T.);
#6970=FACE_OUTER_BOUND('',#10548,.T.);
#6971=FACE_OUTER_BOUND('',#10549,.T.);
#6972=FACE_OUTER_BOUND('',#10550,.T.);
#6973=FACE_OUTER_BOUND('',#10552,.T.);
#6974=FACE_OUTER_BOUND('',#10553,.T.);
#6975=FACE_OUTER_BOUND('',#10554,.T.);
#6976=FACE_OUTER_BOUND('',#10555,.T.);
#6977=FACE_OUTER_BOUND('',#10556,.T.);
#6978=FACE_OUTER_BOUND('',#10557,.T.);
#6979=FACE_OUTER_BOUND('',#10558,.T.);
#6980=FACE_OUTER_BOUND('',#10559,.T.);
#6981=FACE_OUTER_BOUND('',#10560,.T.);
#6982=FACE_OUTER_BOUND('',#10561,.T.);
#6983=FACE_OUTER_BOUND('',#10562,.T.);
#6984=FACE_OUTER_BOUND('',#10563,.T.);
#6985=FACE_OUTER_BOUND('',#10564,.T.);
#6986=FACE_OUTER_BOUND('',#10565,.T.);
#6987=FACE_OUTER_BOUND('',#10566,.T.);
#6988=FACE_OUTER_BOUND('',#10567,.T.);
#6989=FACE_OUTER_BOUND('',#10568,.T.);
#6990=FACE_OUTER_BOUND('',#10569,.T.);
#6991=FACE_OUTER_BOUND('',#10570,.T.);
#6992=FACE_OUTER_BOUND('',#10571,.T.);
#6993=FACE_OUTER_BOUND('',#10572,.T.);
#6994=FACE_OUTER_BOUND('',#10573,.T.);
#6995=FACE_OUTER_BOUND('',#10574,.T.);
#6996=FACE_OUTER_BOUND('',#10575,.T.);
#6997=FACE_OUTER_BOUND('',#10576,.T.);
#6998=FACE_OUTER_BOUND('',#10577,.T.);
#6999=FACE_OUTER_BOUND('',#10578,.T.);
#7000=FACE_OUTER_BOUND('',#10579,.T.);
#7001=FACE_OUTER_BOUND('',#10580,.T.);
#7002=FACE_OUTER_BOUND('',#10581,.T.);
#7003=FACE_OUTER_BOUND('',#10582,.T.);
#7004=FACE_OUTER_BOUND('',#10583,.T.);
#7005=FACE_OUTER_BOUND('',#10584,.T.);
#7006=FACE_OUTER_BOUND('',#10585,.T.);
#7007=FACE_OUTER_BOUND('',#10586,.T.);
#7008=FACE_OUTER_BOUND('',#10587,.T.);
#7009=FACE_OUTER_BOUND('',#10588,.T.);
#7010=FACE_OUTER_BOUND('',#10589,.T.);
#7011=FACE_OUTER_BOUND('',#10590,.T.);
#7012=FACE_OUTER_BOUND('',#10591,.T.);
#7013=FACE_OUTER_BOUND('',#10592,.T.);
#7014=FACE_OUTER_BOUND('',#10593,.T.);
#7015=FACE_OUTER_BOUND('',#10594,.T.);
#7016=FACE_OUTER_BOUND('',#10595,.T.);
#7017=FACE_OUTER_BOUND('',#10596,.T.);
#7018=FACE_OUTER_BOUND('',#10597,.T.);
#7019=FACE_OUTER_BOUND('',#10598,.T.);
#7020=FACE_OUTER_BOUND('',#10599,.T.);
#7021=FACE_OUTER_BOUND('',#10600,.T.);
#7022=FACE_OUTER_BOUND('',#10601,.T.);
#7023=FACE_OUTER_BOUND('',#10602,.T.);
#7024=FACE_OUTER_BOUND('',#10603,.T.);
#7025=FACE_OUTER_BOUND('',#10604,.T.);
#7026=FACE_OUTER_BOUND('',#10605,.T.);
#7027=FACE_OUTER_BOUND('',#10606,.T.);
#7028=FACE_OUTER_BOUND('',#10607,.T.);
#7029=FACE_OUTER_BOUND('',#10608,.T.);
#7030=FACE_OUTER_BOUND('',#10610,.T.);
#7031=FACE_OUTER_BOUND('',#10611,.T.);
#7032=FACE_OUTER_BOUND('',#10612,.T.);
#7033=FACE_OUTER_BOUND('',#10613,.T.);
#7034=FACE_OUTER_BOUND('',#10614,.T.);
#7035=FACE_OUTER_BOUND('',#10615,.T.);
#7036=FACE_OUTER_BOUND('',#10616,.T.);
#7037=FACE_OUTER_BOUND('',#10617,.T.);
#7038=FACE_OUTER_BOUND('',#10618,.T.);
#7039=FACE_OUTER_BOUND('',#10619,.T.);
#7040=FACE_OUTER_BOUND('',#10620,.T.);
#7041=FACE_OUTER_BOUND('',#10621,.T.);
#7042=FACE_OUTER_BOUND('',#10622,.T.);
#7043=FACE_OUTER_BOUND('',#10623,.T.);
#7044=FACE_OUTER_BOUND('',#10624,.T.);
#7045=FACE_OUTER_BOUND('',#10625,.T.);
#7046=FACE_OUTER_BOUND('',#10626,.T.);
#7047=FACE_OUTER_BOUND('',#10627,.T.);
#7048=FACE_OUTER_BOUND('',#10628,.T.);
#7049=FACE_OUTER_BOUND('',#10629,.T.);
#7050=FACE_OUTER_BOUND('',#10630,.T.);
#7051=FACE_OUTER_BOUND('',#10631,.T.);
#7052=FACE_OUTER_BOUND('',#10632,.T.);
#7053=FACE_OUTER_BOUND('',#10633,.T.);
#7054=FACE_OUTER_BOUND('',#10634,.T.);
#7055=FACE_OUTER_BOUND('',#10635,.T.);
#7056=FACE_OUTER_BOUND('',#10636,.T.);
#7057=FACE_OUTER_BOUND('',#10637,.T.);
#7058=FACE_OUTER_BOUND('',#10638,.T.);
#7059=FACE_OUTER_BOUND('',#10639,.T.);
#7060=FACE_OUTER_BOUND('',#10640,.T.);
#7061=FACE_OUTER_BOUND('',#10641,.T.);
#7062=FACE_OUTER_BOUND('',#10642,.T.);
#7063=FACE_OUTER_BOUND('',#10643,.T.);
#7064=FACE_OUTER_BOUND('',#10644,.T.);
#7065=FACE_OUTER_BOUND('',#10645,.T.);
#7066=FACE_OUTER_BOUND('',#10646,.T.);
#7067=FACE_OUTER_BOUND('',#10647,.T.);
#7068=FACE_OUTER_BOUND('',#10648,.T.);
#7069=FACE_OUTER_BOUND('',#10649,.T.);
#7070=FACE_OUTER_BOUND('',#10650,.T.);
#7071=FACE_OUTER_BOUND('',#10651,.T.);
#7072=FACE_OUTER_BOUND('',#10652,.T.);
#7073=FACE_OUTER_BOUND('',#10653,.T.);
#7074=FACE_OUTER_BOUND('',#10654,.T.);
#7075=FACE_OUTER_BOUND('',#10655,.T.);
#7076=FACE_OUTER_BOUND('',#10656,.T.);
#7077=FACE_OUTER_BOUND('',#10657,.T.);
#7078=FACE_OUTER_BOUND('',#10659,.T.);
#7079=FACE_OUTER_BOUND('',#10660,.T.);
#7080=FACE_OUTER_BOUND('',#10661,.T.);
#7081=FACE_OUTER_BOUND('',#10662,.T.);
#7082=FACE_OUTER_BOUND('',#10663,.T.);
#7083=FACE_OUTER_BOUND('',#10664,.T.);
#7084=FACE_OUTER_BOUND('',#10665,.T.);
#7085=FACE_OUTER_BOUND('',#10666,.T.);
#7086=FACE_OUTER_BOUND('',#10667,.T.);
#7087=FACE_OUTER_BOUND('',#10668,.T.);
#7088=FACE_OUTER_BOUND('',#10669,.T.);
#7089=FACE_OUTER_BOUND('',#10670,.T.);
#7090=FACE_OUTER_BOUND('',#10671,.T.);
#7091=FACE_OUTER_BOUND('',#10672,.T.);
#7092=FACE_OUTER_BOUND('',#10673,.T.);
#7093=FACE_OUTER_BOUND('',#10674,.T.);
#7094=FACE_OUTER_BOUND('',#10675,.T.);
#7095=FACE_OUTER_BOUND('',#10676,.T.);
#7096=FACE_OUTER_BOUND('',#10677,.T.);
#7097=FACE_OUTER_BOUND('',#10678,.T.);
#7098=FACE_OUTER_BOUND('',#10679,.T.);
#7099=FACE_OUTER_BOUND('',#10680,.T.);
#7100=FACE_OUTER_BOUND('',#10681,.T.);
#7101=FACE_OUTER_BOUND('',#10682,.T.);
#7102=FACE_OUTER_BOUND('',#10683,.T.);
#7103=FACE_OUTER_BOUND('',#10684,.T.);
#7104=FACE_OUTER_BOUND('',#10685,.T.);
#7105=FACE_OUTER_BOUND('',#10686,.T.);
#7106=FACE_OUTER_BOUND('',#10687,.T.);
#7107=FACE_OUTER_BOUND('',#10688,.T.);
#7108=FACE_OUTER_BOUND('',#10689,.T.);
#7109=FACE_OUTER_BOUND('',#10690,.T.);
#7110=FACE_OUTER_BOUND('',#10691,.T.);
#7111=FACE_OUTER_BOUND('',#10692,.T.);
#7112=FACE_OUTER_BOUND('',#10693,.T.);
#7113=FACE_OUTER_BOUND('',#10694,.T.);
#7114=FACE_OUTER_BOUND('',#10696,.T.);
#7115=FACE_OUTER_BOUND('',#10697,.T.);
#7116=FACE_OUTER_BOUND('',#10698,.T.);
#7117=FACE_OUTER_BOUND('',#10699,.T.);
#7118=FACE_OUTER_BOUND('',#10700,.T.);
#7119=FACE_OUTER_BOUND('',#10701,.T.);
#7120=FACE_OUTER_BOUND('',#10702,.T.);
#7121=FACE_OUTER_BOUND('',#10703,.T.);
#7122=FACE_OUTER_BOUND('',#10704,.T.);
#7123=FACE_OUTER_BOUND('',#10705,.T.);
#7124=FACE_OUTER_BOUND('',#10706,.T.);
#7125=FACE_OUTER_BOUND('',#10707,.T.);
#7126=FACE_OUTER_BOUND('',#10708,.T.);
#7127=FACE_OUTER_BOUND('',#10709,.T.);
#7128=FACE_OUTER_BOUND('',#10710,.T.);
#7129=FACE_OUTER_BOUND('',#10711,.T.);
#7130=FACE_OUTER_BOUND('',#10712,.T.);
#7131=FACE_OUTER_BOUND('',#10713,.T.);
#7132=FACE_OUTER_BOUND('',#10714,.T.);
#7133=FACE_OUTER_BOUND('',#10715,.T.);
#7134=FACE_OUTER_BOUND('',#10716,.T.);
#7135=FACE_OUTER_BOUND('',#10717,.T.);
#7136=FACE_OUTER_BOUND('',#10718,.T.);
#7137=FACE_OUTER_BOUND('',#10719,.T.);
#7138=FACE_OUTER_BOUND('',#10720,.T.);
#7139=FACE_OUTER_BOUND('',#10721,.T.);
#7140=FACE_OUTER_BOUND('',#10722,.T.);
#7141=FACE_OUTER_BOUND('',#10723,.T.);
#7142=FACE_OUTER_BOUND('',#10724,.T.);
#7143=FACE_OUTER_BOUND('',#10725,.T.);
#7144=FACE_OUTER_BOUND('',#10726,.T.);
#7145=FACE_OUTER_BOUND('',#10727,.T.);
#7146=FACE_OUTER_BOUND('',#10728,.T.);
#7147=FACE_OUTER_BOUND('',#10730,.T.);
#7148=FACE_OUTER_BOUND('',#10731,.T.);
#7149=FACE_OUTER_BOUND('',#10732,.T.);
#7150=FACE_OUTER_BOUND('',#10733,.T.);
#7151=FACE_OUTER_BOUND('',#10734,.T.);
#7152=FACE_OUTER_BOUND('',#10735,.T.);
#7153=FACE_OUTER_BOUND('',#10736,.T.);
#7154=FACE_OUTER_BOUND('',#10737,.T.);
#7155=FACE_OUTER_BOUND('',#10738,.T.);
#7156=FACE_OUTER_BOUND('',#10739,.T.);
#7157=FACE_OUTER_BOUND('',#10740,.T.);
#7158=FACE_OUTER_BOUND('',#10741,.T.);
#7159=FACE_OUTER_BOUND('',#10742,.T.);
#7160=FACE_OUTER_BOUND('',#10743,.T.);
#7161=FACE_OUTER_BOUND('',#10744,.T.);
#7162=FACE_OUTER_BOUND('',#10745,.T.);
#7163=FACE_OUTER_BOUND('',#10746,.T.);
#7164=FACE_OUTER_BOUND('',#10747,.T.);
#7165=FACE_OUTER_BOUND('',#10748,.T.);
#7166=FACE_OUTER_BOUND('',#10749,.T.);
#7167=FACE_OUTER_BOUND('',#10750,.T.);
#7168=FACE_OUTER_BOUND('',#10751,.T.);
#7169=FACE_OUTER_BOUND('',#10752,.T.);
#7170=FACE_OUTER_BOUND('',#10753,.T.);
#7171=FACE_OUTER_BOUND('',#10754,.T.);
#7172=FACE_OUTER_BOUND('',#10755,.T.);
#7173=FACE_OUTER_BOUND('',#10756,.T.);
#7174=FACE_OUTER_BOUND('',#10757,.T.);
#7175=FACE_OUTER_BOUND('',#10758,.T.);
#7176=FACE_OUTER_BOUND('',#10759,.T.);
#7177=FACE_OUTER_BOUND('',#10760,.T.);
#7178=FACE_OUTER_BOUND('',#10761,.T.);
#7179=FACE_OUTER_BOUND('',#10762,.T.);
#7180=FACE_OUTER_BOUND('',#10763,.T.);
#7181=FACE_OUTER_BOUND('',#10764,.T.);
#7182=FACE_OUTER_BOUND('',#10765,.T.);
#7183=FACE_OUTER_BOUND('',#10766,.T.);
#7184=FACE_OUTER_BOUND('',#10767,.T.);
#7185=FACE_OUTER_BOUND('',#10768,.T.);
#7186=FACE_OUTER_BOUND('',#10769,.T.);
#7187=FACE_OUTER_BOUND('',#10770,.T.);
#7188=FACE_OUTER_BOUND('',#10771,.T.);
#7189=FACE_OUTER_BOUND('',#10772,.T.);
#7190=FACE_OUTER_BOUND('',#10773,.T.);
#7191=FACE_OUTER_BOUND('',#10774,.T.);
#7192=FACE_OUTER_BOUND('',#10775,.T.);
#7193=FACE_OUTER_BOUND('',#10776,.T.);
#7194=FACE_OUTER_BOUND('',#10777,.T.);
#7195=FACE_OUTER_BOUND('',#10778,.T.);
#7196=FACE_OUTER_BOUND('',#10779,.T.);
#7197=FACE_OUTER_BOUND('',#10780,.T.);
#7198=FACE_OUTER_BOUND('',#10781,.T.);
#7199=FACE_OUTER_BOUND('',#10782,.T.);
#7200=FACE_OUTER_BOUND('',#10783,.T.);
#7201=FACE_OUTER_BOUND('',#10784,.T.);
#7202=FACE_OUTER_BOUND('',#10785,.T.);
#7203=FACE_OUTER_BOUND('',#10786,.T.);
#7204=FACE_OUTER_BOUND('',#10787,.T.);
#7205=FACE_OUTER_BOUND('',#10788,.T.);
#7206=FACE_OUTER_BOUND('',#10789,.T.);
#7207=FACE_OUTER_BOUND('',#10790,.T.);
#7208=FACE_OUTER_BOUND('',#10791,.T.);
#7209=FACE_OUTER_BOUND('',#10792,.T.);
#7210=FACE_OUTER_BOUND('',#10793,.T.);
#7211=FACE_OUTER_BOUND('',#10794,.T.);
#7212=FACE_OUTER_BOUND('',#10795,.T.);
#7213=FACE_OUTER_BOUND('',#10796,.T.);
#7214=FACE_OUTER_BOUND('',#10797,.T.);
#7215=FACE_OUTER_BOUND('',#10798,.T.);
#7216=FACE_OUTER_BOUND('',#10799,.T.);
#7217=FACE_OUTER_BOUND('',#10800,.T.);
#7218=FACE_OUTER_BOUND('',#10801,.T.);
#7219=FACE_OUTER_BOUND('',#10802,.T.);
#7220=FACE_OUTER_BOUND('',#10803,.T.);
#7221=FACE_OUTER_BOUND('',#10804,.T.);
#7222=FACE_OUTER_BOUND('',#10805,.T.);
#7223=FACE_OUTER_BOUND('',#10806,.T.);
#7224=FACE_OUTER_BOUND('',#10807,.T.);
#7225=FACE_OUTER_BOUND('',#10808,.T.);
#7226=FACE_OUTER_BOUND('',#10809,.T.);
#7227=FACE_OUTER_BOUND('',#10810,.T.);
#7228=FACE_OUTER_BOUND('',#10811,.T.);
#7229=FACE_OUTER_BOUND('',#10812,.T.);
#7230=FACE_OUTER_BOUND('',#10813,.T.);
#7231=FACE_OUTER_BOUND('',#10814,.T.);
#7232=FACE_OUTER_BOUND('',#10815,.T.);
#7233=FACE_OUTER_BOUND('',#10816,.T.);
#7234=FACE_OUTER_BOUND('',#10817,.T.);
#7235=FACE_OUTER_BOUND('',#10818,.T.);
#7236=FACE_OUTER_BOUND('',#10819,.T.);
#7237=FACE_OUTER_BOUND('',#10820,.T.);
#7238=FACE_OUTER_BOUND('',#10821,.T.);
#7239=FACE_OUTER_BOUND('',#10822,.T.);
#7240=FACE_OUTER_BOUND('',#10823,.T.);
#7241=FACE_OUTER_BOUND('',#10824,.T.);
#7242=FACE_OUTER_BOUND('',#10825,.T.);
#7243=FACE_OUTER_BOUND('',#10826,.T.);
#7244=FACE_OUTER_BOUND('',#10827,.T.);
#7245=FACE_OUTER_BOUND('',#10828,.T.);
#7246=FACE_OUTER_BOUND('',#10829,.T.);
#7247=FACE_OUTER_BOUND('',#10830,.T.);
#7248=FACE_OUTER_BOUND('',#10831,.T.);
#7249=FACE_OUTER_BOUND('',#10832,.T.);
#7250=FACE_OUTER_BOUND('',#10833,.T.);
#7251=FACE_OUTER_BOUND('',#10834,.T.);
#7252=FACE_OUTER_BOUND('',#10835,.T.);
#7253=FACE_OUTER_BOUND('',#10836,.T.);
#7254=FACE_OUTER_BOUND('',#10837,.T.);
#7255=FACE_OUTER_BOUND('',#10838,.T.);
#7256=FACE_OUTER_BOUND('',#10839,.T.);
#7257=FACE_OUTER_BOUND('',#10840,.T.);
#7258=FACE_OUTER_BOUND('',#10841,.T.);
#7259=FACE_OUTER_BOUND('',#10842,.T.);
#7260=FACE_OUTER_BOUND('',#10843,.T.);
#7261=FACE_OUTER_BOUND('',#10845,.T.);
#7262=FACE_OUTER_BOUND('',#10846,.T.);
#7263=FACE_OUTER_BOUND('',#10847,.T.);
#7264=FACE_OUTER_BOUND('',#10848,.T.);
#7265=FACE_OUTER_BOUND('',#10849,.T.);
#7266=FACE_OUTER_BOUND('',#10850,.T.);
#7267=FACE_OUTER_BOUND('',#10851,.T.);
#7268=FACE_OUTER_BOUND('',#10852,.T.);
#7269=FACE_OUTER_BOUND('',#10853,.T.);
#7270=FACE_OUTER_BOUND('',#10854,.T.);
#7271=FACE_OUTER_BOUND('',#10855,.T.);
#7272=FACE_OUTER_BOUND('',#10856,.T.);
#7273=FACE_OUTER_BOUND('',#10857,.T.);
#7274=FACE_OUTER_BOUND('',#10858,.T.);
#7275=FACE_OUTER_BOUND('',#10859,.T.);
#7276=FACE_OUTER_BOUND('',#10860,.T.);
#7277=FACE_OUTER_BOUND('',#10861,.T.);
#7278=FACE_OUTER_BOUND('',#10862,.T.);
#7279=FACE_OUTER_BOUND('',#10863,.T.);
#7280=FACE_OUTER_BOUND('',#10864,.T.);
#7281=FACE_OUTER_BOUND('',#10865,.T.);
#7282=FACE_OUTER_BOUND('',#10866,.T.);
#7283=FACE_OUTER_BOUND('',#10867,.T.);
#7284=FACE_OUTER_BOUND('',#10868,.T.);
#7285=FACE_OUTER_BOUND('',#10869,.T.);
#7286=FACE_OUTER_BOUND('',#10870,.T.);
#7287=FACE_OUTER_BOUND('',#10871,.T.);
#7288=FACE_OUTER_BOUND('',#10872,.T.);
#7289=FACE_OUTER_BOUND('',#10873,.T.);
#7290=FACE_OUTER_BOUND('',#10874,.T.);
#7291=FACE_OUTER_BOUND('',#10875,.T.);
#7292=EDGE_LOOP('',(#39039,#39040,#39041,#39042));
#7293=EDGE_LOOP('',(#39043,#39044,#39045,#39046));
#7294=EDGE_LOOP('',(#39047,#39048,#39049,#39050));
#7295=EDGE_LOOP('',(#39051,#39052,#39053,#39054));
#7296=EDGE_LOOP('',(#39055,#39056,#39057,#39058));
#7297=EDGE_LOOP('',(#39059,#39060,#39061,#39062));
#7298=EDGE_LOOP('',(#39063,#39064,#39065,#39066));
#7299=EDGE_LOOP('',(#39067,#39068,#39069,#39070));
#7300=EDGE_LOOP('',(#39071,#39072,#39073,#39074));
#7301=EDGE_LOOP('',(#39075,#39076,#39077,#39078));
#7302=EDGE_LOOP('',(#39079,#39080,#39081,#39082));
#7303=EDGE_LOOP('',(#39083,#39084,#39085,#39086));
#7304=EDGE_LOOP('',(#39087,#39088,#39089,#39090));
#7305=EDGE_LOOP('',(#39091,#39092,#39093,#39094));
#7306=EDGE_LOOP('',(#39095,#39096,#39097,#39098));
#7307=EDGE_LOOP('',(#39099,#39100,#39101,#39102));
#7308=EDGE_LOOP('',(#39103,#39104,#39105,#39106));
#7309=EDGE_LOOP('',(#39107,#39108,#39109,#39110));
#7310=EDGE_LOOP('',(#39111,#39112,#39113,#39114));
#7311=EDGE_LOOP('',(#39115,#39116,#39117,#39118));
#7312=EDGE_LOOP('',(#39119,#39120,#39121,#39122,#39123,#39124,#39125,#39126,
#39127,#39128,#39129,#39130));
#7313=EDGE_LOOP('',(#39131,#39132,#39133,#39134,#39135,#39136,#39137,#39138));
#7314=EDGE_LOOP('',(#39139,#39140,#39141,#39142));
#7315=EDGE_LOOP('',(#39143,#39144,#39145,#39146));
#7316=EDGE_LOOP('',(#39147,#39148,#39149,#39150));
#7317=EDGE_LOOP('',(#39151,#39152,#39153,#39154));
#7318=EDGE_LOOP('',(#39155,#39156,#39157,#39158));
#7319=EDGE_LOOP('',(#39159,#39160,#39161,#39162));
#7320=EDGE_LOOP('',(#39163,#39164,#39165,#39166));
#7321=EDGE_LOOP('',(#39167,#39168,#39169,#39170));
#7322=EDGE_LOOP('',(#39171,#39172,#39173,#39174));
#7323=EDGE_LOOP('',(#39175,#39176,#39177,#39178));
#7324=EDGE_LOOP('',(#39179,#39180,#39181,#39182));
#7325=EDGE_LOOP('',(#39183,#39184,#39185,#39186));
#7326=EDGE_LOOP('',(#39187,#39188,#39189,#39190));
#7327=EDGE_LOOP('',(#39191,#39192,#39193,#39194));
#7328=EDGE_LOOP('',(#39195,#39196,#39197,#39198));
#7329=EDGE_LOOP('',(#39199,#39200,#39201,#39202));
#7330=EDGE_LOOP('',(#39203,#39204,#39205,#39206));
#7331=EDGE_LOOP('',(#39207,#39208,#39209,#39210));
#7332=EDGE_LOOP('',(#39211,#39212,#39213,#39214));
#7333=EDGE_LOOP('',(#39215,#39216,#39217,#39218));
#7334=EDGE_LOOP('',(#39219,#39220,#39221,#39222));
#7335=EDGE_LOOP('',(#39223,#39224,#39225,#39226));
#7336=EDGE_LOOP('',(#39227,#39228,#39229,#39230));
#7337=EDGE_LOOP('',(#39231,#39232,#39233,#39234));
#7338=EDGE_LOOP('',(#39235,#39236,#39237,#39238));
#7339=EDGE_LOOP('',(#39239,#39240,#39241,#39242));
#7340=EDGE_LOOP('',(#39243,#39244,#39245,#39246));
#7341=EDGE_LOOP('',(#39247,#39248,#39249,#39250));
#7342=EDGE_LOOP('',(#39251,#39252,#39253,#39254));
#7343=EDGE_LOOP('',(#39255,#39256,#39257,#39258));
#7344=EDGE_LOOP('',(#39259,#39260,#39261,#39262,#39263,#39264,#39265,#39266,
#39267,#39268,#39269,#39270,#39271,#39272,#39273,#39274,#39275,#39276,#39277,
#39278,#39279,#39280));
#7345=EDGE_LOOP('',(#39281,#39282,#39283,#39284,#39285,#39286,#39287,#39288));
#7346=EDGE_LOOP('',(#39289,#39290,#39291,#39292,#39293,#39294,#39295,#39296));
#7347=EDGE_LOOP('',(#39297,#39298,#39299,#39300,#39301,#39302,#39303,#39304));
#7348=EDGE_LOOP('',(#39305,#39306,#39307,#39308));
#7349=EDGE_LOOP('',(#39309,#39310,#39311,#39312));
#7350=EDGE_LOOP('',(#39313,#39314,#39315,#39316));
#7351=EDGE_LOOP('',(#39317,#39318,#39319,#39320));
#7352=EDGE_LOOP('',(#39321,#39322,#39323,#39324));
#7353=EDGE_LOOP('',(#39325,#39326,#39327,#39328));
#7354=EDGE_LOOP('',(#39329,#39330,#39331,#39332));
#7355=EDGE_LOOP('',(#39333,#39334,#39335,#39336));
#7356=EDGE_LOOP('',(#39337,#39338,#39339,#39340));
#7357=EDGE_LOOP('',(#39341,#39342,#39343,#39344));
#7358=EDGE_LOOP('',(#39345,#39346,#39347,#39348));
#7359=EDGE_LOOP('',(#39349,#39350,#39351,#39352));
#7360=EDGE_LOOP('',(#39353,#39354,#39355,#39356));
#7361=EDGE_LOOP('',(#39357,#39358,#39359,#39360));
#7362=EDGE_LOOP('',(#39361,#39362,#39363,#39364));
#7363=EDGE_LOOP('',(#39365,#39366,#39367,#39368));
#7364=EDGE_LOOP('',(#39369,#39370,#39371,#39372));
#7365=EDGE_LOOP('',(#39373,#39374,#39375,#39376));
#7366=EDGE_LOOP('',(#39377,#39378,#39379,#39380));
#7367=EDGE_LOOP('',(#39381,#39382,#39383,#39384));
#7368=EDGE_LOOP('',(#39385,#39386,#39387,#39388,#39389,#39390,#39391,#39392,
#39393,#39394,#39395,#39396));
#7369=EDGE_LOOP('',(#39397,#39398,#39399,#39400,#39401,#39402,#39403,#39404));
#7370=EDGE_LOOP('',(#39405,#39406,#39407,#39408));
#7371=EDGE_LOOP('',(#39409,#39410,#39411,#39412));
#7372=EDGE_LOOP('',(#39413,#39414,#39415,#39416));
#7373=EDGE_LOOP('',(#39417,#39418,#39419,#39420));
#7374=EDGE_LOOP('',(#39421,#39422,#39423,#39424));
#7375=EDGE_LOOP('',(#39425,#39426,#39427,#39428));
#7376=EDGE_LOOP('',(#39429,#39430,#39431,#39432));
#7377=EDGE_LOOP('',(#39433,#39434,#39435,#39436));
#7378=EDGE_LOOP('',(#39437,#39438,#39439,#39440));
#7379=EDGE_LOOP('',(#39441,#39442,#39443,#39444));
#7380=EDGE_LOOP('',(#39445,#39446,#39447,#39448));
#7381=EDGE_LOOP('',(#39449,#39450,#39451,#39452));
#7382=EDGE_LOOP('',(#39453,#39454,#39455,#39456));
#7383=EDGE_LOOP('',(#39457,#39458,#39459,#39460));
#7384=EDGE_LOOP('',(#39461,#39462,#39463,#39464));
#7385=EDGE_LOOP('',(#39465,#39466,#39467,#39468));
#7386=EDGE_LOOP('',(#39469,#39470,#39471,#39472));
#7387=EDGE_LOOP('',(#39473,#39474,#39475,#39476));
#7388=EDGE_LOOP('',(#39477,#39478,#39479,#39480));
#7389=EDGE_LOOP('',(#39481,#39482,#39483,#39484));
#7390=EDGE_LOOP('',(#39485,#39486,#39487,#39488));
#7391=EDGE_LOOP('',(#39489,#39490,#39491,#39492));
#7392=EDGE_LOOP('',(#39493,#39494,#39495,#39496));
#7393=EDGE_LOOP('',(#39497,#39498,#39499,#39500));
#7394=EDGE_LOOP('',(#39501,#39502,#39503,#39504));
#7395=EDGE_LOOP('',(#39505,#39506,#39507,#39508));
#7396=EDGE_LOOP('',(#39509,#39510,#39511,#39512));
#7397=EDGE_LOOP('',(#39513,#39514,#39515,#39516));
#7398=EDGE_LOOP('',(#39517,#39518,#39519,#39520));
#7399=EDGE_LOOP('',(#39521,#39522,#39523,#39524));
#7400=EDGE_LOOP('',(#39525,#39526,#39527,#39528));
#7401=EDGE_LOOP('',(#39529,#39530,#39531,#39532));
#7402=EDGE_LOOP('',(#39533,#39534,#39535,#39536));
#7403=EDGE_LOOP('',(#39537,#39538,#39539,#39540,#39541,#39542,#39543,#39544,
#39545,#39546,#39547,#39548,#39549,#39550,#39551,#39552));
#7404=EDGE_LOOP('',(#39553,#39554,#39555,#39556,#39557,#39558,#39559,#39560,
#39561));
#7405=EDGE_LOOP('',(#39562,#39563,#39564,#39565,#39566,#39567,#39568,#39569));
#7406=EDGE_LOOP('',(#39570,#39571,#39572,#39573,#39574,#39575,#39576,#39577,
#39578));
#7407=EDGE_LOOP('',(#39579,#39580,#39581,#39582,#39583,#39584,#39585,#39586));
#7408=EDGE_LOOP('',(#39587,#39588,#39589,#39590,#39591,#39592,#39593,#39594));
#7409=EDGE_LOOP('',(#39595,#39596,#39597,#39598));
#7410=EDGE_LOOP('',(#39599,#39600,#39601,#39602));
#7411=EDGE_LOOP('',(#39603,#39604,#39605,#39606));
#7412=EDGE_LOOP('',(#39607,#39608,#39609,#39610));
#7413=EDGE_LOOP('',(#39611,#39612,#39613,#39614));
#7414=EDGE_LOOP('',(#39615,#39616,#39617,#39618));
#7415=EDGE_LOOP('',(#39619,#39620,#39621,#39622));
#7416=EDGE_LOOP('',(#39623,#39624,#39625,#39626));
#7417=EDGE_LOOP('',(#39627,#39628,#39629,#39630));
#7418=EDGE_LOOP('',(#39631,#39632,#39633,#39634));
#7419=EDGE_LOOP('',(#39635,#39636,#39637,#39638));
#7420=EDGE_LOOP('',(#39639,#39640,#39641,#39642));
#7421=EDGE_LOOP('',(#39643,#39644,#39645,#39646));
#7422=EDGE_LOOP('',(#39647,#39648,#39649,#39650));
#7423=EDGE_LOOP('',(#39651,#39652,#39653,#39654));
#7424=EDGE_LOOP('',(#39655,#39656,#39657,#39658));
#7425=EDGE_LOOP('',(#39659,#39660,#39661,#39662));
#7426=EDGE_LOOP('',(#39663,#39664,#39665,#39666));
#7427=EDGE_LOOP('',(#39667,#39668,#39669,#39670));
#7428=EDGE_LOOP('',(#39671,#39672,#39673,#39674));
#7429=EDGE_LOOP('',(#39675,#39676,#39677,#39678,#39679,#39680,#39681,#39682,
#39683,#39684,#39685,#39686));
#7430=EDGE_LOOP('',(#39687,#39688,#39689,#39690,#39691,#39692,#39693,#39694));
#7431=EDGE_LOOP('',(#39695,#39696,#39697,#39698));
#7432=EDGE_LOOP('',(#39699,#39700,#39701,#39702));
#7433=EDGE_LOOP('',(#39703,#39704,#39705,#39706));
#7434=EDGE_LOOP('',(#39707,#39708,#39709,#39710));
#7435=EDGE_LOOP('',(#39711,#39712,#39713,#39714));
#7436=EDGE_LOOP('',(#39715,#39716,#39717,#39718));
#7437=EDGE_LOOP('',(#39719,#39720,#39721,#39722));
#7438=EDGE_LOOP('',(#39723,#39724,#39725,#39726));
#7439=EDGE_LOOP('',(#39727,#39728,#39729,#39730));
#7440=EDGE_LOOP('',(#39731,#39732,#39733,#39734));
#7441=EDGE_LOOP('',(#39735,#39736,#39737,#39738));
#7442=EDGE_LOOP('',(#39739,#39740,#39741,#39742,#39743,#39744,#39745,#39746,
#39747,#39748,#39749));
#7443=EDGE_LOOP('',(#39750,#39751,#39752,#39753,#39754,#39755,#39756,#39757));
#7444=EDGE_LOOP('',(#39758,#39759,#39760,#39761));
#7445=EDGE_LOOP('',(#39762,#39763,#39764,#39765));
#7446=EDGE_LOOP('',(#39766,#39767,#39768,#39769));
#7447=EDGE_LOOP('',(#39770,#39771,#39772,#39773));
#7448=EDGE_LOOP('',(#39774,#39775,#39776,#39777));
#7449=EDGE_LOOP('',(#39778,#39779,#39780,#39781));
#7450=EDGE_LOOP('',(#39782,#39783,#39784,#39785));
#7451=EDGE_LOOP('',(#39786,#39787,#39788,#39789));
#7452=EDGE_LOOP('',(#39790,#39791,#39792,#39793));
#7453=EDGE_LOOP('',(#39794,#39795,#39796,#39797));
#7454=EDGE_LOOP('',(#39798,#39799,#39800,#39801));
#7455=EDGE_LOOP('',(#39802,#39803,#39804,#39805));
#7456=EDGE_LOOP('',(#39806,#39807,#39808,#39809));
#7457=EDGE_LOOP('',(#39810,#39811,#39812,#39813));
#7458=EDGE_LOOP('',(#39814,#39815,#39816,#39817));
#7459=EDGE_LOOP('',(#39818,#39819,#39820,#39821));
#7460=EDGE_LOOP('',(#39822,#39823,#39824,#39825));
#7461=EDGE_LOOP('',(#39826,#39827,#39828,#39829));
#7462=EDGE_LOOP('',(#39830,#39831,#39832,#39833));
#7463=EDGE_LOOP('',(#39834,#39835,#39836,#39837));
#7464=EDGE_LOOP('',(#39838,#39839,#39840,#39841,#39842,#39843,#39844,#39845,
#39846,#39847,#39848,#39849));
#7465=EDGE_LOOP('',(#39850,#39851,#39852,#39853,#39854,#39855,#39856,#39857));
#7466=EDGE_LOOP('',(#39858,#39859,#39860,#39861));
#7467=EDGE_LOOP('',(#39862,#39863,#39864,#39865));
#7468=EDGE_LOOP('',(#39866,#39867,#39868,#39869));
#7469=EDGE_LOOP('',(#39870,#39871,#39872,#39873));
#7470=EDGE_LOOP('',(#39874,#39875,#39876,#39877));
#7471=EDGE_LOOP('',(#39878,#39879,#39880,#39881));
#7472=EDGE_LOOP('',(#39882,#39883,#39884,#39885));
#7473=EDGE_LOOP('',(#39886,#39887,#39888,#39889));
#7474=EDGE_LOOP('',(#39890,#39891,#39892,#39893));
#7475=EDGE_LOOP('',(#39894,#39895,#39896,#39897));
#7476=EDGE_LOOP('',(#39898,#39899,#39900,#39901));
#7477=EDGE_LOOP('',(#39902,#39903,#39904,#39905));
#7478=EDGE_LOOP('',(#39906,#39907,#39908,#39909));
#7479=EDGE_LOOP('',(#39910,#39911,#39912,#39913));
#7480=EDGE_LOOP('',(#39914,#39915,#39916,#39917));
#7481=EDGE_LOOP('',(#39918,#39919,#39920,#39921));
#7482=EDGE_LOOP('',(#39922,#39923,#39924,#39925));
#7483=EDGE_LOOP('',(#39926,#39927,#39928,#39929));
#7484=EDGE_LOOP('',(#39930,#39931,#39932,#39933));
#7485=EDGE_LOOP('',(#39934,#39935,#39936,#39937));
#7486=EDGE_LOOP('',(#39938,#39939,#39940,#39941));
#7487=EDGE_LOOP('',(#39942,#39943,#39944,#39945));
#7488=EDGE_LOOP('',(#39946,#39947,#39948,#39949));
#7489=EDGE_LOOP('',(#39950,#39951,#39952,#39953));
#7490=EDGE_LOOP('',(#39954,#39955,#39956,#39957));
#7491=EDGE_LOOP('',(#39958,#39959,#39960,#39961));
#7492=EDGE_LOOP('',(#39962,#39963,#39964,#39965));
#7493=EDGE_LOOP('',(#39966,#39967,#39968,#39969));
#7494=EDGE_LOOP('',(#39970,#39971,#39972,#39973,#39974,#39975,#39976,#39977,
#39978,#39979,#39980,#39981,#39982,#39983,#39984,#39985,#39986,#39987,#39988));
#7495=EDGE_LOOP('',(#39989,#39990,#39991,#39992,#39993,#39994,#39995,#39996,
#39997));
#7496=EDGE_LOOP('',(#39998,#39999,#40000,#40001,#40002,#40003,#40004,#40005,
#40006));
#7497=EDGE_LOOP('',(#40007,#40008,#40009,#40010,#40011,#40012,#40013,#40014));
#7498=EDGE_LOOP('',(#40015,#40016,#40017,#40018));
#7499=EDGE_LOOP('',(#40019,#40020,#40021,#40022));
#7500=EDGE_LOOP('',(#40023,#40024,#40025,#40026));
#7501=EDGE_LOOP('',(#40027,#40028,#40029,#40030));
#7502=EDGE_LOOP('',(#40031,#40032,#40033,#40034));
#7503=EDGE_LOOP('',(#40035,#40036,#40037,#40038));
#7504=EDGE_LOOP('',(#40039,#40040,#40041,#40042));
#7505=EDGE_LOOP('',(#40043,#40044,#40045,#40046));
#7506=EDGE_LOOP('',(#40047,#40048,#40049,#40050));
#7507=EDGE_LOOP('',(#40051,#40052,#40053,#40054));
#7508=EDGE_LOOP('',(#40055,#40056,#40057,#40058));
#7509=EDGE_LOOP('',(#40059,#40060,#40061,#40062));
#7510=EDGE_LOOP('',(#40063,#40064,#40065,#40066));
#7511=EDGE_LOOP('',(#40067,#40068,#40069,#40070));
#7512=EDGE_LOOP('',(#40071,#40072,#40073,#40074));
#7513=EDGE_LOOP('',(#40075,#40076,#40077,#40078));
#7514=EDGE_LOOP('',(#40079,#40080,#40081,#40082));
#7515=EDGE_LOOP('',(#40083,#40084,#40085,#40086));
#7516=EDGE_LOOP('',(#40087,#40088,#40089,#40090));
#7517=EDGE_LOOP('',(#40091,#40092,#40093,#40094));
#7518=EDGE_LOOP('',(#40095,#40096,#40097,#40098,#40099,#40100,#40101,#40102,
#40103,#40104,#40105,#40106));
#7519=EDGE_LOOP('',(#40107,#40108,#40109,#40110,#40111,#40112,#40113,#40114));
#7520=EDGE_LOOP('',(#40115,#40116,#40117,#40118));
#7521=EDGE_LOOP('',(#40119,#40120,#40121,#40122));
#7522=EDGE_LOOP('',(#40123,#40124,#40125,#40126));
#7523=EDGE_LOOP('',(#40127,#40128,#40129,#40130));
#7524=EDGE_LOOP('',(#40131,#40132,#40133,#40134));
#7525=EDGE_LOOP('',(#40135,#40136,#40137,#40138));
#7526=EDGE_LOOP('',(#40139,#40140,#40141,#40142));
#7527=EDGE_LOOP('',(#40143,#40144,#40145,#40146));
#7528=EDGE_LOOP('',(#40147,#40148,#40149,#40150));
#7529=EDGE_LOOP('',(#40151,#40152,#40153,#40154));
#7530=EDGE_LOOP('',(#40155,#40156,#40157,#40158));
#7531=EDGE_LOOP('',(#40159,#40160,#40161,#40162));
#7532=EDGE_LOOP('',(#40163,#40164,#40165,#40166));
#7533=EDGE_LOOP('',(#40167,#40168,#40169,#40170));
#7534=EDGE_LOOP('',(#40171,#40172,#40173,#40174));
#7535=EDGE_LOOP('',(#40175,#40176,#40177,#40178));
#7536=EDGE_LOOP('',(#40179,#40180,#40181,#40182));
#7537=EDGE_LOOP('',(#40183,#40184,#40185,#40186));
#7538=EDGE_LOOP('',(#40187,#40188,#40189,#40190));
#7539=EDGE_LOOP('',(#40191,#40192,#40193,#40194));
#7540=EDGE_LOOP('',(#40195,#40196,#40197,#40198));
#7541=EDGE_LOOP('',(#40199,#40200,#40201,#40202));
#7542=EDGE_LOOP('',(#40203,#40204,#40205,#40206,#40207,#40208,#40209,#40210,
#40211,#40212,#40213,#40214,#40215,#40216,#40217,#40218,#40219,#40220,#40221,
#40222,#40223,#40224));
#7543=EDGE_LOOP('',(#40225,#40226,#40227,#40228,#40229,#40230,#40231,#40232));
#7544=EDGE_LOOP('',(#40233,#40234,#40235,#40236));
#7545=EDGE_LOOP('',(#40237,#40238,#40239,#40240));
#7546=EDGE_LOOP('',(#40241,#40242,#40243,#40244));
#7547=EDGE_LOOP('',(#40245,#40246,#40247,#40248));
#7548=EDGE_LOOP('',(#40249,#40250,#40251,#40252));
#7549=EDGE_LOOP('',(#40253,#40254,#40255,#40256));
#7550=EDGE_LOOP('',(#40257,#40258,#40259,#40260));
#7551=EDGE_LOOP('',(#40261,#40262,#40263,#40264));
#7552=EDGE_LOOP('',(#40265,#40266,#40267,#40268));
#7553=EDGE_LOOP('',(#40269,#40270,#40271,#40272));
#7554=EDGE_LOOP('',(#40273,#40274,#40275,#40276));
#7555=EDGE_LOOP('',(#40277,#40278,#40279,#40280));
#7556=EDGE_LOOP('',(#40281,#40282,#40283,#40284));
#7557=EDGE_LOOP('',(#40285,#40286,#40287,#40288));
#7558=EDGE_LOOP('',(#40289,#40290,#40291,#40292));
#7559=EDGE_LOOP('',(#40293,#40294,#40295,#40296));
#7560=EDGE_LOOP('',(#40297,#40298,#40299,#40300));
#7561=EDGE_LOOP('',(#40301,#40302,#40303,#40304));
#7562=EDGE_LOOP('',(#40305,#40306,#40307,#40308));
#7563=EDGE_LOOP('',(#40309,#40310,#40311,#40312));
#7564=EDGE_LOOP('',(#40313,#40314,#40315,#40316,#40317,#40318,#40319,#40320,
#40321,#40322,#40323,#40324));
#7565=EDGE_LOOP('',(#40325,#40326,#40327,#40328,#40329,#40330,#40331,#40332));
#7566=EDGE_LOOP('',(#40333,#40334,#40335,#40336));
#7567=EDGE_LOOP('',(#40337,#40338,#40339,#40340));
#7568=EDGE_LOOP('',(#40341,#40342,#40343,#40344));
#7569=EDGE_LOOP('',(#40345,#40346,#40347,#40348));
#7570=EDGE_LOOP('',(#40349,#40350,#40351,#40352));
#7571=EDGE_LOOP('',(#40353,#40354,#40355,#40356));
#7572=EDGE_LOOP('',(#40357,#40358,#40359,#40360));
#7573=EDGE_LOOP('',(#40361,#40362,#40363,#40364));
#7574=EDGE_LOOP('',(#40365,#40366,#40367,#40368));
#7575=EDGE_LOOP('',(#40369,#40370,#40371,#40372));
#7576=EDGE_LOOP('',(#40373,#40374,#40375,#40376));
#7577=EDGE_LOOP('',(#40377,#40378,#40379,#40380));
#7578=EDGE_LOOP('',(#40381,#40382,#40383,#40384));
#7579=EDGE_LOOP('',(#40385,#40386,#40387,#40388));
#7580=EDGE_LOOP('',(#40389,#40390,#40391,#40392,#40393,#40394,#40395,#40396,
#40397,#40398,#40399));
#7581=EDGE_LOOP('',(#40400,#40401,#40402));
#7582=EDGE_LOOP('',(#40403,#40404,#40405));
#7583=EDGE_LOOP('',(#40406,#40407,#40408,#40409,#40410,#40411,#40412,#40413));
#7584=EDGE_LOOP('',(#40414,#40415,#40416,#40417));
#7585=EDGE_LOOP('',(#40418,#40419,#40420,#40421));
#7586=EDGE_LOOP('',(#40422,#40423,#40424,#40425));
#7587=EDGE_LOOP('',(#40426,#40427,#40428,#40429));
#7588=EDGE_LOOP('',(#40430,#40431,#40432,#40433));
#7589=EDGE_LOOP('',(#40434,#40435,#40436,#40437));
#7590=EDGE_LOOP('',(#40438,#40439,#40440,#40441));
#7591=EDGE_LOOP('',(#40442,#40443,#40444,#40445));
#7592=EDGE_LOOP('',(#40446,#40447,#40448,#40449));
#7593=EDGE_LOOP('',(#40450,#40451,#40452,#40453));
#7594=EDGE_LOOP('',(#40454,#40455,#40456,#40457));
#7595=EDGE_LOOP('',(#40458,#40459,#40460,#40461));
#7596=EDGE_LOOP('',(#40462,#40463,#40464,#40465));
#7597=EDGE_LOOP('',(#40466,#40467,#40468,#40469));
#7598=EDGE_LOOP('',(#40470,#40471,#40472,#40473));
#7599=EDGE_LOOP('',(#40474,#40475,#40476,#40477));
#7600=EDGE_LOOP('',(#40478,#40479,#40480,#40481));
#7601=EDGE_LOOP('',(#40482,#40483,#40484,#40485));
#7602=EDGE_LOOP('',(#40486,#40487,#40488,#40489));
#7603=EDGE_LOOP('',(#40490,#40491,#40492,#40493));
#7604=EDGE_LOOP('',(#40494,#40495,#40496,#40497,#40498,#40499,#40500,#40501,
#40502,#40503,#40504,#40505));
#7605=EDGE_LOOP('',(#40506,#40507,#40508,#40509,#40510,#40511,#40512,#40513));
#7606=EDGE_LOOP('',(#40514,#40515,#40516,#40517));
#7607=EDGE_LOOP('',(#40518,#40519,#40520,#40521));
#7608=EDGE_LOOP('',(#40522,#40523,#40524,#40525));
#7609=EDGE_LOOP('',(#40526,#40527,#40528,#40529));
#7610=EDGE_LOOP('',(#40530,#40531,#40532,#40533));
#7611=EDGE_LOOP('',(#40534,#40535,#40536,#40537));
#7612=EDGE_LOOP('',(#40538,#40539,#40540,#40541));
#7613=EDGE_LOOP('',(#40542,#40543,#40544,#40545));
#7614=EDGE_LOOP('',(#40546,#40547,#40548,#40549));
#7615=EDGE_LOOP('',(#40550,#40551,#40552,#40553));
#7616=EDGE_LOOP('',(#40554,#40555,#40556,#40557));
#7617=EDGE_LOOP('',(#40558,#40559,#40560,#40561));
#7618=EDGE_LOOP('',(#40562,#40563,#40564,#40565));
#7619=EDGE_LOOP('',(#40566,#40567,#40568,#40569));
#7620=EDGE_LOOP('',(#40570,#40571,#40572,#40573));
#7621=EDGE_LOOP('',(#40574,#40575,#40576,#40577));
#7622=EDGE_LOOP('',(#40578,#40579,#40580,#40581));
#7623=EDGE_LOOP('',(#40582,#40583,#40584,#40585));
#7624=EDGE_LOOP('',(#40586,#40587,#40588,#40589));
#7625=EDGE_LOOP('',(#40590,#40591,#40592,#40593));
#7626=EDGE_LOOP('',(#40594,#40595,#40596,#40597));
#7627=EDGE_LOOP('',(#40598,#40599,#40600,#40601));
#7628=EDGE_LOOP('',(#40602,#40603,#40604,#40605));
#7629=EDGE_LOOP('',(#40606,#40607,#40608,#40609));
#7630=EDGE_LOOP('',(#40610,#40611,#40612,#40613));
#7631=EDGE_LOOP('',(#40614,#40615,#40616,#40617));
#7632=EDGE_LOOP('',(#40618,#40619,#40620,#40621));
#7633=EDGE_LOOP('',(#40622,#40623,#40624,#40625));
#7634=EDGE_LOOP('',(#40626,#40627,#40628,#40629));
#7635=EDGE_LOOP('',(#40630,#40631,#40632,#40633));
#7636=EDGE_LOOP('',(#40634,#40635,#40636,#40637,#40638,#40639,#40640,#40641,
#40642,#40643,#40644,#40645,#40646,#40647,#40648,#40649,#40650,#40651,#40652,
#40653,#40654,#40655,#40656,#40657,#40658,#40659,#40660,#40661,#40662,#40663));
#7637=EDGE_LOOP('',(#40664,#40665,#40666,#40667,#40668,#40669,#40670,#40671));
#7638=EDGE_LOOP('',(#40672,#40673,#40674,#40675));
#7639=EDGE_LOOP('',(#40676,#40677,#40678,#40679));
#7640=EDGE_LOOP('',(#40680,#40681,#40682,#40683));
#7641=EDGE_LOOP('',(#40684,#40685,#40686,#40687));
#7642=EDGE_LOOP('',(#40688,#40689,#40690,#40691));
#7643=EDGE_LOOP('',(#40692,#40693,#40694,#40695));
#7644=EDGE_LOOP('',(#40696,#40697,#40698,#40699));
#7645=EDGE_LOOP('',(#40700,#40701,#40702,#40703));
#7646=EDGE_LOOP('',(#40704,#40705,#40706,#40707));
#7647=EDGE_LOOP('',(#40708,#40709,#40710,#40711));
#7648=EDGE_LOOP('',(#40712,#40713,#40714,#40715));
#7649=EDGE_LOOP('',(#40716,#40717,#40718,#40719));
#7650=EDGE_LOOP('',(#40720,#40721,#40722,#40723));
#7651=EDGE_LOOP('',(#40724,#40725,#40726,#40727));
#7652=EDGE_LOOP('',(#40728,#40729,#40730,#40731));
#7653=EDGE_LOOP('',(#40732,#40733,#40734,#40735));
#7654=EDGE_LOOP('',(#40736,#40737,#40738,#40739));
#7655=EDGE_LOOP('',(#40740,#40741,#40742,#40743));
#7656=EDGE_LOOP('',(#40744,#40745,#40746,#40747));
#7657=EDGE_LOOP('',(#40748,#40749,#40750,#40751));
#7658=EDGE_LOOP('',(#40752,#40753,#40754,#40755,#40756,#40757,#40758,#40759,
#40760,#40761,#40762,#40763));
#7659=EDGE_LOOP('',(#40764,#40765,#40766,#40767,#40768,#40769,#40770,#40771));
#7660=EDGE_LOOP('',(#40772,#40773,#40774,#40775));
#7661=EDGE_LOOP('',(#40776,#40777,#40778,#40779));
#7662=EDGE_LOOP('',(#40780,#40781,#40782,#40783));
#7663=EDGE_LOOP('',(#40784,#40785,#40786,#40787));
#7664=EDGE_LOOP('',(#40788,#40789,#40790,#40791));
#7665=EDGE_LOOP('',(#40792,#40793,#40794,#40795));
#7666=EDGE_LOOP('',(#40796,#40797,#40798,#40799));
#7667=EDGE_LOOP('',(#40800,#40801,#40802,#40803));
#7668=EDGE_LOOP('',(#40804,#40805,#40806,#40807));
#7669=EDGE_LOOP('',(#40808,#40809,#40810,#40811));
#7670=EDGE_LOOP('',(#40812,#40813,#40814,#40815));
#7671=EDGE_LOOP('',(#40816,#40817,#40818,#40819));
#7672=EDGE_LOOP('',(#40820,#40821,#40822,#40823));
#7673=EDGE_LOOP('',(#40824,#40825,#40826,#40827));
#7674=EDGE_LOOP('',(#40828,#40829,#40830,#40831));
#7675=EDGE_LOOP('',(#40832,#40833,#40834,#40835));
#7676=EDGE_LOOP('',(#40836,#40837,#40838,#40839));
#7677=EDGE_LOOP('',(#40840,#40841,#40842,#40843));
#7678=EDGE_LOOP('',(#40844,#40845,#40846,#40847));
#7679=EDGE_LOOP('',(#40848,#40849,#40850,#40851));
#7680=EDGE_LOOP('',(#40852,#40853,#40854,#40855));
#7681=EDGE_LOOP('',(#40856,#40857,#40858,#40859));
#7682=EDGE_LOOP('',(#40860,#40861,#40862,#40863,#40864,#40865,#40866,#40867,
#40868,#40869,#40870,#40871,#40872,#40873,#40874,#40875,#40876,#40877,#40878,
#40879,#40880,#40881));
#7683=EDGE_LOOP('',(#40882,#40883,#40884,#40885,#40886,#40887,#40888,#40889));
#7684=EDGE_LOOP('',(#40890,#40891,#40892,#40893));
#7685=EDGE_LOOP('',(#40894,#40895,#40896,#40897));
#7686=EDGE_LOOP('',(#40898,#40899,#40900,#40901));
#7687=EDGE_LOOP('',(#40902,#40903,#40904,#40905));
#7688=EDGE_LOOP('',(#40906,#40907,#40908,#40909));
#7689=EDGE_LOOP('',(#40910,#40911,#40912,#40913));
#7690=EDGE_LOOP('',(#40914,#40915,#40916,#40917));
#7691=EDGE_LOOP('',(#40918,#40919,#40920,#40921));
#7692=EDGE_LOOP('',(#40922,#40923,#40924,#40925));
#7693=EDGE_LOOP('',(#40926,#40927,#40928,#40929));
#7694=EDGE_LOOP('',(#40930,#40931,#40932,#40933));
#7695=EDGE_LOOP('',(#40934,#40935,#40936,#40937));
#7696=EDGE_LOOP('',(#40938,#40939,#40940,#40941));
#7697=EDGE_LOOP('',(#40942,#40943,#40944,#40945));
#7698=EDGE_LOOP('',(#40946,#40947,#40948,#40949));
#7699=EDGE_LOOP('',(#40950,#40951,#40952,#40953));
#7700=EDGE_LOOP('',(#40954,#40955,#40956,#40957));
#7701=EDGE_LOOP('',(#40958,#40959,#40960,#40961));
#7702=EDGE_LOOP('',(#40962,#40963,#40964,#40965));
#7703=EDGE_LOOP('',(#40966,#40967,#40968,#40969));
#7704=EDGE_LOOP('',(#40970,#40971,#40972,#40973,#40974,#40975,#40976,#40977,
#40978,#40979,#40980,#40981));
#7705=EDGE_LOOP('',(#40982,#40983,#40984,#40985,#40986,#40987,#40988,#40989));
#7706=EDGE_LOOP('',(#40990,#40991,#40992,#40993));
#7707=EDGE_LOOP('',(#40994,#40995,#40996,#40997));
#7708=EDGE_LOOP('',(#40998,#40999,#41000,#41001));
#7709=EDGE_LOOP('',(#41002,#41003,#41004,#41005));
#7710=EDGE_LOOP('',(#41006,#41007,#41008,#41009));
#7711=EDGE_LOOP('',(#41010,#41011,#41012,#41013));
#7712=EDGE_LOOP('',(#41014,#41015,#41016,#41017));
#7713=EDGE_LOOP('',(#41018,#41019,#41020,#41021));
#7714=EDGE_LOOP('',(#41022,#41023,#41024,#41025));
#7715=EDGE_LOOP('',(#41026,#41027,#41028,#41029,#41030,#41031,#41032,#41033,
#41034));
#7716=EDGE_LOOP('',(#41035,#41036,#41037,#41038,#41039,#41040,#41041,#41042));
#7717=EDGE_LOOP('',(#41043,#41044,#41045,#41046));
#7718=EDGE_LOOP('',(#41047,#41048,#41049,#41050));
#7719=EDGE_LOOP('',(#41051,#41052,#41053,#41054));
#7720=EDGE_LOOP('',(#41055,#41056,#41057,#41058));
#7721=EDGE_LOOP('',(#41059,#41060,#41061,#41062));
#7722=EDGE_LOOP('',(#41063,#41064,#41065,#41066));
#7723=EDGE_LOOP('',(#41067,#41068,#41069,#41070));
#7724=EDGE_LOOP('',(#41071,#41072,#41073,#41074));
#7725=EDGE_LOOP('',(#41075,#41076,#41077,#41078));
#7726=EDGE_LOOP('',(#41079,#41080,#41081,#41082));
#7727=EDGE_LOOP('',(#41083,#41084,#41085,#41086));
#7728=EDGE_LOOP('',(#41087,#41088,#41089,#41090));
#7729=EDGE_LOOP('',(#41091,#41092,#41093,#41094));
#7730=EDGE_LOOP('',(#41095,#41096,#41097,#41098));
#7731=EDGE_LOOP('',(#41099,#41100,#41101,#41102));
#7732=EDGE_LOOP('',(#41103,#41104,#41105,#41106));
#7733=EDGE_LOOP('',(#41107,#41108,#41109,#41110));
#7734=EDGE_LOOP('',(#41111,#41112,#41113,#41114));
#7735=EDGE_LOOP('',(#41115,#41116,#41117,#41118));
#7736=EDGE_LOOP('',(#41119,#41120,#41121,#41122));
#7737=EDGE_LOOP('',(#41123,#41124,#41125,#41126,#41127,#41128,#41129,#41130,
#41131,#41132,#41133,#41134));
#7738=EDGE_LOOP('',(#41135,#41136,#41137,#41138,#41139,#41140,#41141,#41142));
#7739=EDGE_LOOP('',(#41143,#41144,#41145,#41146,#41147,#41148,#41149,#41150));
#7740=EDGE_LOOP('',(#41151,#41152,#41153,#41154));
#7741=EDGE_LOOP('',(#41155,#41156,#41157,#41158));
#7742=EDGE_LOOP('',(#41159,#41160,#41161,#41162));
#7743=EDGE_LOOP('',(#41163,#41164,#41165,#41166));
#7744=EDGE_LOOP('',(#41167,#41168,#41169,#41170));
#7745=EDGE_LOOP('',(#41171,#41172,#41173,#41174));
#7746=EDGE_LOOP('',(#41175,#41176,#41177,#41178));
#7747=EDGE_LOOP('',(#41179,#41180,#41181,#41182));
#7748=EDGE_LOOP('',(#41183,#41184,#41185,#41186));
#7749=EDGE_LOOP('',(#41187,#41188,#41189,#41190));
#7750=EDGE_LOOP('',(#41191,#41192,#41193,#41194));
#7751=EDGE_LOOP('',(#41195,#41196,#41197,#41198));
#7752=EDGE_LOOP('',(#41199,#41200,#41201,#41202));
#7753=EDGE_LOOP('',(#41203,#41204,#41205,#41206));
#7754=EDGE_LOOP('',(#41207,#41208,#41209,#41210));
#7755=EDGE_LOOP('',(#41211,#41212,#41213,#41214));
#7756=EDGE_LOOP('',(#41215,#41216,#41217,#41218));
#7757=EDGE_LOOP('',(#41219,#41220,#41221,#41222));
#7758=EDGE_LOOP('',(#41223,#41224,#41225,#41226));
#7759=EDGE_LOOP('',(#41227,#41228,#41229,#41230));
#7760=EDGE_LOOP('',(#41231,#41232,#41233,#41234,#41235,#41236,#41237,#41238,
#41239,#41240,#41241,#41242));
#7761=EDGE_LOOP('',(#41243,#41244,#41245,#41246,#41247,#41248,#41249,#41250));
#7762=EDGE_LOOP('',(#41251,#41252,#41253,#41254));
#7763=EDGE_LOOP('',(#41255,#41256,#41257,#41258));
#7764=EDGE_LOOP('',(#41259,#41260,#41261,#41262));
#7765=EDGE_LOOP('',(#41263,#41264,#41265,#41266));
#7766=EDGE_LOOP('',(#41267,#41268,#41269,#41270));
#7767=EDGE_LOOP('',(#41271,#41272,#41273,#41274));
#7768=EDGE_LOOP('',(#41275,#41276,#41277,#41278));
#7769=EDGE_LOOP('',(#41279,#41280,#41281,#41282));
#7770=EDGE_LOOP('',(#41283,#41284,#41285,#41286));
#7771=EDGE_LOOP('',(#41287,#41288,#41289,#41290,#41291,#41292,#41293,#41294,
#41295));
#7772=EDGE_LOOP('',(#41296,#41297,#41298,#41299,#41300,#41301,#41302,#41303));
#7773=EDGE_LOOP('',(#41304,#41305,#41306,#41307));
#7774=EDGE_LOOP('',(#41308,#41309,#41310,#41311));
#7775=EDGE_LOOP('',(#41312,#41313,#41314,#41315));
#7776=EDGE_LOOP('',(#41316,#41317,#41318,#41319));
#7777=EDGE_LOOP('',(#41320,#41321,#41322,#41323));
#7778=EDGE_LOOP('',(#41324,#41325,#41326,#41327));
#7779=EDGE_LOOP('',(#41328,#41329,#41330,#41331));
#7780=EDGE_LOOP('',(#41332,#41333,#41334,#41335));
#7781=EDGE_LOOP('',(#41336,#41337,#41338,#41339));
#7782=EDGE_LOOP('',(#41340,#41341,#41342,#41343));
#7783=EDGE_LOOP('',(#41344,#41345,#41346,#41347));
#7784=EDGE_LOOP('',(#41348,#41349,#41350,#41351));
#7785=EDGE_LOOP('',(#41352,#41353,#41354,#41355));
#7786=EDGE_LOOP('',(#41356,#41357,#41358,#41359));
#7787=EDGE_LOOP('',(#41360,#41361,#41362,#41363));
#7788=EDGE_LOOP('',(#41364,#41365,#41366,#41367));
#7789=EDGE_LOOP('',(#41368,#41369,#41370,#41371));
#7790=EDGE_LOOP('',(#41372,#41373,#41374,#41375));
#7791=EDGE_LOOP('',(#41376,#41377,#41378,#41379));
#7792=EDGE_LOOP('',(#41380,#41381,#41382,#41383));
#7793=EDGE_LOOP('',(#41384,#41385,#41386,#41387,#41388,#41389,#41390,#41391,
#41392,#41393,#41394,#41395));
#7794=EDGE_LOOP('',(#41396,#41397,#41398,#41399,#41400,#41401,#41402,#41403));
#7795=EDGE_LOOP('',(#41404,#41405,#41406,#41407));
#7796=EDGE_LOOP('',(#41408,#41409,#41410,#41411));
#7797=EDGE_LOOP('',(#41412,#41413,#41414,#41415));
#7798=EDGE_LOOP('',(#41416,#41417,#41418,#41419));
#7799=EDGE_LOOP('',(#41420,#41421,#41422,#41423));
#7800=EDGE_LOOP('',(#41424,#41425,#41426,#41427));
#7801=EDGE_LOOP('',(#41428,#41429,#41430,#41431));
#7802=EDGE_LOOP('',(#41432,#41433,#41434,#41435));
#7803=EDGE_LOOP('',(#41436,#41437,#41438,#41439));
#7804=EDGE_LOOP('',(#41440,#41441,#41442,#41443));
#7805=EDGE_LOOP('',(#41444,#41445,#41446,#41447));
#7806=EDGE_LOOP('',(#41448,#41449,#41450,#41451));
#7807=EDGE_LOOP('',(#41452,#41453,#41454,#41455));
#7808=EDGE_LOOP('',(#41456,#41457,#41458,#41459));
#7809=EDGE_LOOP('',(#41460,#41461,#41462,#41463));
#7810=EDGE_LOOP('',(#41464,#41465,#41466,#41467));
#7811=EDGE_LOOP('',(#41468,#41469,#41470,#41471));
#7812=EDGE_LOOP('',(#41472,#41473,#41474,#41475));
#7813=EDGE_LOOP('',(#41476,#41477,#41478,#41479));
#7814=EDGE_LOOP('',(#41480,#41481,#41482,#41483));
#7815=EDGE_LOOP('',(#41484,#41485,#41486,#41487));
#7816=EDGE_LOOP('',(#41488,#41489,#41490,#41491));
#7817=EDGE_LOOP('',(#41492,#41493,#41494,#41495,#41496,#41497,#41498,#41499,
#41500,#41501,#41502,#41503,#41504,#41505,#41506,#41507,#41508,#41509,#41510,
#41511,#41512,#41513));
#7818=EDGE_LOOP('',(#41514,#41515,#41516,#41517,#41518,#41519,#41520,#41521));
#7819=EDGE_LOOP('',(#41522,#41523,#41524,#41525));
#7820=EDGE_LOOP('',(#41526,#41527,#41528,#41529));
#7821=EDGE_LOOP('',(#41530,#41531,#41532,#41533));
#7822=EDGE_LOOP('',(#41534,#41535,#41536,#41537));
#7823=EDGE_LOOP('',(#41538,#41539,#41540,#41541));
#7824=EDGE_LOOP('',(#41542,#41543,#41544,#41545));
#7825=EDGE_LOOP('',(#41546,#41547,#41548,#41549));
#7826=EDGE_LOOP('',(#41550,#41551,#41552,#41553));
#7827=EDGE_LOOP('',(#41554,#41555,#41556,#41557));
#7828=EDGE_LOOP('',(#41558,#41559,#41560,#41561));
#7829=EDGE_LOOP('',(#41562,#41563,#41564,#41565));
#7830=EDGE_LOOP('',(#41566,#41567,#41568,#41569));
#7831=EDGE_LOOP('',(#41570,#41571,#41572,#41573));
#7832=EDGE_LOOP('',(#41574,#41575,#41576,#41577));
#7833=EDGE_LOOP('',(#41578,#41579,#41580,#41581));
#7834=EDGE_LOOP('',(#41582,#41583,#41584,#41585));
#7835=EDGE_LOOP('',(#41586,#41587,#41588,#41589));
#7836=EDGE_LOOP('',(#41590,#41591,#41592,#41593));
#7837=EDGE_LOOP('',(#41594,#41595,#41596,#41597));
#7838=EDGE_LOOP('',(#41598,#41599,#41600,#41601));
#7839=EDGE_LOOP('',(#41602,#41603,#41604,#41605,#41606,#41607,#41608,#41609,
#41610,#41611,#41612,#41613));
#7840=EDGE_LOOP('',(#41614,#41615,#41616,#41617,#41618,#41619,#41620,#41621));
#7841=EDGE_LOOP('',(#41622,#41623,#41624,#41625));
#7842=EDGE_LOOP('',(#41626,#41627,#41628,#41629));
#7843=EDGE_LOOP('',(#41630,#41631,#41632,#41633));
#7844=EDGE_LOOP('',(#41634,#41635,#41636,#41637));
#7845=EDGE_LOOP('',(#41638,#41639,#41640,#41641));
#7846=EDGE_LOOP('',(#41642,#41643,#41644,#41645));
#7847=EDGE_LOOP('',(#41646,#41647,#41648,#41649));
#7848=EDGE_LOOP('',(#41650,#41651,#41652,#41653));
#7849=EDGE_LOOP('',(#41654,#41655,#41656,#41657));
#7850=EDGE_LOOP('',(#41658,#41659,#41660,#41661));
#7851=EDGE_LOOP('',(#41662,#41663,#41664,#41665));
#7852=EDGE_LOOP('',(#41666,#41667,#41668,#41669));
#7853=EDGE_LOOP('',(#41670,#41671,#41672,#41673));
#7854=EDGE_LOOP('',(#41674,#41675,#41676,#41677));
#7855=EDGE_LOOP('',(#41678,#41679,#41680,#41681));
#7856=EDGE_LOOP('',(#41682,#41683,#41684,#41685));
#7857=EDGE_LOOP('',(#41686,#41687,#41688,#41689));
#7858=EDGE_LOOP('',(#41690,#41691,#41692,#41693));
#7859=EDGE_LOOP('',(#41694,#41695,#41696,#41697));
#7860=EDGE_LOOP('',(#41698,#41699,#41700,#41701));
#7861=EDGE_LOOP('',(#41702,#41703,#41704,#41705));
#7862=EDGE_LOOP('',(#41706,#41707,#41708,#41709));
#7863=EDGE_LOOP('',(#41710,#41711,#41712,#41713));
#7864=EDGE_LOOP('',(#41714,#41715,#41716,#41717));
#7865=EDGE_LOOP('',(#41718,#41719,#41720,#41721));
#7866=EDGE_LOOP('',(#41722,#41723,#41724,#41725));
#7867=EDGE_LOOP('',(#41726,#41727,#41728,#41729));
#7868=EDGE_LOOP('',(#41730,#41731,#41732,#41733));
#7869=EDGE_LOOP('',(#41734,#41735,#41736,#41737));
#7870=EDGE_LOOP('',(#41738,#41739,#41740,#41741));
#7871=EDGE_LOOP('',(#41742,#41743,#41744,#41745,#41746,#41747,#41748,#41749,
#41750,#41751,#41752,#41753,#41754,#41755,#41756,#41757,#41758,#41759,#41760,
#41761,#41762,#41763,#41764,#41765,#41766,#41767,#41768,#41769,#41770,#41771));
#7872=EDGE_LOOP('',(#41772,#41773,#41774,#41775,#41776,#41777,#41778,#41779));
#7873=EDGE_LOOP('',(#41780,#41781,#41782,#41783));
#7874=EDGE_LOOP('',(#41784,#41785,#41786,#41787));
#7875=EDGE_LOOP('',(#41788,#41789,#41790,#41791));
#7876=EDGE_LOOP('',(#41792,#41793,#41794,#41795));
#7877=EDGE_LOOP('',(#41796,#41797,#41798,#41799));
#7878=EDGE_LOOP('',(#41800,#41801,#41802,#41803));
#7879=EDGE_LOOP('',(#41804,#41805,#41806,#41807));
#7880=EDGE_LOOP('',(#41808,#41809,#41810,#41811));
#7881=EDGE_LOOP('',(#41812,#41813,#41814,#41815));
#7882=EDGE_LOOP('',(#41816,#41817,#41818,#41819));
#7883=EDGE_LOOP('',(#41820,#41821,#41822,#41823));
#7884=EDGE_LOOP('',(#41824,#41825,#41826,#41827));
#7885=EDGE_LOOP('',(#41828,#41829,#41830,#41831));
#7886=EDGE_LOOP('',(#41832,#41833,#41834,#41835));
#7887=EDGE_LOOP('',(#41836,#41837,#41838,#41839));
#7888=EDGE_LOOP('',(#41840,#41841,#41842,#41843));
#7889=EDGE_LOOP('',(#41844,#41845,#41846,#41847));
#7890=EDGE_LOOP('',(#41848,#41849,#41850,#41851));
#7891=EDGE_LOOP('',(#41852,#41853,#41854,#41855));
#7892=EDGE_LOOP('',(#41856,#41857,#41858,#41859));
#7893=EDGE_LOOP('',(#41860,#41861,#41862,#41863,#41864,#41865,#41866,#41867,
#41868,#41869,#41870,#41871));
#7894=EDGE_LOOP('',(#41872,#41873,#41874,#41875,#41876,#41877,#41878,#41879));
#7895=EDGE_LOOP('',(#41880,#41881,#41882,#41883));
#7896=EDGE_LOOP('',(#41884,#41885,#41886,#41887));
#7897=EDGE_LOOP('',(#41888,#41889,#41890,#41891));
#7898=EDGE_LOOP('',(#41892,#41893,#41894,#41895));
#7899=EDGE_LOOP('',(#41896,#41897,#41898,#41899));
#7900=EDGE_LOOP('',(#41900,#41901,#41902,#41903));
#7901=EDGE_LOOP('',(#41904,#41905,#41906,#41907));
#7902=EDGE_LOOP('',(#41908,#41909,#41910,#41911));
#7903=EDGE_LOOP('',(#41912,#41913,#41914,#41915));
#7904=EDGE_LOOP('',(#41916,#41917,#41918,#41919));
#7905=EDGE_LOOP('',(#41920,#41921,#41922,#41923));
#7906=EDGE_LOOP('',(#41924,#41925,#41926,#41927));
#7907=EDGE_LOOP('',(#41928,#41929,#41930,#41931));
#7908=EDGE_LOOP('',(#41932,#41933,#41934,#41935));
#7909=EDGE_LOOP('',(#41936,#41937,#41938,#41939,#41940,#41941,#41942,#41943,
#41944,#41945,#41946));
#7910=EDGE_LOOP('',(#41947,#41948,#41949));
#7911=EDGE_LOOP('',(#41950,#41951,#41952));
#7912=EDGE_LOOP('',(#41953,#41954,#41955,#41956,#41957,#41958,#41959,#41960));
#7913=EDGE_LOOP('',(#41961,#41962,#41963,#41964));
#7914=EDGE_LOOP('',(#41965,#41966,#41967,#41968));
#7915=EDGE_LOOP('',(#41969,#41970,#41971,#41972));
#7916=EDGE_LOOP('',(#41973,#41974,#41975,#41976));
#7917=EDGE_LOOP('',(#41977,#41978,#41979,#41980));
#7918=EDGE_LOOP('',(#41981,#41982,#41983,#41984));
#7919=EDGE_LOOP('',(#41985,#41986,#41987,#41988));
#7920=EDGE_LOOP('',(#41989,#41990,#41991,#41992));
#7921=EDGE_LOOP('',(#41993,#41994,#41995,#41996));
#7922=EDGE_LOOP('',(#41997,#41998,#41999,#42000));
#7923=EDGE_LOOP('',(#42001,#42002,#42003,#42004));
#7924=EDGE_LOOP('',(#42005,#42006,#42007,#42008));
#7925=EDGE_LOOP('',(#42009,#42010,#42011,#42012));
#7926=EDGE_LOOP('',(#42013,#42014,#42015,#42016));
#7927=EDGE_LOOP('',(#42017,#42018,#42019,#42020));
#7928=EDGE_LOOP('',(#42021,#42022,#42023,#42024));
#7929=EDGE_LOOP('',(#42025,#42026,#42027,#42028));
#7930=EDGE_LOOP('',(#42029,#42030,#42031,#42032));
#7931=EDGE_LOOP('',(#42033,#42034,#42035,#42036));
#7932=EDGE_LOOP('',(#42037,#42038,#42039,#42040));
#7933=EDGE_LOOP('',(#42041,#42042,#42043,#42044,#42045,#42046,#42047,#42048,
#42049,#42050,#42051,#42052));
#7934=EDGE_LOOP('',(#42053,#42054,#42055,#42056,#42057,#42058,#42059,#42060));
#7935=EDGE_LOOP('',(#42061,#42062,#42063,#42064));
#7936=EDGE_LOOP('',(#42065,#42066,#42067,#42068));
#7937=EDGE_LOOP('',(#42069,#42070,#42071,#42072));
#7938=EDGE_LOOP('',(#42073,#42074,#42075,#42076));
#7939=EDGE_LOOP('',(#42077,#42078,#42079,#42080));
#7940=EDGE_LOOP('',(#42081,#42082,#42083,#42084));
#7941=EDGE_LOOP('',(#42085,#42086,#42087,#42088));
#7942=EDGE_LOOP('',(#42089,#42090,#42091,#42092));
#7943=EDGE_LOOP('',(#42093,#42094,#42095,#42096));
#7944=EDGE_LOOP('',(#42097,#42098,#42099,#42100));
#7945=EDGE_LOOP('',(#42101,#42102,#42103,#42104));
#7946=EDGE_LOOP('',(#42105,#42106,#42107,#42108));
#7947=EDGE_LOOP('',(#42109,#42110,#42111,#42112));
#7948=EDGE_LOOP('',(#42113,#42114,#42115,#42116));
#7949=EDGE_LOOP('',(#42117,#42118,#42119,#42120));
#7950=EDGE_LOOP('',(#42121,#42122,#42123,#42124));
#7951=EDGE_LOOP('',(#42125,#42126,#42127,#42128));
#7952=EDGE_LOOP('',(#42129,#42130,#42131,#42132));
#7953=EDGE_LOOP('',(#42133,#42134,#42135,#42136));
#7954=EDGE_LOOP('',(#42137,#42138,#42139,#42140));
#7955=EDGE_LOOP('',(#42141,#42142,#42143,#42144));
#7956=EDGE_LOOP('',(#42145,#42146,#42147,#42148));
#7957=EDGE_LOOP('',(#42149,#42150,#42151,#42152,#42153,#42154,#42155,#42156,
#42157,#42158,#42159,#42160,#42161,#42162,#42163,#42164,#42165,#42166,#42167,
#42168,#42169,#42170));
#7958=EDGE_LOOP('',(#42171,#42172,#42173,#42174,#42175,#42176,#42177,#42178));
#7959=EDGE_LOOP('',(#42179,#42180,#42181,#42182));
#7960=EDGE_LOOP('',(#42183,#42184,#42185,#42186));
#7961=EDGE_LOOP('',(#42187,#42188,#42189,#42190));
#7962=EDGE_LOOP('',(#42191,#42192,#42193,#42194));
#7963=EDGE_LOOP('',(#42195,#42196,#42197,#42198));
#7964=EDGE_LOOP('',(#42199,#42200,#42201,#42202));
#7965=EDGE_LOOP('',(#42203,#42204,#42205,#42206));
#7966=EDGE_LOOP('',(#42207,#42208,#42209,#42210));
#7967=EDGE_LOOP('',(#42211,#42212,#42213,#42214));
#7968=EDGE_LOOP('',(#42215,#42216,#42217,#42218));
#7969=EDGE_LOOP('',(#42219,#42220,#42221,#42222));
#7970=EDGE_LOOP('',(#42223,#42224,#42225,#42226));
#7971=EDGE_LOOP('',(#42227,#42228,#42229,#42230));
#7972=EDGE_LOOP('',(#42231,#42232,#42233,#42234));
#7973=EDGE_LOOP('',(#42235,#42236,#42237,#42238));
#7974=EDGE_LOOP('',(#42239,#42240,#42241,#42242));
#7975=EDGE_LOOP('',(#42243,#42244,#42245,#42246));
#7976=EDGE_LOOP('',(#42247,#42248,#42249,#42250));
#7977=EDGE_LOOP('',(#42251,#42252,#42253,#42254));
#7978=EDGE_LOOP('',(#42255,#42256,#42257,#42258));
#7979=EDGE_LOOP('',(#42259,#42260,#42261,#42262,#42263,#42264,#42265,#42266,
#42267,#42268,#42269,#42270));
#7980=EDGE_LOOP('',(#42271,#42272,#42273,#42274,#42275,#42276,#42277,#42278));
#7981=EDGE_LOOP('',(#42279,#42280,#42281,#42282));
#7982=EDGE_LOOP('',(#42283,#42284,#42285,#42286));
#7983=EDGE_LOOP('',(#42287,#42288,#42289,#42290));
#7984=EDGE_LOOP('',(#42291,#42292,#42293,#42294));
#7985=EDGE_LOOP('',(#42295,#42296,#42297,#42298));
#7986=EDGE_LOOP('',(#42299,#42300,#42301,#42302));
#7987=EDGE_LOOP('',(#42303,#42304,#42305,#42306));
#7988=EDGE_LOOP('',(#42307,#42308,#42309,#42310));
#7989=EDGE_LOOP('',(#42311,#42312,#42313,#42314));
#7990=EDGE_LOOP('',(#42315,#42316,#42317,#42318));
#7991=EDGE_LOOP('',(#42319,#42320,#42321,#42322));
#7992=EDGE_LOOP('',(#42323,#42324,#42325,#42326));
#7993=EDGE_LOOP('',(#42327,#42328,#42329,#42330));
#7994=EDGE_LOOP('',(#42331,#42332,#42333,#42334));
#7995=EDGE_LOOP('',(#42335,#42336,#42337,#42338));
#7996=EDGE_LOOP('',(#42339,#42340,#42341,#42342));
#7997=EDGE_LOOP('',(#42343,#42344,#42345,#42346));
#7998=EDGE_LOOP('',(#42347,#42348,#42349,#42350));
#7999=EDGE_LOOP('',(#42351,#42352,#42353,#42354));
#8000=EDGE_LOOP('',(#42355,#42356,#42357,#42358));
#8001=EDGE_LOOP('',(#42359,#42360,#42361,#42362));
#8002=EDGE_LOOP('',(#42363,#42364,#42365,#42366));
#8003=EDGE_LOOP('',(#42367,#42368,#42369,#42370));
#8004=EDGE_LOOP('',(#42371,#42372,#42373,#42374));
#8005=EDGE_LOOP('',(#42375,#42376,#42377,#42378));
#8006=EDGE_LOOP('',(#42379,#42380,#42381,#42382));
#8007=EDGE_LOOP('',(#42383,#42384,#42385,#42386));
#8008=EDGE_LOOP('',(#42387,#42388,#42389,#42390));
#8009=EDGE_LOOP('',(#42391,#42392,#42393,#42394,#42395,#42396,#42397,#42398,
#42399,#42400,#42401,#42402,#42403,#42404,#42405,#42406,#42407,#42408,#42409));
#8010=EDGE_LOOP('',(#42410,#42411,#42412,#42413,#42414,#42415,#42416,#42417,
#42418));
#8011=EDGE_LOOP('',(#42419,#42420,#42421,#42422,#42423,#42424,#42425,#42426,
#42427));
#8012=EDGE_LOOP('',(#42428,#42429,#42430,#42431,#42432,#42433,#42434,#42435));
#8013=EDGE_LOOP('',(#42436,#42437,#42438,#42439));
#8014=EDGE_LOOP('',(#42440,#42441,#42442,#42443));
#8015=EDGE_LOOP('',(#42444,#42445,#42446,#42447));
#8016=EDGE_LOOP('',(#42448,#42449,#42450,#42451));
#8017=EDGE_LOOP('',(#42452,#42453,#42454,#42455));
#8018=EDGE_LOOP('',(#42456,#42457,#42458,#42459));
#8019=EDGE_LOOP('',(#42460,#42461,#42462,#42463));
#8020=EDGE_LOOP('',(#42464,#42465,#42466,#42467));
#8021=EDGE_LOOP('',(#42468,#42469,#42470,#42471));
#8022=EDGE_LOOP('',(#42472,#42473,#42474,#42475));
#8023=EDGE_LOOP('',(#42476,#42477,#42478,#42479));
#8024=EDGE_LOOP('',(#42480,#42481,#42482,#42483));
#8025=EDGE_LOOP('',(#42484,#42485,#42486,#42487));
#8026=EDGE_LOOP('',(#42488,#42489,#42490,#42491));
#8027=EDGE_LOOP('',(#42492,#42493,#42494,#42495));
#8028=EDGE_LOOP('',(#42496,#42497,#42498,#42499));
#8029=EDGE_LOOP('',(#42500,#42501,#42502,#42503));
#8030=EDGE_LOOP('',(#42504,#42505,#42506,#42507));
#8031=EDGE_LOOP('',(#42508,#42509,#42510,#42511));
#8032=EDGE_LOOP('',(#42512,#42513,#42514,#42515));
#8033=EDGE_LOOP('',(#42516,#42517,#42518,#42519,#42520,#42521,#42522,#42523,
#42524,#42525,#42526,#42527));
#8034=EDGE_LOOP('',(#42528,#42529,#42530,#42531,#42532,#42533,#42534,#42535));
#8035=EDGE_LOOP('',(#42536,#42537,#42538,#42539));
#8036=EDGE_LOOP('',(#42540,#42541,#42542,#42543));
#8037=EDGE_LOOP('',(#42544,#42545,#42546,#42547));
#8038=EDGE_LOOP('',(#42548,#42549,#42550,#42551));
#8039=EDGE_LOOP('',(#42552,#42553,#42554,#42555));
#8040=EDGE_LOOP('',(#42556,#42557,#42558,#42559));
#8041=EDGE_LOOP('',(#42560,#42561,#42562,#42563));
#8042=EDGE_LOOP('',(#42564,#42565,#42566,#42567));
#8043=EDGE_LOOP('',(#42568,#42569,#42570,#42571));
#8044=EDGE_LOOP('',(#42572,#42573,#42574,#42575));
#8045=EDGE_LOOP('',(#42576,#42577,#42578,#42579));
#8046=EDGE_LOOP('',(#42580,#42581,#42582,#42583,#42584,#42585,#42586,#42587,
#42588,#42589,#42590));
#8047=EDGE_LOOP('',(#42591,#42592,#42593,#42594,#42595,#42596,#42597,#42598));
#8048=EDGE_LOOP('',(#42599,#42600,#42601,#42602));
#8049=EDGE_LOOP('',(#42603,#42604,#42605,#42606));
#8050=EDGE_LOOP('',(#42607,#42608,#42609,#42610));
#8051=EDGE_LOOP('',(#42611,#42612,#42613,#42614));
#8052=EDGE_LOOP('',(#42615,#42616,#42617,#42618));
#8053=EDGE_LOOP('',(#42619,#42620,#42621,#42622));
#8054=EDGE_LOOP('',(#42623,#42624,#42625,#42626));
#8055=EDGE_LOOP('',(#42627,#42628,#42629,#42630));
#8056=EDGE_LOOP('',(#42631,#42632,#42633,#42634));
#8057=EDGE_LOOP('',(#42635,#42636,#42637,#42638));
#8058=EDGE_LOOP('',(#42639,#42640,#42641,#42642));
#8059=EDGE_LOOP('',(#42643,#42644,#42645,#42646));
#8060=EDGE_LOOP('',(#42647,#42648,#42649,#42650));
#8061=EDGE_LOOP('',(#42651,#42652,#42653,#42654));
#8062=EDGE_LOOP('',(#42655,#42656,#42657,#42658));
#8063=EDGE_LOOP('',(#42659,#42660,#42661,#42662));
#8064=EDGE_LOOP('',(#42663,#42664,#42665,#42666));
#8065=EDGE_LOOP('',(#42667,#42668,#42669,#42670));
#8066=EDGE_LOOP('',(#42671,#42672,#42673,#42674));
#8067=EDGE_LOOP('',(#42675,#42676,#42677,#42678));
#8068=EDGE_LOOP('',(#42679,#42680,#42681,#42682,#42683,#42684,#42685,#42686,
#42687,#42688,#42689,#42690));
#8069=EDGE_LOOP('',(#42691,#42692,#42693,#42694,#42695,#42696,#42697,#42698));
#8070=EDGE_LOOP('',(#42699,#42700,#42701,#42702));
#8071=EDGE_LOOP('',(#42703,#42704,#42705,#42706));
#8072=EDGE_LOOP('',(#42707,#42708,#42709,#42710));
#8073=EDGE_LOOP('',(#42711,#42712,#42713,#42714));
#8074=EDGE_LOOP('',(#42715,#42716,#42717,#42718));
#8075=EDGE_LOOP('',(#42719,#42720,#42721,#42722));
#8076=EDGE_LOOP('',(#42723,#42724,#42725,#42726));
#8077=EDGE_LOOP('',(#42727,#42728,#42729,#42730));
#8078=EDGE_LOOP('',(#42731,#42732,#42733,#42734));
#8079=EDGE_LOOP('',(#42735,#42736,#42737,#42738));
#8080=EDGE_LOOP('',(#42739,#42740,#42741,#42742));
#8081=EDGE_LOOP('',(#42743,#42744,#42745,#42746));
#8082=EDGE_LOOP('',(#42747,#42748,#42749,#42750));
#8083=EDGE_LOOP('',(#42751,#42752,#42753,#42754));
#8084=EDGE_LOOP('',(#42755,#42756,#42757,#42758));
#8085=EDGE_LOOP('',(#42759,#42760,#42761,#42762));
#8086=EDGE_LOOP('',(#42763,#42764,#42765,#42766));
#8087=EDGE_LOOP('',(#42767,#42768,#42769,#42770));
#8088=EDGE_LOOP('',(#42771,#42772,#42773,#42774));
#8089=EDGE_LOOP('',(#42775,#42776,#42777,#42778));
#8090=EDGE_LOOP('',(#42779,#42780,#42781,#42782));
#8091=EDGE_LOOP('',(#42783,#42784,#42785,#42786));
#8092=EDGE_LOOP('',(#42787,#42788,#42789,#42790));
#8093=EDGE_LOOP('',(#42791,#42792,#42793,#42794));
#8094=EDGE_LOOP('',(#42795,#42796,#42797,#42798));
#8095=EDGE_LOOP('',(#42799,#42800,#42801,#42802));
#8096=EDGE_LOOP('',(#42803,#42804,#42805,#42806));
#8097=EDGE_LOOP('',(#42807,#42808,#42809,#42810));
#8098=EDGE_LOOP('',(#42811,#42812,#42813,#42814));
#8099=EDGE_LOOP('',(#42815,#42816,#42817,#42818));
#8100=EDGE_LOOP('',(#42819,#42820,#42821,#42822));
#8101=EDGE_LOOP('',(#42823,#42824,#42825,#42826));
#8102=EDGE_LOOP('',(#42827,#42828,#42829,#42830));
#8103=EDGE_LOOP('',(#42831,#42832,#42833,#42834,#42835,#42836,#42837,#42838,
#42839,#42840,#42841,#42842,#42843,#42844,#42845,#42846));
#8104=EDGE_LOOP('',(#42847,#42848,#42849,#42850,#42851,#42852,#42853,#42854,
#42855));
#8105=EDGE_LOOP('',(#42856,#42857,#42858,#42859,#42860,#42861,#42862,#42863));
#8106=EDGE_LOOP('',(#42864,#42865,#42866,#42867,#42868,#42869,#42870,#42871,
#42872));
#8107=EDGE_LOOP('',(#42873,#42874,#42875,#42876,#42877,#42878,#42879,#42880));
#8108=EDGE_LOOP('',(#42881,#42882,#42883,#42884,#42885,#42886,#42887,#42888));
#8109=EDGE_LOOP('',(#42889,#42890,#42891,#42892));
#8110=EDGE_LOOP('',(#42893,#42894,#42895,#42896));
#8111=EDGE_LOOP('',(#42897,#42898,#42899,#42900));
#8112=EDGE_LOOP('',(#42901,#42902,#42903,#42904));
#8113=EDGE_LOOP('',(#42905,#42906,#42907,#42908));
#8114=EDGE_LOOP('',(#42909,#42910,#42911,#42912));
#8115=EDGE_LOOP('',(#42913,#42914,#42915,#42916));
#8116=EDGE_LOOP('',(#42917,#42918,#42919,#42920));
#8117=EDGE_LOOP('',(#42921,#42922,#42923,#42924));
#8118=EDGE_LOOP('',(#42925,#42926,#42927,#42928));
#8119=EDGE_LOOP('',(#42929,#42930,#42931,#42932));
#8120=EDGE_LOOP('',(#42933,#42934,#42935,#42936));
#8121=EDGE_LOOP('',(#42937,#42938,#42939,#42940));
#8122=EDGE_LOOP('',(#42941,#42942,#42943,#42944));
#8123=EDGE_LOOP('',(#42945,#42946,#42947,#42948));
#8124=EDGE_LOOP('',(#42949,#42950,#42951,#42952));
#8125=EDGE_LOOP('',(#42953,#42954,#42955,#42956));
#8126=EDGE_LOOP('',(#42957,#42958,#42959,#42960));
#8127=EDGE_LOOP('',(#42961,#42962,#42963,#42964));
#8128=EDGE_LOOP('',(#42965,#42966,#42967,#42968));
#8129=EDGE_LOOP('',(#42969,#42970,#42971,#42972,#42973,#42974,#42975,#42976,
#42977,#42978,#42979,#42980));
#8130=EDGE_LOOP('',(#42981,#42982,#42983,#42984,#42985,#42986,#42987,#42988));
#8131=EDGE_LOOP('',(#42989,#42990,#42991,#42992));
#8132=EDGE_LOOP('',(#42993,#42994,#42995,#42996));
#8133=EDGE_LOOP('',(#42997,#42998,#42999,#43000));
#8134=EDGE_LOOP('',(#43001,#43002,#43003,#43004));
#8135=EDGE_LOOP('',(#43005,#43006,#43007,#43008));
#8136=EDGE_LOOP('',(#43009,#43010,#43011,#43012));
#8137=EDGE_LOOP('',(#43013,#43014,#43015,#43016));
#8138=EDGE_LOOP('',(#43017,#43018,#43019,#43020));
#8139=EDGE_LOOP('',(#43021,#43022,#43023,#43024));
#8140=EDGE_LOOP('',(#43025,#43026,#43027,#43028));
#8141=EDGE_LOOP('',(#43029,#43030,#43031,#43032));
#8142=EDGE_LOOP('',(#43033,#43034,#43035,#43036));
#8143=EDGE_LOOP('',(#43037,#43038,#43039,#43040));
#8144=EDGE_LOOP('',(#43041,#43042,#43043,#43044));
#8145=EDGE_LOOP('',(#43045,#43046,#43047,#43048));
#8146=EDGE_LOOP('',(#43049,#43050,#43051,#43052));
#8147=EDGE_LOOP('',(#43053,#43054,#43055,#43056));
#8148=EDGE_LOOP('',(#43057,#43058,#43059,#43060));
#8149=EDGE_LOOP('',(#43061,#43062,#43063,#43064));
#8150=EDGE_LOOP('',(#43065,#43066,#43067,#43068));
#8151=EDGE_LOOP('',(#43069,#43070,#43071,#43072));
#8152=EDGE_LOOP('',(#43073,#43074,#43075,#43076));
#8153=EDGE_LOOP('',(#43077,#43078,#43079,#43080));
#8154=EDGE_LOOP('',(#43081,#43082,#43083,#43084));
#8155=EDGE_LOOP('',(#43085,#43086,#43087,#43088));
#8156=EDGE_LOOP('',(#43089,#43090,#43091,#43092));
#8157=EDGE_LOOP('',(#43093,#43094,#43095,#43096));
#8158=EDGE_LOOP('',(#43097,#43098,#43099,#43100));
#8159=EDGE_LOOP('',(#43101,#43102,#43103,#43104));
#8160=EDGE_LOOP('',(#43105,#43106,#43107,#43108));
#8161=EDGE_LOOP('',(#43109,#43110,#43111,#43112,#43113,#43114,#43115,#43116,
#43117,#43118,#43119,#43120,#43121,#43122,#43123,#43124,#43125,#43126,#43127,
#43128,#43129,#43130));
#8162=EDGE_LOOP('',(#43131,#43132,#43133,#43134,#43135,#43136,#43137,#43138));
#8163=EDGE_LOOP('',(#43139,#43140,#43141,#43142,#43143,#43144,#43145,#43146));
#8164=EDGE_LOOP('',(#43147,#43148,#43149,#43150,#43151,#43152,#43153,#43154));
#8165=EDGE_LOOP('',(#43155,#43156,#43157,#43158));
#8166=EDGE_LOOP('',(#43159,#43160,#43161,#43162));
#8167=EDGE_LOOP('',(#43163,#43164,#43165,#43166));
#8168=EDGE_LOOP('',(#43167,#43168,#43169,#43170));
#8169=EDGE_LOOP('',(#43171,#43172,#43173,#43174));
#8170=EDGE_LOOP('',(#43175,#43176,#43177,#43178));
#8171=EDGE_LOOP('',(#43179,#43180,#43181,#43182));
#8172=EDGE_LOOP('',(#43183,#43184,#43185,#43186));
#8173=EDGE_LOOP('',(#43187,#43188,#43189,#43190));
#8174=EDGE_LOOP('',(#43191,#43192,#43193,#43194));
#8175=EDGE_LOOP('',(#43195,#43196,#43197,#43198));
#8176=EDGE_LOOP('',(#43199,#43200,#43201,#43202));
#8177=EDGE_LOOP('',(#43203,#43204,#43205,#43206));
#8178=EDGE_LOOP('',(#43207,#43208,#43209,#43210));
#8179=EDGE_LOOP('',(#43211,#43212,#43213,#43214));
#8180=EDGE_LOOP('',(#43215,#43216,#43217,#43218));
#8181=EDGE_LOOP('',(#43219,#43220,#43221,#43222));
#8182=EDGE_LOOP('',(#43223,#43224,#43225,#43226));
#8183=EDGE_LOOP('',(#43227,#43228,#43229,#43230));
#8184=EDGE_LOOP('',(#43231,#43232,#43233,#43234));
#8185=EDGE_LOOP('',(#43235,#43236,#43237,#43238));
#8186=EDGE_LOOP('',(#43239,#43240,#43241,#43242));
#8187=EDGE_LOOP('',(#43243,#43244,#43245,#43246));
#8188=EDGE_LOOP('',(#43247,#43248,#43249,#43250));
#8189=EDGE_LOOP('',(#43251,#43252,#43253,#43254));
#8190=EDGE_LOOP('',(#43255,#43256,#43257,#43258));
#8191=EDGE_LOOP('',(#43259,#43260,#43261,#43262));
#8192=EDGE_LOOP('',(#43263,#43264,#43265,#43266));
#8193=EDGE_LOOP('',(#43267,#43268,#43269,#43270));
#8194=EDGE_LOOP('',(#43271,#43272,#43273,#43274));
#8195=EDGE_LOOP('',(#43275,#43276,#43277,#43278));
#8196=EDGE_LOOP('',(#43279,#43280,#43281,#43282));
#8197=EDGE_LOOP('',(#43283,#43284,#43285,#43286));
#8198=EDGE_LOOP('',(#43287,#43288,#43289,#43290));
#8199=EDGE_LOOP('',(#43291,#43292,#43293,#43294));
#8200=EDGE_LOOP('',(#43295,#43296,#43297,#43298));
#8201=EDGE_LOOP('',(#43299,#43300,#43301,#43302));
#8202=EDGE_LOOP('',(#43303,#43304,#43305,#43306));
#8203=EDGE_LOOP('',(#43307,#43308,#43309,#43310));
#8204=EDGE_LOOP('',(#43311,#43312,#43313,#43314));
#8205=EDGE_LOOP('',(#43315,#43316,#43317,#43318));
#8206=EDGE_LOOP('',(#43319,#43320,#43321,#43322));
#8207=EDGE_LOOP('',(#43323,#43324,#43325,#43326));
#8208=EDGE_LOOP('',(#43327,#43328,#43329,#43330));
#8209=EDGE_LOOP('',(#43331,#43332,#43333,#43334));
#8210=EDGE_LOOP('',(#43335,#43336,#43337,#43338));
#8211=EDGE_LOOP('',(#43339,#43340,#43341,#43342));
#8212=EDGE_LOOP('',(#43343,#43344,#43345,#43346));
#8213=EDGE_LOOP('',(#43347,#43348,#43349,#43350));
#8214=EDGE_LOOP('',(#43351,#43352,#43353,#43354));
#8215=EDGE_LOOP('',(#43355,#43356,#43357,#43358));
#8216=EDGE_LOOP('',(#43359,#43360,#43361,#43362));
#8217=EDGE_LOOP('',(#43363,#43364,#43365,#43366));
#8218=EDGE_LOOP('',(#43367,#43368,#43369,#43370));
#8219=EDGE_LOOP('',(#43371,#43372,#43373,#43374));
#8220=EDGE_LOOP('',(#43375,#43376,#43377,#43378));
#8221=EDGE_LOOP('',(#43379,#43380,#43381,#43382));
#8222=EDGE_LOOP('',(#43383,#43384,#43385,#43386));
#8223=EDGE_LOOP('',(#43387,#43388,#43389,#43390));
#8224=EDGE_LOOP('',(#43391,#43392,#43393,#43394));
#8225=EDGE_LOOP('',(#43395,#43396,#43397,#43398));
#8226=EDGE_LOOP('',(#43399,#43400,#43401,#43402));
#8227=EDGE_LOOP('',(#43403,#43404,#43405,#43406));
#8228=EDGE_LOOP('',(#43407,#43408,#43409,#43410));
#8229=EDGE_LOOP('',(#43411,#43412,#43413,#43414));
#8230=EDGE_LOOP('',(#43415,#43416,#43417,#43418));
#8231=EDGE_LOOP('',(#43419,#43420,#43421,#43422));
#8232=EDGE_LOOP('',(#43423,#43424,#43425,#43426));
#8233=EDGE_LOOP('',(#43427,#43428,#43429,#43430));
#8234=EDGE_LOOP('',(#43431,#43432,#43433,#43434));
#8235=EDGE_LOOP('',(#43435,#43436,#43437,#43438));
#8236=EDGE_LOOP('',(#43439,#43440,#43441,#43442));
#8237=EDGE_LOOP('',(#43443,#43444,#43445,#43446));
#8238=EDGE_LOOP('',(#43447,#43448,#43449,#43450));
#8239=EDGE_LOOP('',(#43451,#43452,#43453,#43454));
#8240=EDGE_LOOP('',(#43455,#43456,#43457,#43458));
#8241=EDGE_LOOP('',(#43459,#43460,#43461,#43462));
#8242=EDGE_LOOP('',(#43463,#43464,#43465,#43466));
#8243=EDGE_LOOP('',(#43467,#43468,#43469,#43470));
#8244=EDGE_LOOP('',(#43471,#43472,#43473,#43474));
#8245=EDGE_LOOP('',(#43475,#43476,#43477,#43478));
#8246=EDGE_LOOP('',(#43479,#43480,#43481,#43482));
#8247=EDGE_LOOP('',(#43483,#43484,#43485,#43486));
#8248=EDGE_LOOP('',(#43487,#43488,#43489,#43490));
#8249=EDGE_LOOP('',(#43491,#43492,#43493,#43494));
#8250=EDGE_LOOP('',(#43495,#43496,#43497,#43498));
#8251=EDGE_LOOP('',(#43499,#43500,#43501,#43502));
#8252=EDGE_LOOP('',(#43503,#43504,#43505,#43506));
#8253=EDGE_LOOP('',(#43507,#43508,#43509,#43510));
#8254=EDGE_LOOP('',(#43511,#43512,#43513,#43514));
#8255=EDGE_LOOP('',(#43515,#43516,#43517,#43518));
#8256=EDGE_LOOP('',(#43519,#43520,#43521,#43522));
#8257=EDGE_LOOP('',(#43523,#43524,#43525,#43526));
#8258=EDGE_LOOP('',(#43527,#43528,#43529,#43530));
#8259=EDGE_LOOP('',(#43531,#43532,#43533,#43534));
#8260=EDGE_LOOP('',(#43535,#43536,#43537,#43538));
#8261=EDGE_LOOP('',(#43539,#43540,#43541,#43542));
#8262=EDGE_LOOP('',(#43543,#43544,#43545,#43546));
#8263=EDGE_LOOP('',(#43547,#43548,#43549,#43550));
#8264=EDGE_LOOP('',(#43551,#43552,#43553,#43554));
#8265=EDGE_LOOP('',(#43555,#43556,#43557,#43558));
#8266=EDGE_LOOP('',(#43559,#43560,#43561,#43562));
#8267=EDGE_LOOP('',(#43563,#43564,#43565,#43566));
#8268=EDGE_LOOP('',(#43567,#43568,#43569,#43570));
#8269=EDGE_LOOP('',(#43571,#43572,#43573,#43574));
#8270=EDGE_LOOP('',(#43575,#43576,#43577,#43578));
#8271=EDGE_LOOP('',(#43579,#43580,#43581,#43582));
#8272=EDGE_LOOP('',(#43583,#43584,#43585,#43586));
#8273=EDGE_LOOP('',(#43587,#43588,#43589,#43590));
#8274=EDGE_LOOP('',(#43591,#43592,#43593,#43594));
#8275=EDGE_LOOP('',(#43595,#43596,#43597,#43598));
#8276=EDGE_LOOP('',(#43599,#43600,#43601,#43602));
#8277=EDGE_LOOP('',(#43603,#43604,#43605,#43606));
#8278=EDGE_LOOP('',(#43607,#43608,#43609,#43610));
#8279=EDGE_LOOP('',(#43611,#43612,#43613,#43614));
#8280=EDGE_LOOP('',(#43615,#43616,#43617,#43618));
#8281=EDGE_LOOP('',(#43619,#43620,#43621,#43622));
#8282=EDGE_LOOP('',(#43623,#43624,#43625,#43626));
#8283=EDGE_LOOP('',(#43627,#43628,#43629,#43630));
#8284=EDGE_LOOP('',(#43631,#43632,#43633,#43634));
#8285=EDGE_LOOP('',(#43635,#43636,#43637,#43638));
#8286=EDGE_LOOP('',(#43639,#43640,#43641,#43642));
#8287=EDGE_LOOP('',(#43643,#43644,#43645,#43646));
#8288=EDGE_LOOP('',(#43647,#43648,#43649,#43650));
#8289=EDGE_LOOP('',(#43651,#43652,#43653,#43654));
#8290=EDGE_LOOP('',(#43655,#43656,#43657,#43658));
#8291=EDGE_LOOP('',(#43659,#43660,#43661,#43662));
#8292=EDGE_LOOP('',(#43663,#43664,#43665,#43666));
#8293=EDGE_LOOP('',(#43667,#43668,#43669,#43670));
#8294=EDGE_LOOP('',(#43671,#43672,#43673,#43674));
#8295=EDGE_LOOP('',(#43675,#43676,#43677,#43678));
#8296=EDGE_LOOP('',(#43679,#43680,#43681,#43682));
#8297=EDGE_LOOP('',(#43683,#43684,#43685,#43686));
#8298=EDGE_LOOP('',(#43687,#43688,#43689,#43690));
#8299=EDGE_LOOP('',(#43691,#43692,#43693,#43694));
#8300=EDGE_LOOP('',(#43695,#43696,#43697,#43698));
#8301=EDGE_LOOP('',(#43699,#43700,#43701,#43702));
#8302=EDGE_LOOP('',(#43703,#43704,#43705,#43706));
#8303=EDGE_LOOP('',(#43707,#43708,#43709,#43710));
#8304=EDGE_LOOP('',(#43711,#43712,#43713,#43714));
#8305=EDGE_LOOP('',(#43715,#43716,#43717,#43718));
#8306=EDGE_LOOP('',(#43719,#43720,#43721,#43722));
#8307=EDGE_LOOP('',(#43723,#43724,#43725,#43726));
#8308=EDGE_LOOP('',(#43727,#43728,#43729,#43730));
#8309=EDGE_LOOP('',(#43731,#43732,#43733,#43734));
#8310=EDGE_LOOP('',(#43735,#43736,#43737,#43738));
#8311=EDGE_LOOP('',(#43739,#43740,#43741,#43742));
#8312=EDGE_LOOP('',(#43743,#43744,#43745,#43746));
#8313=EDGE_LOOP('',(#43747,#43748,#43749,#43750));
#8314=EDGE_LOOP('',(#43751,#43752,#43753,#43754));
#8315=EDGE_LOOP('',(#43755,#43756,#43757,#43758));
#8316=EDGE_LOOP('',(#43759,#43760,#43761,#43762));
#8317=EDGE_LOOP('',(#43763,#43764,#43765,#43766));
#8318=EDGE_LOOP('',(#43767,#43768,#43769,#43770));
#8319=EDGE_LOOP('',(#43771,#43772,#43773,#43774));
#8320=EDGE_LOOP('',(#43775,#43776,#43777,#43778));
#8321=EDGE_LOOP('',(#43779,#43780,#43781,#43782));
#8322=EDGE_LOOP('',(#43783,#43784,#43785,#43786));
#8323=EDGE_LOOP('',(#43787,#43788,#43789,#43790));
#8324=EDGE_LOOP('',(#43791,#43792,#43793,#43794));
#8325=EDGE_LOOP('',(#43795,#43796,#43797,#43798));
#8326=EDGE_LOOP('',(#43799,#43800,#43801,#43802));
#8327=EDGE_LOOP('',(#43803,#43804,#43805,#43806));
#8328=EDGE_LOOP('',(#43807,#43808,#43809,#43810));
#8329=EDGE_LOOP('',(#43811,#43812,#43813,#43814));
#8330=EDGE_LOOP('',(#43815,#43816,#43817,#43818));
#8331=EDGE_LOOP('',(#43819,#43820,#43821,#43822));
#8332=EDGE_LOOP('',(#43823,#43824,#43825,#43826));
#8333=EDGE_LOOP('',(#43827,#43828,#43829,#43830));
#8334=EDGE_LOOP('',(#43831,#43832,#43833,#43834));
#8335=EDGE_LOOP('',(#43835,#43836,#43837,#43838));
#8336=EDGE_LOOP('',(#43839,#43840,#43841,#43842));
#8337=EDGE_LOOP('',(#43843,#43844,#43845,#43846));
#8338=EDGE_LOOP('',(#43847,#43848,#43849,#43850));
#8339=EDGE_LOOP('',(#43851,#43852,#43853,#43854));
#8340=EDGE_LOOP('',(#43855,#43856,#43857,#43858));
#8341=EDGE_LOOP('',(#43859,#43860,#43861,#43862));
#8342=EDGE_LOOP('',(#43863,#43864,#43865,#43866));
#8343=EDGE_LOOP('',(#43867,#43868,#43869,#43870));
#8344=EDGE_LOOP('',(#43871,#43872,#43873,#43874));
#8345=EDGE_LOOP('',(#43875,#43876,#43877,#43878));
#8346=EDGE_LOOP('',(#43879,#43880,#43881,#43882));
#8347=EDGE_LOOP('',(#43883,#43884,#43885,#43886));
#8348=EDGE_LOOP('',(#43887,#43888,#43889,#43890));
#8349=EDGE_LOOP('',(#43891,#43892,#43893,#43894));
#8350=EDGE_LOOP('',(#43895,#43896,#43897,#43898));
#8351=EDGE_LOOP('',(#43899,#43900,#43901,#43902));
#8352=EDGE_LOOP('',(#43903,#43904,#43905,#43906));
#8353=EDGE_LOOP('',(#43907,#43908,#43909,#43910));
#8354=EDGE_LOOP('',(#43911,#43912,#43913,#43914));
#8355=EDGE_LOOP('',(#43915,#43916,#43917,#43918));
#8356=EDGE_LOOP('',(#43919,#43920,#43921,#43922));
#8357=EDGE_LOOP('',(#43923,#43924,#43925,#43926));
#8358=EDGE_LOOP('',(#43927,#43928,#43929,#43930));
#8359=EDGE_LOOP('',(#43931,#43932,#43933,#43934));
#8360=EDGE_LOOP('',(#43935,#43936,#43937,#43938));
#8361=EDGE_LOOP('',(#43939,#43940,#43941,#43942));
#8362=EDGE_LOOP('',(#43943,#43944,#43945,#43946));
#8363=EDGE_LOOP('',(#43947,#43948,#43949,#43950));
#8364=EDGE_LOOP('',(#43951,#43952,#43953,#43954));
#8365=EDGE_LOOP('',(#43955,#43956,#43957,#43958));
#8366=EDGE_LOOP('',(#43959,#43960,#43961,#43962));
#8367=EDGE_LOOP('',(#43963,#43964,#43965,#43966));
#8368=EDGE_LOOP('',(#43967,#43968,#43969,#43970));
#8369=EDGE_LOOP('',(#43971,#43972,#43973,#43974));
#8370=EDGE_LOOP('',(#43975,#43976,#43977,#43978));
#8371=EDGE_LOOP('',(#43979,#43980,#43981,#43982));
#8372=EDGE_LOOP('',(#43983,#43984,#43985,#43986));
#8373=EDGE_LOOP('',(#43987,#43988,#43989,#43990));
#8374=EDGE_LOOP('',(#43991,#43992,#43993,#43994));
#8375=EDGE_LOOP('',(#43995,#43996,#43997,#43998));
#8376=EDGE_LOOP('',(#43999,#44000,#44001,#44002));
#8377=EDGE_LOOP('',(#44003,#44004,#44005,#44006));
#8378=EDGE_LOOP('',(#44007,#44008,#44009,#44010));
#8379=EDGE_LOOP('',(#44011,#44012,#44013,#44014));
#8380=EDGE_LOOP('',(#44015,#44016,#44017,#44018));
#8381=EDGE_LOOP('',(#44019,#44020,#44021,#44022));
#8382=EDGE_LOOP('',(#44023,#44024,#44025,#44026));
#8383=EDGE_LOOP('',(#44027,#44028,#44029,#44030));
#8384=EDGE_LOOP('',(#44031,#44032,#44033,#44034));
#8385=EDGE_LOOP('',(#44035,#44036,#44037,#44038));
#8386=EDGE_LOOP('',(#44039,#44040,#44041,#44042));
#8387=EDGE_LOOP('',(#44043,#44044,#44045,#44046));
#8388=EDGE_LOOP('',(#44047,#44048,#44049,#44050));
#8389=EDGE_LOOP('',(#44051,#44052,#44053,#44054));
#8390=EDGE_LOOP('',(#44055,#44056,#44057,#44058));
#8391=EDGE_LOOP('',(#44059,#44060,#44061,#44062));
#8392=EDGE_LOOP('',(#44063,#44064,#44065,#44066));
#8393=EDGE_LOOP('',(#44067,#44068,#44069,#44070));
#8394=EDGE_LOOP('',(#44071,#44072,#44073,#44074));
#8395=EDGE_LOOP('',(#44075,#44076,#44077,#44078));
#8396=EDGE_LOOP('',(#44079,#44080,#44081,#44082));
#8397=EDGE_LOOP('',(#44083,#44084,#44085,#44086));
#8398=EDGE_LOOP('',(#44087,#44088,#44089,#44090));
#8399=EDGE_LOOP('',(#44091,#44092,#44093,#44094));
#8400=EDGE_LOOP('',(#44095,#44096,#44097,#44098));
#8401=EDGE_LOOP('',(#44099,#44100,#44101,#44102));
#8402=EDGE_LOOP('',(#44103,#44104,#44105,#44106));
#8403=EDGE_LOOP('',(#44107,#44108,#44109,#44110));
#8404=EDGE_LOOP('',(#44111,#44112,#44113,#44114));
#8405=EDGE_LOOP('',(#44115,#44116,#44117,#44118));
#8406=EDGE_LOOP('',(#44119,#44120,#44121,#44122));
#8407=EDGE_LOOP('',(#44123,#44124,#44125,#44126));
#8408=EDGE_LOOP('',(#44127,#44128,#44129,#44130));
#8409=EDGE_LOOP('',(#44131,#44132,#44133,#44134));
#8410=EDGE_LOOP('',(#44135,#44136,#44137,#44138));
#8411=EDGE_LOOP('',(#44139,#44140,#44141,#44142));
#8412=EDGE_LOOP('',(#44143,#44144,#44145,#44146));
#8413=EDGE_LOOP('',(#44147,#44148,#44149,#44150));
#8414=EDGE_LOOP('',(#44151,#44152,#44153,#44154));
#8415=EDGE_LOOP('',(#44155,#44156,#44157,#44158));
#8416=EDGE_LOOP('',(#44159,#44160,#44161,#44162));
#8417=EDGE_LOOP('',(#44163,#44164,#44165,#44166));
#8418=EDGE_LOOP('',(#44167,#44168,#44169,#44170));
#8419=EDGE_LOOP('',(#44171,#44172,#44173,#44174));
#8420=EDGE_LOOP('',(#44175,#44176,#44177,#44178));
#8421=EDGE_LOOP('',(#44179,#44180,#44181,#44182));
#8422=EDGE_LOOP('',(#44183,#44184,#44185,#44186));
#8423=EDGE_LOOP('',(#44187,#44188,#44189,#44190));
#8424=EDGE_LOOP('',(#44191,#44192,#44193,#44194));
#8425=EDGE_LOOP('',(#44195,#44196,#44197,#44198));
#8426=EDGE_LOOP('',(#44199,#44200,#44201,#44202));
#8427=EDGE_LOOP('',(#44203,#44204,#44205,#44206));
#8428=EDGE_LOOP('',(#44207,#44208,#44209,#44210));
#8429=EDGE_LOOP('',(#44211,#44212,#44213,#44214));
#8430=EDGE_LOOP('',(#44215,#44216,#44217,#44218));
#8431=EDGE_LOOP('',(#44219,#44220,#44221,#44222));
#8432=EDGE_LOOP('',(#44223,#44224,#44225,#44226));
#8433=EDGE_LOOP('',(#44227,#44228,#44229,#44230));
#8434=EDGE_LOOP('',(#44231,#44232,#44233,#44234));
#8435=EDGE_LOOP('',(#44235,#44236,#44237,#44238));
#8436=EDGE_LOOP('',(#44239,#44240,#44241,#44242));
#8437=EDGE_LOOP('',(#44243,#44244,#44245,#44246));
#8438=EDGE_LOOP('',(#44247,#44248,#44249,#44250));
#8439=EDGE_LOOP('',(#44251,#44252,#44253,#44254));
#8440=EDGE_LOOP('',(#44255,#44256,#44257,#44258));
#8441=EDGE_LOOP('',(#44259,#44260,#44261,#44262));
#8442=EDGE_LOOP('',(#44263,#44264,#44265,#44266));
#8443=EDGE_LOOP('',(#44267,#44268,#44269,#44270));
#8444=EDGE_LOOP('',(#44271,#44272,#44273,#44274));
#8445=EDGE_LOOP('',(#44275,#44276,#44277,#44278));
#8446=EDGE_LOOP('',(#44279,#44280,#44281,#44282));
#8447=EDGE_LOOP('',(#44283,#44284,#44285,#44286));
#8448=EDGE_LOOP('',(#44287,#44288,#44289,#44290));
#8449=EDGE_LOOP('',(#44291,#44292,#44293,#44294));
#8450=EDGE_LOOP('',(#44295,#44296,#44297,#44298));
#8451=EDGE_LOOP('',(#44299,#44300,#44301,#44302));
#8452=EDGE_LOOP('',(#44303,#44304,#44305,#44306));
#8453=EDGE_LOOP('',(#44307,#44308,#44309,#44310));
#8454=EDGE_LOOP('',(#44311,#44312,#44313,#44314));
#8455=EDGE_LOOP('',(#44315,#44316,#44317,#44318));
#8456=EDGE_LOOP('',(#44319,#44320,#44321,#44322));
#8457=EDGE_LOOP('',(#44323,#44324,#44325,#44326));
#8458=EDGE_LOOP('',(#44327,#44328,#44329,#44330));
#8459=EDGE_LOOP('',(#44331,#44332,#44333,#44334));
#8460=EDGE_LOOP('',(#44335,#44336,#44337,#44338));
#8461=EDGE_LOOP('',(#44339,#44340,#44341,#44342));
#8462=EDGE_LOOP('',(#44343,#44344,#44345,#44346));
#8463=EDGE_LOOP('',(#44347,#44348,#44349,#44350));
#8464=EDGE_LOOP('',(#44351,#44352,#44353,#44354));
#8465=EDGE_LOOP('',(#44355,#44356,#44357,#44358));
#8466=EDGE_LOOP('',(#44359,#44360,#44361,#44362));
#8467=EDGE_LOOP('',(#44363,#44364,#44365,#44366));
#8468=EDGE_LOOP('',(#44367,#44368,#44369,#44370));
#8469=EDGE_LOOP('',(#44371,#44372,#44373,#44374));
#8470=EDGE_LOOP('',(#44375,#44376,#44377,#44378));
#8471=EDGE_LOOP('',(#44379,#44380,#44381,#44382));
#8472=EDGE_LOOP('',(#44383,#44384,#44385,#44386));
#8473=EDGE_LOOP('',(#44387,#44388,#44389,#44390));
#8474=EDGE_LOOP('',(#44391,#44392,#44393,#44394));
#8475=EDGE_LOOP('',(#44395,#44396,#44397,#44398));
#8476=EDGE_LOOP('',(#44399,#44400,#44401,#44402));
#8477=EDGE_LOOP('',(#44403,#44404,#44405,#44406));
#8478=EDGE_LOOP('',(#44407,#44408,#44409,#44410));
#8479=EDGE_LOOP('',(#44411,#44412,#44413,#44414));
#8480=EDGE_LOOP('',(#44415,#44416,#44417,#44418));
#8481=EDGE_LOOP('',(#44419,#44420,#44421,#44422));
#8482=EDGE_LOOP('',(#44423,#44424,#44425,#44426));
#8483=EDGE_LOOP('',(#44427,#44428,#44429,#44430));
#8484=EDGE_LOOP('',(#44431,#44432,#44433,#44434));
#8485=EDGE_LOOP('',(#44435,#44436,#44437,#44438));
#8486=EDGE_LOOP('',(#44439,#44440,#44441,#44442));
#8487=EDGE_LOOP('',(#44443,#44444,#44445,#44446));
#8488=EDGE_LOOP('',(#44447,#44448,#44449,#44450));
#8489=EDGE_LOOP('',(#44451,#44452,#44453,#44454));
#8490=EDGE_LOOP('',(#44455,#44456,#44457,#44458));
#8491=EDGE_LOOP('',(#44459,#44460,#44461,#44462));
#8492=EDGE_LOOP('',(#44463,#44464,#44465,#44466));
#8493=EDGE_LOOP('',(#44467,#44468,#44469,#44470));
#8494=EDGE_LOOP('',(#44471,#44472,#44473,#44474));
#8495=EDGE_LOOP('',(#44475,#44476,#44477,#44478));
#8496=EDGE_LOOP('',(#44479,#44480,#44481,#44482));
#8497=EDGE_LOOP('',(#44483,#44484,#44485,#44486));
#8498=EDGE_LOOP('',(#44487,#44488,#44489,#44490));
#8499=EDGE_LOOP('',(#44491,#44492,#44493,#44494));
#8500=EDGE_LOOP('',(#44495,#44496,#44497,#44498));
#8501=EDGE_LOOP('',(#44499,#44500,#44501,#44502));
#8502=EDGE_LOOP('',(#44503,#44504,#44505,#44506));
#8503=EDGE_LOOP('',(#44507,#44508,#44509,#44510));
#8504=EDGE_LOOP('',(#44511,#44512,#44513,#44514));
#8505=EDGE_LOOP('',(#44515,#44516,#44517,#44518));
#8506=EDGE_LOOP('',(#44519,#44520,#44521,#44522));
#8507=EDGE_LOOP('',(#44523,#44524,#44525,#44526));
#8508=EDGE_LOOP('',(#44527,#44528,#44529,#44530));
#8509=EDGE_LOOP('',(#44531,#44532,#44533,#44534));
#8510=EDGE_LOOP('',(#44535,#44536,#44537,#44538));
#8511=EDGE_LOOP('',(#44539,#44540,#44541,#44542));
#8512=EDGE_LOOP('',(#44543,#44544,#44545,#44546));
#8513=EDGE_LOOP('',(#44547,#44548,#44549,#44550));
#8514=EDGE_LOOP('',(#44551,#44552,#44553,#44554));
#8515=EDGE_LOOP('',(#44555,#44556,#44557,#44558));
#8516=EDGE_LOOP('',(#44559,#44560,#44561,#44562));
#8517=EDGE_LOOP('',(#44563,#44564,#44565,#44566));
#8518=EDGE_LOOP('',(#44567,#44568,#44569,#44570));
#8519=EDGE_LOOP('',(#44571,#44572,#44573,#44574));
#8520=EDGE_LOOP('',(#44575,#44576,#44577,#44578));
#8521=EDGE_LOOP('',(#44579,#44580,#44581,#44582));
#8522=EDGE_LOOP('',(#44583,#44584,#44585,#44586));
#8523=EDGE_LOOP('',(#44587,#44588,#44589,#44590));
#8524=EDGE_LOOP('',(#44591,#44592,#44593,#44594));
#8525=EDGE_LOOP('',(#44595,#44596,#44597,#44598));
#8526=EDGE_LOOP('',(#44599,#44600,#44601,#44602));
#8527=EDGE_LOOP('',(#44603,#44604,#44605,#44606));
#8528=EDGE_LOOP('',(#44607,#44608,#44609,#44610));
#8529=EDGE_LOOP('',(#44611,#44612,#44613,#44614));
#8530=EDGE_LOOP('',(#44615,#44616,#44617,#44618));
#8531=EDGE_LOOP('',(#44619,#44620,#44621,#44622));
#8532=EDGE_LOOP('',(#44623,#44624,#44625,#44626));
#8533=EDGE_LOOP('',(#44627,#44628,#44629,#44630));
#8534=EDGE_LOOP('',(#44631,#44632,#44633,#44634));
#8535=EDGE_LOOP('',(#44635,#44636,#44637,#44638));
#8536=EDGE_LOOP('',(#44639,#44640,#44641,#44642));
#8537=EDGE_LOOP('',(#44643,#44644,#44645,#44646));
#8538=EDGE_LOOP('',(#44647,#44648,#44649,#44650));
#8539=EDGE_LOOP('',(#44651,#44652,#44653,#44654));
#8540=EDGE_LOOP('',(#44655,#44656,#44657,#44658));
#8541=EDGE_LOOP('',(#44659,#44660,#44661,#44662));
#8542=EDGE_LOOP('',(#44663,#44664,#44665,#44666));
#8543=EDGE_LOOP('',(#44667,#44668,#44669,#44670));
#8544=EDGE_LOOP('',(#44671,#44672,#44673,#44674));
#8545=EDGE_LOOP('',(#44675,#44676,#44677,#44678));
#8546=EDGE_LOOP('',(#44679,#44680,#44681,#44682));
#8547=EDGE_LOOP('',(#44683,#44684,#44685,#44686));
#8548=EDGE_LOOP('',(#44687,#44688,#44689,#44690));
#8549=EDGE_LOOP('',(#44691,#44692,#44693,#44694));
#8550=EDGE_LOOP('',(#44695,#44696,#44697,#44698));
#8551=EDGE_LOOP('',(#44699,#44700,#44701,#44702));
#8552=EDGE_LOOP('',(#44703,#44704,#44705,#44706));
#8553=EDGE_LOOP('',(#44707,#44708,#44709,#44710));
#8554=EDGE_LOOP('',(#44711,#44712,#44713,#44714));
#8555=EDGE_LOOP('',(#44715,#44716,#44717,#44718));
#8556=EDGE_LOOP('',(#44719,#44720,#44721,#44722));
#8557=EDGE_LOOP('',(#44723,#44724,#44725,#44726));
#8558=EDGE_LOOP('',(#44727,#44728,#44729,#44730));
#8559=EDGE_LOOP('',(#44731,#44732,#44733,#44734));
#8560=EDGE_LOOP('',(#44735,#44736,#44737,#44738));
#8561=EDGE_LOOP('',(#44739,#44740,#44741,#44742));
#8562=EDGE_LOOP('',(#44743,#44744,#44745,#44746));
#8563=EDGE_LOOP('',(#44747,#44748,#44749,#44750));
#8564=EDGE_LOOP('',(#44751,#44752,#44753,#44754));
#8565=EDGE_LOOP('',(#44755,#44756,#44757,#44758));
#8566=EDGE_LOOP('',(#44759,#44760,#44761,#44762));
#8567=EDGE_LOOP('',(#44763,#44764,#44765,#44766));
#8568=EDGE_LOOP('',(#44767,#44768,#44769,#44770));
#8569=EDGE_LOOP('',(#44771,#44772,#44773,#44774));
#8570=EDGE_LOOP('',(#44775,#44776,#44777,#44778));
#8571=EDGE_LOOP('',(#44779,#44780,#44781,#44782));
#8572=EDGE_LOOP('',(#44783,#44784,#44785,#44786));
#8573=EDGE_LOOP('',(#44787,#44788,#44789,#44790));
#8574=EDGE_LOOP('',(#44791,#44792,#44793,#44794));
#8575=EDGE_LOOP('',(#44795,#44796,#44797,#44798));
#8576=EDGE_LOOP('',(#44799,#44800,#44801,#44802));
#8577=EDGE_LOOP('',(#44803,#44804,#44805,#44806));
#8578=EDGE_LOOP('',(#44807,#44808,#44809,#44810));
#8579=EDGE_LOOP('',(#44811,#44812,#44813,#44814));
#8580=EDGE_LOOP('',(#44815,#44816,#44817,#44818));
#8581=EDGE_LOOP('',(#44819,#44820,#44821,#44822));
#8582=EDGE_LOOP('',(#44823,#44824,#44825,#44826));
#8583=EDGE_LOOP('',(#44827,#44828,#44829,#44830));
#8584=EDGE_LOOP('',(#44831,#44832,#44833,#44834));
#8585=EDGE_LOOP('',(#44835,#44836,#44837,#44838));
#8586=EDGE_LOOP('',(#44839,#44840,#44841,#44842));
#8587=EDGE_LOOP('',(#44843,#44844,#44845,#44846));
#8588=EDGE_LOOP('',(#44847,#44848,#44849,#44850));
#8589=EDGE_LOOP('',(#44851,#44852,#44853,#44854));
#8590=EDGE_LOOP('',(#44855,#44856,#44857,#44858));
#8591=EDGE_LOOP('',(#44859,#44860,#44861,#44862));
#8592=EDGE_LOOP('',(#44863,#44864,#44865,#44866));
#8593=EDGE_LOOP('',(#44867,#44868,#44869,#44870));
#8594=EDGE_LOOP('',(#44871,#44872,#44873,#44874));
#8595=EDGE_LOOP('',(#44875,#44876,#44877,#44878));
#8596=EDGE_LOOP('',(#44879,#44880,#44881,#44882));
#8597=EDGE_LOOP('',(#44883,#44884,#44885,#44886));
#8598=EDGE_LOOP('',(#44887,#44888,#44889,#44890));
#8599=EDGE_LOOP('',(#44891,#44892,#44893,#44894));
#8600=EDGE_LOOP('',(#44895,#44896,#44897,#44898));
#8601=EDGE_LOOP('',(#44899,#44900,#44901,#44902));
#8602=EDGE_LOOP('',(#44903,#44904,#44905,#44906));
#8603=EDGE_LOOP('',(#44907,#44908,#44909,#44910));
#8604=EDGE_LOOP('',(#44911,#44912,#44913,#44914));
#8605=EDGE_LOOP('',(#44915,#44916,#44917,#44918));
#8606=EDGE_LOOP('',(#44919,#44920,#44921,#44922));
#8607=EDGE_LOOP('',(#44923,#44924,#44925,#44926));
#8608=EDGE_LOOP('',(#44927,#44928,#44929,#44930));
#8609=EDGE_LOOP('',(#44931,#44932,#44933,#44934));
#8610=EDGE_LOOP('',(#44935,#44936,#44937,#44938));
#8611=EDGE_LOOP('',(#44939,#44940,#44941,#44942));
#8612=EDGE_LOOP('',(#44943,#44944,#44945,#44946));
#8613=EDGE_LOOP('',(#44947,#44948,#44949,#44950));
#8614=EDGE_LOOP('',(#44951,#44952,#44953,#44954));
#8615=EDGE_LOOP('',(#44955,#44956,#44957,#44958));
#8616=EDGE_LOOP('',(#44959,#44960,#44961,#44962));
#8617=EDGE_LOOP('',(#44963,#44964,#44965,#44966));
#8618=EDGE_LOOP('',(#44967,#44968,#44969,#44970));
#8619=EDGE_LOOP('',(#44971,#44972,#44973,#44974));
#8620=EDGE_LOOP('',(#44975,#44976,#44977,#44978));
#8621=EDGE_LOOP('',(#44979,#44980,#44981,#44982));
#8622=EDGE_LOOP('',(#44983,#44984,#44985,#44986));
#8623=EDGE_LOOP('',(#44987,#44988,#44989,#44990));
#8624=EDGE_LOOP('',(#44991,#44992,#44993,#44994));
#8625=EDGE_LOOP('',(#44995,#44996,#44997,#44998));
#8626=EDGE_LOOP('',(#44999,#45000,#45001,#45002));
#8627=EDGE_LOOP('',(#45003,#45004,#45005,#45006));
#8628=EDGE_LOOP('',(#45007,#45008,#45009,#45010));
#8629=EDGE_LOOP('',(#45011,#45012,#45013,#45014));
#8630=EDGE_LOOP('',(#45015,#45016,#45017,#45018));
#8631=EDGE_LOOP('',(#45019,#45020,#45021,#45022));
#8632=EDGE_LOOP('',(#45023,#45024,#45025,#45026));
#8633=EDGE_LOOP('',(#45027,#45028,#45029,#45030));
#8634=EDGE_LOOP('',(#45031,#45032,#45033,#45034));
#8635=EDGE_LOOP('',(#45035,#45036,#45037,#45038));
#8636=EDGE_LOOP('',(#45039,#45040,#45041,#45042));
#8637=EDGE_LOOP('',(#45043,#45044,#45045,#45046));
#8638=EDGE_LOOP('',(#45047,#45048,#45049,#45050));
#8639=EDGE_LOOP('',(#45051,#45052,#45053,#45054));
#8640=EDGE_LOOP('',(#45055,#45056,#45057,#45058));
#8641=EDGE_LOOP('',(#45059,#45060,#45061,#45062));
#8642=EDGE_LOOP('',(#45063,#45064,#45065,#45066));
#8643=EDGE_LOOP('',(#45067,#45068,#45069,#45070));
#8644=EDGE_LOOP('',(#45071,#45072,#45073,#45074));
#8645=EDGE_LOOP('',(#45075,#45076,#45077,#45078));
#8646=EDGE_LOOP('',(#45079,#45080,#45081,#45082));
#8647=EDGE_LOOP('',(#45083,#45084,#45085,#45086));
#8648=EDGE_LOOP('',(#45087,#45088,#45089,#45090));
#8649=EDGE_LOOP('',(#45091,#45092,#45093,#45094));
#8650=EDGE_LOOP('',(#45095,#45096,#45097,#45098));
#8651=EDGE_LOOP('',(#45099,#45100,#45101,#45102));
#8652=EDGE_LOOP('',(#45103,#45104,#45105,#45106));
#8653=EDGE_LOOP('',(#45107,#45108,#45109,#45110));
#8654=EDGE_LOOP('',(#45111,#45112,#45113,#45114));
#8655=EDGE_LOOP('',(#45115,#45116,#45117,#45118));
#8656=EDGE_LOOP('',(#45119,#45120,#45121,#45122));
#8657=EDGE_LOOP('',(#45123,#45124,#45125,#45126));
#8658=EDGE_LOOP('',(#45127,#45128,#45129,#45130));
#8659=EDGE_LOOP('',(#45131,#45132,#45133,#45134));
#8660=EDGE_LOOP('',(#45135,#45136,#45137,#45138));
#8661=EDGE_LOOP('',(#45139,#45140,#45141,#45142));
#8662=EDGE_LOOP('',(#45143,#45144,#45145,#45146));
#8663=EDGE_LOOP('',(#45147,#45148,#45149,#45150));
#8664=EDGE_LOOP('',(#45151,#45152,#45153,#45154));
#8665=EDGE_LOOP('',(#45155,#45156,#45157,#45158));
#8666=EDGE_LOOP('',(#45159,#45160,#45161,#45162));
#8667=EDGE_LOOP('',(#45163,#45164,#45165,#45166));
#8668=EDGE_LOOP('',(#45167,#45168,#45169,#45170));
#8669=EDGE_LOOP('',(#45171,#45172,#45173,#45174));
#8670=EDGE_LOOP('',(#45175,#45176,#45177,#45178));
#8671=EDGE_LOOP('',(#45179,#45180,#45181,#45182));
#8672=EDGE_LOOP('',(#45183,#45184,#45185,#45186));
#8673=EDGE_LOOP('',(#45187,#45188,#45189,#45190));
#8674=EDGE_LOOP('',(#45191,#45192,#45193,#45194));
#8675=EDGE_LOOP('',(#45195,#45196,#45197,#45198));
#8676=EDGE_LOOP('',(#45199,#45200,#45201,#45202));
#8677=EDGE_LOOP('',(#45203,#45204,#45205,#45206));
#8678=EDGE_LOOP('',(#45207,#45208,#45209,#45210));
#8679=EDGE_LOOP('',(#45211,#45212,#45213,#45214));
#8680=EDGE_LOOP('',(#45215,#45216,#45217,#45218));
#8681=EDGE_LOOP('',(#45219,#45220,#45221,#45222));
#8682=EDGE_LOOP('',(#45223,#45224,#45225,#45226));
#8683=EDGE_LOOP('',(#45227,#45228,#45229,#45230));
#8684=EDGE_LOOP('',(#45231,#45232,#45233,#45234));
#8685=EDGE_LOOP('',(#45235,#45236,#45237,#45238));
#8686=EDGE_LOOP('',(#45239,#45240,#45241,#45242));
#8687=EDGE_LOOP('',(#45243,#45244,#45245,#45246));
#8688=EDGE_LOOP('',(#45247,#45248,#45249,#45250));
#8689=EDGE_LOOP('',(#45251,#45252,#45253,#45254));
#8690=EDGE_LOOP('',(#45255,#45256,#45257,#45258));
#8691=EDGE_LOOP('',(#45259,#45260,#45261,#45262));
#8692=EDGE_LOOP('',(#45263,#45264,#45265,#45266));
#8693=EDGE_LOOP('',(#45267,#45268,#45269,#45270));
#8694=EDGE_LOOP('',(#45271,#45272,#45273,#45274));
#8695=EDGE_LOOP('',(#45275,#45276,#45277,#45278));
#8696=EDGE_LOOP('',(#45279,#45280,#45281,#45282));
#8697=EDGE_LOOP('',(#45283,#45284,#45285,#45286));
#8698=EDGE_LOOP('',(#45287,#45288,#45289,#45290));
#8699=EDGE_LOOP('',(#45291,#45292,#45293,#45294));
#8700=EDGE_LOOP('',(#45295,#45296,#45297,#45298));
#8701=EDGE_LOOP('',(#45299,#45300,#45301,#45302));
#8702=EDGE_LOOP('',(#45303,#45304,#45305,#45306));
#8703=EDGE_LOOP('',(#45307,#45308,#45309,#45310));
#8704=EDGE_LOOP('',(#45311,#45312,#45313,#45314));
#8705=EDGE_LOOP('',(#45315,#45316,#45317,#45318));
#8706=EDGE_LOOP('',(#45319,#45320,#45321,#45322));
#8707=EDGE_LOOP('',(#45323,#45324,#45325,#45326));
#8708=EDGE_LOOP('',(#45327,#45328,#45329,#45330));
#8709=EDGE_LOOP('',(#45331,#45332,#45333,#45334));
#8710=EDGE_LOOP('',(#45335,#45336,#45337,#45338));
#8711=EDGE_LOOP('',(#45339,#45340,#45341,#45342));
#8712=EDGE_LOOP('',(#45343,#45344,#45345,#45346));
#8713=EDGE_LOOP('',(#45347,#45348,#45349,#45350));
#8714=EDGE_LOOP('',(#45351,#45352,#45353,#45354));
#8715=EDGE_LOOP('',(#45355,#45356,#45357,#45358));
#8716=EDGE_LOOP('',(#45359,#45360,#45361,#45362));
#8717=EDGE_LOOP('',(#45363,#45364,#45365,#45366));
#8718=EDGE_LOOP('',(#45367,#45368,#45369,#45370));
#8719=EDGE_LOOP('',(#45371,#45372,#45373,#45374));
#8720=EDGE_LOOP('',(#45375,#45376,#45377,#45378));
#8721=EDGE_LOOP('',(#45379,#45380,#45381,#45382));
#8722=EDGE_LOOP('',(#45383,#45384,#45385,#45386));
#8723=EDGE_LOOP('',(#45387,#45388,#45389,#45390));
#8724=EDGE_LOOP('',(#45391,#45392,#45393,#45394));
#8725=EDGE_LOOP('',(#45395,#45396,#45397,#45398));
#8726=EDGE_LOOP('',(#45399,#45400,#45401,#45402));
#8727=EDGE_LOOP('',(#45403,#45404,#45405,#45406));
#8728=EDGE_LOOP('',(#45407,#45408,#45409,#45410));
#8729=EDGE_LOOP('',(#45411,#45412,#45413,#45414));
#8730=EDGE_LOOP('',(#45415,#45416,#45417,#45418));
#8731=EDGE_LOOP('',(#45419,#45420,#45421,#45422));
#8732=EDGE_LOOP('',(#45423,#45424,#45425,#45426));
#8733=EDGE_LOOP('',(#45427,#45428,#45429,#45430));
#8734=EDGE_LOOP('',(#45431,#45432,#45433,#45434));
#8735=EDGE_LOOP('',(#45435,#45436,#45437,#45438));
#8736=EDGE_LOOP('',(#45439,#45440,#45441,#45442));
#8737=EDGE_LOOP('',(#45443,#45444,#45445,#45446));
#8738=EDGE_LOOP('',(#45447,#45448,#45449,#45450));
#8739=EDGE_LOOP('',(#45451,#45452,#45453,#45454));
#8740=EDGE_LOOP('',(#45455,#45456,#45457,#45458));
#8741=EDGE_LOOP('',(#45459,#45460,#45461,#45462));
#8742=EDGE_LOOP('',(#45463,#45464,#45465,#45466));
#8743=EDGE_LOOP('',(#45467,#45468,#45469,#45470));
#8744=EDGE_LOOP('',(#45471,#45472,#45473,#45474));
#8745=EDGE_LOOP('',(#45475,#45476,#45477,#45478));
#8746=EDGE_LOOP('',(#45479,#45480,#45481,#45482));
#8747=EDGE_LOOP('',(#45483,#45484,#45485,#45486));
#8748=EDGE_LOOP('',(#45487,#45488,#45489,#45490));
#8749=EDGE_LOOP('',(#45491,#45492,#45493,#45494));
#8750=EDGE_LOOP('',(#45495,#45496,#45497,#45498));
#8751=EDGE_LOOP('',(#45499,#45500,#45501,#45502));
#8752=EDGE_LOOP('',(#45503,#45504,#45505,#45506));
#8753=EDGE_LOOP('',(#45507,#45508,#45509,#45510));
#8754=EDGE_LOOP('',(#45511,#45512,#45513,#45514));
#8755=EDGE_LOOP('',(#45515,#45516,#45517,#45518));
#8756=EDGE_LOOP('',(#45519,#45520,#45521,#45522));
#8757=EDGE_LOOP('',(#45523,#45524,#45525,#45526));
#8758=EDGE_LOOP('',(#45527,#45528,#45529,#45530));
#8759=EDGE_LOOP('',(#45531,#45532,#45533,#45534));
#8760=EDGE_LOOP('',(#45535,#45536,#45537,#45538));
#8761=EDGE_LOOP('',(#45539,#45540,#45541,#45542));
#8762=EDGE_LOOP('',(#45543,#45544,#45545,#45546));
#8763=EDGE_LOOP('',(#45547,#45548,#45549,#45550));
#8764=EDGE_LOOP('',(#45551,#45552,#45553,#45554));
#8765=EDGE_LOOP('',(#45555,#45556,#45557,#45558));
#8766=EDGE_LOOP('',(#45559,#45560,#45561,#45562));
#8767=EDGE_LOOP('',(#45563,#45564,#45565,#45566));
#8768=EDGE_LOOP('',(#45567,#45568,#45569,#45570));
#8769=EDGE_LOOP('',(#45571,#45572,#45573,#45574));
#8770=EDGE_LOOP('',(#45575,#45576,#45577,#45578));
#8771=EDGE_LOOP('',(#45579,#45580,#45581,#45582));
#8772=EDGE_LOOP('',(#45583,#45584,#45585,#45586));
#8773=EDGE_LOOP('',(#45587,#45588,#45589,#45590));
#8774=EDGE_LOOP('',(#45591,#45592,#45593,#45594));
#8775=EDGE_LOOP('',(#45595,#45596,#45597,#45598));
#8776=EDGE_LOOP('',(#45599,#45600,#45601,#45602));
#8777=EDGE_LOOP('',(#45603,#45604,#45605,#45606));
#8778=EDGE_LOOP('',(#45607,#45608,#45609,#45610));
#8779=EDGE_LOOP('',(#45611,#45612,#45613,#45614));
#8780=EDGE_LOOP('',(#45615,#45616,#45617,#45618));
#8781=EDGE_LOOP('',(#45619,#45620,#45621,#45622));
#8782=EDGE_LOOP('',(#45623,#45624,#45625,#45626));
#8783=EDGE_LOOP('',(#45627,#45628,#45629,#45630));
#8784=EDGE_LOOP('',(#45631,#45632,#45633,#45634));
#8785=EDGE_LOOP('',(#45635,#45636,#45637,#45638));
#8786=EDGE_LOOP('',(#45639,#45640,#45641,#45642));
#8787=EDGE_LOOP('',(#45643,#45644,#45645,#45646));
#8788=EDGE_LOOP('',(#45647,#45648,#45649,#45650));
#8789=EDGE_LOOP('',(#45651,#45652,#45653,#45654));
#8790=EDGE_LOOP('',(#45655,#45656,#45657,#45658));
#8791=EDGE_LOOP('',(#45659,#45660,#45661,#45662));
#8792=EDGE_LOOP('',(#45663,#45664,#45665,#45666));
#8793=EDGE_LOOP('',(#45667,#45668,#45669,#45670));
#8794=EDGE_LOOP('',(#45671,#45672,#45673,#45674));
#8795=EDGE_LOOP('',(#45675,#45676,#45677,#45678));
#8796=EDGE_LOOP('',(#45679,#45680,#45681,#45682));
#8797=EDGE_LOOP('',(#45683,#45684,#45685,#45686));
#8798=EDGE_LOOP('',(#45687,#45688,#45689,#45690));
#8799=EDGE_LOOP('',(#45691,#45692,#45693,#45694));
#8800=EDGE_LOOP('',(#45695,#45696,#45697,#45698));
#8801=EDGE_LOOP('',(#45699,#45700,#45701,#45702));
#8802=EDGE_LOOP('',(#45703,#45704,#45705,#45706));
#8803=EDGE_LOOP('',(#45707,#45708,#45709,#45710));
#8804=EDGE_LOOP('',(#45711,#45712,#45713,#45714));
#8805=EDGE_LOOP('',(#45715,#45716,#45717,#45718));
#8806=EDGE_LOOP('',(#45719,#45720,#45721,#45722));
#8807=EDGE_LOOP('',(#45723,#45724,#45725,#45726));
#8808=EDGE_LOOP('',(#45727,#45728,#45729,#45730));
#8809=EDGE_LOOP('',(#45731,#45732,#45733,#45734));
#8810=EDGE_LOOP('',(#45735,#45736,#45737,#45738));
#8811=EDGE_LOOP('',(#45739,#45740,#45741,#45742));
#8812=EDGE_LOOP('',(#45743,#45744,#45745,#45746));
#8813=EDGE_LOOP('',(#45747,#45748,#45749,#45750));
#8814=EDGE_LOOP('',(#45751,#45752,#45753,#45754));
#8815=EDGE_LOOP('',(#45755,#45756,#45757,#45758));
#8816=EDGE_LOOP('',(#45759,#45760,#45761,#45762));
#8817=EDGE_LOOP('',(#45763,#45764,#45765,#45766));
#8818=EDGE_LOOP('',(#45767,#45768,#45769,#45770));
#8819=EDGE_LOOP('',(#45771,#45772,#45773,#45774));
#8820=EDGE_LOOP('',(#45775,#45776,#45777,#45778));
#8821=EDGE_LOOP('',(#45779,#45780,#45781,#45782));
#8822=EDGE_LOOP('',(#45783,#45784,#45785,#45786));
#8823=EDGE_LOOP('',(#45787,#45788,#45789,#45790));
#8824=EDGE_LOOP('',(#45791,#45792,#45793,#45794));
#8825=EDGE_LOOP('',(#45795,#45796,#45797,#45798));
#8826=EDGE_LOOP('',(#45799,#45800,#45801,#45802));
#8827=EDGE_LOOP('',(#45803,#45804,#45805,#45806));
#8828=EDGE_LOOP('',(#45807,#45808,#45809,#45810));
#8829=EDGE_LOOP('',(#45811,#45812,#45813,#45814));
#8830=EDGE_LOOP('',(#45815,#45816,#45817,#45818));
#8831=EDGE_LOOP('',(#45819,#45820,#45821,#45822));
#8832=EDGE_LOOP('',(#45823,#45824,#45825,#45826));
#8833=EDGE_LOOP('',(#45827,#45828,#45829,#45830));
#8834=EDGE_LOOP('',(#45831,#45832,#45833,#45834));
#8835=EDGE_LOOP('',(#45835,#45836,#45837,#45838));
#8836=EDGE_LOOP('',(#45839,#45840,#45841,#45842));
#8837=EDGE_LOOP('',(#45843,#45844,#45845,#45846));
#8838=EDGE_LOOP('',(#45847,#45848,#45849,#45850));
#8839=EDGE_LOOP('',(#45851,#45852,#45853,#45854));
#8840=EDGE_LOOP('',(#45855,#45856,#45857,#45858));
#8841=EDGE_LOOP('',(#45859,#45860,#45861,#45862));
#8842=EDGE_LOOP('',(#45863,#45864,#45865,#45866));
#8843=EDGE_LOOP('',(#45867,#45868,#45869,#45870));
#8844=EDGE_LOOP('',(#45871,#45872,#45873,#45874));
#8845=EDGE_LOOP('',(#45875,#45876,#45877,#45878));
#8846=EDGE_LOOP('',(#45879,#45880,#45881,#45882));
#8847=EDGE_LOOP('',(#45883,#45884,#45885,#45886));
#8848=EDGE_LOOP('',(#45887,#45888,#45889,#45890));
#8849=EDGE_LOOP('',(#45891,#45892,#45893,#45894));
#8850=EDGE_LOOP('',(#45895,#45896,#45897,#45898));
#8851=EDGE_LOOP('',(#45899,#45900,#45901,#45902));
#8852=EDGE_LOOP('',(#45903,#45904,#45905,#45906));
#8853=EDGE_LOOP('',(#45907,#45908,#45909,#45910));
#8854=EDGE_LOOP('',(#45911,#45912,#45913,#45914));
#8855=EDGE_LOOP('',(#45915,#45916,#45917,#45918));
#8856=EDGE_LOOP('',(#45919,#45920,#45921,#45922));
#8857=EDGE_LOOP('',(#45923,#45924,#45925,#45926));
#8858=EDGE_LOOP('',(#45927,#45928,#45929,#45930));
#8859=EDGE_LOOP('',(#45931,#45932,#45933,#45934));
#8860=EDGE_LOOP('',(#45935,#45936,#45937,#45938));
#8861=EDGE_LOOP('',(#45939,#45940,#45941,#45942));
#8862=EDGE_LOOP('',(#45943,#45944,#45945,#45946));
#8863=EDGE_LOOP('',(#45947,#45948,#45949,#45950));
#8864=EDGE_LOOP('',(#45951,#45952,#45953,#45954));
#8865=EDGE_LOOP('',(#45955,#45956,#45957,#45958));
#8866=EDGE_LOOP('',(#45959,#45960,#45961,#45962));
#8867=EDGE_LOOP('',(#45963,#45964,#45965,#45966));
#8868=EDGE_LOOP('',(#45967,#45968,#45969,#45970));
#8869=EDGE_LOOP('',(#45971,#45972,#45973,#45974));
#8870=EDGE_LOOP('',(#45975,#45976,#45977,#45978));
#8871=EDGE_LOOP('',(#45979,#45980,#45981,#45982));
#8872=EDGE_LOOP('',(#45983,#45984,#45985,#45986));
#8873=EDGE_LOOP('',(#45987,#45988,#45989,#45990));
#8874=EDGE_LOOP('',(#45991,#45992,#45993,#45994));
#8875=EDGE_LOOP('',(#45995,#45996,#45997,#45998));
#8876=EDGE_LOOP('',(#45999,#46000,#46001,#46002));
#8877=EDGE_LOOP('',(#46003,#46004,#46005,#46006));
#8878=EDGE_LOOP('',(#46007,#46008,#46009,#46010));
#8879=EDGE_LOOP('',(#46011,#46012,#46013,#46014));
#8880=EDGE_LOOP('',(#46015,#46016,#46017,#46018));
#8881=EDGE_LOOP('',(#46019,#46020,#46021,#46022));
#8882=EDGE_LOOP('',(#46023,#46024,#46025,#46026));
#8883=EDGE_LOOP('',(#46027,#46028,#46029,#46030));
#8884=EDGE_LOOP('',(#46031,#46032,#46033,#46034));
#8885=EDGE_LOOP('',(#46035,#46036,#46037,#46038));
#8886=EDGE_LOOP('',(#46039,#46040,#46041,#46042));
#8887=EDGE_LOOP('',(#46043,#46044,#46045,#46046));
#8888=EDGE_LOOP('',(#46047,#46048,#46049,#46050));
#8889=EDGE_LOOP('',(#46051,#46052,#46053,#46054));
#8890=EDGE_LOOP('',(#46055,#46056,#46057,#46058));
#8891=EDGE_LOOP('',(#46059,#46060,#46061,#46062));
#8892=EDGE_LOOP('',(#46063,#46064,#46065,#46066));
#8893=EDGE_LOOP('',(#46067,#46068,#46069,#46070));
#8894=EDGE_LOOP('',(#46071,#46072,#46073,#46074));
#8895=EDGE_LOOP('',(#46075,#46076,#46077,#46078));
#8896=EDGE_LOOP('',(#46079,#46080,#46081,#46082));
#8897=EDGE_LOOP('',(#46083,#46084,#46085,#46086));
#8898=EDGE_LOOP('',(#46087,#46088,#46089,#46090));
#8899=EDGE_LOOP('',(#46091,#46092,#46093,#46094));
#8900=EDGE_LOOP('',(#46095,#46096,#46097,#46098));
#8901=EDGE_LOOP('',(#46099,#46100,#46101,#46102));
#8902=EDGE_LOOP('',(#46103,#46104,#46105,#46106));
#8903=EDGE_LOOP('',(#46107,#46108,#46109,#46110));
#8904=EDGE_LOOP('',(#46111,#46112,#46113,#46114));
#8905=EDGE_LOOP('',(#46115,#46116,#46117,#46118));
#8906=EDGE_LOOP('',(#46119,#46120,#46121,#46122));
#8907=EDGE_LOOP('',(#46123,#46124,#46125,#46126));
#8908=EDGE_LOOP('',(#46127,#46128,#46129,#46130));
#8909=EDGE_LOOP('',(#46131,#46132,#46133,#46134));
#8910=EDGE_LOOP('',(#46135,#46136,#46137,#46138));
#8911=EDGE_LOOP('',(#46139,#46140,#46141,#46142));
#8912=EDGE_LOOP('',(#46143,#46144,#46145,#46146));
#8913=EDGE_LOOP('',(#46147,#46148,#46149,#46150));
#8914=EDGE_LOOP('',(#46151,#46152,#46153,#46154));
#8915=EDGE_LOOP('',(#46155,#46156,#46157,#46158));
#8916=EDGE_LOOP('',(#46159,#46160,#46161,#46162));
#8917=EDGE_LOOP('',(#46163,#46164,#46165,#46166));
#8918=EDGE_LOOP('',(#46167,#46168,#46169,#46170));
#8919=EDGE_LOOP('',(#46171,#46172,#46173,#46174));
#8920=EDGE_LOOP('',(#46175,#46176,#46177,#46178));
#8921=EDGE_LOOP('',(#46179,#46180,#46181,#46182));
#8922=EDGE_LOOP('',(#46183,#46184,#46185,#46186));
#8923=EDGE_LOOP('',(#46187,#46188,#46189,#46190));
#8924=EDGE_LOOP('',(#46191,#46192,#46193,#46194));
#8925=EDGE_LOOP('',(#46195,#46196,#46197,#46198));
#8926=EDGE_LOOP('',(#46199,#46200,#46201,#46202));
#8927=EDGE_LOOP('',(#46203,#46204,#46205,#46206));
#8928=EDGE_LOOP('',(#46207,#46208,#46209,#46210));
#8929=EDGE_LOOP('',(#46211,#46212,#46213,#46214));
#8930=EDGE_LOOP('',(#46215,#46216,#46217,#46218));
#8931=EDGE_LOOP('',(#46219,#46220,#46221,#46222));
#8932=EDGE_LOOP('',(#46223,#46224,#46225,#46226));
#8933=EDGE_LOOP('',(#46227,#46228,#46229,#46230));
#8934=EDGE_LOOP('',(#46231,#46232,#46233,#46234));
#8935=EDGE_LOOP('',(#46235,#46236,#46237,#46238));
#8936=EDGE_LOOP('',(#46239,#46240,#46241,#46242));
#8937=EDGE_LOOP('',(#46243,#46244,#46245,#46246));
#8938=EDGE_LOOP('',(#46247,#46248,#46249,#46250));
#8939=EDGE_LOOP('',(#46251,#46252,#46253,#46254));
#8940=EDGE_LOOP('',(#46255,#46256,#46257,#46258));
#8941=EDGE_LOOP('',(#46259,#46260,#46261,#46262));
#8942=EDGE_LOOP('',(#46263,#46264,#46265,#46266));
#8943=EDGE_LOOP('',(#46267,#46268,#46269,#46270));
#8944=EDGE_LOOP('',(#46271,#46272,#46273,#46274));
#8945=EDGE_LOOP('',(#46275,#46276,#46277,#46278));
#8946=EDGE_LOOP('',(#46279,#46280,#46281,#46282));
#8947=EDGE_LOOP('',(#46283,#46284,#46285,#46286));
#8948=EDGE_LOOP('',(#46287,#46288,#46289,#46290));
#8949=EDGE_LOOP('',(#46291,#46292,#46293,#46294));
#8950=EDGE_LOOP('',(#46295,#46296,#46297,#46298));
#8951=EDGE_LOOP('',(#46299,#46300,#46301,#46302));
#8952=EDGE_LOOP('',(#46303,#46304,#46305,#46306));
#8953=EDGE_LOOP('',(#46307,#46308,#46309,#46310));
#8954=EDGE_LOOP('',(#46311,#46312,#46313,#46314));
#8955=EDGE_LOOP('',(#46315,#46316,#46317,#46318));
#8956=EDGE_LOOP('',(#46319,#46320,#46321,#46322));
#8957=EDGE_LOOP('',(#46323,#46324,#46325,#46326));
#8958=EDGE_LOOP('',(#46327,#46328,#46329,#46330));
#8959=EDGE_LOOP('',(#46331,#46332,#46333,#46334));
#8960=EDGE_LOOP('',(#46335,#46336,#46337,#46338));
#8961=EDGE_LOOP('',(#46339,#46340,#46341,#46342));
#8962=EDGE_LOOP('',(#46343,#46344,#46345,#46346));
#8963=EDGE_LOOP('',(#46347,#46348,#46349,#46350));
#8964=EDGE_LOOP('',(#46351,#46352,#46353,#46354));
#8965=EDGE_LOOP('',(#46355,#46356,#46357,#46358));
#8966=EDGE_LOOP('',(#46359,#46360,#46361,#46362));
#8967=EDGE_LOOP('',(#46363,#46364,#46365,#46366));
#8968=EDGE_LOOP('',(#46367,#46368,#46369,#46370));
#8969=EDGE_LOOP('',(#46371,#46372,#46373,#46374));
#8970=EDGE_LOOP('',(#46375,#46376,#46377,#46378));
#8971=EDGE_LOOP('',(#46379,#46380,#46381,#46382));
#8972=EDGE_LOOP('',(#46383,#46384,#46385,#46386));
#8973=EDGE_LOOP('',(#46387,#46388,#46389,#46390));
#8974=EDGE_LOOP('',(#46391,#46392,#46393,#46394));
#8975=EDGE_LOOP('',(#46395,#46396,#46397,#46398));
#8976=EDGE_LOOP('',(#46399,#46400,#46401,#46402));
#8977=EDGE_LOOP('',(#46403,#46404,#46405,#46406));
#8978=EDGE_LOOP('',(#46407,#46408,#46409,#46410));
#8979=EDGE_LOOP('',(#46411,#46412,#46413,#46414));
#8980=EDGE_LOOP('',(#46415,#46416,#46417,#46418));
#8981=EDGE_LOOP('',(#46419,#46420,#46421,#46422));
#8982=EDGE_LOOP('',(#46423,#46424,#46425,#46426));
#8983=EDGE_LOOP('',(#46427,#46428,#46429,#46430));
#8984=EDGE_LOOP('',(#46431,#46432,#46433,#46434));
#8985=EDGE_LOOP('',(#46435,#46436,#46437,#46438));
#8986=EDGE_LOOP('',(#46439,#46440,#46441,#46442));
#8987=EDGE_LOOP('',(#46443,#46444,#46445,#46446));
#8988=EDGE_LOOP('',(#46447,#46448,#46449,#46450));
#8989=EDGE_LOOP('',(#46451,#46452,#46453,#46454));
#8990=EDGE_LOOP('',(#46455,#46456,#46457,#46458));
#8991=EDGE_LOOP('',(#46459,#46460,#46461,#46462));
#8992=EDGE_LOOP('',(#46463,#46464,#46465,#46466));
#8993=EDGE_LOOP('',(#46467,#46468,#46469,#46470));
#8994=EDGE_LOOP('',(#46471,#46472,#46473,#46474));
#8995=EDGE_LOOP('',(#46475,#46476,#46477,#46478));
#8996=EDGE_LOOP('',(#46479,#46480,#46481,#46482));
#8997=EDGE_LOOP('',(#46483,#46484,#46485,#46486));
#8998=EDGE_LOOP('',(#46487,#46488,#46489,#46490));
#8999=EDGE_LOOP('',(#46491,#46492,#46493,#46494));
#9000=EDGE_LOOP('',(#46495,#46496,#46497,#46498));
#9001=EDGE_LOOP('',(#46499,#46500,#46501,#46502));
#9002=EDGE_LOOP('',(#46503,#46504,#46505,#46506));
#9003=EDGE_LOOP('',(#46507,#46508,#46509,#46510));
#9004=EDGE_LOOP('',(#46511,#46512,#46513,#46514));
#9005=EDGE_LOOP('',(#46515,#46516,#46517,#46518));
#9006=EDGE_LOOP('',(#46519,#46520,#46521,#46522));
#9007=EDGE_LOOP('',(#46523,#46524,#46525,#46526));
#9008=EDGE_LOOP('',(#46527,#46528,#46529,#46530));
#9009=EDGE_LOOP('',(#46531,#46532,#46533,#46534));
#9010=EDGE_LOOP('',(#46535,#46536,#46537,#46538));
#9011=EDGE_LOOP('',(#46539,#46540,#46541,#46542));
#9012=EDGE_LOOP('',(#46543,#46544,#46545,#46546));
#9013=EDGE_LOOP('',(#46547,#46548,#46549,#46550));
#9014=EDGE_LOOP('',(#46551,#46552,#46553,#46554));
#9015=EDGE_LOOP('',(#46555,#46556,#46557,#46558));
#9016=EDGE_LOOP('',(#46559,#46560,#46561,#46562));
#9017=EDGE_LOOP('',(#46563,#46564,#46565,#46566));
#9018=EDGE_LOOP('',(#46567,#46568,#46569,#46570));
#9019=EDGE_LOOP('',(#46571,#46572,#46573,#46574));
#9020=EDGE_LOOP('',(#46575,#46576,#46577,#46578));
#9021=EDGE_LOOP('',(#46579,#46580,#46581,#46582));
#9022=EDGE_LOOP('',(#46583,#46584,#46585,#46586));
#9023=EDGE_LOOP('',(#46587,#46588,#46589,#46590));
#9024=EDGE_LOOP('',(#46591,#46592,#46593,#46594));
#9025=EDGE_LOOP('',(#46595,#46596,#46597,#46598));
#9026=EDGE_LOOP('',(#46599,#46600,#46601,#46602));
#9027=EDGE_LOOP('',(#46603,#46604,#46605,#46606));
#9028=EDGE_LOOP('',(#46607,#46608,#46609,#46610));
#9029=EDGE_LOOP('',(#46611,#46612,#46613,#46614));
#9030=EDGE_LOOP('',(#46615,#46616,#46617,#46618));
#9031=EDGE_LOOP('',(#46619,#46620,#46621,#46622));
#9032=EDGE_LOOP('',(#46623,#46624,#46625,#46626));
#9033=EDGE_LOOP('',(#46627,#46628,#46629,#46630));
#9034=EDGE_LOOP('',(#46631,#46632,#46633,#46634));
#9035=EDGE_LOOP('',(#46635,#46636,#46637,#46638));
#9036=EDGE_LOOP('',(#46639,#46640,#46641,#46642));
#9037=EDGE_LOOP('',(#46643,#46644,#46645,#46646));
#9038=EDGE_LOOP('',(#46647,#46648,#46649,#46650));
#9039=EDGE_LOOP('',(#46651,#46652,#46653,#46654));
#9040=EDGE_LOOP('',(#46655,#46656,#46657,#46658));
#9041=EDGE_LOOP('',(#46659,#46660,#46661,#46662));
#9042=EDGE_LOOP('',(#46663,#46664,#46665,#46666));
#9043=EDGE_LOOP('',(#46667,#46668,#46669,#46670));
#9044=EDGE_LOOP('',(#46671,#46672,#46673,#46674));
#9045=EDGE_LOOP('',(#46675,#46676,#46677,#46678));
#9046=EDGE_LOOP('',(#46679,#46680,#46681,#46682));
#9047=EDGE_LOOP('',(#46683,#46684,#46685,#46686));
#9048=EDGE_LOOP('',(#46687,#46688,#46689,#46690));
#9049=EDGE_LOOP('',(#46691,#46692,#46693,#46694));
#9050=EDGE_LOOP('',(#46695,#46696,#46697,#46698));
#9051=EDGE_LOOP('',(#46699,#46700,#46701,#46702));
#9052=EDGE_LOOP('',(#46703,#46704,#46705,#46706));
#9053=EDGE_LOOP('',(#46707,#46708,#46709,#46710));
#9054=EDGE_LOOP('',(#46711,#46712,#46713,#46714));
#9055=EDGE_LOOP('',(#46715,#46716,#46717,#46718));
#9056=EDGE_LOOP('',(#46719,#46720,#46721,#46722));
#9057=EDGE_LOOP('',(#46723,#46724,#46725,#46726));
#9058=EDGE_LOOP('',(#46727,#46728,#46729,#46730));
#9059=EDGE_LOOP('',(#46731,#46732,#46733,#46734));
#9060=EDGE_LOOP('',(#46735,#46736,#46737,#46738));
#9061=EDGE_LOOP('',(#46739,#46740,#46741,#46742));
#9062=EDGE_LOOP('',(#46743,#46744,#46745,#46746));
#9063=EDGE_LOOP('',(#46747,#46748,#46749,#46750));
#9064=EDGE_LOOP('',(#46751,#46752,#46753,#46754));
#9065=EDGE_LOOP('',(#46755,#46756,#46757,#46758));
#9066=EDGE_LOOP('',(#46759,#46760,#46761,#46762));
#9067=EDGE_LOOP('',(#46763,#46764,#46765,#46766));
#9068=EDGE_LOOP('',(#46767,#46768,#46769,#46770));
#9069=EDGE_LOOP('',(#46771,#46772,#46773,#46774));
#9070=EDGE_LOOP('',(#46775,#46776,#46777,#46778,#46779,#46780));
#9071=EDGE_LOOP('',(#46781,#46782,#46783,#46784,#46785,#46786));
#9072=EDGE_LOOP('',(#46787,#46788,#46789,#46790));
#9073=EDGE_LOOP('',(#46791,#46792,#46793,#46794,#46795,#46796,#46797,#46798,
#46799,#46800,#46801,#46802,#46803,#46804,#46805,#46806,#46807,#46808,#46809,
#46810,#46811,#46812,#46813,#46814));
#9074=EDGE_LOOP('',(#46815,#46816,#46817,#46818));
#9075=EDGE_LOOP('',(#46819,#46820,#46821,#46822));
#9076=EDGE_LOOP('',(#46823,#46824,#46825,#46826));
#9077=EDGE_LOOP('',(#46827,#46828,#46829,#46830));
#9078=EDGE_LOOP('',(#46831));
#9079=EDGE_LOOP('',(#46832));
#9080=EDGE_LOOP('',(#46833));
#9081=EDGE_LOOP('',(#46834,#46835,#46836));
#9082=EDGE_LOOP('',(#46837,#46838,#46839));
#9083=EDGE_LOOP('',(#46840,#46841,#46842,#46843));
#9084=EDGE_LOOP('',(#46844,#46845,#46846,#46847));
#9085=EDGE_LOOP('',(#46848,#46849,#46850,#46851));
#9086=EDGE_LOOP('',(#46852,#46853,#46854,#46855));
#9087=EDGE_LOOP('',(#46856,#46857,#46858,#46859));
#9088=EDGE_LOOP('',(#46860));
#9089=EDGE_LOOP('',(#46861));
#9090=EDGE_LOOP('',(#46862,#46863,#46864));
#9091=EDGE_LOOP('',(#46865,#46866,#46867,#46868));
#9092=EDGE_LOOP('',(#46869,#46870,#46871,#46872));
#9093=EDGE_LOOP('',(#46873,#46874,#46875));
#9094=EDGE_LOOP('',(#46876,#46877,#46878,#46879));
#9095=EDGE_LOOP('',(#46880));
#9096=EDGE_LOOP('',(#46881));
#9097=EDGE_LOOP('',(#46882,#46883,#46884,#46885));
#9098=EDGE_LOOP('',(#46886));
#9099=EDGE_LOOP('',(#46887));
#9100=EDGE_LOOP('',(#46888,#46889,#46890,#46891));
#9101=EDGE_LOOP('',(#46892));
#9102=EDGE_LOOP('',(#46893));
#9103=EDGE_LOOP('',(#46894,#46895,#46896,#46897));
#9104=EDGE_LOOP('',(#46898));
#9105=EDGE_LOOP('',(#46899));
#9106=EDGE_LOOP('',(#46900,#46901,#46902,#46903));
#9107=EDGE_LOOP('',(#46904));
#9108=EDGE_LOOP('',(#46905));
#9109=EDGE_LOOP('',(#46906,#46907,#46908,#46909));
#9110=EDGE_LOOP('',(#46910));
#9111=EDGE_LOOP('',(#46911));
#9112=EDGE_LOOP('',(#46912,#46913,#46914,#46915));
#9113=EDGE_LOOP('',(#46916,#46917,#46918,#46919));
#9114=EDGE_LOOP('',(#46920));
#9115=EDGE_LOOP('',(#46921));
#9116=EDGE_LOOP('',(#46922));
#9117=EDGE_LOOP('',(#46923,#46924,#46925,#46926));
#9118=EDGE_LOOP('',(#46927,#46928,#46929,#46930));
#9119=EDGE_LOOP('',(#46931,#46932,#46933,#46934));
#9120=EDGE_LOOP('',(#46935,#46936,#46937,#46938));
#9121=EDGE_LOOP('',(#46939,#46940,#46941,#46942));
#9122=EDGE_LOOP('',(#46943,#46944,#46945,#46946));
#9123=EDGE_LOOP('',(#46947,#46948,#46949,#46950));
#9124=EDGE_LOOP('',(#46951,#46952,#46953,#46954));
#9125=EDGE_LOOP('',(#46955,#46956,#46957,#46958));
#9126=EDGE_LOOP('',(#46959,#46960,#46961,#46962));
#9127=EDGE_LOOP('',(#46963,#46964,#46965,#46966));
#9128=EDGE_LOOP('',(#46967,#46968,#46969,#46970));
#9129=EDGE_LOOP('',(#46971,#46972,#46973,#46974));
#9130=EDGE_LOOP('',(#46975,#46976,#46977,#46978));
#9131=EDGE_LOOP('',(#46979,#46980,#46981,#46982));
#9132=EDGE_LOOP('',(#46983,#46984,#46985,#46986));
#9133=EDGE_LOOP('',(#46987,#46988,#46989,#46990));
#9134=EDGE_LOOP('',(#46991,#46992,#46993,#46994));
#9135=EDGE_LOOP('',(#46995,#46996,#46997,#46998));
#9136=EDGE_LOOP('',(#46999,#47000,#47001,#47002));
#9137=EDGE_LOOP('',(#47003,#47004,#47005,#47006,#47007,#47008,#47009,#47010));
#9138=EDGE_LOOP('',(#47011,#47012,#47013,#47014));
#9139=EDGE_LOOP('',(#47015,#47016,#47017,#47018));
#9140=EDGE_LOOP('',(#47019,#47020,#47021,#47022));
#9141=EDGE_LOOP('',(#47023,#47024,#47025,#47026));
#9142=EDGE_LOOP('',(#47027,#47028,#47029,#47030));
#9143=EDGE_LOOP('',(#47031,#47032,#47033,#47034));
#9144=EDGE_LOOP('',(#47035,#47036,#47037,#47038));
#9145=EDGE_LOOP('',(#47039,#47040,#47041,#47042));
#9146=EDGE_LOOP('',(#47043,#47044,#47045,#47046));
#9147=EDGE_LOOP('',(#47047,#47048,#47049,#47050));
#9148=EDGE_LOOP('',(#47051,#47052,#47053,#47054));
#9149=EDGE_LOOP('',(#47055,#47056,#47057,#47058));
#9150=EDGE_LOOP('',(#47059,#47060,#47061,#47062));
#9151=EDGE_LOOP('',(#47063,#47064,#47065,#47066));
#9152=EDGE_LOOP('',(#47067));
#9153=EDGE_LOOP('',(#47068));
#9154=EDGE_LOOP('',(#47069));
#9155=EDGE_LOOP('',(#47070));
#9156=EDGE_LOOP('',(#47071,#47072,#47073,#47074));
#9157=EDGE_LOOP('',(#47075,#47076,#47077,#47078));
#9158=EDGE_LOOP('',(#47079,#47080,#47081,#47082));
#9159=EDGE_LOOP('',(#47083,#47084,#47085,#47086));
#9160=EDGE_LOOP('',(#47087,#47088,#47089,#47090));
#9161=EDGE_LOOP('',(#47091,#47092,#47093,#47094,#47095,#47096,#47097,#47098,
#47099,#47100,#47101,#47102));
#9162=EDGE_LOOP('',(#47103,#47104,#47105,#47106,#47107,#47108,#47109,#47110,
#47111,#47112,#47113,#47114,#47115,#47116,#47117,#47118));
#9163=EDGE_LOOP('',(#47119,#47120,#47121,#47122,#47123,#47124,#47125,#47126,
#47127,#47128,#47129,#47130));
#9164=EDGE_LOOP('',(#47131,#47132,#47133,#47134,#47135,#47136,#47137,#47138,
#47139,#47140,#47141,#47142,#47143,#47144,#47145,#47146,#47147,#47148,#47149));
#9165=EDGE_LOOP('',(#47150,#47151,#47152,#47153,#47154,#47155,#47156,#47157,
#47158,#47159,#47160,#47161));
#9166=EDGE_LOOP('',(#47162,#47163,#47164,#47165,#47166,#47167,#47168,#47169,
#47170,#47171,#47172));
#9167=EDGE_LOOP('',(#47173,#47174,#47175,#47176,#47177,#47178,#47179,#47180,
#47181,#47182,#47183,#47184));
#9168=EDGE_LOOP('',(#47185,#47186,#47187,#47188,#47189,#47190,#47191,#47192,
#47193,#47194,#47195,#47196,#47197,#47198,#47199,#47200,#47201,#47202,#47203,
#47204,#47205,#47206));
#9169=EDGE_LOOP('',(#47207,#47208,#47209,#47210,#47211,#47212,#47213,#47214,
#47215,#47216,#47217,#47218));
#9170=EDGE_LOOP('',(#47219,#47220,#47221,#47222,#47223,#47224,#47225,#47226,
#47227,#47228,#47229,#47230));
#9171=EDGE_LOOP('',(#47231,#47232,#47233,#47234,#47235,#47236,#47237,#47238,
#47239,#47240,#47241,#47242,#47243,#47244,#47245,#47246,#47247,#47248,#47249,
#47250,#47251,#47252));
#9172=EDGE_LOOP('',(#47253,#47254,#47255,#47256,#47257,#47258,#47259,#47260,
#47261,#47262,#47263,#47264));
#9173=EDGE_LOOP('',(#47265,#47266,#47267,#47268,#47269,#47270,#47271,#47272,
#47273,#47274,#47275));
#9174=EDGE_LOOP('',(#47276,#47277,#47278,#47279,#47280,#47281,#47282,#47283,
#47284,#47285,#47286,#47287));
#9175=EDGE_LOOP('',(#47288,#47289,#47290,#47291,#47292,#47293,#47294,#47295,
#47296,#47297,#47298,#47299,#47300,#47301,#47302,#47303,#47304,#47305,#47306));
#9176=EDGE_LOOP('',(#47307,#47308,#47309,#47310,#47311,#47312,#47313,#47314,
#47315,#47316,#47317,#47318));
#9177=EDGE_LOOP('',(#47319,#47320,#47321,#47322,#47323,#47324,#47325,#47326,
#47327,#47328,#47329,#47330,#47331,#47332,#47333,#47334));
#9178=EDGE_LOOP('',(#47335,#47336,#47337,#47338));
#9179=EDGE_LOOP('',(#47339,#47340,#47341,#47342));
#9180=EDGE_LOOP('',(#47343,#47344,#47345,#47346));
#9181=EDGE_LOOP('',(#47347,#47348,#47349,#47350));
#9182=EDGE_LOOP('',(#47351,#47352,#47353,#47354));
#9183=EDGE_LOOP('',(#47355,#47356,#47357,#47358));
#9184=EDGE_LOOP('',(#47359,#47360,#47361,#47362));
#9185=EDGE_LOOP('',(#47363,#47364,#47365,#47366));
#9186=EDGE_LOOP('',(#47367,#47368,#47369,#47370));
#9187=EDGE_LOOP('',(#47371,#47372,#47373,#47374));
#9188=EDGE_LOOP('',(#47375,#47376,#47377,#47378));
#9189=EDGE_LOOP('',(#47379,#47380,#47381,#47382));
#9190=EDGE_LOOP('',(#47383,#47384,#47385,#47386));
#9191=EDGE_LOOP('',(#47387,#47388,#47389,#47390));
#9192=EDGE_LOOP('',(#47391,#47392,#47393,#47394));
#9193=EDGE_LOOP('',(#47395,#47396,#47397,#47398));
#9194=EDGE_LOOP('',(#47399,#47400,#47401,#47402));
#9195=EDGE_LOOP('',(#47403,#47404,#47405,#47406));
#9196=EDGE_LOOP('',(#47407,#47408,#47409,#47410));
#9197=EDGE_LOOP('',(#47411,#47412,#47413,#47414));
#9198=EDGE_LOOP('',(#47415,#47416,#47417,#47418));
#9199=EDGE_LOOP('',(#47419,#47420,#47421,#47422));
#9200=EDGE_LOOP('',(#47423,#47424,#47425,#47426));
#9201=EDGE_LOOP('',(#47427,#47428,#47429,#47430));
#9202=EDGE_LOOP('',(#47431,#47432,#47433,#47434));
#9203=EDGE_LOOP('',(#47435,#47436,#47437,#47438));
#9204=EDGE_LOOP('',(#47439,#47440,#47441,#47442));
#9205=EDGE_LOOP('',(#47443,#47444,#47445,#47446));
#9206=EDGE_LOOP('',(#47447,#47448,#47449,#47450));
#9207=EDGE_LOOP('',(#47451,#47452,#47453,#47454));
#9208=EDGE_LOOP('',(#47455,#47456,#47457,#47458));
#9209=EDGE_LOOP('',(#47459,#47460,#47461,#47462));
#9210=EDGE_LOOP('',(#47463,#47464,#47465,#47466));
#9211=EDGE_LOOP('',(#47467,#47468,#47469,#47470));
#9212=EDGE_LOOP('',(#47471,#47472,#47473,#47474));
#9213=EDGE_LOOP('',(#47475,#47476,#47477,#47478));
#9214=EDGE_LOOP('',(#47479,#47480,#47481,#47482));
#9215=EDGE_LOOP('',(#47483,#47484,#47485,#47486));
#9216=EDGE_LOOP('',(#47487,#47488,#47489,#47490));
#9217=EDGE_LOOP('',(#47491,#47492,#47493,#47494));
#9218=EDGE_LOOP('',(#47495,#47496,#47497,#47498));
#9219=EDGE_LOOP('',(#47499,#47500,#47501,#47502));
#9220=EDGE_LOOP('',(#47503,#47504,#47505,#47506));
#9221=EDGE_LOOP('',(#47507,#47508,#47509,#47510));
#9222=EDGE_LOOP('',(#47511,#47512,#47513,#47514));
#9223=EDGE_LOOP('',(#47515,#47516,#47517,#47518));
#9224=EDGE_LOOP('',(#47519,#47520,#47521,#47522));
#9225=EDGE_LOOP('',(#47523,#47524,#47525,#47526));
#9226=EDGE_LOOP('',(#47527,#47528,#47529,#47530));
#9227=EDGE_LOOP('',(#47531,#47532,#47533,#47534));
#9228=EDGE_LOOP('',(#47535,#47536,#47537,#47538));
#9229=EDGE_LOOP('',(#47539,#47540,#47541,#47542));
#9230=EDGE_LOOP('',(#47543,#47544,#47545,#47546));
#9231=EDGE_LOOP('',(#47547,#47548,#47549,#47550));
#9232=EDGE_LOOP('',(#47551,#47552,#47553,#47554));
#9233=EDGE_LOOP('',(#47555,#47556,#47557,#47558));
#9234=EDGE_LOOP('',(#47559,#47560,#47561,#47562));
#9235=EDGE_LOOP('',(#47563,#47564,#47565,#47566));
#9236=EDGE_LOOP('',(#47567,#47568,#47569,#47570));
#9237=EDGE_LOOP('',(#47571,#47572,#47573,#47574));
#9238=EDGE_LOOP('',(#47575,#47576,#47577,#47578));
#9239=EDGE_LOOP('',(#47579,#47580,#47581,#47582));
#9240=EDGE_LOOP('',(#47583,#47584,#47585,#47586));
#9241=EDGE_LOOP('',(#47587,#47588,#47589,#47590));
#9242=EDGE_LOOP('',(#47591,#47592,#47593,#47594));
#9243=EDGE_LOOP('',(#47595,#47596,#47597,#47598));
#9244=EDGE_LOOP('',(#47599,#47600,#47601,#47602));
#9245=EDGE_LOOP('',(#47603,#47604,#47605,#47606));
#9246=EDGE_LOOP('',(#47607,#47608,#47609,#47610));
#9247=EDGE_LOOP('',(#47611,#47612,#47613,#47614));
#9248=EDGE_LOOP('',(#47615,#47616,#47617,#47618));
#9249=EDGE_LOOP('',(#47619,#47620,#47621,#47622));
#9250=EDGE_LOOP('',(#47623,#47624,#47625,#47626));
#9251=EDGE_LOOP('',(#47627,#47628,#47629,#47630));
#9252=EDGE_LOOP('',(#47631,#47632,#47633,#47634));
#9253=EDGE_LOOP('',(#47635,#47636,#47637,#47638));
#9254=EDGE_LOOP('',(#47639,#47640,#47641,#47642));
#9255=EDGE_LOOP('',(#47643,#47644,#47645,#47646));
#9256=EDGE_LOOP('',(#47647,#47648,#47649,#47650));
#9257=EDGE_LOOP('',(#47651,#47652,#47653,#47654));
#9258=EDGE_LOOP('',(#47655,#47656,#47657,#47658));
#9259=EDGE_LOOP('',(#47659,#47660,#47661,#47662));
#9260=EDGE_LOOP('',(#47663,#47664,#47665,#47666));
#9261=EDGE_LOOP('',(#47667,#47668,#47669,#47670));
#9262=EDGE_LOOP('',(#47671,#47672,#47673,#47674));
#9263=EDGE_LOOP('',(#47675,#47676,#47677,#47678));
#9264=EDGE_LOOP('',(#47679,#47680,#47681,#47682));
#9265=EDGE_LOOP('',(#47683,#47684,#47685,#47686));
#9266=EDGE_LOOP('',(#47687,#47688,#47689,#47690));
#9267=EDGE_LOOP('',(#47691,#47692,#47693,#47694));
#9268=EDGE_LOOP('',(#47695,#47696,#47697,#47698));
#9269=EDGE_LOOP('',(#47699,#47700,#47701,#47702));
#9270=EDGE_LOOP('',(#47703,#47704,#47705,#47706));
#9271=EDGE_LOOP('',(#47707,#47708,#47709,#47710));
#9272=EDGE_LOOP('',(#47711,#47712,#47713,#47714));
#9273=EDGE_LOOP('',(#47715,#47716,#47717,#47718));
#9274=EDGE_LOOP('',(#47719,#47720,#47721,#47722));
#9275=EDGE_LOOP('',(#47723,#47724,#47725,#47726));
#9276=EDGE_LOOP('',(#47727,#47728,#47729,#47730));
#9277=EDGE_LOOP('',(#47731,#47732,#47733,#47734));
#9278=EDGE_LOOP('',(#47735,#47736,#47737,#47738));
#9279=EDGE_LOOP('',(#47739,#47740,#47741,#47742));
#9280=EDGE_LOOP('',(#47743,#47744,#47745,#47746));
#9281=EDGE_LOOP('',(#47747,#47748,#47749,#47750));
#9282=EDGE_LOOP('',(#47751,#47752,#47753,#47754));
#9283=EDGE_LOOP('',(#47755,#47756,#47757,#47758));
#9284=EDGE_LOOP('',(#47759,#47760,#47761,#47762));
#9285=EDGE_LOOP('',(#47763,#47764,#47765,#47766));
#9286=EDGE_LOOP('',(#47767,#47768,#47769,#47770));
#9287=EDGE_LOOP('',(#47771,#47772,#47773,#47774));
#9288=EDGE_LOOP('',(#47775,#47776,#47777,#47778));
#9289=EDGE_LOOP('',(#47779,#47780,#47781,#47782));
#9290=EDGE_LOOP('',(#47783,#47784,#47785,#47786));
#9291=EDGE_LOOP('',(#47787,#47788,#47789,#47790));
#9292=EDGE_LOOP('',(#47791,#47792,#47793,#47794));
#9293=EDGE_LOOP('',(#47795,#47796,#47797,#47798));
#9294=EDGE_LOOP('',(#47799,#47800,#47801,#47802));
#9295=EDGE_LOOP('',(#47803,#47804,#47805,#47806));
#9296=EDGE_LOOP('',(#47807,#47808,#47809,#47810));
#9297=EDGE_LOOP('',(#47811,#47812,#47813,#47814));
#9298=EDGE_LOOP('',(#47815,#47816,#47817,#47818));
#9299=EDGE_LOOP('',(#47819,#47820,#47821,#47822));
#9300=EDGE_LOOP('',(#47823,#47824,#47825,#47826));
#9301=EDGE_LOOP('',(#47827,#47828,#47829,#47830));
#9302=EDGE_LOOP('',(#47831,#47832,#47833,#47834));
#9303=EDGE_LOOP('',(#47835,#47836,#47837,#47838));
#9304=EDGE_LOOP('',(#47839,#47840,#47841,#47842));
#9305=EDGE_LOOP('',(#47843,#47844,#47845,#47846));
#9306=EDGE_LOOP('',(#47847,#47848,#47849,#47850));
#9307=EDGE_LOOP('',(#47851,#47852,#47853,#47854));
#9308=EDGE_LOOP('',(#47855,#47856,#47857,#47858));
#9309=EDGE_LOOP('',(#47859,#47860,#47861,#47862));
#9310=EDGE_LOOP('',(#47863,#47864,#47865,#47866));
#9311=EDGE_LOOP('',(#47867,#47868,#47869,#47870));
#9312=EDGE_LOOP('',(#47871,#47872,#47873,#47874));
#9313=EDGE_LOOP('',(#47875,#47876,#47877,#47878));
#9314=EDGE_LOOP('',(#47879,#47880,#47881,#47882));
#9315=EDGE_LOOP('',(#47883,#47884,#47885,#47886));
#9316=EDGE_LOOP('',(#47887,#47888,#47889,#47890));
#9317=EDGE_LOOP('',(#47891,#47892,#47893,#47894));
#9318=EDGE_LOOP('',(#47895,#47896,#47897,#47898));
#9319=EDGE_LOOP('',(#47899,#47900,#47901,#47902));
#9320=EDGE_LOOP('',(#47903,#47904,#47905,#47906));
#9321=EDGE_LOOP('',(#47907,#47908,#47909,#47910));
#9322=EDGE_LOOP('',(#47911,#47912,#47913,#47914));
#9323=EDGE_LOOP('',(#47915,#47916,#47917,#47918));
#9324=EDGE_LOOP('',(#47919,#47920,#47921,#47922));
#9325=EDGE_LOOP('',(#47923,#47924,#47925,#47926));
#9326=EDGE_LOOP('',(#47927,#47928,#47929,#47930));
#9327=EDGE_LOOP('',(#47931,#47932,#47933,#47934));
#9328=EDGE_LOOP('',(#47935,#47936,#47937,#47938));
#9329=EDGE_LOOP('',(#47939,#47940,#47941,#47942));
#9330=EDGE_LOOP('',(#47943,#47944,#47945,#47946));
#9331=EDGE_LOOP('',(#47947,#47948,#47949,#47950));
#9332=EDGE_LOOP('',(#47951,#47952,#47953,#47954));
#9333=EDGE_LOOP('',(#47955,#47956,#47957,#47958));
#9334=EDGE_LOOP('',(#47959,#47960,#47961,#47962));
#9335=EDGE_LOOP('',(#47963,#47964,#47965,#47966));
#9336=EDGE_LOOP('',(#47967,#47968,#47969,#47970));
#9337=EDGE_LOOP('',(#47971,#47972,#47973,#47974));
#9338=EDGE_LOOP('',(#47975,#47976,#47977,#47978));
#9339=EDGE_LOOP('',(#47979,#47980,#47981,#47982));
#9340=EDGE_LOOP('',(#47983,#47984,#47985,#47986));
#9341=EDGE_LOOP('',(#47987,#47988,#47989,#47990));
#9342=EDGE_LOOP('',(#47991,#47992,#47993,#47994));
#9343=EDGE_LOOP('',(#47995,#47996,#47997,#47998));
#9344=EDGE_LOOP('',(#47999,#48000,#48001,#48002));
#9345=EDGE_LOOP('',(#48003,#48004,#48005,#48006));
#9346=EDGE_LOOP('',(#48007,#48008,#48009,#48010));
#9347=EDGE_LOOP('',(#48011,#48012,#48013,#48014));
#9348=EDGE_LOOP('',(#48015,#48016,#48017,#48018));
#9349=EDGE_LOOP('',(#48019,#48020,#48021,#48022));
#9350=EDGE_LOOP('',(#48023,#48024,#48025,#48026));
#9351=EDGE_LOOP('',(#48027,#48028,#48029,#48030));
#9352=EDGE_LOOP('',(#48031,#48032,#48033,#48034));
#9353=EDGE_LOOP('',(#48035,#48036,#48037,#48038));
#9354=EDGE_LOOP('',(#48039,#48040,#48041,#48042));
#9355=EDGE_LOOP('',(#48043,#48044,#48045,#48046));
#9356=EDGE_LOOP('',(#48047,#48048,#48049,#48050));
#9357=EDGE_LOOP('',(#48051,#48052,#48053,#48054));
#9358=EDGE_LOOP('',(#48055,#48056,#48057,#48058));
#9359=EDGE_LOOP('',(#48059,#48060,#48061,#48062,#48063,#48064,#48065,#48066,
#48067,#48068,#48069,#48070,#48071,#48072,#48073,#48074,#48075,#48076,#48077,
#48078,#48079,#48080));
#9360=EDGE_LOOP('',(#48081,#48082,#48083,#48084,#48085,#48086,#48087,#48088,
#48089,#48090,#48091,#48092));
#9361=EDGE_LOOP('',(#48093,#48094,#48095,#48096,#48097,#48098,#48099,#48100,
#48101,#48102,#48103));
#9362=EDGE_LOOP('',(#48104,#48105,#48106,#48107,#48108,#48109,#48110,#48111,
#48112,#48113,#48114,#48115));
#9363=EDGE_LOOP('',(#48116,#48117,#48118,#48119,#48120,#48121,#48122,#48123,
#48124,#48125,#48126,#48127,#48128,#48129,#48130,#48131,#48132,#48133,#48134,
#48135,#48136,#48137));
#9364=EDGE_LOOP('',(#48138,#48139,#48140,#48141,#48142,#48143,#48144,#48145,
#48146,#48147,#48148,#48149));
#9365=EDGE_LOOP('',(#48150,#48151,#48152,#48153,#48154,#48155,#48156,#48157,
#48158,#48159,#48160,#48161,#48162,#48163,#48164,#48165,#48166,#48167,#48168,
#48169,#48170,#48171,#48172,#48173,#48174,#48175,#48176,#48177,#48178,#48179));
#9366=EDGE_LOOP('',(#48180,#48181,#48182,#48183,#48184,#48185,#48186,#48187,
#48188,#48189,#48190,#48191));
#9367=EDGE_LOOP('',(#48192,#48193,#48194,#48195,#48196,#48197,#48198,#48199,
#48200));
#9368=EDGE_LOOP('',(#48201,#48202,#48203,#48204,#48205,#48206,#48207,#48208,
#48209,#48210,#48211,#48212));
#9369=EDGE_LOOP('',(#48213,#48214,#48215,#48216,#48217,#48218,#48219,#48220,
#48221));
#9370=EDGE_LOOP('',(#48222,#48223,#48224,#48225,#48226,#48227,#48228,#48229,
#48230,#48231,#48232,#48233));
#9371=EDGE_LOOP('',(#48234,#48235,#48236,#48237,#48238,#48239,#48240,#48241,
#48242,#48243,#48244,#48245,#48246,#48247,#48248,#48249,#48250,#48251,#48252,
#48253,#48254,#48255,#48256,#48257,#48258,#48259,#48260,#48261,#48262,#48263));
#9372=EDGE_LOOP('',(#48264,#48265,#48266,#48267,#48268,#48269,#48270,#48271,
#48272,#48273,#48274,#48275));
#9373=EDGE_LOOP('',(#48276,#48277,#48278,#48279,#48280,#48281,#48282,#48283,
#48284,#48285,#48286,#48287,#48288,#48289,#48290,#48291,#48292,#48293,#48294,
#48295,#48296,#48297));
#9374=EDGE_LOOP('',(#48298,#48299,#48300,#48301,#48302,#48303,#48304,#48305,
#48306,#48307,#48308,#48309));
#9375=EDGE_LOOP('',(#48310,#48311,#48312,#48313,#48314,#48315,#48316,#48317,
#48318,#48319,#48320));
#9376=EDGE_LOOP('',(#48321,#48322,#48323,#48324,#48325,#48326,#48327,#48328,
#48329,#48330,#48331,#48332));
#9377=EDGE_LOOP('',(#48333,#48334,#48335,#48336,#48337,#48338,#48339,#48340,
#48341,#48342,#48343,#48344,#48345,#48346,#48347,#48348,#48349,#48350,#48351,
#48352,#48353,#48354));
#9378=EDGE_LOOP('',(#48355,#48356,#48357,#48358,#48359,#48360,#48361,#48362,
#48363,#48364,#48365,#48366));
#9379=EDGE_LOOP('',(#48367,#48368,#48369,#48370));
#9380=EDGE_LOOP('',(#48371,#48372,#48373,#48374));
#9381=EDGE_LOOP('',(#48375));
#9382=EDGE_LOOP('',(#48376));
#9383=EDGE_LOOP('',(#48377));
#9384=EDGE_LOOP('',(#48378));
#9385=EDGE_LOOP('',(#48379,#48380,#48381,#48382));
#9386=EDGE_LOOP('',(#48383,#48384,#48385,#48386));
#9387=EDGE_LOOP('',(#48387,#48388,#48389,#48390));
#9388=EDGE_LOOP('',(#48391,#48392,#48393,#48394));
#9389=EDGE_LOOP('',(#48395,#48396,#48397,#48398));
#9390=EDGE_LOOP('',(#48399,#48400,#48401,#48402));
#9391=EDGE_LOOP('',(#48403,#48404,#48405,#48406));
#9392=EDGE_LOOP('',(#48407,#48408,#48409,#48410));
#9393=EDGE_LOOP('',(#48411,#48412,#48413,#48414));
#9394=EDGE_LOOP('',(#48415,#48416,#48417,#48418));
#9395=EDGE_LOOP('',(#48419,#48420,#48421,#48422));
#9396=EDGE_LOOP('',(#48423,#48424,#48425,#48426));
#9397=EDGE_LOOP('',(#48427,#48428,#48429,#48430));
#9398=EDGE_LOOP('',(#48431,#48432,#48433,#48434));
#9399=EDGE_LOOP('',(#48435,#48436,#48437,#48438));
#9400=EDGE_LOOP('',(#48439,#48440,#48441,#48442));
#9401=EDGE_LOOP('',(#48443,#48444,#48445,#48446));
#9402=EDGE_LOOP('',(#48447,#48448,#48449,#48450));
#9403=EDGE_LOOP('',(#48451,#48452,#48453,#48454,#48455,#48456,#48457,#48458,
#48459,#48460,#48461,#48462,#48463,#48464,#48465,#48466,#48467,#48468,#48469,
#48470,#48471,#48472,#48473,#48474));
#9404=EDGE_LOOP('',(#48475,#48476,#48477,#48478));
#9405=EDGE_LOOP('',(#48479,#48480,#48481,#48482,#48483,#48484,#48485,#48486));
#9406=EDGE_LOOP('',(#48487,#48488,#48489,#48490));
#9407=EDGE_LOOP('',(#48491,#48492,#48493,#48494));
#9408=EDGE_LOOP('',(#48495,#48496,#48497,#48498));
#9409=EDGE_LOOP('',(#48499,#48500,#48501,#48502,#48503));
#9410=EDGE_LOOP('',(#48504,#48505,#48506,#48507,#48508,#48509,#48510,#48511,
#48512,#48513));
#9411=EDGE_LOOP('',(#48514));
#9412=EDGE_LOOP('',(#48515,#48516,#48517,#48518));
#9413=EDGE_LOOP('',(#48519,#48520,#48521,#48522,#48523));
#9414=EDGE_LOOP('',(#48524,#48525,#48526,#48527));
#9415=EDGE_LOOP('',(#48528,#48529,#48530));
#9416=EDGE_LOOP('',(#48531,#48532,#48533));
#9417=EDGE_LOOP('',(#48534,#48535,#48536,#48537,#48538,#48539));
#9418=EDGE_LOOP('',(#48540,#48541,#48542,#48543,#48544,#48545,#48546,#48547,
#48548,#48549,#48550));
#9419=EDGE_LOOP('',(#48551,#48552,#48553,#48554));
#9420=EDGE_LOOP('',(#48555,#48556,#48557,#48558,#48559,#48560));
#9421=EDGE_LOOP('',(#48561,#48562,#48563,#48564));
#9422=EDGE_LOOP('',(#48565,#48566,#48567,#48568));
#9423=EDGE_LOOP('',(#48569,#48570,#48571,#48572,#48573));
#9424=EDGE_LOOP('',(#48574,#48575,#48576,#48577,#48578,#48579,#48580,#48581,
#48582,#48583,#48584,#48585,#48586));
#9425=EDGE_LOOP('',(#48587,#48588,#48589,#48590,#48591,#48592));
#9426=EDGE_LOOP('',(#48593,#48594,#48595,#48596,#48597,#48598));
#9427=EDGE_LOOP('',(#48599,#48600,#48601,#48602,#48603,#48604));
#9428=EDGE_LOOP('',(#48605,#48606,#48607,#48608));
#9429=EDGE_LOOP('',(#48609,#48610,#48611,#48612,#48613,#48614,#48615));
#9430=EDGE_LOOP('',(#48616));
#9431=EDGE_LOOP('',(#48617));
#9432=EDGE_LOOP('',(#48618));
#9433=EDGE_LOOP('',(#48619));
#9434=EDGE_LOOP('',(#48620));
#9435=EDGE_LOOP('',(#48621));
#9436=EDGE_LOOP('',(#48622,#48623,#48624,#48625,#48626,#48627));
#9437=EDGE_LOOP('',(#48628,#48629,#48630,#48631));
#9438=EDGE_LOOP('',(#48632,#48633,#48634,#48635,#48636,#48637));
#9439=EDGE_LOOP('',(#48638,#48639));
#9440=EDGE_LOOP('',(#48640,#48641,#48642));
#9441=EDGE_LOOP('',(#48643,#48644));
#9442=EDGE_LOOP('',(#48645,#48646,#48647));
#9443=EDGE_LOOP('',(#48648,#48649));
#9444=EDGE_LOOP('',(#48650,#48651,#48652));
#9445=EDGE_LOOP('',(#48653,#48654,#48655,#48656));
#9446=EDGE_LOOP('',(#48657,#48658,#48659,#48660));
#9447=EDGE_LOOP('',(#48661,#48662,#48663,#48664));
#9448=EDGE_LOOP('',(#48665,#48666,#48667,#48668));
#9449=EDGE_LOOP('',(#48669,#48670,#48671,#48672));
#9450=EDGE_LOOP('',(#48673,#48674,#48675,#48676));
#9451=EDGE_LOOP('',(#48677,#48678,#48679,#48680));
#9452=EDGE_LOOP('',(#48681,#48682,#48683,#48684));
#9453=EDGE_LOOP('',(#48685,#48686,#48687));
#9454=EDGE_LOOP('',(#48688,#48689,#48690));
#9455=EDGE_LOOP('',(#48691,#48692,#48693));
#9456=EDGE_LOOP('',(#48694,#48695,#48696));
#9457=EDGE_LOOP('',(#48697,#48698,#48699,#48700,#48701));
#9458=EDGE_LOOP('',(#48702,#48703,#48704,#48705,#48706,#48707,#48708,#48709,
#48710,#48711,#48712,#48713,#48714,#48715,#48716,#48717,#48718,#48719,#48720,
#48721,#48722));
#9459=EDGE_LOOP('',(#48723,#48724,#48725));
#9460=EDGE_LOOP('',(#48726,#48727,#48728,#48729));
#9461=EDGE_LOOP('',(#48730,#48731,#48732));
#9462=EDGE_LOOP('',(#48733));
#9463=EDGE_LOOP('',(#48734,#48735,#48736,#48737,#48738,#48739,#48740,#48741));
#9464=EDGE_LOOP('',(#48742,#48743,#48744,#48745));
#9465=EDGE_LOOP('',(#48746,#48747,#48748,#48749,#48750,#48751));
#9466=EDGE_LOOP('',(#48752,#48753,#48754,#48755,#48756,#48757,#48758,#48759,
#48760,#48761,#48762,#48763));
#9467=EDGE_LOOP('',(#48764,#48765,#48766,#48767));
#9468=EDGE_LOOP('',(#48768,#48769,#48770,#48771,#48772,#48773));
#9469=EDGE_LOOP('',(#48774,#48775,#48776,#48777,#48778,#48779));
#9470=EDGE_LOOP('',(#48780));
#9471=EDGE_LOOP('',(#48781));
#9472=EDGE_LOOP('',(#48782));
#9473=EDGE_LOOP('',(#48783,#48784,#48785,#48786));
#9474=EDGE_LOOP('',(#48787,#48788,#48789,#48790));
#9475=EDGE_LOOP('',(#48791,#48792,#48793,#48794));
#9476=EDGE_LOOP('',(#48795,#48796,#48797,#48798));
#9477=EDGE_LOOP('',(#48799,#48800,#48801,#48802));
#9478=EDGE_LOOP('',(#48803,#48804,#48805));
#9479=EDGE_LOOP('',(#48806,#48807,#48808));
#9480=EDGE_LOOP('',(#48809,#48810,#48811));
#9481=EDGE_LOOP('',(#48812,#48813,#48814));
#9482=EDGE_LOOP('',(#48815,#48816,#48817));
#9483=EDGE_LOOP('',(#48818,#48819,#48820));
#9484=EDGE_LOOP('',(#48821,#48822,#48823));
#9485=EDGE_LOOP('',(#48824,#48825,#48826));
#9486=EDGE_LOOP('',(#48827,#48828,#48829,#48830));
#9487=EDGE_LOOP('',(#48831,#48832,#48833,#48834));
#9488=EDGE_LOOP('',(#48835,#48836,#48837,#48838));
#9489=EDGE_LOOP('',(#48839,#48840,#48841,#48842));
#9490=EDGE_LOOP('',(#48843,#48844,#48845,#48846));
#9491=EDGE_LOOP('',(#48847,#48848,#48849,#48850));
#9492=EDGE_LOOP('',(#48851,#48852,#48853,#48854));
#9493=EDGE_LOOP('',(#48855,#48856,#48857,#48858,#48859,#48860));
#9494=EDGE_LOOP('',(#48861,#48862,#48863,#48864));
#9495=EDGE_LOOP('',(#48865,#48866,#48867,#48868));
#9496=EDGE_LOOP('',(#48869,#48870,#48871,#48872,#48873,#48874,#48875,#48876,
#48877,#48878,#48879,#48880));
#9497=EDGE_LOOP('',(#48881,#48882,#48883));
#9498=EDGE_LOOP('',(#48884,#48885,#48886));
#9499=EDGE_LOOP('',(#48887,#48888,#48889));
#9500=EDGE_LOOP('',(#48890,#48891,#48892,#48893));
#9501=EDGE_LOOP('',(#48894,#48895,#48896,#48897));
#9502=EDGE_LOOP('',(#48898,#48899,#48900,#48901));
#9503=EDGE_LOOP('',(#48902,#48903,#48904,#48905));
#9504=EDGE_LOOP('',(#48906,#48907,#48908,#48909));
#9505=EDGE_LOOP('',(#48910,#48911,#48912,#48913));
#9506=EDGE_LOOP('',(#48914,#48915,#48916,#48917));
#9507=EDGE_LOOP('',(#48918,#48919,#48920,#48921));
#9508=EDGE_LOOP('',(#48922,#48923,#48924,#48925));
#9509=EDGE_LOOP('',(#48926,#48927,#48928,#48929));
#9510=EDGE_LOOP('',(#48930,#48931,#48932,#48933));
#9511=EDGE_LOOP('',(#48934,#48935,#48936,#48937));
#9512=EDGE_LOOP('',(#48938));
#9513=EDGE_LOOP('',(#48939));
#9514=EDGE_LOOP('',(#48940));
#9515=EDGE_LOOP('',(#48941,#48942,#48943,#48944));
#9516=EDGE_LOOP('',(#48945,#48946,#48947,#48948));
#9517=EDGE_LOOP('',(#48949,#48950));
#9518=EDGE_LOOP('',(#48951,#48952));
#9519=EDGE_LOOP('',(#48953,#48954,#48955,#48956));
#9520=EDGE_LOOP('',(#48957,#48958));
#9521=EDGE_LOOP('',(#48959,#48960));
#9522=EDGE_LOOP('',(#48961,#48962,#48963,#48964));
#9523=EDGE_LOOP('',(#48965));
#9524=EDGE_LOOP('',(#48966,#48967,#48968,#48969));
#9525=EDGE_LOOP('',(#48970,#48971,#48972,#48973));
#9526=EDGE_LOOP('',(#48974,#48975,#48976,#48977));
#9527=EDGE_LOOP('',(#48978,#48979,#48980,#48981));
#9528=EDGE_LOOP('',(#48982,#48983,#48984,#48985));
#9529=EDGE_LOOP('',(#48986));
#9530=EDGE_LOOP('',(#48987,#48988));
#9531=EDGE_LOOP('',(#48989,#48990,#48991,#48992,#48993,#48994,#48995,#48996,
#48997,#48998));
#9532=EDGE_LOOP('',(#48999,#49000,#49001));
#9533=EDGE_LOOP('',(#49002,#49003,#49004,#49005));
#9534=EDGE_LOOP('',(#49006,#49007,#49008,#49009));
#9535=EDGE_LOOP('',(#49010,#49011,#49012,#49013));
#9536=EDGE_LOOP('',(#49014,#49015,#49016,#49017));
#9537=EDGE_LOOP('',(#49018,#49019,#49020,#49021));
#9538=EDGE_LOOP('',(#49022,#49023,#49024,#49025,#49026,#49027));
#9539=EDGE_LOOP('',(#49028,#49029,#49030,#49031,#49032,#49033,#49034,#49035,
#49036,#49037,#49038,#49039,#49040,#49041,#49042,#49043,#49044,#49045,#49046,
#49047,#49048,#49049,#49050,#49051,#49052,#49053,#49054,#49055,#49056,#49057,
#49058,#49059,#49060,#49061,#49062,#49063,#49064,#49065,#49066,#49067,#49068,
#49069,#49070,#49071,#49072,#49073,#49074,#49075,#49076,#49077,#49078,#49079,
#49080,#49081,#49082,#49083,#49084,#49085,#49086,#49087,#49088,#49089,#49090,
#49091,#49092,#49093,#49094,#49095));
#9540=EDGE_LOOP('',(#49096,#49097,#49098,#49099));
#9541=EDGE_LOOP('',(#49100,#49101,#49102,#49103));
#9542=EDGE_LOOP('',(#49104,#49105,#49106,#49107));
#9543=EDGE_LOOP('',(#49108,#49109,#49110,#49111));
#9544=EDGE_LOOP('',(#49112,#49113,#49114,#49115));
#9545=EDGE_LOOP('',(#49116,#49117,#49118,#49119,#49120,#49121));
#9546=EDGE_LOOP('',(#49122,#49123,#49124,#49125));
#9547=EDGE_LOOP('',(#49126,#49127,#49128,#49129));
#9548=EDGE_LOOP('',(#49130,#49131,#49132,#49133));
#9549=EDGE_LOOP('',(#49134,#49135,#49136,#49137));
#9550=EDGE_LOOP('',(#49138,#49139,#49140,#49141));
#9551=EDGE_LOOP('',(#49142,#49143,#49144,#49145,#49146,#49147));
#9552=EDGE_LOOP('',(#49148,#49149,#49150,#49151));
#9553=EDGE_LOOP('',(#49152,#49153,#49154,#49155));
#9554=EDGE_LOOP('',(#49156,#49157,#49158,#49159));
#9555=EDGE_LOOP('',(#49160,#49161,#49162,#49163));
#9556=EDGE_LOOP('',(#49164,#49165,#49166,#49167));
#9557=EDGE_LOOP('',(#49168,#49169,#49170,#49171,#49172,#49173,#49174));
#9558=EDGE_LOOP('',(#49175,#49176,#49177,#49178));
#9559=EDGE_LOOP('',(#49179,#49180,#49181,#49182));
#9560=EDGE_LOOP('',(#49183,#49184,#49185,#49186));
#9561=EDGE_LOOP('',(#49187,#49188,#49189,#49190));
#9562=EDGE_LOOP('',(#49191,#49192,#49193,#49194));
#9563=EDGE_LOOP('',(#49195,#49196,#49197,#49198,#49199,#49200));
#9564=EDGE_LOOP('',(#49201,#49202,#49203,#49204));
#9565=EDGE_LOOP('',(#49205,#49206,#49207,#49208));
#9566=EDGE_LOOP('',(#49209,#49210,#49211,#49212));
#9567=EDGE_LOOP('',(#49213,#49214,#49215,#49216));
#9568=EDGE_LOOP('',(#49217,#49218,#49219,#49220));
#9569=EDGE_LOOP('',(#49221,#49222,#49223,#49224,#49225,#49226));
#9570=EDGE_LOOP('',(#49227,#49228,#49229,#49230));
#9571=EDGE_LOOP('',(#49231,#49232,#49233,#49234));
#9572=EDGE_LOOP('',(#49235,#49236,#49237,#49238));
#9573=EDGE_LOOP('',(#49239,#49240,#49241,#49242));
#9574=EDGE_LOOP('',(#49243,#49244,#49245,#49246));
#9575=EDGE_LOOP('',(#49247,#49248,#49249,#49250,#49251,#49252));
#9576=EDGE_LOOP('',(#49253,#49254,#49255,#49256));
#9577=EDGE_LOOP('',(#49257,#49258,#49259,#49260));
#9578=EDGE_LOOP('',(#49261,#49262,#49263,#49264));
#9579=EDGE_LOOP('',(#49265,#49266,#49267,#49268));
#9580=EDGE_LOOP('',(#49269,#49270,#49271,#49272));
#9581=EDGE_LOOP('',(#49273,#49274,#49275,#49276,#49277,#49278));
#9582=EDGE_LOOP('',(#49279,#49280,#49281,#49282));
#9583=EDGE_LOOP('',(#49283,#49284,#49285,#49286));
#9584=EDGE_LOOP('',(#49287,#49288,#49289,#49290));
#9585=EDGE_LOOP('',(#49291,#49292,#49293,#49294));
#9586=EDGE_LOOP('',(#49295,#49296,#49297,#49298));
#9587=EDGE_LOOP('',(#49299,#49300,#49301,#49302,#49303,#49304));
#9588=EDGE_LOOP('',(#49305,#49306,#49307,#49308));
#9589=EDGE_LOOP('',(#49309,#49310,#49311,#49312));
#9590=EDGE_LOOP('',(#49313,#49314,#49315,#49316));
#9591=EDGE_LOOP('',(#49317,#49318,#49319,#49320));
#9592=EDGE_LOOP('',(#49321,#49322,#49323,#49324));
#9593=EDGE_LOOP('',(#49325,#49326,#49327,#49328,#49329,#49330));
#9594=EDGE_LOOP('',(#49331,#49332,#49333,#49334));
#9595=EDGE_LOOP('',(#49335,#49336,#49337,#49338));
#9596=EDGE_LOOP('',(#49339,#49340,#49341,#49342));
#9597=EDGE_LOOP('',(#49343,#49344,#49345,#49346));
#9598=EDGE_LOOP('',(#49347,#49348,#49349,#49350));
#9599=EDGE_LOOP('',(#49351,#49352,#49353,#49354,#49355,#49356));
#9600=EDGE_LOOP('',(#49357,#49358,#49359,#49360));
#9601=EDGE_LOOP('',(#49361,#49362,#49363,#49364));
#9602=EDGE_LOOP('',(#49365,#49366,#49367,#49368));
#9603=EDGE_LOOP('',(#49369,#49370,#49371,#49372));
#9604=EDGE_LOOP('',(#49373,#49374,#49375,#49376));
#9605=EDGE_LOOP('',(#49377,#49378,#49379,#49380,#49381,#49382));
#9606=EDGE_LOOP('',(#49383,#49384,#49385,#49386));
#9607=EDGE_LOOP('',(#49387,#49388,#49389,#49390));
#9608=EDGE_LOOP('',(#49391,#49392,#49393,#49394));
#9609=EDGE_LOOP('',(#49395,#49396,#49397,#49398));
#9610=EDGE_LOOP('',(#49399,#49400,#49401,#49402));
#9611=EDGE_LOOP('',(#49403,#49404,#49405,#49406,#49407,#49408));
#9612=EDGE_LOOP('',(#49409,#49410,#49411,#49412));
#9613=EDGE_LOOP('',(#49413,#49414,#49415,#49416));
#9614=EDGE_LOOP('',(#49417,#49418,#49419,#49420));
#9615=EDGE_LOOP('',(#49421,#49422,#49423,#49424));
#9616=EDGE_LOOP('',(#49425,#49426,#49427,#49428));
#9617=EDGE_LOOP('',(#49429,#49430,#49431,#49432,#49433,#49434));
#9618=EDGE_LOOP('',(#49435,#49436,#49437,#49438));
#9619=EDGE_LOOP('',(#49439,#49440,#49441,#49442));
#9620=EDGE_LOOP('',(#49443,#49444,#49445,#49446));
#9621=EDGE_LOOP('',(#49447,#49448,#49449,#49450));
#9622=EDGE_LOOP('',(#49451,#49452,#49453,#49454));
#9623=EDGE_LOOP('',(#49455,#49456,#49457,#49458,#49459,#49460));
#9624=EDGE_LOOP('',(#49461,#49462,#49463,#49464));
#9625=EDGE_LOOP('',(#49465,#49466,#49467,#49468));
#9626=EDGE_LOOP('',(#49469,#49470,#49471,#49472));
#9627=EDGE_LOOP('',(#49473,#49474,#49475,#49476));
#9628=EDGE_LOOP('',(#49477,#49478,#49479,#49480));
#9629=EDGE_LOOP('',(#49481,#49482,#49483,#49484,#49485,#49486));
#9630=EDGE_LOOP('',(#49487,#49488,#49489,#49490));
#9631=EDGE_LOOP('',(#49491,#49492,#49493,#49494));
#9632=EDGE_LOOP('',(#49495,#49496,#49497,#49498,#49499,#49500,#49501,#49502,
#49503,#49504,#49505,#49506,#49507,#49508,#49509,#49510,#49511,#49512,#49513,
#49514,#49515,#49516,#49517,#49518,#49519,#49520,#49521,#49522,#49523,#49524,
#49525,#49526,#49527,#49528,#49529,#49530,#49531,#49532,#49533,#49534,#49535,
#49536,#49537,#49538,#49539,#49540,#49541,#49542,#49543,#49544,#49545,#49546,
#49547,#49548,#49549,#49550,#49551,#49552,#49553,#49554,#49555,#49556,#49557,
#49558,#49559,#49560,#49561,#49562,#49563,#49564,#49565,#49566,#49567,#49568,
#49569,#49570,#49571,#49572,#49573,#49574,#49575,#49576,#49577,#49578,#49579,
#49580,#49581,#49582,#49583,#49584,#49585,#49586,#49587,#49588,#49589,#49590));
#9633=EDGE_LOOP('',(#49591));
#9634=EDGE_LOOP('',(#49592));
#9635=EDGE_LOOP('',(#49593));
#9636=EDGE_LOOP('',(#49594,#49595,#49596,#49597));
#9637=EDGE_LOOP('',(#49598,#49599,#49600));
#9638=EDGE_LOOP('',(#49601,#49602,#49603,#49604));
#9639=EDGE_LOOP('',(#49605));
#9640=EDGE_LOOP('',(#49606));
#9641=EDGE_LOOP('',(#49607,#49608,#49609));
#9642=EDGE_LOOP('',(#49610,#49611,#49612,#49613,#49614,#49615,#49616,#49617,
#49618,#49619));
#9643=EDGE_LOOP('',(#49620,#49621));
#9644=EDGE_LOOP('',(#49622,#49623,#49624,#49625));
#9645=EDGE_LOOP('',(#49626,#49627,#49628,#49629));
#9646=EDGE_LOOP('',(#49630,#49631,#49632,#49633,#49634,#49635,#49636,#49637,
#49638,#49639,#49640,#49641,#49642,#49643,#49644,#49645,#49646,#49647,#49648,
#49649,#49650,#49651,#49652,#49653,#49654,#49655,#49656,#49657,#49658,#49659,
#49660,#49661,#49662,#49663,#49664,#49665,#49666,#49667,#49668,#49669,#49670,
#49671,#49672,#49673,#49674,#49675,#49676,#49677,#49678,#49679,#49680,#49681,
#49682,#49683,#49684,#49685,#49686,#49687,#49688,#49689,#49690,#49691,#49692,
#49693,#49694,#49695,#49696,#49697,#49698,#49699,#49700,#49701,#49702,#49703,
#49704,#49705,#49706,#49707,#49708,#49709,#49710,#49711,#49712,#49713,#49714,
#49715,#49716,#49717,#49718,#49719,#49720,#49721,#49722,#49723,#49724,#49725,
#49726,#49727,#49728,#49729,#49730,#49731,#49732,#49733,#49734,#49735,#49736,
#49737,#49738,#49739,#49740,#49741,#49742,#49743,#49744,#49745,#49746,#49747,
#49748,#49749,#49750,#49751,#49752));
#9647=EDGE_LOOP('',(#49753,#49754,#49755,#49756));
#9648=EDGE_LOOP('',(#49757,#49758,#49759,#49760));
#9649=EDGE_LOOP('',(#49761,#49762,#49763,#49764));
#9650=EDGE_LOOP('',(#49765,#49766,#49767,#49768));
#9651=EDGE_LOOP('',(#49769,#49770,#49771,#49772));
#9652=EDGE_LOOP('',(#49773,#49774,#49775,#49776,#49777,#49778,#49779,#49780,
#49781,#49782,#49783,#49784,#49785,#49786,#49787,#49788,#49789,#49790,#49791,
#49792,#49793,#49794,#49795,#49796,#49797,#49798,#49799,#49800,#49801,#49802,
#49803,#49804,#49805,#49806,#49807,#49808,#49809,#49810,#49811,#49812,#49813,
#49814,#49815,#49816,#49817,#49818,#49819,#49820,#49821,#49822,#49823,#49824,
#49825,#49826,#49827,#49828,#49829,#49830,#49831,#49832,#49833,#49834,#49835,
#49836,#49837,#49838,#49839,#49840,#49841,#49842,#49843,#49844,#49845,#49846,
#49847,#49848,#49849,#49850,#49851,#49852,#49853,#49854,#49855,#49856,#49857,
#49858,#49859,#49860,#49861,#49862,#49863,#49864,#49865,#49866,#49867,#49868,
#49869,#49870,#49871,#49872,#49873,#49874,#49875,#49876,#49877,#49878,#49879,
#49880,#49881,#49882,#49883,#49884,#49885,#49886,#49887,#49888,#49889,#49890,
#49891,#49892,#49893,#49894,#49895));
#9653=EDGE_LOOP('',(#49896,#49897,#49898,#49899));
#9654=EDGE_LOOP('',(#49900,#49901,#49902,#49903));
#9655=EDGE_LOOP('',(#49904,#49905,#49906,#49907));
#9656=EDGE_LOOP('',(#49908,#49909,#49910,#49911));
#9657=EDGE_LOOP('',(#49912,#49913,#49914,#49915));
#9658=EDGE_LOOP('',(#49916,#49917,#49918,#49919));
#9659=EDGE_LOOP('',(#49920,#49921,#49922,#49923));
#9660=EDGE_LOOP('',(#49924,#49925,#49926,#49927));
#9661=EDGE_LOOP('',(#49928,#49929,#49930,#49931));
#9662=EDGE_LOOP('',(#49932,#49933,#49934,#49935));
#9663=EDGE_LOOP('',(#49936,#49937,#49938,#49939));
#9664=EDGE_LOOP('',(#49940,#49941,#49942,#49943));
#9665=EDGE_LOOP('',(#49944,#49945,#49946,#49947));
#9666=EDGE_LOOP('',(#49948,#49949,#49950,#49951));
#9667=EDGE_LOOP('',(#49952,#49953,#49954,#49955));
#9668=EDGE_LOOP('',(#49956,#49957,#49958,#49959));
#9669=EDGE_LOOP('',(#49960,#49961,#49962,#49963));
#9670=EDGE_LOOP('',(#49964,#49965,#49966,#49967));
#9671=EDGE_LOOP('',(#49968,#49969,#49970,#49971));
#9672=EDGE_LOOP('',(#49972,#49973,#49974,#49975));
#9673=EDGE_LOOP('',(#49976,#49977,#49978,#49979));
#9674=EDGE_LOOP('',(#49980,#49981,#49982,#49983));
#9675=EDGE_LOOP('',(#49984,#49985,#49986,#49987));
#9676=EDGE_LOOP('',(#49988,#49989,#49990,#49991));
#9677=EDGE_LOOP('',(#49992,#49993,#49994,#49995));
#9678=EDGE_LOOP('',(#49996,#49997,#49998,#49999));
#9679=EDGE_LOOP('',(#50000,#50001,#50002,#50003));
#9680=EDGE_LOOP('',(#50004,#50005,#50006,#50007));
#9681=EDGE_LOOP('',(#50008,#50009,#50010,#50011));
#9682=EDGE_LOOP('',(#50012,#50013,#50014,#50015));
#9683=EDGE_LOOP('',(#50016,#50017,#50018,#50019));
#9684=EDGE_LOOP('',(#50020,#50021,#50022,#50023));
#9685=EDGE_LOOP('',(#50024,#50025,#50026,#50027));
#9686=EDGE_LOOP('',(#50028,#50029,#50030,#50031));
#9687=EDGE_LOOP('',(#50032,#50033,#50034,#50035));
#9688=EDGE_LOOP('',(#50036,#50037,#50038,#50039));
#9689=EDGE_LOOP('',(#50040,#50041,#50042,#50043));
#9690=EDGE_LOOP('',(#50044,#50045,#50046,#50047));
#9691=EDGE_LOOP('',(#50048,#50049,#50050,#50051));
#9692=EDGE_LOOP('',(#50052,#50053,#50054,#50055));
#9693=EDGE_LOOP('',(#50056,#50057,#50058,#50059));
#9694=EDGE_LOOP('',(#50060,#50061,#50062,#50063));
#9695=EDGE_LOOP('',(#50064,#50065,#50066,#50067));
#9696=EDGE_LOOP('',(#50068,#50069,#50070,#50071));
#9697=EDGE_LOOP('',(#50072,#50073,#50074,#50075));
#9698=EDGE_LOOP('',(#50076,#50077,#50078,#50079));
#9699=EDGE_LOOP('',(#50080,#50081,#50082,#50083));
#9700=EDGE_LOOP('',(#50084,#50085,#50086,#50087));
#9701=EDGE_LOOP('',(#50088,#50089,#50090,#50091));
#9702=EDGE_LOOP('',(#50092,#50093,#50094,#50095));
#9703=EDGE_LOOP('',(#50096,#50097,#50098,#50099));
#9704=EDGE_LOOP('',(#50100,#50101,#50102,#50103));
#9705=EDGE_LOOP('',(#50104,#50105,#50106,#50107));
#9706=EDGE_LOOP('',(#50108,#50109,#50110,#50111));
#9707=EDGE_LOOP('',(#50112,#50113,#50114,#50115));
#9708=EDGE_LOOP('',(#50116,#50117,#50118,#50119));
#9709=EDGE_LOOP('',(#50120,#50121,#50122,#50123));
#9710=EDGE_LOOP('',(#50124,#50125,#50126,#50127));
#9711=EDGE_LOOP('',(#50128,#50129,#50130,#50131));
#9712=EDGE_LOOP('',(#50132,#50133,#50134,#50135));
#9713=EDGE_LOOP('',(#50136,#50137,#50138,#50139));
#9714=EDGE_LOOP('',(#50140,#50141,#50142,#50143));
#9715=EDGE_LOOP('',(#50144,#50145,#50146,#50147));
#9716=EDGE_LOOP('',(#50148,#50149,#50150,#50151));
#9717=EDGE_LOOP('',(#50152,#50153,#50154,#50155));
#9718=EDGE_LOOP('',(#50156,#50157,#50158,#50159));
#9719=EDGE_LOOP('',(#50160,#50161,#50162,#50163));
#9720=EDGE_LOOP('',(#50164,#50165,#50166,#50167));
#9721=EDGE_LOOP('',(#50168,#50169,#50170,#50171));
#9722=EDGE_LOOP('',(#50172,#50173,#50174,#50175));
#9723=EDGE_LOOP('',(#50176,#50177,#50178,#50179));
#9724=EDGE_LOOP('',(#50180,#50181,#50182,#50183));
#9725=EDGE_LOOP('',(#50184,#50185,#50186,#50187));
#9726=EDGE_LOOP('',(#50188,#50189,#50190,#50191));
#9727=EDGE_LOOP('',(#50192,#50193,#50194,#50195));
#9728=EDGE_LOOP('',(#50196,#50197,#50198,#50199));
#9729=EDGE_LOOP('',(#50200,#50201,#50202,#50203));
#9730=EDGE_LOOP('',(#50204,#50205,#50206,#50207));
#9731=EDGE_LOOP('',(#50208,#50209,#50210,#50211));
#9732=EDGE_LOOP('',(#50212,#50213,#50214,#50215));
#9733=EDGE_LOOP('',(#50216,#50217,#50218,#50219));
#9734=EDGE_LOOP('',(#50220,#50221,#50222,#50223));
#9735=EDGE_LOOP('',(#50224,#50225,#50226,#50227));
#9736=EDGE_LOOP('',(#50228,#50229,#50230,#50231));
#9737=EDGE_LOOP('',(#50232,#50233,#50234,#50235));
#9738=EDGE_LOOP('',(#50236,#50237,#50238,#50239));
#9739=EDGE_LOOP('',(#50240,#50241,#50242,#50243));
#9740=EDGE_LOOP('',(#50244,#50245,#50246,#50247));
#9741=EDGE_LOOP('',(#50248,#50249,#50250,#50251));
#9742=EDGE_LOOP('',(#50252,#50253,#50254,#50255));
#9743=EDGE_LOOP('',(#50256,#50257,#50258,#50259));
#9744=EDGE_LOOP('',(#50260,#50261,#50262,#50263));
#9745=EDGE_LOOP('',(#50264,#50265,#50266,#50267));
#9746=EDGE_LOOP('',(#50268,#50269,#50270,#50271));
#9747=EDGE_LOOP('',(#50272,#50273,#50274,#50275));
#9748=EDGE_LOOP('',(#50276,#50277,#50278,#50279));
#9749=EDGE_LOOP('',(#50280,#50281,#50282,#50283));
#9750=EDGE_LOOP('',(#50284,#50285,#50286,#50287));
#9751=EDGE_LOOP('',(#50288,#50289,#50290,#50291));
#9752=EDGE_LOOP('',(#50292,#50293,#50294,#50295));
#9753=EDGE_LOOP('',(#50296,#50297,#50298,#50299));
#9754=EDGE_LOOP('',(#50300,#50301,#50302,#50303));
#9755=EDGE_LOOP('',(#50304,#50305,#50306,#50307));
#9756=EDGE_LOOP('',(#50308,#50309,#50310,#50311));
#9757=EDGE_LOOP('',(#50312,#50313,#50314,#50315));
#9758=EDGE_LOOP('',(#50316,#50317,#50318,#50319));
#9759=EDGE_LOOP('',(#50320,#50321,#50322,#50323));
#9760=EDGE_LOOP('',(#50324,#50325,#50326,#50327));
#9761=EDGE_LOOP('',(#50328,#50329,#50330,#50331));
#9762=EDGE_LOOP('',(#50332,#50333,#50334,#50335));
#9763=EDGE_LOOP('',(#50336,#50337,#50338,#50339));
#9764=EDGE_LOOP('',(#50340,#50341,#50342,#50343));
#9765=EDGE_LOOP('',(#50344,#50345,#50346,#50347));
#9766=EDGE_LOOP('',(#50348));
#9767=EDGE_LOOP('',(#50349));
#9768=EDGE_LOOP('',(#50350,#50351,#50352,#50353));
#9769=EDGE_LOOP('',(#50354,#50355,#50356,#50357));
#9770=EDGE_LOOP('',(#50358,#50359,#50360,#50361));
#9771=EDGE_LOOP('',(#50362));
#9772=EDGE_LOOP('',(#50363));
#9773=EDGE_LOOP('',(#50364,#50365,#50366,#50367));
#9774=EDGE_LOOP('',(#50368,#50369,#50370));
#9775=EDGE_LOOP('',(#50371,#50372,#50373,#50374));
#9776=EDGE_LOOP('',(#50375));
#9777=EDGE_LOOP('',(#50376));
#9778=EDGE_LOOP('',(#50377,#50378,#50379,#50380));
#9779=EDGE_LOOP('',(#50381));
#9780=EDGE_LOOP('',(#50382));
#9781=EDGE_LOOP('',(#50383,#50384,#50385,#50386));
#9782=EDGE_LOOP('',(#50387));
#9783=EDGE_LOOP('',(#50388,#50389,#50390));
#9784=EDGE_LOOP('',(#50391,#50392,#50393,#50394));
#9785=EDGE_LOOP('',(#50395,#50396,#50397,#50398));
#9786=EDGE_LOOP('',(#50399,#50400,#50401,#50402));
#9787=EDGE_LOOP('',(#50403));
#9788=EDGE_LOOP('',(#50404));
#9789=EDGE_LOOP('',(#50405,#50406,#50407,#50408));
#9790=EDGE_LOOP('',(#50409,#50410,#50411,#50412));
#9791=EDGE_LOOP('',(#50413));
#9792=EDGE_LOOP('',(#50414));
#9793=EDGE_LOOP('',(#50415,#50416,#50417,#50418));
#9794=EDGE_LOOP('',(#50419,#50420,#50421,#50422));
#9795=EDGE_LOOP('',(#50423));
#9796=EDGE_LOOP('',(#50424));
#9797=EDGE_LOOP('',(#50425,#50426,#50427,#50428));
#9798=EDGE_LOOP('',(#50429,#50430,#50431,#50432));
#9799=EDGE_LOOP('',(#50433,#50434,#50435,#50436));
#9800=EDGE_LOOP('',(#50437,#50438,#50439,#50440));
#9801=EDGE_LOOP('',(#50441,#50442,#50443,#50444));
#9802=EDGE_LOOP('',(#50445));
#9803=EDGE_LOOP('',(#50446,#50447,#50448,#50449));
#9804=EDGE_LOOP('',(#50450,#50451,#50452,#50453));
#9805=EDGE_LOOP('',(#50454,#50455,#50456,#50457));
#9806=EDGE_LOOP('',(#50458));
#9807=EDGE_LOOP('',(#50459));
#9808=EDGE_LOOP('',(#50460));
#9809=EDGE_LOOP('',(#50461));
#9810=EDGE_LOOP('',(#50462));
#9811=EDGE_LOOP('',(#50463,#50464,#50465,#50466));
#9812=EDGE_LOOP('',(#50467,#50468,#50469,#50470));
#9813=EDGE_LOOP('',(#50471,#50472,#50473,#50474));
#9814=EDGE_LOOP('',(#50475,#50476,#50477,#50478,#50479,#50480));
#9815=EDGE_LOOP('',(#50481,#50482,#50483,#50484));
#9816=EDGE_LOOP('',(#50485));
#9817=EDGE_LOOP('',(#50486));
#9818=EDGE_LOOP('',(#50487,#50488,#50489,#50490));
#9819=EDGE_LOOP('',(#50491,#50492,#50493,#50494));
#9820=EDGE_LOOP('',(#50495,#50496,#50497,#50498));
#9821=EDGE_LOOP('',(#50499,#50500,#50501,#50502));
#9822=EDGE_LOOP('',(#50503,#50504,#50505,#50506));
#9823=EDGE_LOOP('',(#50507,#50508,#50509,#50510));
#9824=EDGE_LOOP('',(#50511,#50512,#50513,#50514));
#9825=EDGE_LOOP('',(#50515,#50516,#50517,#50518));
#9826=EDGE_LOOP('',(#50519,#50520,#50521,#50522));
#9827=EDGE_LOOP('',(#50523,#50524,#50525,#50526));
#9828=EDGE_LOOP('',(#50527,#50528,#50529,#50530));
#9829=EDGE_LOOP('',(#50531,#50532,#50533,#50534));
#9830=EDGE_LOOP('',(#50535,#50536,#50537,#50538));
#9831=EDGE_LOOP('',(#50539,#50540,#50541,#50542));
#9832=EDGE_LOOP('',(#50543,#50544,#50545,#50546));
#9833=EDGE_LOOP('',(#50547,#50548,#50549,#50550));
#9834=EDGE_LOOP('',(#50551,#50552,#50553,#50554));
#9835=EDGE_LOOP('',(#50555,#50556,#50557,#50558));
#9836=EDGE_LOOP('',(#50559,#50560,#50561,#50562));
#9837=EDGE_LOOP('',(#50563,#50564,#50565,#50566));
#9838=EDGE_LOOP('',(#50567,#50568,#50569,#50570));
#9839=EDGE_LOOP('',(#50571,#50572,#50573,#50574));
#9840=EDGE_LOOP('',(#50575,#50576,#50577,#50578));
#9841=EDGE_LOOP('',(#50579,#50580,#50581,#50582));
#9842=EDGE_LOOP('',(#50583,#50584,#50585,#50586));
#9843=EDGE_LOOP('',(#50587,#50588,#50589,#50590));
#9844=EDGE_LOOP('',(#50591,#50592,#50593,#50594));
#9845=EDGE_LOOP('',(#50595,#50596,#50597,#50598));
#9846=EDGE_LOOP('',(#50599,#50600,#50601,#50602));
#9847=EDGE_LOOP('',(#50603,#50604,#50605,#50606));
#9848=EDGE_LOOP('',(#50607,#50608,#50609,#50610));
#9849=EDGE_LOOP('',(#50611,#50612,#50613,#50614));
#9850=EDGE_LOOP('',(#50615,#50616,#50617,#50618));
#9851=EDGE_LOOP('',(#50619,#50620,#50621,#50622));
#9852=EDGE_LOOP('',(#50623,#50624,#50625,#50626));
#9853=EDGE_LOOP('',(#50627,#50628,#50629,#50630));
#9854=EDGE_LOOP('',(#50631,#50632,#50633,#50634));
#9855=EDGE_LOOP('',(#50635,#50636,#50637,#50638));
#9856=EDGE_LOOP('',(#50639,#50640,#50641,#50642));
#9857=EDGE_LOOP('',(#50643,#50644,#50645,#50646));
#9858=EDGE_LOOP('',(#50647,#50648,#50649,#50650));
#9859=EDGE_LOOP('',(#50651,#50652,#50653,#50654));
#9860=EDGE_LOOP('',(#50655,#50656,#50657,#50658));
#9861=EDGE_LOOP('',(#50659,#50660,#50661,#50662));
#9862=EDGE_LOOP('',(#50663,#50664,#50665,#50666));
#9863=EDGE_LOOP('',(#50667,#50668,#50669,#50670));
#9864=EDGE_LOOP('',(#50671,#50672,#50673,#50674));
#9865=EDGE_LOOP('',(#50675,#50676,#50677,#50678));
#9866=EDGE_LOOP('',(#50679,#50680,#50681,#50682));
#9867=EDGE_LOOP('',(#50683,#50684,#50685,#50686));
#9868=EDGE_LOOP('',(#50687,#50688,#50689,#50690));
#9869=EDGE_LOOP('',(#50691,#50692,#50693,#50694));
#9870=EDGE_LOOP('',(#50695,#50696,#50697,#50698));
#9871=EDGE_LOOP('',(#50699,#50700,#50701,#50702));
#9872=EDGE_LOOP('',(#50703,#50704,#50705,#50706));
#9873=EDGE_LOOP('',(#50707,#50708,#50709,#50710));
#9874=EDGE_LOOP('',(#50711,#50712,#50713,#50714));
#9875=EDGE_LOOP('',(#50715,#50716,#50717,#50718));
#9876=EDGE_LOOP('',(#50719,#50720,#50721,#50722));
#9877=EDGE_LOOP('',(#50723,#50724,#50725,#50726));
#9878=EDGE_LOOP('',(#50727,#50728,#50729,#50730));
#9879=EDGE_LOOP('',(#50731,#50732,#50733,#50734));
#9880=EDGE_LOOP('',(#50735,#50736,#50737,#50738));
#9881=EDGE_LOOP('',(#50739,#50740,#50741,#50742));
#9882=EDGE_LOOP('',(#50743,#50744,#50745,#50746));
#9883=EDGE_LOOP('',(#50747,#50748,#50749,#50750));
#9884=EDGE_LOOP('',(#50751,#50752,#50753,#50754));
#9885=EDGE_LOOP('',(#50755,#50756,#50757,#50758));
#9886=EDGE_LOOP('',(#50759,#50760,#50761,#50762));
#9887=EDGE_LOOP('',(#50763,#50764,#50765,#50766));
#9888=EDGE_LOOP('',(#50767,#50768,#50769,#50770));
#9889=EDGE_LOOP('',(#50771,#50772,#50773,#50774));
#9890=EDGE_LOOP('',(#50775,#50776,#50777,#50778));
#9891=EDGE_LOOP('',(#50779,#50780,#50781,#50782));
#9892=EDGE_LOOP('',(#50783,#50784,#50785,#50786));
#9893=EDGE_LOOP('',(#50787,#50788,#50789,#50790));
#9894=EDGE_LOOP('',(#50791,#50792,#50793,#50794));
#9895=EDGE_LOOP('',(#50795,#50796,#50797,#50798));
#9896=EDGE_LOOP('',(#50799,#50800,#50801,#50802));
#9897=EDGE_LOOP('',(#50803,#50804,#50805,#50806));
#9898=EDGE_LOOP('',(#50807,#50808,#50809,#50810));
#9899=EDGE_LOOP('',(#50811,#50812,#50813,#50814));
#9900=EDGE_LOOP('',(#50815,#50816,#50817,#50818));
#9901=EDGE_LOOP('',(#50819,#50820,#50821,#50822));
#9902=EDGE_LOOP('',(#50823,#50824,#50825,#50826));
#9903=EDGE_LOOP('',(#50827,#50828,#50829,#50830));
#9904=EDGE_LOOP('',(#50831,#50832,#50833,#50834));
#9905=EDGE_LOOP('',(#50835,#50836,#50837,#50838));
#9906=EDGE_LOOP('',(#50839,#50840,#50841,#50842));
#9907=EDGE_LOOP('',(#50843,#50844,#50845,#50846));
#9908=EDGE_LOOP('',(#50847,#50848,#50849,#50850));
#9909=EDGE_LOOP('',(#50851,#50852,#50853,#50854));
#9910=EDGE_LOOP('',(#50855,#50856,#50857,#50858));
#9911=EDGE_LOOP('',(#50859,#50860,#50861,#50862));
#9912=EDGE_LOOP('',(#50863,#50864,#50865,#50866));
#9913=EDGE_LOOP('',(#50867,#50868,#50869,#50870));
#9914=EDGE_LOOP('',(#50871,#50872,#50873,#50874));
#9915=EDGE_LOOP('',(#50875,#50876,#50877,#50878));
#9916=EDGE_LOOP('',(#50879,#50880,#50881,#50882));
#9917=EDGE_LOOP('',(#50883,#50884,#50885,#50886));
#9918=EDGE_LOOP('',(#50887,#50888,#50889,#50890));
#9919=EDGE_LOOP('',(#50891,#50892,#50893,#50894));
#9920=EDGE_LOOP('',(#50895,#50896,#50897,#50898));
#9921=EDGE_LOOP('',(#50899,#50900,#50901,#50902));
#9922=EDGE_LOOP('',(#50903,#50904,#50905,#50906));
#9923=EDGE_LOOP('',(#50907,#50908,#50909,#50910));
#9924=EDGE_LOOP('',(#50911,#50912,#50913,#50914));
#9925=EDGE_LOOP('',(#50915,#50916,#50917,#50918));
#9926=EDGE_LOOP('',(#50919,#50920,#50921,#50922));
#9927=EDGE_LOOP('',(#50923,#50924,#50925,#50926));
#9928=EDGE_LOOP('',(#50927,#50928,#50929,#50930));
#9929=EDGE_LOOP('',(#50931,#50932,#50933,#50934));
#9930=EDGE_LOOP('',(#50935,#50936,#50937,#50938));
#9931=EDGE_LOOP('',(#50939,#50940,#50941,#50942));
#9932=EDGE_LOOP('',(#50943,#50944,#50945,#50946));
#9933=EDGE_LOOP('',(#50947,#50948,#50949,#50950));
#9934=EDGE_LOOP('',(#50951,#50952,#50953,#50954));
#9935=EDGE_LOOP('',(#50955,#50956,#50957,#50958));
#9936=EDGE_LOOP('',(#50959,#50960,#50961,#50962));
#9937=EDGE_LOOP('',(#50963,#50964,#50965,#50966));
#9938=EDGE_LOOP('',(#50967,#50968,#50969,#50970));
#9939=EDGE_LOOP('',(#50971,#50972,#50973,#50974));
#9940=EDGE_LOOP('',(#50975,#50976,#50977,#50978));
#9941=EDGE_LOOP('',(#50979,#50980,#50981,#50982));
#9942=EDGE_LOOP('',(#50983,#50984,#50985,#50986));
#9943=EDGE_LOOP('',(#50987,#50988,#50989,#50990));
#9944=EDGE_LOOP('',(#50991,#50992,#50993,#50994));
#9945=EDGE_LOOP('',(#50995,#50996,#50997,#50998));
#9946=EDGE_LOOP('',(#50999,#51000,#51001,#51002));
#9947=EDGE_LOOP('',(#51003,#51004,#51005,#51006));
#9948=EDGE_LOOP('',(#51007,#51008,#51009,#51010));
#9949=EDGE_LOOP('',(#51011,#51012,#51013,#51014));
#9950=EDGE_LOOP('',(#51015,#51016,#51017,#51018));
#9951=EDGE_LOOP('',(#51019,#51020,#51021,#51022));
#9952=EDGE_LOOP('',(#51023,#51024,#51025,#51026));
#9953=EDGE_LOOP('',(#51027,#51028,#51029,#51030));
#9954=EDGE_LOOP('',(#51031,#51032,#51033,#51034));
#9955=EDGE_LOOP('',(#51035,#51036,#51037,#51038));
#9956=EDGE_LOOP('',(#51039,#51040,#51041,#51042));
#9957=EDGE_LOOP('',(#51043,#51044,#51045,#51046));
#9958=EDGE_LOOP('',(#51047,#51048,#51049,#51050));
#9959=EDGE_LOOP('',(#51051,#51052,#51053,#51054));
#9960=EDGE_LOOP('',(#51055,#51056,#51057,#51058));
#9961=EDGE_LOOP('',(#51059,#51060,#51061,#51062));
#9962=EDGE_LOOP('',(#51063,#51064,#51065,#51066));
#9963=EDGE_LOOP('',(#51067,#51068,#51069,#51070));
#9964=EDGE_LOOP('',(#51071,#51072,#51073,#51074));
#9965=EDGE_LOOP('',(#51075,#51076,#51077,#51078));
#9966=EDGE_LOOP('',(#51079,#51080,#51081,#51082));
#9967=EDGE_LOOP('',(#51083,#51084,#51085,#51086));
#9968=EDGE_LOOP('',(#51087,#51088,#51089,#51090));
#9969=EDGE_LOOP('',(#51091,#51092,#51093,#51094));
#9970=EDGE_LOOP('',(#51095,#51096,#51097,#51098));
#9971=EDGE_LOOP('',(#51099,#51100,#51101,#51102));
#9972=EDGE_LOOP('',(#51103,#51104,#51105,#51106));
#9973=EDGE_LOOP('',(#51107,#51108,#51109,#51110));
#9974=EDGE_LOOP('',(#51111,#51112,#51113,#51114));
#9975=EDGE_LOOP('',(#51115,#51116,#51117,#51118));
#9976=EDGE_LOOP('',(#51119,#51120,#51121,#51122));
#9977=EDGE_LOOP('',(#51123,#51124,#51125,#51126));
#9978=EDGE_LOOP('',(#51127,#51128,#51129,#51130));
#9979=EDGE_LOOP('',(#51131,#51132,#51133,#51134));
#9980=EDGE_LOOP('',(#51135,#51136,#51137,#51138));
#9981=EDGE_LOOP('',(#51139,#51140,#51141,#51142));
#9982=EDGE_LOOP('',(#51143,#51144,#51145,#51146));
#9983=EDGE_LOOP('',(#51147,#51148,#51149,#51150));
#9984=EDGE_LOOP('',(#51151,#51152,#51153,#51154));
#9985=EDGE_LOOP('',(#51155,#51156,#51157,#51158));
#9986=EDGE_LOOP('',(#51159,#51160,#51161,#51162));
#9987=EDGE_LOOP('',(#51163,#51164,#51165,#51166));
#9988=EDGE_LOOP('',(#51167,#51168,#51169,#51170));
#9989=EDGE_LOOP('',(#51171,#51172,#51173,#51174));
#9990=EDGE_LOOP('',(#51175,#51176,#51177,#51178));
#9991=EDGE_LOOP('',(#51179,#51180,#51181,#51182));
#9992=EDGE_LOOP('',(#51183,#51184,#51185,#51186));
#9993=EDGE_LOOP('',(#51187,#51188,#51189,#51190));
#9994=EDGE_LOOP('',(#51191,#51192,#51193,#51194));
#9995=EDGE_LOOP('',(#51195,#51196,#51197,#51198));
#9996=EDGE_LOOP('',(#51199,#51200,#51201,#51202));
#9997=EDGE_LOOP('',(#51203,#51204,#51205,#51206));
#9998=EDGE_LOOP('',(#51207,#51208,#51209,#51210));
#9999=EDGE_LOOP('',(#51211,#51212,#51213,#51214));
#10000=EDGE_LOOP('',(#51215,#51216,#51217,#51218));
#10001=EDGE_LOOP('',(#51219,#51220,#51221,#51222));
#10002=EDGE_LOOP('',(#51223,#51224,#51225,#51226));
#10003=EDGE_LOOP('',(#51227,#51228,#51229,#51230));
#10004=EDGE_LOOP('',(#51231,#51232,#51233,#51234));
#10005=EDGE_LOOP('',(#51235,#51236,#51237,#51238));
#10006=EDGE_LOOP('',(#51239,#51240,#51241,#51242));
#10007=EDGE_LOOP('',(#51243,#51244,#51245,#51246));
#10008=EDGE_LOOP('',(#51247,#51248,#51249,#51250));
#10009=EDGE_LOOP('',(#51251,#51252,#51253,#51254));
#10010=EDGE_LOOP('',(#51255,#51256,#51257,#51258));
#10011=EDGE_LOOP('',(#51259,#51260,#51261,#51262));
#10012=EDGE_LOOP('',(#51263,#51264,#51265,#51266));
#10013=EDGE_LOOP('',(#51267,#51268,#51269,#51270));
#10014=EDGE_LOOP('',(#51271,#51272,#51273,#51274));
#10015=EDGE_LOOP('',(#51275,#51276,#51277,#51278));
#10016=EDGE_LOOP('',(#51279,#51280,#51281,#51282));
#10017=EDGE_LOOP('',(#51283,#51284,#51285,#51286));
#10018=EDGE_LOOP('',(#51287,#51288,#51289,#51290));
#10019=EDGE_LOOP('',(#51291,#51292,#51293,#51294));
#10020=EDGE_LOOP('',(#51295,#51296,#51297,#51298));
#10021=EDGE_LOOP('',(#51299,#51300,#51301,#51302));
#10022=EDGE_LOOP('',(#51303,#51304,#51305,#51306));
#10023=EDGE_LOOP('',(#51307,#51308,#51309,#51310));
#10024=EDGE_LOOP('',(#51311,#51312,#51313,#51314));
#10025=EDGE_LOOP('',(#51315,#51316,#51317,#51318));
#10026=EDGE_LOOP('',(#51319,#51320,#51321,#51322));
#10027=EDGE_LOOP('',(#51323,#51324,#51325,#51326));
#10028=EDGE_LOOP('',(#51327,#51328,#51329,#51330));
#10029=EDGE_LOOP('',(#51331,#51332,#51333,#51334));
#10030=EDGE_LOOP('',(#51335,#51336,#51337,#51338));
#10031=EDGE_LOOP('',(#51339,#51340,#51341,#51342));
#10032=EDGE_LOOP('',(#51343,#51344,#51345,#51346));
#10033=EDGE_LOOP('',(#51347,#51348,#51349,#51350));
#10034=EDGE_LOOP('',(#51351,#51352,#51353,#51354));
#10035=EDGE_LOOP('',(#51355,#51356,#51357,#51358));
#10036=EDGE_LOOP('',(#51359,#51360,#51361,#51362));
#10037=EDGE_LOOP('',(#51363,#51364,#51365,#51366));
#10038=EDGE_LOOP('',(#51367,#51368,#51369,#51370));
#10039=EDGE_LOOP('',(#51371,#51372,#51373,#51374));
#10040=EDGE_LOOP('',(#51375,#51376,#51377,#51378));
#10041=EDGE_LOOP('',(#51379,#51380,#51381,#51382));
#10042=EDGE_LOOP('',(#51383,#51384,#51385,#51386));
#10043=EDGE_LOOP('',(#51387,#51388,#51389,#51390));
#10044=EDGE_LOOP('',(#51391,#51392,#51393,#51394));
#10045=EDGE_LOOP('',(#51395,#51396,#51397,#51398));
#10046=EDGE_LOOP('',(#51399,#51400,#51401,#51402));
#10047=EDGE_LOOP('',(#51403,#51404,#51405,#51406));
#10048=EDGE_LOOP('',(#51407,#51408,#51409,#51410));
#10049=EDGE_LOOP('',(#51411,#51412,#51413,#51414));
#10050=EDGE_LOOP('',(#51415,#51416,#51417,#51418));
#10051=EDGE_LOOP('',(#51419,#51420,#51421,#51422));
#10052=EDGE_LOOP('',(#51423,#51424,#51425,#51426));
#10053=EDGE_LOOP('',(#51427,#51428,#51429,#51430));
#10054=EDGE_LOOP('',(#51431,#51432,#51433,#51434));
#10055=EDGE_LOOP('',(#51435,#51436,#51437,#51438));
#10056=EDGE_LOOP('',(#51439,#51440,#51441,#51442));
#10057=EDGE_LOOP('',(#51443,#51444,#51445,#51446));
#10058=EDGE_LOOP('',(#51447,#51448,#51449,#51450));
#10059=EDGE_LOOP('',(#51451,#51452,#51453,#51454));
#10060=EDGE_LOOP('',(#51455,#51456,#51457,#51458));
#10061=EDGE_LOOP('',(#51459,#51460,#51461,#51462));
#10062=EDGE_LOOP('',(#51463,#51464,#51465,#51466));
#10063=EDGE_LOOP('',(#51467,#51468,#51469,#51470));
#10064=EDGE_LOOP('',(#51471,#51472,#51473,#51474));
#10065=EDGE_LOOP('',(#51475,#51476,#51477,#51478));
#10066=EDGE_LOOP('',(#51479,#51480,#51481,#51482));
#10067=EDGE_LOOP('',(#51483,#51484,#51485,#51486));
#10068=EDGE_LOOP('',(#51487,#51488,#51489,#51490));
#10069=EDGE_LOOP('',(#51491,#51492,#51493,#51494));
#10070=EDGE_LOOP('',(#51495,#51496,#51497,#51498));
#10071=EDGE_LOOP('',(#51499,#51500,#51501,#51502));
#10072=EDGE_LOOP('',(#51503,#51504,#51505,#51506));
#10073=EDGE_LOOP('',(#51507,#51508,#51509,#51510));
#10074=EDGE_LOOP('',(#51511,#51512,#51513,#51514));
#10075=EDGE_LOOP('',(#51515,#51516,#51517,#51518));
#10076=EDGE_LOOP('',(#51519,#51520,#51521,#51522));
#10077=EDGE_LOOP('',(#51523,#51524,#51525,#51526));
#10078=EDGE_LOOP('',(#51527,#51528,#51529,#51530));
#10079=EDGE_LOOP('',(#51531,#51532,#51533,#51534));
#10080=EDGE_LOOP('',(#51535,#51536,#51537,#51538));
#10081=EDGE_LOOP('',(#51539,#51540,#51541,#51542));
#10082=EDGE_LOOP('',(#51543,#51544,#51545,#51546));
#10083=EDGE_LOOP('',(#51547,#51548,#51549,#51550));
#10084=EDGE_LOOP('',(#51551,#51552,#51553,#51554));
#10085=EDGE_LOOP('',(#51555,#51556,#51557,#51558));
#10086=EDGE_LOOP('',(#51559,#51560,#51561,#51562));
#10087=EDGE_LOOP('',(#51563,#51564,#51565,#51566));
#10088=EDGE_LOOP('',(#51567,#51568,#51569,#51570));
#10089=EDGE_LOOP('',(#51571,#51572,#51573,#51574));
#10090=EDGE_LOOP('',(#51575,#51576,#51577,#51578));
#10091=EDGE_LOOP('',(#51579,#51580,#51581,#51582));
#10092=EDGE_LOOP('',(#51583,#51584,#51585,#51586));
#10093=EDGE_LOOP('',(#51587,#51588,#51589,#51590));
#10094=EDGE_LOOP('',(#51591,#51592,#51593,#51594));
#10095=EDGE_LOOP('',(#51595,#51596,#51597,#51598));
#10096=EDGE_LOOP('',(#51599,#51600,#51601,#51602));
#10097=EDGE_LOOP('',(#51603,#51604,#51605,#51606));
#10098=EDGE_LOOP('',(#51607,#51608,#51609,#51610));
#10099=EDGE_LOOP('',(#51611,#51612,#51613,#51614));
#10100=EDGE_LOOP('',(#51615,#51616,#51617,#51618));
#10101=EDGE_LOOP('',(#51619,#51620,#51621,#51622));
#10102=EDGE_LOOP('',(#51623,#51624,#51625,#51626));
#10103=EDGE_LOOP('',(#51627,#51628,#51629,#51630));
#10104=EDGE_LOOP('',(#51631,#51632,#51633,#51634));
#10105=EDGE_LOOP('',(#51635,#51636,#51637,#51638));
#10106=EDGE_LOOP('',(#51639,#51640,#51641,#51642));
#10107=EDGE_LOOP('',(#51643,#51644,#51645,#51646));
#10108=EDGE_LOOP('',(#51647,#51648,#51649,#51650));
#10109=EDGE_LOOP('',(#51651,#51652,#51653,#51654));
#10110=EDGE_LOOP('',(#51655,#51656,#51657,#51658));
#10111=EDGE_LOOP('',(#51659,#51660,#51661,#51662));
#10112=EDGE_LOOP('',(#51663,#51664,#51665,#51666));
#10113=EDGE_LOOP('',(#51667,#51668,#51669,#51670));
#10114=EDGE_LOOP('',(#51671,#51672,#51673,#51674));
#10115=EDGE_LOOP('',(#51675,#51676,#51677,#51678));
#10116=EDGE_LOOP('',(#51679,#51680,#51681,#51682));
#10117=EDGE_LOOP('',(#51683,#51684,#51685,#51686));
#10118=EDGE_LOOP('',(#51687,#51688,#51689,#51690));
#10119=EDGE_LOOP('',(#51691,#51692,#51693,#51694));
#10120=EDGE_LOOP('',(#51695,#51696,#51697,#51698));
#10121=EDGE_LOOP('',(#51699,#51700,#51701,#51702));
#10122=EDGE_LOOP('',(#51703,#51704,#51705,#51706));
#10123=EDGE_LOOP('',(#51707,#51708,#51709,#51710));
#10124=EDGE_LOOP('',(#51711,#51712,#51713,#51714));
#10125=EDGE_LOOP('',(#51715,#51716,#51717,#51718));
#10126=EDGE_LOOP('',(#51719,#51720,#51721,#51722));
#10127=EDGE_LOOP('',(#51723,#51724,#51725,#51726));
#10128=EDGE_LOOP('',(#51727,#51728,#51729,#51730));
#10129=EDGE_LOOP('',(#51731,#51732,#51733,#51734));
#10130=EDGE_LOOP('',(#51735,#51736,#51737,#51738));
#10131=EDGE_LOOP('',(#51739,#51740,#51741,#51742));
#10132=EDGE_LOOP('',(#51743,#51744,#51745,#51746));
#10133=EDGE_LOOP('',(#51747,#51748,#51749,#51750));
#10134=EDGE_LOOP('',(#51751,#51752,#51753,#51754));
#10135=EDGE_LOOP('',(#51755,#51756,#51757,#51758));
#10136=EDGE_LOOP('',(#51759,#51760,#51761,#51762));
#10137=EDGE_LOOP('',(#51763,#51764,#51765,#51766));
#10138=EDGE_LOOP('',(#51767,#51768,#51769,#51770));
#10139=EDGE_LOOP('',(#51771,#51772,#51773,#51774));
#10140=EDGE_LOOP('',(#51775,#51776,#51777,#51778));
#10141=EDGE_LOOP('',(#51779,#51780,#51781,#51782));
#10142=EDGE_LOOP('',(#51783,#51784,#51785,#51786));
#10143=EDGE_LOOP('',(#51787,#51788,#51789,#51790));
#10144=EDGE_LOOP('',(#51791,#51792,#51793,#51794));
#10145=EDGE_LOOP('',(#51795,#51796,#51797,#51798));
#10146=EDGE_LOOP('',(#51799,#51800,#51801,#51802));
#10147=EDGE_LOOP('',(#51803,#51804,#51805,#51806));
#10148=EDGE_LOOP('',(#51807,#51808,#51809,#51810));
#10149=EDGE_LOOP('',(#51811,#51812,#51813,#51814));
#10150=EDGE_LOOP('',(#51815,#51816,#51817,#51818));
#10151=EDGE_LOOP('',(#51819,#51820,#51821,#51822));
#10152=EDGE_LOOP('',(#51823,#51824,#51825,#51826));
#10153=EDGE_LOOP('',(#51827,#51828,#51829,#51830));
#10154=EDGE_LOOP('',(#51831,#51832,#51833,#51834));
#10155=EDGE_LOOP('',(#51835,#51836,#51837,#51838));
#10156=EDGE_LOOP('',(#51839,#51840,#51841,#51842));
#10157=EDGE_LOOP('',(#51843,#51844,#51845,#51846));
#10158=EDGE_LOOP('',(#51847,#51848,#51849,#51850));
#10159=EDGE_LOOP('',(#51851,#51852,#51853,#51854));
#10160=EDGE_LOOP('',(#51855,#51856,#51857,#51858));
#10161=EDGE_LOOP('',(#51859,#51860,#51861,#51862));
#10162=EDGE_LOOP('',(#51863,#51864,#51865,#51866));
#10163=EDGE_LOOP('',(#51867,#51868,#51869,#51870));
#10164=EDGE_LOOP('',(#51871,#51872,#51873,#51874));
#10165=EDGE_LOOP('',(#51875,#51876,#51877,#51878));
#10166=EDGE_LOOP('',(#51879,#51880,#51881,#51882));
#10167=EDGE_LOOP('',(#51883,#51884,#51885,#51886));
#10168=EDGE_LOOP('',(#51887,#51888,#51889,#51890));
#10169=EDGE_LOOP('',(#51891,#51892,#51893,#51894));
#10170=EDGE_LOOP('',(#51895,#51896,#51897,#51898));
#10171=EDGE_LOOP('',(#51899,#51900,#51901,#51902));
#10172=EDGE_LOOP('',(#51903,#51904,#51905,#51906));
#10173=EDGE_LOOP('',(#51907,#51908,#51909,#51910));
#10174=EDGE_LOOP('',(#51911,#51912,#51913,#51914));
#10175=EDGE_LOOP('',(#51915,#51916,#51917,#51918));
#10176=EDGE_LOOP('',(#51919,#51920,#51921,#51922));
#10177=EDGE_LOOP('',(#51923,#51924,#51925,#51926));
#10178=EDGE_LOOP('',(#51927,#51928,#51929,#51930));
#10179=EDGE_LOOP('',(#51931,#51932,#51933,#51934));
#10180=EDGE_LOOP('',(#51935,#51936,#51937,#51938));
#10181=EDGE_LOOP('',(#51939,#51940,#51941,#51942));
#10182=EDGE_LOOP('',(#51943,#51944,#51945,#51946));
#10183=EDGE_LOOP('',(#51947,#51948,#51949,#51950));
#10184=EDGE_LOOP('',(#51951,#51952,#51953,#51954));
#10185=EDGE_LOOP('',(#51955,#51956,#51957,#51958));
#10186=EDGE_LOOP('',(#51959,#51960,#51961,#51962));
#10187=EDGE_LOOP('',(#51963,#51964,#51965,#51966));
#10188=EDGE_LOOP('',(#51967,#51968,#51969,#51970));
#10189=EDGE_LOOP('',(#51971,#51972,#51973,#51974));
#10190=EDGE_LOOP('',(#51975,#51976,#51977,#51978));
#10191=EDGE_LOOP('',(#51979,#51980,#51981,#51982));
#10192=EDGE_LOOP('',(#51983,#51984,#51985,#51986));
#10193=EDGE_LOOP('',(#51987,#51988,#51989,#51990));
#10194=EDGE_LOOP('',(#51991,#51992,#51993,#51994));
#10195=EDGE_LOOP('',(#51995,#51996,#51997,#51998));
#10196=EDGE_LOOP('',(#51999,#52000,#52001,#52002));
#10197=EDGE_LOOP('',(#52003,#52004,#52005,#52006));
#10198=EDGE_LOOP('',(#52007,#52008,#52009,#52010));
#10199=EDGE_LOOP('',(#52011,#52012,#52013,#52014));
#10200=EDGE_LOOP('',(#52015,#52016,#52017,#52018));
#10201=EDGE_LOOP('',(#52019,#52020,#52021,#52022));
#10202=EDGE_LOOP('',(#52023,#52024,#52025,#52026));
#10203=EDGE_LOOP('',(#52027,#52028,#52029,#52030));
#10204=EDGE_LOOP('',(#52031,#52032,#52033,#52034));
#10205=EDGE_LOOP('',(#52035,#52036,#52037,#52038));
#10206=EDGE_LOOP('',(#52039,#52040,#52041,#52042));
#10207=EDGE_LOOP('',(#52043,#52044,#52045,#52046));
#10208=EDGE_LOOP('',(#52047,#52048,#52049,#52050));
#10209=EDGE_LOOP('',(#52051,#52052,#52053,#52054));
#10210=EDGE_LOOP('',(#52055,#52056,#52057,#52058));
#10211=EDGE_LOOP('',(#52059,#52060,#52061,#52062));
#10212=EDGE_LOOP('',(#52063,#52064,#52065,#52066));
#10213=EDGE_LOOP('',(#52067,#52068,#52069,#52070));
#10214=EDGE_LOOP('',(#52071,#52072,#52073,#52074));
#10215=EDGE_LOOP('',(#52075,#52076,#52077,#52078));
#10216=EDGE_LOOP('',(#52079,#52080,#52081,#52082));
#10217=EDGE_LOOP('',(#52083,#52084,#52085,#52086));
#10218=EDGE_LOOP('',(#52087,#52088,#52089,#52090));
#10219=EDGE_LOOP('',(#52091,#52092,#52093,#52094));
#10220=EDGE_LOOP('',(#52095,#52096,#52097,#52098));
#10221=EDGE_LOOP('',(#52099,#52100,#52101,#52102));
#10222=EDGE_LOOP('',(#52103,#52104,#52105,#52106));
#10223=EDGE_LOOP('',(#52107,#52108,#52109,#52110));
#10224=EDGE_LOOP('',(#52111,#52112,#52113,#52114));
#10225=EDGE_LOOP('',(#52115,#52116,#52117,#52118));
#10226=EDGE_LOOP('',(#52119,#52120,#52121,#52122));
#10227=EDGE_LOOP('',(#52123,#52124,#52125,#52126));
#10228=EDGE_LOOP('',(#52127,#52128,#52129,#52130));
#10229=EDGE_LOOP('',(#52131,#52132,#52133,#52134));
#10230=EDGE_LOOP('',(#52135,#52136,#52137,#52138));
#10231=EDGE_LOOP('',(#52139,#52140,#52141,#52142));
#10232=EDGE_LOOP('',(#52143,#52144,#52145,#52146));
#10233=EDGE_LOOP('',(#52147,#52148,#52149,#52150));
#10234=EDGE_LOOP('',(#52151,#52152,#52153,#52154));
#10235=EDGE_LOOP('',(#52155,#52156,#52157,#52158));
#10236=EDGE_LOOP('',(#52159,#52160,#52161,#52162));
#10237=EDGE_LOOP('',(#52163,#52164,#52165,#52166));
#10238=EDGE_LOOP('',(#52167,#52168,#52169,#52170));
#10239=EDGE_LOOP('',(#52171,#52172,#52173,#52174));
#10240=EDGE_LOOP('',(#52175,#52176,#52177,#52178));
#10241=EDGE_LOOP('',(#52179,#52180,#52181,#52182));
#10242=EDGE_LOOP('',(#52183,#52184,#52185,#52186));
#10243=EDGE_LOOP('',(#52187,#52188,#52189,#52190));
#10244=EDGE_LOOP('',(#52191,#52192,#52193,#52194));
#10245=EDGE_LOOP('',(#52195,#52196,#52197,#52198));
#10246=EDGE_LOOP('',(#52199,#52200,#52201,#52202));
#10247=EDGE_LOOP('',(#52203,#52204,#52205,#52206));
#10248=EDGE_LOOP('',(#52207,#52208,#52209,#52210));
#10249=EDGE_LOOP('',(#52211,#52212,#52213,#52214));
#10250=EDGE_LOOP('',(#52215,#52216,#52217,#52218));
#10251=EDGE_LOOP('',(#52219,#52220,#52221,#52222));
#10252=EDGE_LOOP('',(#52223,#52224,#52225,#52226));
#10253=EDGE_LOOP('',(#52227,#52228,#52229,#52230));
#10254=EDGE_LOOP('',(#52231,#52232,#52233,#52234));
#10255=EDGE_LOOP('',(#52235,#52236,#52237,#52238));
#10256=EDGE_LOOP('',(#52239,#52240,#52241,#52242));
#10257=EDGE_LOOP('',(#52243,#52244,#52245,#52246));
#10258=EDGE_LOOP('',(#52247,#52248,#52249,#52250));
#10259=EDGE_LOOP('',(#52251,#52252,#52253,#52254));
#10260=EDGE_LOOP('',(#52255,#52256,#52257,#52258));
#10261=EDGE_LOOP('',(#52259,#52260,#52261,#52262));
#10262=EDGE_LOOP('',(#52263,#52264,#52265,#52266));
#10263=EDGE_LOOP('',(#52267,#52268,#52269,#52270));
#10264=EDGE_LOOP('',(#52271,#52272,#52273,#52274));
#10265=EDGE_LOOP('',(#52275,#52276,#52277,#52278));
#10266=EDGE_LOOP('',(#52279,#52280,#52281,#52282));
#10267=EDGE_LOOP('',(#52283,#52284,#52285,#52286));
#10268=EDGE_LOOP('',(#52287,#52288,#52289,#52290));
#10269=EDGE_LOOP('',(#52291,#52292,#52293,#52294));
#10270=EDGE_LOOP('',(#52295,#52296,#52297,#52298));
#10271=EDGE_LOOP('',(#52299,#52300,#52301,#52302));
#10272=EDGE_LOOP('',(#52303,#52304,#52305,#52306));
#10273=EDGE_LOOP('',(#52307,#52308,#52309,#52310));
#10274=EDGE_LOOP('',(#52311,#52312,#52313,#52314));
#10275=EDGE_LOOP('',(#52315,#52316,#52317,#52318));
#10276=EDGE_LOOP('',(#52319,#52320,#52321,#52322));
#10277=EDGE_LOOP('',(#52323,#52324,#52325,#52326));
#10278=EDGE_LOOP('',(#52327,#52328,#52329,#52330));
#10279=EDGE_LOOP('',(#52331,#52332,#52333,#52334));
#10280=EDGE_LOOP('',(#52335,#52336,#52337,#52338));
#10281=EDGE_LOOP('',(#52339,#52340,#52341,#52342));
#10282=EDGE_LOOP('',(#52343,#52344,#52345,#52346));
#10283=EDGE_LOOP('',(#52347,#52348,#52349,#52350));
#10284=EDGE_LOOP('',(#52351,#52352,#52353,#52354));
#10285=EDGE_LOOP('',(#52355,#52356,#52357,#52358));
#10286=EDGE_LOOP('',(#52359,#52360,#52361,#52362));
#10287=EDGE_LOOP('',(#52363,#52364,#52365,#52366));
#10288=EDGE_LOOP('',(#52367,#52368,#52369,#52370));
#10289=EDGE_LOOP('',(#52371,#52372,#52373,#52374));
#10290=EDGE_LOOP('',(#52375,#52376,#52377,#52378));
#10291=EDGE_LOOP('',(#52379,#52380,#52381,#52382));
#10292=EDGE_LOOP('',(#52383,#52384,#52385,#52386));
#10293=EDGE_LOOP('',(#52387,#52388,#52389,#52390));
#10294=EDGE_LOOP('',(#52391,#52392,#52393,#52394));
#10295=EDGE_LOOP('',(#52395,#52396,#52397,#52398));
#10296=EDGE_LOOP('',(#52399,#52400,#52401,#52402));
#10297=EDGE_LOOP('',(#52403,#52404,#52405,#52406));
#10298=EDGE_LOOP('',(#52407,#52408,#52409,#52410));
#10299=EDGE_LOOP('',(#52411,#52412,#52413,#52414));
#10300=EDGE_LOOP('',(#52415,#52416,#52417,#52418));
#10301=EDGE_LOOP('',(#52419,#52420,#52421,#52422));
#10302=EDGE_LOOP('',(#52423,#52424,#52425,#52426));
#10303=EDGE_LOOP('',(#52427,#52428,#52429,#52430));
#10304=EDGE_LOOP('',(#52431,#52432,#52433,#52434));
#10305=EDGE_LOOP('',(#52435,#52436,#52437,#52438));
#10306=EDGE_LOOP('',(#52439,#52440,#52441,#52442));
#10307=EDGE_LOOP('',(#52443,#52444,#52445,#52446));
#10308=EDGE_LOOP('',(#52447,#52448,#52449,#52450));
#10309=EDGE_LOOP('',(#52451,#52452,#52453,#52454));
#10310=EDGE_LOOP('',(#52455,#52456,#52457,#52458));
#10311=EDGE_LOOP('',(#52459,#52460,#52461,#52462));
#10312=EDGE_LOOP('',(#52463,#52464,#52465,#52466));
#10313=EDGE_LOOP('',(#52467,#52468,#52469,#52470));
#10314=EDGE_LOOP('',(#52471,#52472,#52473,#52474));
#10315=EDGE_LOOP('',(#52475,#52476,#52477,#52478));
#10316=EDGE_LOOP('',(#52479,#52480,#52481,#52482));
#10317=EDGE_LOOP('',(#52483,#52484,#52485,#52486));
#10318=EDGE_LOOP('',(#52487,#52488,#52489,#52490,#52491,#52492));
#10319=EDGE_LOOP('',(#52493,#52494,#52495,#52496,#52497,#52498,#52499,#52500,
#52501,#52502,#52503,#52504,#52505,#52506,#52507,#52508,#52509,#52510,#52511,
#52512,#52513,#52514,#52515,#52516,#52517,#52518,#52519,#52520,#52521,#52522,
#52523,#52524,#52525,#52526,#52527,#52528,#52529,#52530,#52531,#52532,#52533,
#52534,#52535,#52536,#52537,#52538,#52539,#52540,#52541,#52542,#52543,#52544,
#52545,#52546,#52547,#52548,#52549,#52550,#52551,#52552,#52553,#52554,#52555,
#52556,#52557,#52558,#52559,#52560,#52561,#52562,#52563,#52564,#52565,#52566,
#52567,#52568,#52569,#52570,#52571,#52572,#52573,#52574,#52575,#52576,#52577,
#52578,#52579,#52580,#52581,#52582,#52583,#52584,#52585,#52586,#52587,#52588,
#52589,#52590,#52591,#52592,#52593,#52594,#52595,#52596,#52597,#52598,#52599,
#52600,#52601,#52602,#52603,#52604,#52605,#52606,#52607,#52608,#52609,#52610,
#52611,#52612,#52613,#52614,#52615,#52616,#52617,#52618,#52619,#52620,#52621,
#52622,#52623,#52624,#52625,#52626,#52627,#52628,#52629,#52630,#52631,#52632,
#52633,#52634,#52635,#52636,#52637,#52638,#52639,#52640,#52641,#52642,#52643,
#52644,#52645,#52646,#52647,#52648,#52649,#52650,#52651,#52652,#52653,#52654,
#52655,#52656,#52657,#52658,#52659,#52660,#52661,#52662,#52663,#52664,#52665,
#52666,#52667,#52668,#52669,#52670,#52671,#52672,#52673,#52674,#52675,#52676,
#52677,#52678,#52679,#52680,#52681,#52682,#52683,#52684,#52685,#52686,#52687,
#52688,#52689,#52690,#52691,#52692,#52693,#52694,#52695,#52696,#52697,#52698,
#52699,#52700,#52701,#52702,#52703,#52704,#52705,#52706,#52707,#52708,#52709,
#52710,#52711,#52712,#52713,#52714,#52715,#52716,#52717,#52718,#52719,#52720,
#52721,#52722,#52723,#52724,#52725,#52726,#52727,#52728,#52729,#52730,#52731,
#52732,#52733,#52734,#52735,#52736,#52737,#52738,#52739,#52740,#52741,#52742,
#52743,#52744,#52745,#52746,#52747,#52748,#52749,#52750,#52751,#52752,#52753,
#52754,#52755,#52756,#52757,#52758,#52759,#52760,#52761,#52762,#52763,#52764,
#52765,#52766,#52767,#52768,#52769,#52770,#52771,#52772,#52773,#52774,#52775,
#52776,#52777,#52778,#52779,#52780,#52781,#52782,#52783,#52784,#52785,#52786,
#52787,#52788,#52789,#52790,#52791,#52792,#52793,#52794,#52795,#52796,#52797,
#52798,#52799,#52800,#52801,#52802,#52803,#52804,#52805,#52806,#52807,#52808,
#52809,#52810,#52811,#52812,#52813,#52814,#52815,#52816,#52817,#52818,#52819,
#52820,#52821,#52822,#52823,#52824,#52825,#52826,#52827,#52828,#52829,#52830,
#52831,#52832,#52833,#52834,#52835,#52836,#52837,#52838,#52839,#52840,#52841,
#52842,#52843,#52844,#52845,#52846,#52847,#52848,#52849,#52850,#52851,#52852,
#52853,#52854,#52855,#52856,#52857,#52858,#52859,#52860,#52861,#52862,#52863,
#52864,#52865,#52866,#52867,#52868,#52869,#52870,#52871,#52872,#52873,#52874,
#52875,#52876,#52877,#52878,#52879,#52880,#52881,#52882,#52883,#52884,#52885,
#52886,#52887,#52888,#52889,#52890,#52891,#52892,#52893,#52894,#52895,#52896,
#52897,#52898,#52899,#52900,#52901,#52902,#52903,#52904,#52905,#52906,#52907,
#52908,#52909,#52910,#52911,#52912,#52913,#52914,#52915,#52916,#52917,#52918,
#52919,#52920,#52921,#52922,#52923,#52924,#52925,#52926,#52927,#52928,#52929,
#52930,#52931,#52932,#52933,#52934,#52935,#52936,#52937,#52938,#52939,#52940,
#52941,#52942,#52943,#52944,#52945,#52946,#52947,#52948,#52949,#52950,#52951,
#52952,#52953,#52954,#52955,#52956,#52957,#52958,#52959,#52960,#52961,#52962,
#52963,#52964,#52965,#52966,#52967,#52968,#52969,#52970,#52971,#52972,#52973,
#52974,#52975,#52976,#52977,#52978,#52979,#52980,#52981,#52982,#52983,#52984,
#52985,#52986,#52987,#52988,#52989,#52990,#52991,#52992,#52993,#52994,#52995,
#52996));
#10320=EDGE_LOOP('',(#52997,#52998,#52999,#53000,#53001,#53002,#53003,#53004,
#53005,#53006,#53007,#53008,#53009,#53010,#53011,#53012,#53013,#53014,#53015,
#53016,#53017,#53018,#53019,#53020,#53021,#53022,#53023,#53024,#53025,#53026,
#53027,#53028,#53029,#53030,#53031,#53032,#53033,#53034,#53035,#53036,#53037,
#53038,#53039,#53040,#53041,#53042,#53043,#53044,#53045,#53046,#53047,#53048,
#53049,#53050,#53051,#53052,#53053,#53054,#53055,#53056,#53057,#53058,#53059,
#53060,#53061,#53062,#53063,#53064,#53065,#53066,#53067,#53068,#53069,#53070,
#53071,#53072,#53073,#53074,#53075,#53076,#53077,#53078,#53079,#53080,#53081,
#53082,#53083,#53084,#53085,#53086,#53087,#53088,#53089,#53090,#53091,#53092,
#53093,#53094,#53095,#53096,#53097,#53098,#53099,#53100,#53101,#53102,#53103,
#53104,#53105,#53106,#53107,#53108,#53109,#53110,#53111,#53112,#53113,#53114,
#53115,#53116,#53117,#53118,#53119,#53120,#53121,#53122,#53123,#53124,#53125,
#53126,#53127,#53128,#53129,#53130,#53131,#53132,#53133,#53134,#53135,#53136,
#53137,#53138,#53139,#53140,#53141,#53142,#53143,#53144,#53145,#53146,#53147,
#53148,#53149,#53150,#53151,#53152,#53153,#53154,#53155,#53156,#53157,#53158,
#53159,#53160,#53161,#53162,#53163,#53164,#53165,#53166,#53167,#53168,#53169,
#53170,#53171,#53172,#53173,#53174,#53175,#53176,#53177,#53178,#53179,#53180,
#53181,#53182,#53183,#53184,#53185,#53186,#53187,#53188,#53189,#53190,#53191,
#53192,#53193,#53194,#53195,#53196,#53197,#53198,#53199,#53200,#53201,#53202,
#53203,#53204,#53205,#53206,#53207,#53208,#53209,#53210,#53211,#53212,#53213,
#53214,#53215,#53216,#53217,#53218,#53219,#53220,#53221,#53222,#53223,#53224,
#53225,#53226,#53227,#53228,#53229,#53230,#53231,#53232,#53233,#53234,#53235,
#53236,#53237,#53238,#53239,#53240,#53241,#53242,#53243,#53244,#53245,#53246,
#53247,#53248,#53249,#53250,#53251,#53252,#53253,#53254,#53255,#53256,#53257,
#53258,#53259,#53260,#53261,#53262,#53263,#53264,#53265,#53266,#53267,#53268,
#53269,#53270,#53271,#53272,#53273,#53274,#53275,#53276,#53277,#53278,#53279,
#53280,#53281,#53282,#53283,#53284,#53285,#53286,#53287,#53288,#53289,#53290,
#53291,#53292,#53293,#53294,#53295,#53296,#53297,#53298,#53299,#53300,#53301,
#53302,#53303,#53304,#53305,#53306,#53307,#53308,#53309,#53310,#53311,#53312,
#53313,#53314,#53315,#53316,#53317,#53318,#53319,#53320,#53321,#53322,#53323,
#53324,#53325,#53326,#53327,#53328,#53329,#53330,#53331,#53332,#53333,#53334,
#53335,#53336,#53337,#53338,#53339,#53340,#53341,#53342,#53343,#53344,#53345,
#53346,#53347,#53348,#53349,#53350,#53351,#53352,#53353,#53354,#53355,#53356,
#53357,#53358,#53359,#53360,#53361,#53362,#53363,#53364,#53365,#53366,#53367,
#53368,#53369,#53370,#53371,#53372,#53373,#53374,#53375,#53376,#53377,#53378,
#53379,#53380,#53381,#53382,#53383,#53384,#53385,#53386,#53387,#53388,#53389,
#53390,#53391,#53392,#53393,#53394,#53395,#53396,#53397,#53398,#53399,#53400,
#53401,#53402,#53403,#53404,#53405,#53406,#53407,#53408,#53409,#53410,#53411,
#53412,#53413,#53414,#53415,#53416,#53417,#53418,#53419,#53420,#53421,#53422,
#53423,#53424,#53425,#53426,#53427,#53428,#53429,#53430,#53431,#53432,#53433,
#53434,#53435,#53436,#53437,#53438,#53439,#53440,#53441,#53442,#53443,#53444,
#53445,#53446,#53447,#53448,#53449,#53450,#53451,#53452,#53453,#53454,#53455,
#53456,#53457,#53458,#53459,#53460,#53461,#53462,#53463,#53464,#53465,#53466,
#53467,#53468,#53469,#53470,#53471,#53472,#53473,#53474,#53475,#53476,#53477,
#53478,#53479,#53480,#53481,#53482,#53483,#53484,#53485,#53486,#53487,#53488,
#53489,#53490,#53491,#53492,#53493,#53494,#53495,#53496,#53497,#53498,#53499,
#53500));
#10321=EDGE_LOOP('',(#53501,#53502,#53503,#53504));
#10322=EDGE_LOOP('',(#53505,#53506,#53507,#53508));
#10323=EDGE_LOOP('',(#53509,#53510,#53511,#53512));
#10324=EDGE_LOOP('',(#53513,#53514,#53515,#53516,#53517,#53518));
#10325=EDGE_LOOP('',(#53519,#53520,#53521,#53522));
#10326=EDGE_LOOP('',(#53523,#53524,#53525,#53526));
#10327=EDGE_LOOP('',(#53527,#53528,#53529,#53530,#53531,#53532,#53533));
#10328=EDGE_LOOP('',(#53534,#53535,#53536,#53537));
#10329=EDGE_LOOP('',(#53538,#53539,#53540,#53541,#53542,#53543,#53544,#53545,
#53546,#53547,#53548));
#10330=EDGE_LOOP('',(#53549));
#10331=EDGE_LOOP('',(#53550,#53551,#53552,#53553));
#10332=EDGE_LOOP('',(#53554,#53555,#53556,#53557,#53558,#53559));
#10333=EDGE_LOOP('',(#53560,#53561,#53562,#53563));
#10334=EDGE_LOOP('',(#53564,#53565,#53566,#53567,#53568,#53569,#53570,#53571,
#53572));
#10335=EDGE_LOOP('',(#53573,#53574,#53575,#53576));
#10336=EDGE_LOOP('',(#53577,#53578,#53579,#53580,#53581));
#10337=EDGE_LOOP('',(#53582,#53583,#53584,#53585));
#10338=EDGE_LOOP('',(#53586,#53587,#53588,#53589));
#10339=EDGE_LOOP('',(#53590,#53591,#53592,#53593));
#10340=EDGE_LOOP('',(#53594,#53595,#53596,#53597,#53598,#53599,#53600,#53601));
#10341=EDGE_LOOP('',(#53602));
#10342=EDGE_LOOP('',(#53603,#53604,#53605,#53606));
#10343=EDGE_LOOP('',(#53607,#53608,#53609,#53610));
#10344=EDGE_LOOP('',(#53611,#53612,#53613,#53614));
#10345=EDGE_LOOP('',(#53615,#53616,#53617,#53618));
#10346=EDGE_LOOP('',(#53619,#53620,#53621,#53622));
#10347=EDGE_LOOP('',(#53623,#53624,#53625,#53626));
#10348=EDGE_LOOP('',(#53627,#53628,#53629,#53630));
#10349=EDGE_LOOP('',(#53631,#53632,#53633,#53634));
#10350=EDGE_LOOP('',(#53635,#53636,#53637,#53638));
#10351=EDGE_LOOP('',(#53639,#53640,#53641,#53642));
#10352=EDGE_LOOP('',(#53643,#53644,#53645,#53646));
#10353=EDGE_LOOP('',(#53647,#53648,#53649,#53650));
#10354=EDGE_LOOP('',(#53651,#53652,#53653,#53654));
#10355=EDGE_LOOP('',(#53655,#53656,#53657,#53658));
#10356=EDGE_LOOP('',(#53659,#53660,#53661,#53662));
#10357=EDGE_LOOP('',(#53663,#53664,#53665,#53666));
#10358=EDGE_LOOP('',(#53667,#53668,#53669,#53670));
#10359=EDGE_LOOP('',(#53671,#53672,#53673,#53674));
#10360=EDGE_LOOP('',(#53675,#53676,#53677,#53678));
#10361=EDGE_LOOP('',(#53679,#53680,#53681,#53682));
#10362=EDGE_LOOP('',(#53683,#53684,#53685,#53686));
#10363=EDGE_LOOP('',(#53687,#53688,#53689,#53690));
#10364=EDGE_LOOP('',(#53691,#53692,#53693,#53694));
#10365=EDGE_LOOP('',(#53695,#53696,#53697,#53698));
#10366=EDGE_LOOP('',(#53699,#53700,#53701,#53702));
#10367=EDGE_LOOP('',(#53703,#53704,#53705,#53706));
#10368=EDGE_LOOP('',(#53707,#53708,#53709,#53710));
#10369=EDGE_LOOP('',(#53711,#53712,#53713,#53714));
#10370=EDGE_LOOP('',(#53715,#53716,#53717,#53718));
#10371=EDGE_LOOP('',(#53719,#53720,#53721,#53722));
#10372=EDGE_LOOP('',(#53723,#53724,#53725,#53726));
#10373=EDGE_LOOP('',(#53727,#53728,#53729,#53730));
#10374=EDGE_LOOP('',(#53731,#53732,#53733,#53734));
#10375=EDGE_LOOP('',(#53735,#53736,#53737,#53738));
#10376=EDGE_LOOP('',(#53739,#53740,#53741,#53742));
#10377=EDGE_LOOP('',(#53743,#53744,#53745,#53746));
#10378=EDGE_LOOP('',(#53747,#53748,#53749,#53750));
#10379=EDGE_LOOP('',(#53751,#53752,#53753,#53754));
#10380=EDGE_LOOP('',(#53755,#53756,#53757,#53758));
#10381=EDGE_LOOP('',(#53759,#53760,#53761,#53762));
#10382=EDGE_LOOP('',(#53763,#53764,#53765,#53766));
#10383=EDGE_LOOP('',(#53767,#53768,#53769,#53770));
#10384=EDGE_LOOP('',(#53771,#53772,#53773,#53774));
#10385=EDGE_LOOP('',(#53775,#53776,#53777,#53778));
#10386=EDGE_LOOP('',(#53779,#53780,#53781,#53782));
#10387=EDGE_LOOP('',(#53783,#53784,#53785,#53786));
#10388=EDGE_LOOP('',(#53787,#53788,#53789,#53790));
#10389=EDGE_LOOP('',(#53791,#53792,#53793,#53794));
#10390=EDGE_LOOP('',(#53795,#53796,#53797,#53798));
#10391=EDGE_LOOP('',(#53799,#53800,#53801,#53802));
#10392=EDGE_LOOP('',(#53803,#53804,#53805,#53806));
#10393=EDGE_LOOP('',(#53807,#53808,#53809,#53810));
#10394=EDGE_LOOP('',(#53811,#53812,#53813,#53814));
#10395=EDGE_LOOP('',(#53815,#53816,#53817,#53818));
#10396=EDGE_LOOP('',(#53819,#53820,#53821,#53822));
#10397=EDGE_LOOP('',(#53823,#53824,#53825,#53826));
#10398=EDGE_LOOP('',(#53827,#53828,#53829,#53830));
#10399=EDGE_LOOP('',(#53831,#53832,#53833,#53834));
#10400=EDGE_LOOP('',(#53835,#53836,#53837,#53838));
#10401=EDGE_LOOP('',(#53839,#53840,#53841,#53842));
#10402=EDGE_LOOP('',(#53843,#53844,#53845,#53846));
#10403=EDGE_LOOP('',(#53847,#53848,#53849,#53850));
#10404=EDGE_LOOP('',(#53851,#53852,#53853,#53854));
#10405=EDGE_LOOP('',(#53855,#53856,#53857,#53858));
#10406=EDGE_LOOP('',(#53859,#53860,#53861,#53862));
#10407=EDGE_LOOP('',(#53863,#53864,#53865,#53866));
#10408=EDGE_LOOP('',(#53867,#53868,#53869));
#10409=EDGE_LOOP('',(#53870,#53871,#53872));
#10410=EDGE_LOOP('',(#53873,#53874,#53875,#53876,#53877,#53878,#53879,#53880,
#53881,#53882,#53883,#53884,#53885,#53886,#53887,#53888,#53889,#53890,#53891,
#53892,#53893,#53894,#53895,#53896,#53897,#53898,#53899,#53900,#53901,#53902,
#53903,#53904,#53905,#53906,#53907,#53908,#53909,#53910,#53911,#53912,#53913,
#53914,#53915,#53916,#53917,#53918,#53919,#53920,#53921,#53922,#53923,#53924,
#53925,#53926,#53927,#53928,#53929,#53930,#53931,#53932,#53933,#53934,#53935,
#53936,#53937,#53938,#53939,#53940,#53941,#53942,#53943,#53944,#53945,#53946,
#53947,#53948));
#10411=EDGE_LOOP('',(#53949,#53950,#53951,#53952));
#10412=EDGE_LOOP('',(#53953,#53954,#53955,#53956,#53957,#53958,#53959,#53960,
#53961,#53962,#53963,#53964));
#10413=EDGE_LOOP('',(#53965,#53966,#53967,#53968,#53969,#53970,#53971,#53972,
#53973,#53974,#53975,#53976,#53977,#53978,#53979,#53980,#53981,#53982,#53983,
#53984,#53985,#53986,#53987,#53988,#53989,#53990,#53991,#53992,#53993,#53994,
#53995,#53996,#53997,#53998,#53999,#54000,#54001,#54002,#54003,#54004,#54005,
#54006,#54007,#54008,#54009,#54010,#54011,#54012,#54013,#54014,#54015,#54016,
#54017,#54018,#54019,#54020,#54021,#54022,#54023,#54024,#54025,#54026,#54027,
#54028,#54029,#54030,#54031));
#10414=EDGE_LOOP('',(#54032,#54033,#54034,#54035,#54036));
#10415=EDGE_LOOP('',(#54037,#54038,#54039,#54040));
#10416=EDGE_LOOP('',(#54041,#54042,#54043,#54044,#54045,#54046,#54047,#54048,
#54049,#54050,#54051,#54052));
#10417=EDGE_LOOP('',(#54053,#54054,#54055,#54056,#54057,#54058));
#10418=EDGE_LOOP('',(#54059,#54060,#54061,#54062));
#10419=EDGE_LOOP('',(#54063,#54064,#54065,#54066,#54067,#54068,#54069,#54070));
#10420=EDGE_LOOP('',(#54071,#54072,#54073,#54074));
#10421=EDGE_LOOP('',(#54075,#54076,#54077,#54078));
#10422=EDGE_LOOP('',(#54079,#54080,#54081,#54082));
#10423=EDGE_LOOP('',(#54083,#54084,#54085,#54086,#54087,#54088));
#10424=EDGE_LOOP('',(#54089));
#10425=EDGE_LOOP('',(#54090));
#10426=EDGE_LOOP('',(#54091,#54092,#54093,#54094));
#10427=EDGE_LOOP('',(#54095,#54096,#54097,#54098));
#10428=EDGE_LOOP('',(#54099,#54100,#54101,#54102));
#10429=EDGE_LOOP('',(#54103,#54104,#54105,#54106));
#10430=EDGE_LOOP('',(#54107,#54108,#54109,#54110));
#10431=EDGE_LOOP('',(#54111,#54112,#54113,#54114));
#10432=EDGE_LOOP('',(#54115,#54116,#54117,#54118));
#10433=EDGE_LOOP('',(#54119,#54120,#54121,#54122));
#10434=EDGE_LOOP('',(#54123,#54124,#54125,#54126));
#10435=EDGE_LOOP('',(#54127,#54128,#54129,#54130));
#10436=EDGE_LOOP('',(#54131,#54132,#54133,#54134));
#10437=EDGE_LOOP('',(#54135,#54136,#54137,#54138));
#10438=EDGE_LOOP('',(#54139,#54140,#54141,#54142));
#10439=EDGE_LOOP('',(#54143,#54144,#54145,#54146));
#10440=EDGE_LOOP('',(#54147,#54148,#54149,#54150));
#10441=EDGE_LOOP('',(#54151,#54152,#54153,#54154));
#10442=EDGE_LOOP('',(#54155,#54156,#54157,#54158));
#10443=EDGE_LOOP('',(#54159,#54160,#54161,#54162));
#10444=EDGE_LOOP('',(#54163,#54164,#54165,#54166));
#10445=EDGE_LOOP('',(#54167,#54168,#54169,#54170));
#10446=EDGE_LOOP('',(#54171,#54172,#54173,#54174));
#10447=EDGE_LOOP('',(#54175,#54176,#54177,#54178,#54179));
#10448=EDGE_LOOP('',(#54180,#54181,#54182,#54183,#54184,#54185,#54186,#54187,
#54188,#54189,#54190,#54191,#54192,#54193,#54194,#54195,#54196,#54197,#54198,
#54199,#54200,#54201,#54202,#54203,#54204));
#10449=EDGE_LOOP('',(#54205,#54206,#54207,#54208,#54209));
#10450=EDGE_LOOP('',(#54210,#54211,#54212,#54213));
#10451=EDGE_LOOP('',(#54214,#54215,#54216,#54217,#54218,#54219,#54220,#54221,
#54222,#54223,#54224,#54225,#54226,#54227,#54228,#54229,#54230,#54231,#54232,
#54233,#54234,#54235,#54236,#54237,#54238));
#10452=EDGE_LOOP('',(#54239,#54240,#54241,#54242,#54243,#54244));
#10453=EDGE_LOOP('',(#54245));
#10454=EDGE_LOOP('',(#54246));
#10455=EDGE_LOOP('',(#54247,#54248,#54249,#54250));
#10456=EDGE_LOOP('',(#54251,#54252,#54253,#54254,#54255,#54256));
#10457=EDGE_LOOP('',(#54257,#54258,#54259,#54260,#54261,#54262));
#10458=EDGE_LOOP('',(#54263,#54264,#54265,#54266,#54267));
#10459=EDGE_LOOP('',(#54268,#54269,#54270,#54271));
#10460=EDGE_LOOP('',(#54272,#54273,#54274,#54275));
#10461=EDGE_LOOP('',(#54276,#54277));
#10462=EDGE_LOOP('',(#54278,#54279));
#10463=EDGE_LOOP('',(#54280,#54281,#54282,#54283,#54284,#54285,#54286,#54287,
#54288,#54289,#54290,#54291));
#10464=EDGE_LOOP('',(#54292,#54293,#54294,#54295,#54296,#54297));
#10465=EDGE_LOOP('',(#54298));
#10466=EDGE_LOOP('',(#54299,#54300,#54301,#54302));
#10467=EDGE_LOOP('',(#54303,#54304,#54305,#54306));
#10468=EDGE_LOOP('',(#54307,#54308,#54309,#54310));
#10469=EDGE_LOOP('',(#54311,#54312,#54313,#54314));
#10470=EDGE_LOOP('',(#54315,#54316,#54317,#54318));
#10471=EDGE_LOOP('',(#54319,#54320,#54321,#54322));
#10472=EDGE_LOOP('',(#54323,#54324,#54325,#54326));
#10473=EDGE_LOOP('',(#54327,#54328,#54329,#54330));
#10474=EDGE_LOOP('',(#54331,#54332,#54333,#54334));
#10475=EDGE_LOOP('',(#54335,#54336,#54337,#54338,#54339));
#10476=EDGE_LOOP('',(#54340,#54341,#54342,#54343,#54344,#54345,#54346,#54347,
#54348,#54349,#54350,#54351,#54352));
#10477=EDGE_LOOP('',(#54353,#54354,#54355,#54356,#54357));
#10478=EDGE_LOOP('',(#54358,#54359,#54360,#54361));
#10479=EDGE_LOOP('',(#54362,#54363,#54364,#54365,#54366,#54367,#54368,#54369,
#54370,#54371,#54372,#54373,#54374));
#10480=EDGE_LOOP('',(#54375,#54376,#54377,#54378,#54379,#54380,#54381,#54382,
#54383,#54384,#54385,#54386,#54387,#54388,#54389,#54390,#54391,#54392,#54393,
#54394,#54395));
#10481=EDGE_LOOP('',(#54396,#54397,#54398,#54399));
#10482=EDGE_LOOP('',(#54400,#54401,#54402,#54403));
#10483=EDGE_LOOP('',(#54404,#54405,#54406,#54407));
#10484=EDGE_LOOP('',(#54408,#54409,#54410,#54411));
#10485=EDGE_LOOP('',(#54412,#54413,#54414,#54415));
#10486=EDGE_LOOP('',(#54416,#54417,#54418,#54419));
#10487=EDGE_LOOP('',(#54420,#54421,#54422,#54423,#54424,#54425,#54426,#54427));
#10488=EDGE_LOOP('',(#54428,#54429,#54430,#54431,#54432,#54433,#54434,#54435));
#10489=EDGE_LOOP('',(#54436,#54437,#54438,#54439,#54440,#54441,#54442,#54443));
#10490=EDGE_LOOP('',(#54444,#54445));
#10491=EDGE_LOOP('',(#54446,#54447));
#10492=EDGE_LOOP('',(#54448,#54449));
#10493=EDGE_LOOP('',(#54450,#54451));
#10494=EDGE_LOOP('',(#54452,#54453));
#10495=EDGE_LOOP('',(#54454,#54455));
#10496=EDGE_LOOP('',(#54456,#54457));
#10497=EDGE_LOOP('',(#54458,#54459));
#10498=EDGE_LOOP('',(#54460,#54461));
#10499=EDGE_LOOP('',(#54462,#54463));
#10500=EDGE_LOOP('',(#54464,#54465));
#10501=EDGE_LOOP('',(#54466,#54467));
#10502=EDGE_LOOP('',(#54468,#54469,#54470,#54471,#54472,#54473,#54474,#54475));
#10503=EDGE_LOOP('',(#54476,#54477,#54478,#54479,#54480,#54481,#54482,#54483));
#10504=EDGE_LOOP('',(#54484,#54485,#54486,#54487,#54488,#54489,#54490,#54491));
#10505=EDGE_LOOP('',(#54492,#54493,#54494,#54495,#54496,#54497,#54498,#54499));
#10506=EDGE_LOOP('',(#54500));
#10507=EDGE_LOOP('',(#54501));
#10508=EDGE_LOOP('',(#54502,#54503,#54504,#54505,#54506,#54507));
#10509=EDGE_LOOP('',(#54508,#54509,#54510,#54511));
#10510=EDGE_LOOP('',(#54512,#54513,#54514,#54515,#54516,#54517));
#10511=EDGE_LOOP('',(#54518));
#10512=EDGE_LOOP('',(#54519,#54520,#54521,#54522));
#10513=EDGE_LOOP('',(#54523,#54524,#54525,#54526));
#10514=EDGE_LOOP('',(#54527,#54528,#54529,#54530));
#10515=EDGE_LOOP('',(#54531,#54532,#54533,#54534,#54535));
#10516=EDGE_LOOP('',(#54536,#54537,#54538,#54539));
#10517=EDGE_LOOP('',(#54540,#54541,#54542,#54543));
#10518=EDGE_LOOP('',(#54544,#54545,#54546,#54547));
#10519=EDGE_LOOP('',(#54548,#54549,#54550,#54551));
#10520=EDGE_LOOP('',(#54552,#54553,#54554,#54555,#54556,#54557,#54558,#54559,
#54560,#54561,#54562));
#10521=EDGE_LOOP('',(#54563,#54564,#54565,#54566,#54567));
#10522=EDGE_LOOP('',(#54568,#54569,#54570,#54571));
#10523=EDGE_LOOP('',(#54572,#54573,#54574,#54575,#54576,#54577,#54578,#54579,
#54580,#54581));
#10524=EDGE_LOOP('',(#54582,#54583,#54584,#54585,#54586,#54587,#54588,#54589,
#54590,#54591,#54592,#54593,#54594,#54595,#54596,#54597,#54598,#54599,#54600,
#54601,#54602));
#10525=EDGE_LOOP('',(#54603,#54604,#54605,#54606));
#10526=EDGE_LOOP('',(#54607,#54608,#54609,#54610));
#10527=EDGE_LOOP('',(#54611,#54612,#54613,#54614));
#10528=EDGE_LOOP('',(#54615,#54616,#54617,#54618));
#10529=EDGE_LOOP('',(#54619,#54620,#54621,#54622));
#10530=EDGE_LOOP('',(#54623,#54624,#54625,#54626));
#10531=EDGE_LOOP('',(#54627,#54628,#54629,#54630,#54631,#54632,#54633,#54634));
#10532=EDGE_LOOP('',(#54635,#54636,#54637,#54638,#54639,#54640,#54641,#54642));
#10533=EDGE_LOOP('',(#54643,#54644,#54645,#54646,#54647,#54648,#54649,#54650));
#10534=EDGE_LOOP('',(#54651,#54652));
#10535=EDGE_LOOP('',(#54653,#54654));
#10536=EDGE_LOOP('',(#54655,#54656));
#10537=EDGE_LOOP('',(#54657,#54658));
#10538=EDGE_LOOP('',(#54659,#54660));
#10539=EDGE_LOOP('',(#54661,#54662));
#10540=EDGE_LOOP('',(#54663,#54664));
#10541=EDGE_LOOP('',(#54665,#54666));
#10542=EDGE_LOOP('',(#54667,#54668));
#10543=EDGE_LOOP('',(#54669,#54670));
#10544=EDGE_LOOP('',(#54671,#54672));
#10545=EDGE_LOOP('',(#54673,#54674));
#10546=EDGE_LOOP('',(#54675,#54676,#54677,#54678,#54679,#54680,#54681,#54682));
#10547=EDGE_LOOP('',(#54683,#54684,#54685,#54686,#54687,#54688,#54689,#54690));
#10548=EDGE_LOOP('',(#54691,#54692,#54693,#54694,#54695,#54696,#54697,#54698));
#10549=EDGE_LOOP('',(#54699,#54700,#54701,#54702,#54703,#54704,#54705,#54706));
#10550=EDGE_LOOP('',(#54707));
#10551=EDGE_LOOP('',(#54708));
#10552=EDGE_LOOP('',(#54709,#54710,#54711,#54712,#54713,#54714));
#10553=EDGE_LOOP('',(#54715,#54716,#54717));
#10554=EDGE_LOOP('',(#54718,#54719,#54720,#54721,#54722,#54723));
#10555=EDGE_LOOP('',(#54724));
#10556=EDGE_LOOP('',(#54725,#54726,#54727,#54728));
#10557=EDGE_LOOP('',(#54729,#54730,#54731,#54732));
#10558=EDGE_LOOP('',(#54733,#54734,#54735,#54736));
#10559=EDGE_LOOP('',(#54737,#54738,#54739,#54740));
#10560=EDGE_LOOP('',(#54741,#54742,#54743,#54744));
#10561=EDGE_LOOP('',(#54745,#54746,#54747,#54748));
#10562=EDGE_LOOP('',(#54749,#54750,#54751,#54752));
#10563=EDGE_LOOP('',(#54753,#54754,#54755,#54756));
#10564=EDGE_LOOP('',(#54757,#54758,#54759,#54760));
#10565=EDGE_LOOP('',(#54761,#54762,#54763,#54764));
#10566=EDGE_LOOP('',(#54765,#54766,#54767,#54768));
#10567=EDGE_LOOP('',(#54769,#54770,#54771,#54772));
#10568=EDGE_LOOP('',(#54773,#54774,#54775,#54776));
#10569=EDGE_LOOP('',(#54777,#54778,#54779,#54780));
#10570=EDGE_LOOP('',(#54781,#54782,#54783,#54784));
#10571=EDGE_LOOP('',(#54785,#54786,#54787,#54788));
#10572=EDGE_LOOP('',(#54789,#54790,#54791,#54792));
#10573=EDGE_LOOP('',(#54793,#54794,#54795,#54796));
#10574=EDGE_LOOP('',(#54797,#54798,#54799,#54800));
#10575=EDGE_LOOP('',(#54801,#54802,#54803,#54804));
#10576=EDGE_LOOP('',(#54805,#54806,#54807,#54808));
#10577=EDGE_LOOP('',(#54809,#54810,#54811,#54812,#54813));
#10578=EDGE_LOOP('',(#54814,#54815,#54816,#54817,#54818,#54819,#54820,#54821,
#54822,#54823,#54824,#54825,#54826,#54827,#54828,#54829,#54830,#54831,#54832,
#54833,#54834,#54835,#54836,#54837,#54838));
#10579=EDGE_LOOP('',(#54839,#54840,#54841,#54842,#54843));
#10580=EDGE_LOOP('',(#54844,#54845,#54846,#54847));
#10581=EDGE_LOOP('',(#54848,#54849,#54850,#54851,#54852,#54853,#54854,#54855,
#54856,#54857,#54858,#54859,#54860,#54861,#54862,#54863,#54864,#54865,#54866,
#54867,#54868,#54869,#54870,#54871,#54872));
#10582=EDGE_LOOP('',(#54873,#54874,#54875,#54876,#54877,#54878,#54879,#54880,
#54881,#54882,#54883,#54884,#54885,#54886,#54887,#54888,#54889,#54890,#54891,
#54892,#54893));
#10583=EDGE_LOOP('',(#54894,#54895,#54896,#54897));
#10584=EDGE_LOOP('',(#54898,#54899,#54900,#54901));
#10585=EDGE_LOOP('',(#54902,#54903,#54904,#54905));
#10586=EDGE_LOOP('',(#54906,#54907,#54908,#54909));
#10587=EDGE_LOOP('',(#54910,#54911,#54912,#54913));
#10588=EDGE_LOOP('',(#54914,#54915,#54916,#54917));
#10589=EDGE_LOOP('',(#54918,#54919,#54920,#54921,#54922,#54923,#54924,#54925));
#10590=EDGE_LOOP('',(#54926,#54927,#54928,#54929,#54930,#54931,#54932,#54933));
#10591=EDGE_LOOP('',(#54934,#54935,#54936,#54937,#54938,#54939,#54940,#54941));
#10592=EDGE_LOOP('',(#54942,#54943));
#10593=EDGE_LOOP('',(#54944,#54945));
#10594=EDGE_LOOP('',(#54946,#54947));
#10595=EDGE_LOOP('',(#54948,#54949));
#10596=EDGE_LOOP('',(#54950,#54951));
#10597=EDGE_LOOP('',(#54952,#54953));
#10598=EDGE_LOOP('',(#54954,#54955));
#10599=EDGE_LOOP('',(#54956,#54957));
#10600=EDGE_LOOP('',(#54958,#54959));
#10601=EDGE_LOOP('',(#54960,#54961));
#10602=EDGE_LOOP('',(#54962,#54963));
#10603=EDGE_LOOP('',(#54964,#54965));
#10604=EDGE_LOOP('',(#54966,#54967,#54968,#54969,#54970,#54971,#54972,#54973));
#10605=EDGE_LOOP('',(#54974,#54975,#54976,#54977,#54978,#54979,#54980,#54981));
#10606=EDGE_LOOP('',(#54982,#54983,#54984,#54985,#54986,#54987,#54988,#54989));
#10607=EDGE_LOOP('',(#54990,#54991,#54992,#54993,#54994,#54995,#54996,#54997));
#10608=EDGE_LOOP('',(#54998));
#10609=EDGE_LOOP('',(#54999));
#10610=EDGE_LOOP('',(#55000,#55001,#55002,#55003,#55004,#55005));
#10611=EDGE_LOOP('',(#55006,#55007,#55008,#55009));
#10612=EDGE_LOOP('',(#55010,#55011,#55012,#55013,#55014,#55015));
#10613=EDGE_LOOP('',(#55016));
#10614=EDGE_LOOP('',(#55017,#55018,#55019,#55020));
#10615=EDGE_LOOP('',(#55021,#55022,#55023,#55024));
#10616=EDGE_LOOP('',(#55025,#55026,#55027,#55028));
#10617=EDGE_LOOP('',(#55029,#55030,#55031,#55032));
#10618=EDGE_LOOP('',(#55033,#55034,#55035,#55036));
#10619=EDGE_LOOP('',(#55037,#55038,#55039,#55040));
#10620=EDGE_LOOP('',(#55041,#55042,#55043));
#10621=EDGE_LOOP('',(#55044,#55045,#55046,#55047,#55048));
#10622=EDGE_LOOP('',(#55049,#55050,#55051,#55052));
#10623=EDGE_LOOP('',(#55053,#55054,#55055,#55056));
#10624=EDGE_LOOP('',(#55057,#55058,#55059,#55060));
#10625=EDGE_LOOP('',(#55061,#55062,#55063,#55064));
#10626=EDGE_LOOP('',(#55065,#55066,#55067,#55068,#55069,#55070));
#10627=EDGE_LOOP('',(#55071,#55072,#55073,#55074,#55075,#55076,#55077,#55078,
#55079,#55080,#55081,#55082,#55083,#55084,#55085));
#10628=EDGE_LOOP('',(#55086,#55087,#55088,#55089,#55090));
#10629=EDGE_LOOP('',(#55091,#55092,#55093,#55094));
#10630=EDGE_LOOP('',(#55095,#55096,#55097,#55098,#55099,#55100,#55101,#55102,
#55103,#55104,#55105,#55106,#55107,#55108,#55109,#55110));
#10631=EDGE_LOOP('',(#55111,#55112,#55113,#55114,#55115,#55116,#55117,#55118,
#55119,#55120,#55121,#55122,#55123,#55124,#55125,#55126,#55127,#55128,#55129,
#55130,#55131));
#10632=EDGE_LOOP('',(#55132,#55133,#55134,#55135));
#10633=EDGE_LOOP('',(#55136,#55137,#55138,#55139));
#10634=EDGE_LOOP('',(#55140,#55141,#55142,#55143));
#10635=EDGE_LOOP('',(#55144,#55145,#55146,#55147));
#10636=EDGE_LOOP('',(#55148,#55149,#55150,#55151));
#10637=EDGE_LOOP('',(#55152,#55153,#55154,#55155));
#10638=EDGE_LOOP('',(#55156,#55157,#55158,#55159,#55160,#55161,#55162,#55163));
#10639=EDGE_LOOP('',(#55164,#55165,#55166,#55167,#55168,#55169,#55170,#55171));
#10640=EDGE_LOOP('',(#55172,#55173,#55174,#55175,#55176,#55177,#55178,#55179));
#10641=EDGE_LOOP('',(#55180,#55181));
#10642=EDGE_LOOP('',(#55182,#55183));
#10643=EDGE_LOOP('',(#55184,#55185));
#10644=EDGE_LOOP('',(#55186,#55187));
#10645=EDGE_LOOP('',(#55188,#55189));
#10646=EDGE_LOOP('',(#55190,#55191));
#10647=EDGE_LOOP('',(#55192,#55193));
#10648=EDGE_LOOP('',(#55194,#55195));
#10649=EDGE_LOOP('',(#55196,#55197));
#10650=EDGE_LOOP('',(#55198,#55199));
#10651=EDGE_LOOP('',(#55200,#55201));
#10652=EDGE_LOOP('',(#55202,#55203));
#10653=EDGE_LOOP('',(#55204,#55205,#55206,#55207,#55208,#55209,#55210,#55211));
#10654=EDGE_LOOP('',(#55212,#55213,#55214,#55215,#55216,#55217,#55218,#55219));
#10655=EDGE_LOOP('',(#55220,#55221,#55222,#55223,#55224,#55225,#55226,#55227));
#10656=EDGE_LOOP('',(#55228,#55229,#55230,#55231,#55232,#55233,#55234,#55235));
#10657=EDGE_LOOP('',(#55236));
#10658=EDGE_LOOP('',(#55237));
#10659=EDGE_LOOP('',(#55238,#55239,#55240,#55241,#55242,#55243));
#10660=EDGE_LOOP('',(#55244,#55245,#55246,#55247));
#10661=EDGE_LOOP('',(#55248,#55249,#55250,#55251,#55252,#55253));
#10662=EDGE_LOOP('',(#55254));
#10663=EDGE_LOOP('',(#55255,#55256,#55257,#55258));
#10664=EDGE_LOOP('',(#55259,#55260,#55261,#55262));
#10665=EDGE_LOOP('',(#55263,#55264,#55265,#55266));
#10666=EDGE_LOOP('',(#55267,#55268,#55269,#55270));
#10667=EDGE_LOOP('',(#55271,#55272,#55273,#55274));
#10668=EDGE_LOOP('',(#55275,#55276,#55277,#55278));
#10669=EDGE_LOOP('',(#55279,#55280,#55281,#55282));
#10670=EDGE_LOOP('',(#55283,#55284,#55285,#55286,#55287));
#10671=EDGE_LOOP('',(#55288,#55289,#55290,#55291));
#10672=EDGE_LOOP('',(#55292,#55293,#55294,#55295));
#10673=EDGE_LOOP('',(#55296,#55297,#55298,#55299));
#10674=EDGE_LOOP('',(#55300,#55301,#55302,#55303));
#10675=EDGE_LOOP('',(#55304,#55305,#55306,#55307));
#10676=EDGE_LOOP('',(#55308,#55309,#55310,#55311));
#10677=EDGE_LOOP('',(#55312,#55313,#55314,#55315));
#10678=EDGE_LOOP('',(#55316,#55317,#55318,#55319));
#10679=EDGE_LOOP('',(#55320,#55321,#55322,#55323,#55324,#55325,#55326,#55327,
#55328,#55329,#55330,#55331,#55332,#55333,#55334,#55335,#55336,#55337,#55338));
#10680=EDGE_LOOP('',(#55339,#55340,#55341,#55342,#55343));
#10681=EDGE_LOOP('',(#55344,#55345,#55346,#55347));
#10682=EDGE_LOOP('',(#55348,#55349,#55350,#55351,#55352,#55353,#55354,#55355,
#55356,#55357,#55358,#55359,#55360,#55361,#55362,#55363,#55364,#55365));
#10683=EDGE_LOOP('',(#55366,#55367,#55368,#55369));
#10684=EDGE_LOOP('',(#55370,#55371,#55372,#55373));
#10685=EDGE_LOOP('',(#55374,#55375,#55376,#55377));
#10686=EDGE_LOOP('',(#55378,#55379,#55380,#55381));
#10687=EDGE_LOOP('',(#55382,#55383,#55384,#55385));
#10688=EDGE_LOOP('',(#55386,#55387,#55388,#55389));
#10689=EDGE_LOOP('',(#55390,#55391,#55392,#55393,#55394,#55395));
#10690=EDGE_LOOP('',(#55396));
#10691=EDGE_LOOP('',(#55397,#55398,#55399,#55400,#55401,#55402));
#10692=EDGE_LOOP('',(#55403,#55404,#55405));
#10693=EDGE_LOOP('',(#55406,#55407,#55408,#55409,#55410,#55411));
#10694=EDGE_LOOP('',(#55412));
#10695=EDGE_LOOP('',(#55413,#55414,#55415,#55416,#55417,#55418));
#10696=EDGE_LOOP('',(#55419,#55420,#55421,#55422));
#10697=EDGE_LOOP('',(#55423,#55424,#55425,#55426));
#10698=EDGE_LOOP('',(#55427,#55428,#55429,#55430));
#10699=EDGE_LOOP('',(#55431,#55432,#55433,#55434));
#10700=EDGE_LOOP('',(#55435,#55436,#55437,#55438));
#10701=EDGE_LOOP('',(#55439,#55440,#55441,#55442));
#10702=EDGE_LOOP('',(#55443,#55444,#55445,#55446));
#10703=EDGE_LOOP('',(#55447,#55448,#55449,#55450));
#10704=EDGE_LOOP('',(#55451,#55452,#55453,#55454));
#10705=EDGE_LOOP('',(#55455,#55456,#55457,#55458));
#10706=EDGE_LOOP('',(#55459,#55460,#55461,#55462));
#10707=EDGE_LOOP('',(#55463,#55464,#55465,#55466));
#10708=EDGE_LOOP('',(#55467,#55468,#55469,#55470));
#10709=EDGE_LOOP('',(#55471,#55472,#55473,#55474));
#10710=EDGE_LOOP('',(#55475,#55476,#55477,#55478));
#10711=EDGE_LOOP('',(#55479,#55480,#55481,#55482));
#10712=EDGE_LOOP('',(#55483,#55484,#55485,#55486));
#10713=EDGE_LOOP('',(#55487,#55488,#55489,#55490));
#10714=EDGE_LOOP('',(#55491,#55492,#55493,#55494));
#10715=EDGE_LOOP('',(#55495,#55496,#55497,#55498));
#10716=EDGE_LOOP('',(#55499,#55500,#55501,#55502));
#10717=EDGE_LOOP('',(#55503,#55504,#55505,#55506));
#10718=EDGE_LOOP('',(#55507,#55508,#55509,#55510));
#10719=EDGE_LOOP('',(#55511,#55512,#55513,#55514));
#10720=EDGE_LOOP('',(#55515,#55516,#55517,#55518));
#10721=EDGE_LOOP('',(#55519,#55520,#55521,#55522,#55523));
#10722=EDGE_LOOP('',(#55524,#55525,#55526,#55527,#55528,#55529,#55530,#55531,
#55532,#55533,#55534,#55535,#55536,#55537,#55538,#55539,#55540,#55541,#55542,
#55543,#55544,#55545,#55546,#55547,#55548,#55549,#55550,#55551,#55552));
#10723=EDGE_LOOP('',(#55553,#55554,#55555,#55556,#55557));
#10724=EDGE_LOOP('',(#55558,#55559,#55560,#55561));
#10725=EDGE_LOOP('',(#55562,#55563,#55564,#55565,#55566,#55567,#55568,#55569,
#55570,#55571,#55572,#55573,#55574,#55575,#55576,#55577,#55578,#55579,#55580,
#55581,#55582,#55583,#55584,#55585,#55586,#55587,#55588,#55589,#55590));
#10726=EDGE_LOOP('',(#55591,#55592,#55593,#55594,#55595,#55596));
#10727=EDGE_LOOP('',(#55597,#55598,#55599,#55600));
#10728=EDGE_LOOP('',(#55601));
#10729=EDGE_LOOP('',(#55602));
#10730=EDGE_LOOP('',(#55603,#55604,#55605,#55606,#55607,#55608));
#10731=EDGE_LOOP('',(#55609));
#10732=EDGE_LOOP('',(#55610,#55611,#55612,#55613));
#10733=EDGE_LOOP('',(#55614,#55615,#55616));
#10734=EDGE_LOOP('',(#55617,#55618,#55619,#55620));
#10735=EDGE_LOOP('',(#55621,#55622,#55623,#55624,#55625,#55626,#55627,#55628,
#55629,#55630,#55631,#55632,#55633,#55634,#55635,#55636,#55637,#55638,#55639,
#55640,#55641,#55642,#55643,#55644,#55645,#55646,#55647,#55648,#55649,#55650,
#55651,#55652,#55653,#55654,#55655,#55656,#55657,#55658,#55659,#55660,#55661,
#55662,#55663,#55664,#55665,#55666,#55667,#55668,#55669,#55670,#55671,#55672,
#55673,#55674,#55675,#55676,#55677,#55678,#55679,#55680,#55681,#55682,#55683,
#55684,#55685,#55686,#55687,#55688,#55689,#55690,#55691,#55692,#55693,#55694,
#55695,#55696,#55697,#55698,#55699,#55700,#55701,#55702,#55703,#55704,#55705,
#55706,#55707,#55708,#55709,#55710,#55711,#55712,#55713,#55714,#55715,#55716,
#55717,#55718,#55719,#55720,#55721,#55722,#55723,#55724,#55725,#55726,#55727,
#55728,#55729,#55730,#55731,#55732,#55733,#55734,#55735,#55736,#55737,#55738,
#55739,#55740,#55741,#55742,#55743,#55744,#55745,#55746,#55747,#55748,#55749,
#55750,#55751,#55752,#55753,#55754,#55755,#55756,#55757,#55758,#55759,#55760,
#55761,#55762,#55763,#55764,#55765,#55766,#55767,#55768,#55769));
#10736=EDGE_LOOP('',(#55770,#55771,#55772,#55773));
#10737=EDGE_LOOP('',(#55774,#55775,#55776));
#10738=EDGE_LOOP('',(#55777,#55778,#55779,#55780));
#10739=EDGE_LOOP('',(#55781,#55782,#55783,#55784));
#10740=EDGE_LOOP('',(#55785,#55786,#55787));
#10741=EDGE_LOOP('',(#55788,#55789,#55790,#55791));
#10742=EDGE_LOOP('',(#55792,#55793,#55794,#55795));
#10743=EDGE_LOOP('',(#55796,#55797,#55798));
#10744=EDGE_LOOP('',(#55799,#55800,#55801,#55802));
#10745=EDGE_LOOP('',(#55803,#55804,#55805,#55806));
#10746=EDGE_LOOP('',(#55807,#55808,#55809));
#10747=EDGE_LOOP('',(#55810,#55811,#55812,#55813));
#10748=EDGE_LOOP('',(#55814,#55815,#55816,#55817));
#10749=EDGE_LOOP('',(#55818,#55819,#55820));
#10750=EDGE_LOOP('',(#55821,#55822,#55823,#55824));
#10751=EDGE_LOOP('',(#55825,#55826,#55827,#55828));
#10752=EDGE_LOOP('',(#55829,#55830,#55831));
#10753=EDGE_LOOP('',(#55832,#55833,#55834,#55835));
#10754=EDGE_LOOP('',(#55836,#55837,#55838,#55839));
#10755=EDGE_LOOP('',(#55840,#55841,#55842));
#10756=EDGE_LOOP('',(#55843,#55844,#55845,#55846));
#10757=EDGE_LOOP('',(#55847,#55848,#55849,#55850));
#10758=EDGE_LOOP('',(#55851,#55852,#55853));
#10759=EDGE_LOOP('',(#55854,#55855,#55856,#55857));
#10760=EDGE_LOOP('',(#55858,#55859,#55860,#55861));
#10761=EDGE_LOOP('',(#55862,#55863,#55864));
#10762=EDGE_LOOP('',(#55865,#55866,#55867,#55868));
#10763=EDGE_LOOP('',(#55869,#55870,#55871,#55872));
#10764=EDGE_LOOP('',(#55873,#55874,#55875));
#10765=EDGE_LOOP('',(#55876,#55877,#55878,#55879));
#10766=EDGE_LOOP('',(#55880,#55881,#55882,#55883));
#10767=EDGE_LOOP('',(#55884,#55885,#55886));
#10768=EDGE_LOOP('',(#55887,#55888,#55889,#55890));
#10769=EDGE_LOOP('',(#55891,#55892,#55893,#55894));
#10770=EDGE_LOOP('',(#55895,#55896,#55897));
#10771=EDGE_LOOP('',(#55898,#55899,#55900,#55901));
#10772=EDGE_LOOP('',(#55902,#55903,#55904,#55905));
#10773=EDGE_LOOP('',(#55906,#55907,#55908));
#10774=EDGE_LOOP('',(#55909,#55910,#55911,#55912));
#10775=EDGE_LOOP('',(#55913,#55914,#55915,#55916));
#10776=EDGE_LOOP('',(#55917,#55918,#55919));
#10777=EDGE_LOOP('',(#55920,#55921,#55922,#55923));
#10778=EDGE_LOOP('',(#55924,#55925,#55926,#55927));
#10779=EDGE_LOOP('',(#55928,#55929,#55930));
#10780=EDGE_LOOP('',(#55931,#55932,#55933,#55934));
#10781=EDGE_LOOP('',(#55935,#55936,#55937,#55938));
#10782=EDGE_LOOP('',(#55939,#55940,#55941));
#10783=EDGE_LOOP('',(#55942,#55943,#55944,#55945));
#10784=EDGE_LOOP('',(#55946,#55947,#55948,#55949));
#10785=EDGE_LOOP('',(#55950,#55951,#55952,#55953));
#10786=EDGE_LOOP('',(#55954,#55955,#55956,#55957));
#10787=EDGE_LOOP('',(#55958,#55959,#55960,#55961));
#10788=EDGE_LOOP('',(#55962,#55963,#55964));
#10789=EDGE_LOOP('',(#55965,#55966,#55967,#55968));
#10790=EDGE_LOOP('',(#55969,#55970,#55971,#55972));
#10791=EDGE_LOOP('',(#55973,#55974,#55975));
#10792=EDGE_LOOP('',(#55976,#55977,#55978,#55979));
#10793=EDGE_LOOP('',(#55980,#55981,#55982,#55983));
#10794=EDGE_LOOP('',(#55984,#55985,#55986));
#10795=EDGE_LOOP('',(#55987,#55988,#55989,#55990));
#10796=EDGE_LOOP('',(#55991,#55992,#55993,#55994));
#10797=EDGE_LOOP('',(#55995,#55996,#55997));
#10798=EDGE_LOOP('',(#55998,#55999,#56000,#56001));
#10799=EDGE_LOOP('',(#56002,#56003,#56004,#56005));
#10800=EDGE_LOOP('',(#56006,#56007,#56008));
#10801=EDGE_LOOP('',(#56009,#56010,#56011,#56012));
#10802=EDGE_LOOP('',(#56013,#56014,#56015,#56016));
#10803=EDGE_LOOP('',(#56017,#56018,#56019));
#10804=EDGE_LOOP('',(#56020,#56021,#56022,#56023));
#10805=EDGE_LOOP('',(#56024,#56025,#56026,#56027));
#10806=EDGE_LOOP('',(#56028,#56029,#56030));
#10807=EDGE_LOOP('',(#56031,#56032,#56033,#56034));
#10808=EDGE_LOOP('',(#56035,#56036,#56037,#56038));
#10809=EDGE_LOOP('',(#56039,#56040,#56041));
#10810=EDGE_LOOP('',(#56042,#56043,#56044,#56045));
#10811=EDGE_LOOP('',(#56046,#56047,#56048,#56049));
#10812=EDGE_LOOP('',(#56050,#56051,#56052));
#10813=EDGE_LOOP('',(#56053,#56054,#56055,#56056));
#10814=EDGE_LOOP('',(#56057,#56058,#56059,#56060));
#10815=EDGE_LOOP('',(#56061,#56062,#56063));
#10816=EDGE_LOOP('',(#56064,#56065,#56066,#56067));
#10817=EDGE_LOOP('',(#56068,#56069,#56070,#56071));
#10818=EDGE_LOOP('',(#56072,#56073,#56074));
#10819=EDGE_LOOP('',(#56075,#56076,#56077,#56078));
#10820=EDGE_LOOP('',(#56079,#56080,#56081,#56082));
#10821=EDGE_LOOP('',(#56083,#56084,#56085));
#10822=EDGE_LOOP('',(#56086,#56087,#56088,#56089));
#10823=EDGE_LOOP('',(#56090,#56091,#56092,#56093));
#10824=EDGE_LOOP('',(#56094,#56095,#56096));
#10825=EDGE_LOOP('',(#56097,#56098,#56099,#56100));
#10826=EDGE_LOOP('',(#56101,#56102,#56103,#56104));
#10827=EDGE_LOOP('',(#56105,#56106,#56107));
#10828=EDGE_LOOP('',(#56108,#56109,#56110,#56111));
#10829=EDGE_LOOP('',(#56112,#56113,#56114,#56115));
#10830=EDGE_LOOP('',(#56116,#56117,#56118));
#10831=EDGE_LOOP('',(#56119,#56120,#56121,#56122));
#10832=EDGE_LOOP('',(#56123,#56124,#56125,#56126));
#10833=EDGE_LOOP('',(#56127,#56128,#56129));
#10834=EDGE_LOOP('',(#56130,#56131,#56132,#56133));
#10835=EDGE_LOOP('',(#56134,#56135,#56136,#56137));
#10836=EDGE_LOOP('',(#56138,#56139,#56140));
#10837=EDGE_LOOP('',(#56141,#56142,#56143,#56144));
#10838=EDGE_LOOP('',(#56145,#56146,#56147,#56148));
#10839=EDGE_LOOP('',(#56149,#56150,#56151));
#10840=EDGE_LOOP('',(#56152,#56153,#56154,#56155));
#10841=EDGE_LOOP('',(#56156,#56157,#56158,#56159,#56160));
#10842=EDGE_LOOP('',(#56161,#56162,#56163,#56164,#56165,#56166,#56167,#56168,
#56169,#56170,#56171,#56172,#56173,#56174,#56175,#56176,#56177,#56178,#56179,
#56180,#56181,#56182,#56183,#56184,#56185,#56186,#56187,#56188,#56189,#56190,
#56191,#56192,#56193,#56194,#56195,#56196,#56197,#56198,#56199,#56200,#56201,
#56202,#56203,#56204,#56205,#56206,#56207,#56208,#56209,#56210,#56211,#56212,
#56213,#56214,#56215,#56216,#56217,#56218,#56219,#56220,#56221,#56222,#56223,
#56224,#56225,#56226,#56227,#56228,#56229,#56230,#56231,#56232,#56233,#56234,
#56235,#56236,#56237,#56238,#56239,#56240,#56241,#56242,#56243,#56244,#56245,
#56246,#56247,#56248,#56249,#56250,#56251,#56252,#56253,#56254,#56255,#56256,
#56257,#56258,#56259,#56260,#56261,#56262,#56263,#56264,#56265,#56266,#56267,
#56268,#56269,#56270,#56271));
#10843=EDGE_LOOP('',(#56272));
#10844=EDGE_LOOP('',(#56273));
#10845=EDGE_LOOP('',(#56274,#56275,#56276,#56277,#56278,#56279,#56280,#56281,
#56282,#56283,#56284,#56285,#56286,#56287,#56288,#56289,#56290,#56291,#56292,
#56293,#56294));
#10846=EDGE_LOOP('',(#56295,#56296,#56297,#56298));
#10847=EDGE_LOOP('',(#56299,#56300,#56301,#56302));
#10848=EDGE_LOOP('',(#56303,#56304,#56305,#56306));
#10849=EDGE_LOOP('',(#56307,#56308,#56309,#56310));
#10850=EDGE_LOOP('',(#56311,#56312,#56313,#56314));
#10851=EDGE_LOOP('',(#56315,#56316,#56317,#56318));
#10852=EDGE_LOOP('',(#56319,#56320,#56321,#56322,#56323,#56324,#56325,#56326));
#10853=EDGE_LOOP('',(#56327,#56328,#56329,#56330,#56331,#56332,#56333,#56334));
#10854=EDGE_LOOP('',(#56335,#56336,#56337,#56338,#56339,#56340,#56341,#56342));
#10855=EDGE_LOOP('',(#56343,#56344));
#10856=EDGE_LOOP('',(#56345,#56346));
#10857=EDGE_LOOP('',(#56347,#56348));
#10858=EDGE_LOOP('',(#56349,#56350));
#10859=EDGE_LOOP('',(#56351,#56352));
#10860=EDGE_LOOP('',(#56353,#56354));
#10861=EDGE_LOOP('',(#56355,#56356));
#10862=EDGE_LOOP('',(#56357,#56358));
#10863=EDGE_LOOP('',(#56359,#56360));
#10864=EDGE_LOOP('',(#56361,#56362));
#10865=EDGE_LOOP('',(#56363,#56364));
#10866=EDGE_LOOP('',(#56365,#56366));
#10867=EDGE_LOOP('',(#56367,#56368,#56369,#56370,#56371,#56372,#56373,#56374));
#10868=EDGE_LOOP('',(#56375,#56376,#56377,#56378,#56379,#56380,#56381,#56382));
#10869=EDGE_LOOP('',(#56383,#56384,#56385,#56386,#56387,#56388,#56389,#56390));
#10870=EDGE_LOOP('',(#56391,#56392,#56393,#56394,#56395,#56396,#56397,#56398));
#10871=EDGE_LOOP('',(#56399));
#10872=EDGE_LOOP('',(#56400,#56401,#56402,#56403));
#10873=EDGE_LOOP('',(#56404,#56405,#56406,#56407));
#10874=EDGE_LOOP('',(#56408,#56409,#56410,#56411));
#10875=EDGE_LOOP('',(#56412));
#10876=LINE('',#76158,#16910);
#10877=LINE('',#76163,#16911);
#10878=LINE('',#76175,#16912);
#10879=LINE('',#76190,#16913);
#10880=LINE('',#76205,#16914);
#10881=LINE('',#76220,#16915);
#10882=LINE('',#76235,#16916);
#10883=LINE('',#76250,#16917);
#10884=LINE('',#76278,#16918);
#10885=LINE('',#76283,#16919);
#10886=LINE('',#76295,#16920);
#10887=LINE('',#76310,#16921);
#10888=LINE('',#76325,#16922);
#10889=LINE('',#76340,#16923);
#10890=LINE('',#76355,#16924);
#10891=LINE('',#76370,#16925);
#10892=LINE('',#76385,#16926);
#10893=LINE('',#76400,#16927);
#10894=LINE('',#76415,#16928);
#10895=LINE('',#76430,#16929);
#10896=LINE('',#76459,#16930);
#10897=LINE('',#76464,#16931);
#10898=LINE('',#76476,#16932);
#10899=LINE('',#76491,#16933);
#10900=LINE('',#76506,#16934);
#10901=LINE('',#76521,#16935);
#10902=LINE('',#76536,#16936);
#10903=LINE('',#76551,#16937);
#10904=LINE('',#76579,#16938);
#10905=LINE('',#76584,#16939);
#10906=LINE('',#76596,#16940);
#10907=LINE('',#76611,#16941);
#10908=LINE('',#76626,#16942);
#10909=LINE('',#76641,#16943);
#10910=LINE('',#76656,#16944);
#10911=LINE('',#76671,#16945);
#10912=LINE('',#76686,#16946);
#10913=LINE('',#76701,#16947);
#10914=LINE('',#76716,#16948);
#10915=LINE('',#76731,#16949);
#10916=LINE('',#76746,#16950);
#10917=LINE('',#76761,#16951);
#10918=LINE('',#76776,#16952);
#10919=LINE('',#76791,#16953);
#10920=LINE('',#76806,#16954);
#10921=LINE('',#76821,#16955);
#10922=LINE('',#76836,#16956);
#10923=LINE('',#76851,#16957);
#10924=LINE('',#76866,#16958);
#10925=LINE('',#76872,#16959);
#10926=LINE('',#76874,#16960);
#10927=LINE('',#76875,#16961);
#10928=LINE('',#76903,#16962);
#10929=LINE('',#76908,#16963);
#10930=LINE('',#76920,#16964);
#10931=LINE('',#76935,#16965);
#10932=LINE('',#76950,#16966);
#10933=LINE('',#76965,#16967);
#10934=LINE('',#76980,#16968);
#10935=LINE('',#76995,#16969);
#10936=LINE('',#77023,#16970);
#10937=LINE('',#77028,#16971);
#10938=LINE('',#77040,#16972);
#10939=LINE('',#77055,#16973);
#10940=LINE('',#77070,#16974);
#10941=LINE('',#77085,#16975);
#10942=LINE('',#77100,#16976);
#10943=LINE('',#77115,#16977);
#10944=LINE('',#77130,#16978);
#10945=LINE('',#77145,#16979);
#10946=LINE('',#77160,#16980);
#10947=LINE('',#77175,#16981);
#10948=LINE('',#77204,#16982);
#10949=LINE('',#77209,#16983);
#10950=LINE('',#77221,#16984);
#10951=LINE('',#77236,#16985);
#10952=LINE('',#77251,#16986);
#10953=LINE('',#77266,#16987);
#10954=LINE('',#77281,#16988);
#10955=LINE('',#77296,#16989);
#10956=LINE('',#77324,#16990);
#10957=LINE('',#77329,#16991);
#10958=LINE('',#77341,#16992);
#10959=LINE('',#77356,#16993);
#10960=LINE('',#77371,#16994);
#10961=LINE('',#77386,#16995);
#10962=LINE('',#77401,#16996);
#10963=LINE('',#77416,#16997);
#10964=LINE('',#77431,#16998);
#10965=LINE('',#77459,#16999);
#10966=LINE('',#77464,#17000);
#10967=LINE('',#77476,#17001);
#10968=LINE('',#77491,#17002);
#10969=LINE('',#77506,#17003);
#10970=LINE('',#77521,#17004);
#10971=LINE('',#77536,#17005);
#10972=LINE('',#77551,#17006);
#10973=LINE('',#77566,#17007);
#10974=LINE('',#77581,#17008);
#10975=LINE('',#77596,#17009);
#10976=LINE('',#77611,#17010);
#10977=LINE('',#77626,#17011);
#10978=LINE('',#77641,#17012);
#10979=LINE('',#77656,#17013);
#10980=LINE('',#77671,#17014);
#10981=LINE('',#77703,#17015);
#10982=LINE('',#77708,#17016);
#10983=LINE('',#77720,#17017);
#10984=LINE('',#77735,#17018);
#10985=LINE('',#77750,#17019);
#10986=LINE('',#77765,#17020);
#10987=LINE('',#77780,#17021);
#10988=LINE('',#77795,#17022);
#10989=LINE('',#77823,#17023);
#10990=LINE('',#77828,#17024);
#10991=LINE('',#77840,#17025);
#10992=LINE('',#77855,#17026);
#10993=LINE('',#77870,#17027);
#10994=LINE('',#77885,#17028);
#10995=LINE('',#77900,#17029);
#10996=LINE('',#77915,#17030);
#10997=LINE('',#77930,#17031);
#10998=LINE('',#77945,#17032);
#10999=LINE('',#77960,#17033);
#11000=LINE('',#77975,#17034);
#11001=LINE('',#78004,#17035);
#11002=LINE('',#78009,#17036);
#11003=LINE('',#78021,#17037);
#11004=LINE('',#78036,#17038);
#11005=LINE('',#78042,#17039);
#11006=LINE('',#78044,#17040);
#11007=LINE('',#78045,#17041);
#11008=LINE('',#78057,#17042);
#11009=LINE('',#78072,#17043);
#11010=LINE('',#78087,#17044);
#11011=LINE('',#78093,#17045);
#11012=LINE('',#78095,#17046);
#11013=LINE('',#78096,#17047);
#11014=LINE('',#78099,#17048);
#11015=LINE('',#78101,#17049);
#11016=LINE('',#78102,#17050);
#11017=LINE('',#78105,#17051);
#11018=LINE('',#78107,#17052);
#11019=LINE('',#78108,#17053);
#11020=LINE('',#78110,#17054);
#11021=LINE('',#78111,#17055);
#11022=LINE('',#78126,#17056);
#11023=LINE('',#78131,#17057);
#11024=LINE('',#78143,#17058);
#11025=LINE('',#78158,#17059);
#11026=LINE('',#78173,#17060);
#11027=LINE('',#78188,#17061);
#11028=LINE('',#78203,#17062);
#11029=LINE('',#78218,#17063);
#11030=LINE('',#78246,#17064);
#11031=LINE('',#78251,#17065);
#11032=LINE('',#78263,#17066);
#11033=LINE('',#78278,#17067);
#11034=LINE('',#78293,#17068);
#11035=LINE('',#78308,#17069);
#11036=LINE('',#78323,#17070);
#11037=LINE('',#78338,#17071);
#11038=LINE('',#78353,#17072);
#11039=LINE('',#78368,#17073);
#11040=LINE('',#78383,#17074);
#11041=LINE('',#78398,#17075);
#11042=LINE('',#78427,#17076);
#11043=LINE('',#78432,#17077);
#11044=LINE('',#78444,#17078);
#11045=LINE('',#78459,#17079);
#11046=LINE('',#78474,#17080);
#11047=LINE('',#78489,#17081);
#11048=LINE('',#78504,#17082);
#11049=LINE('',#78519,#17083);
#11050=LINE('',#78534,#17084);
#11051=LINE('',#78562,#17085);
#11052=LINE('',#78567,#17086);
#11053=LINE('',#78579,#17087);
#11054=LINE('',#78594,#17088);
#11055=LINE('',#78609,#17089);
#11056=LINE('',#78624,#17090);
#11057=LINE('',#78639,#17091);
#11058=LINE('',#78654,#17092);
#11059=LINE('',#78669,#17093);
#11060=LINE('',#78684,#17094);
#11061=LINE('',#78699,#17095);
#11062=LINE('',#78714,#17096);
#11063=LINE('',#78729,#17097);
#11064=LINE('',#78744,#17098);
#11065=LINE('',#78759,#17099);
#11066=LINE('',#78774,#17100);
#11067=LINE('',#78789,#17101);
#11068=LINE('',#78804,#17102);
#11069=LINE('',#78810,#17103);
#11070=LINE('',#78812,#17104);
#11071=LINE('',#78813,#17105);
#11072=LINE('',#78841,#17106);
#11073=LINE('',#78846,#17107);
#11074=LINE('',#78858,#17108);
#11075=LINE('',#78873,#17109);
#11076=LINE('',#78888,#17110);
#11077=LINE('',#78903,#17111);
#11078=LINE('',#78918,#17112);
#11079=LINE('',#78933,#17113);
#11080=LINE('',#78961,#17114);
#11081=LINE('',#78966,#17115);
#11082=LINE('',#78978,#17116);
#11083=LINE('',#78993,#17117);
#11084=LINE('',#79008,#17118);
#11085=LINE('',#79023,#17119);
#11086=LINE('',#79038,#17120);
#11087=LINE('',#79053,#17121);
#11088=LINE('',#79068,#17122);
#11089=LINE('',#79083,#17123);
#11090=LINE('',#79098,#17124);
#11091=LINE('',#79113,#17125);
#11092=LINE('',#79142,#17126);
#11093=LINE('',#79147,#17127);
#11094=LINE('',#79159,#17128);
#11095=LINE('',#79174,#17129);
#11096=LINE('',#79189,#17130);
#11097=LINE('',#79204,#17131);
#11098=LINE('',#79219,#17132);
#11099=LINE('',#79225,#17133);
#11100=LINE('',#79227,#17134);
#11101=LINE('',#79228,#17135);
#11102=LINE('',#79231,#17136);
#11103=LINE('',#79233,#17137);
#11104=LINE('',#79234,#17138);
#11105=LINE('',#79237,#17139);
#11106=LINE('',#79239,#17140);
#11107=LINE('',#79240,#17141);
#11108=LINE('',#79243,#17142);
#11109=LINE('',#79245,#17143);
#11110=LINE('',#79246,#17144);
#11111=LINE('',#79249,#17145);
#11112=LINE('',#79251,#17146);
#11113=LINE('',#79252,#17147);
#11114=LINE('',#79255,#17148);
#11115=LINE('',#79257,#17149);
#11116=LINE('',#79258,#17150);
#11117=LINE('',#79270,#17151);
#11118=LINE('',#79285,#17152);
#11119=LINE('',#79300,#17153);
#11120=LINE('',#79315,#17154);
#11121=LINE('',#79330,#17155);
#11122=LINE('',#79345,#17156);
#11123=LINE('',#79360,#17157);
#11124=LINE('',#79375,#17158);
#11125=LINE('',#79381,#17159);
#11126=LINE('',#79383,#17160);
#11127=LINE('',#79384,#17161);
#11128=LINE('',#79411,#17162);
#11129=LINE('',#79416,#17163);
#11130=LINE('',#79428,#17164);
#11131=LINE('',#79443,#17165);
#11132=LINE('',#79458,#17166);
#11133=LINE('',#79473,#17167);
#11134=LINE('',#79488,#17168);
#11135=LINE('',#79503,#17169);
#11136=LINE('',#79531,#17170);
#11137=LINE('',#79536,#17171);
#11138=LINE('',#79548,#17172);
#11139=LINE('',#79563,#17173);
#11140=LINE('',#79578,#17174);
#11141=LINE('',#79593,#17175);
#11142=LINE('',#79608,#17176);
#11143=LINE('',#79623,#17177);
#11144=LINE('',#79638,#17178);
#11145=LINE('',#79653,#17179);
#11146=LINE('',#79668,#17180);
#11147=LINE('',#79683,#17181);
#11148=LINE('',#79703,#17182);
#11149=LINE('',#79705,#17183);
#11150=LINE('',#79707,#17184);
#11151=LINE('',#79708,#17185);
#11152=LINE('',#79711,#17186);
#11153=LINE('',#79713,#17187);
#11154=LINE('',#79714,#17188);
#11155=LINE('',#79716,#17189);
#11156=LINE('',#79717,#17190);
#11157=LINE('',#79721,#17191);
#11158=LINE('',#79723,#17192);
#11159=LINE('',#79725,#17193);
#11160=LINE('',#79726,#17194);
#11161=LINE('',#79729,#17195);
#11162=LINE('',#79731,#17196);
#11163=LINE('',#79732,#17197);
#11164=LINE('',#79735,#17198);
#11165=LINE('',#79737,#17199);
#11166=LINE('',#79738,#17200);
#11167=LINE('',#79741,#17201);
#11168=LINE('',#79743,#17202);
#11169=LINE('',#79744,#17203);
#11170=LINE('',#79747,#17204);
#11171=LINE('',#79749,#17205);
#11172=LINE('',#79750,#17206);
#11173=LINE('',#79753,#17207);
#11174=LINE('',#79755,#17208);
#11175=LINE('',#79756,#17209);
#11176=LINE('',#79759,#17210);
#11177=LINE('',#79761,#17211);
#11178=LINE('',#79762,#17212);
#11179=LINE('',#79765,#17213);
#11180=LINE('',#79767,#17214);
#11181=LINE('',#79768,#17215);
#11182=LINE('',#79771,#17216);
#11183=LINE('',#79773,#17217);
#11184=LINE('',#79774,#17218);
#11185=LINE('',#79777,#17219);
#11186=LINE('',#79779,#17220);
#11187=LINE('',#79780,#17221);
#11188=LINE('',#79782,#17222);
#11189=LINE('',#79783,#17223);
#11190=LINE('',#79799,#17224);
#11191=LINE('',#79804,#17225);
#11192=LINE('',#79816,#17226);
#11193=LINE('',#79831,#17227);
#11194=LINE('',#79846,#17228);
#11195=LINE('',#79861,#17229);
#11196=LINE('',#79876,#17230);
#11197=LINE('',#79891,#17231);
#11198=LINE('',#79919,#17232);
#11199=LINE('',#79924,#17233);
#11200=LINE('',#79936,#17234);
#11201=LINE('',#79951,#17235);
#11202=LINE('',#79966,#17236);
#11203=LINE('',#79981,#17237);
#11204=LINE('',#79996,#17238);
#11205=LINE('',#80011,#17239);
#11206=LINE('',#80026,#17240);
#11207=LINE('',#80041,#17241);
#11208=LINE('',#80056,#17242);
#11209=LINE('',#80071,#17243);
#11210=LINE('',#80100,#17244);
#11211=LINE('',#80105,#17245);
#11212=LINE('',#80117,#17246);
#11213=LINE('',#80132,#17247);
#11214=LINE('',#80147,#17248);
#11215=LINE('',#80162,#17249);
#11216=LINE('',#80177,#17250);
#11217=LINE('',#80192,#17251);
#11218=LINE('',#80207,#17252);
#11219=LINE('',#80222,#17253);
#11220=LINE('',#80237,#17254);
#11221=LINE('',#80252,#17255);
#11222=LINE('',#80267,#17256);
#11223=LINE('',#80273,#17257);
#11224=LINE('',#80275,#17258);
#11225=LINE('',#80276,#17259);
#11226=LINE('',#80288,#17260);
#11227=LINE('',#80303,#17261);
#11228=LINE('',#80318,#17262);
#11229=LINE('',#80333,#17263);
#11230=LINE('',#80348,#17264);
#11231=LINE('',#80363,#17265);
#11232=LINE('',#80378,#17266);
#11233=LINE('',#80384,#17267);
#11234=LINE('',#80386,#17268);
#11235=LINE('',#80387,#17269);
#11236=LINE('',#80399,#17270);
#11237=LINE('',#80414,#17271);
#11238=LINE('',#80429,#17272);
#11239=LINE('',#80444,#17273);
#11240=LINE('',#80459,#17274);
#11241=LINE('',#80474,#17275);
#11242=LINE('',#80489,#17276);
#11243=LINE('',#80495,#17277);
#11244=LINE('',#80497,#17278);
#11245=LINE('',#80498,#17279);
#11246=LINE('',#80525,#17280);
#11247=LINE('',#80530,#17281);
#11248=LINE('',#80542,#17282);
#11249=LINE('',#80557,#17283);
#11250=LINE('',#80572,#17284);
#11251=LINE('',#80587,#17285);
#11252=LINE('',#80602,#17286);
#11253=LINE('',#80617,#17287);
#11254=LINE('',#80645,#17288);
#11255=LINE('',#80650,#17289);
#11256=LINE('',#80662,#17290);
#11257=LINE('',#80677,#17291);
#11258=LINE('',#80692,#17292);
#11259=LINE('',#80707,#17293);
#11260=LINE('',#80722,#17294);
#11261=LINE('',#80737,#17295);
#11262=LINE('',#80752,#17296);
#11263=LINE('',#80767,#17297);
#11264=LINE('',#80782,#17298);
#11265=LINE('',#80797,#17299);
#11266=LINE('',#80826,#17300);
#11267=LINE('',#80831,#17301);
#11268=LINE('',#80843,#17302);
#11269=LINE('',#80858,#17303);
#11270=LINE('',#80873,#17304);
#11271=LINE('',#80888,#17305);
#11272=LINE('',#80903,#17306);
#11273=LINE('',#80918,#17307);
#11274=LINE('',#80933,#17308);
#11275=LINE('',#80948,#17309);
#11276=LINE('',#80954,#17310);
#11277=LINE('',#80956,#17311);
#11278=LINE('',#80957,#17312);
#11279=LINE('',#80969,#17313);
#11280=LINE('',#80984,#17314);
#11281=LINE('',#80999,#17315);
#11282=LINE('',#81014,#17316);
#11283=LINE('',#81029,#17317);
#11284=LINE('',#81044,#17318);
#11285=LINE('',#81059,#17319);
#11286=LINE('',#81074,#17320);
#11287=LINE('',#81089,#17321);
#11288=LINE('',#81095,#17322);
#11289=LINE('',#81097,#17323);
#11290=LINE('',#81098,#17324);
#11291=LINE('',#81101,#17325);
#11292=LINE('',#81103,#17326);
#11293=LINE('',#81104,#17327);
#11294=LINE('',#81106,#17328);
#11295=LINE('',#81107,#17329);
#11296=LINE('',#81122,#17330);
#11297=LINE('',#81127,#17331);
#11298=LINE('',#81139,#17332);
#11299=LINE('',#81154,#17333);
#11300=LINE('',#81169,#17334);
#11301=LINE('',#81184,#17335);
#11302=LINE('',#81199,#17336);
#11303=LINE('',#81214,#17337);
#11304=LINE('',#81242,#17338);
#11305=LINE('',#81247,#17339);
#11306=LINE('',#81259,#17340);
#11307=LINE('',#81274,#17341);
#11308=LINE('',#81289,#17342);
#11309=LINE('',#81304,#17343);
#11310=LINE('',#81319,#17344);
#11311=LINE('',#81334,#17345);
#11312=LINE('',#81349,#17346);
#11313=LINE('',#81364,#17347);
#11314=LINE('',#81379,#17348);
#11315=LINE('',#81394,#17349);
#11316=LINE('',#81414,#17350);
#11317=LINE('',#81416,#17351);
#11318=LINE('',#81418,#17352);
#11319=LINE('',#81419,#17353);
#11320=LINE('',#81431,#17354);
#11321=LINE('',#81446,#17355);
#11322=LINE('',#81452,#17356);
#11323=LINE('',#81454,#17357);
#11324=LINE('',#81455,#17358);
#11325=LINE('',#81467,#17359);
#11326=LINE('',#81482,#17360);
#11327=LINE('',#81488,#17361);
#11328=LINE('',#81490,#17362);
#11329=LINE('',#81491,#17363);
#11330=LINE('',#81494,#17364);
#11331=LINE('',#81496,#17365);
#11332=LINE('',#81497,#17366);
#11333=LINE('',#81499,#17367);
#11334=LINE('',#81500,#17368);
#11335=LINE('',#81515,#17369);
#11336=LINE('',#81520,#17370);
#11337=LINE('',#81532,#17371);
#11338=LINE('',#81547,#17372);
#11339=LINE('',#81562,#17373);
#11340=LINE('',#81577,#17374);
#11341=LINE('',#81592,#17375);
#11342=LINE('',#81607,#17376);
#11343=LINE('',#81635,#17377);
#11344=LINE('',#81640,#17378);
#11345=LINE('',#81652,#17379);
#11346=LINE('',#81667,#17380);
#11347=LINE('',#81682,#17381);
#11348=LINE('',#81697,#17382);
#11349=LINE('',#81712,#17383);
#11350=LINE('',#81727,#17384);
#11351=LINE('',#81742,#17385);
#11352=LINE('',#81757,#17386);
#11353=LINE('',#81772,#17387);
#11354=LINE('',#81787,#17388);
#11355=LINE('',#81817,#17389);
#11356=LINE('',#81822,#17390);
#11357=LINE('',#81834,#17391);
#11358=LINE('',#81849,#17392);
#11359=LINE('',#81864,#17393);
#11360=LINE('',#81879,#17394);
#11361=LINE('',#81894,#17395);
#11362=LINE('',#81909,#17396);
#11363=LINE('',#81937,#17397);
#11364=LINE('',#81942,#17398);
#11365=LINE('',#81954,#17399);
#11366=LINE('',#81969,#17400);
#11367=LINE('',#81984,#17401);
#11368=LINE('',#81999,#17402);
#11369=LINE('',#82014,#17403);
#11370=LINE('',#82029,#17404);
#11371=LINE('',#82044,#17405);
#11372=LINE('',#82059,#17406);
#11373=LINE('',#82074,#17407);
#11374=LINE('',#82089,#17408);
#11375=LINE('',#82109,#17409);
#11376=LINE('',#82111,#17410);
#11377=LINE('',#82113,#17411);
#11378=LINE('',#82114,#17412);
#11379=LINE('',#82126,#17413);
#11380=LINE('',#82141,#17414);
#11381=LINE('',#82147,#17415);
#11382=LINE('',#82149,#17416);
#11383=LINE('',#82150,#17417);
#11384=LINE('',#82162,#17418);
#11385=LINE('',#82177,#17419);
#11386=LINE('',#82183,#17420);
#11387=LINE('',#82185,#17421);
#11388=LINE('',#82186,#17422);
#11389=LINE('',#82189,#17423);
#11390=LINE('',#82191,#17424);
#11391=LINE('',#82192,#17425);
#11392=LINE('',#82194,#17426);
#11393=LINE('',#82195,#17427);
#11394=LINE('',#82210,#17428);
#11395=LINE('',#82215,#17429);
#11396=LINE('',#82227,#17430);
#11397=LINE('',#82242,#17431);
#11398=LINE('',#82257,#17432);
#11399=LINE('',#82272,#17433);
#11400=LINE('',#82287,#17434);
#11401=LINE('',#82302,#17435);
#11402=LINE('',#82330,#17436);
#11403=LINE('',#82335,#17437);
#11404=LINE('',#82347,#17438);
#11405=LINE('',#82362,#17439);
#11406=LINE('',#82377,#17440);
#11407=LINE('',#82392,#17441);
#11408=LINE('',#82407,#17442);
#11409=LINE('',#82422,#17443);
#11410=LINE('',#82437,#17444);
#11411=LINE('',#82452,#17445);
#11412=LINE('',#82467,#17446);
#11413=LINE('',#82482,#17447);
#11414=LINE('',#82511,#17448);
#11415=LINE('',#82516,#17449);
#11416=LINE('',#82528,#17450);
#11417=LINE('',#82543,#17451);
#11418=LINE('',#82558,#17452);
#11419=LINE('',#82573,#17453);
#11420=LINE('',#82588,#17454);
#11421=LINE('',#82603,#17455);
#11422=LINE('',#82618,#17456);
#11423=LINE('',#82633,#17457);
#11424=LINE('',#82639,#17458);
#11425=LINE('',#82641,#17459);
#11426=LINE('',#82642,#17460);
#11427=LINE('',#82654,#17461);
#11428=LINE('',#82669,#17462);
#11429=LINE('',#82684,#17463);
#11430=LINE('',#82699,#17464);
#11431=LINE('',#82714,#17465);
#11432=LINE('',#82729,#17466);
#11433=LINE('',#82744,#17467);
#11434=LINE('',#82759,#17468);
#11435=LINE('',#82774,#17469);
#11436=LINE('',#82780,#17470);
#11437=LINE('',#82782,#17471);
#11438=LINE('',#82783,#17472);
#11439=LINE('',#82786,#17473);
#11440=LINE('',#82788,#17474);
#11441=LINE('',#82789,#17475);
#11442=LINE('',#82791,#17476);
#11443=LINE('',#82792,#17477);
#11444=LINE('',#82807,#17478);
#11445=LINE('',#82812,#17479);
#11446=LINE('',#82824,#17480);
#11447=LINE('',#82839,#17481);
#11448=LINE('',#82854,#17482);
#11449=LINE('',#82869,#17483);
#11450=LINE('',#82884,#17484);
#11451=LINE('',#82899,#17485);
#11452=LINE('',#82927,#17486);
#11453=LINE('',#82932,#17487);
#11454=LINE('',#82944,#17488);
#11455=LINE('',#82959,#17489);
#11456=LINE('',#82974,#17490);
#11457=LINE('',#82989,#17491);
#11458=LINE('',#83004,#17492);
#11459=LINE('',#83019,#17493);
#11460=LINE('',#83034,#17494);
#11461=LINE('',#83049,#17495);
#11462=LINE('',#83064,#17496);
#11463=LINE('',#83079,#17497);
#11464=LINE('',#83108,#17498);
#11465=LINE('',#83113,#17499);
#11466=LINE('',#83125,#17500);
#11467=LINE('',#83140,#17501);
#11468=LINE('',#83155,#17502);
#11469=LINE('',#83170,#17503);
#11470=LINE('',#83185,#17504);
#11471=LINE('',#83200,#17505);
#11472=LINE('',#83215,#17506);
#11473=LINE('',#83230,#17507);
#11474=LINE('',#83245,#17508);
#11475=LINE('',#83260,#17509);
#11476=LINE('',#83275,#17510);
#11477=LINE('',#83281,#17511);
#11478=LINE('',#83283,#17512);
#11479=LINE('',#83284,#17513);
#11480=LINE('',#83296,#17514);
#11481=LINE('',#83311,#17515);
#11482=LINE('',#83326,#17516);
#11483=LINE('',#83341,#17517);
#11484=LINE('',#83356,#17518);
#11485=LINE('',#83371,#17519);
#11486=LINE('',#83386,#17520);
#11487=LINE('',#83392,#17521);
#11488=LINE('',#83394,#17522);
#11489=LINE('',#83395,#17523);
#11490=LINE('',#83407,#17524);
#11491=LINE('',#83422,#17525);
#11492=LINE('',#83437,#17526);
#11493=LINE('',#83452,#17527);
#11494=LINE('',#83467,#17528);
#11495=LINE('',#83482,#17529);
#11496=LINE('',#83497,#17530);
#11497=LINE('',#83503,#17531);
#11498=LINE('',#83505,#17532);
#11499=LINE('',#83506,#17533);
#11500=LINE('',#83533,#17534);
#11501=LINE('',#83538,#17535);
#11502=LINE('',#83550,#17536);
#11503=LINE('',#83565,#17537);
#11504=LINE('',#83580,#17538);
#11505=LINE('',#83595,#17539);
#11506=LINE('',#83610,#17540);
#11507=LINE('',#83625,#17541);
#11508=LINE('',#83653,#17542);
#11509=LINE('',#83658,#17543);
#11510=LINE('',#83670,#17544);
#11511=LINE('',#83685,#17545);
#11512=LINE('',#83700,#17546);
#11513=LINE('',#83715,#17547);
#11514=LINE('',#83730,#17548);
#11515=LINE('',#83745,#17549);
#11516=LINE('',#83760,#17550);
#11517=LINE('',#83775,#17551);
#11518=LINE('',#83790,#17552);
#11519=LINE('',#83805,#17553);
#11520=LINE('',#83825,#17554);
#11521=LINE('',#83827,#17555);
#11522=LINE('',#83829,#17556);
#11523=LINE('',#83830,#17557);
#11524=LINE('',#83833,#17558);
#11525=LINE('',#83835,#17559);
#11526=LINE('',#83836,#17560);
#11527=LINE('',#83838,#17561);
#11528=LINE('',#83839,#17562);
#11529=LINE('',#83843,#17563);
#11530=LINE('',#83845,#17564);
#11531=LINE('',#83847,#17565);
#11532=LINE('',#83848,#17566);
#11533=LINE('',#83851,#17567);
#11534=LINE('',#83853,#17568);
#11535=LINE('',#83854,#17569);
#11536=LINE('',#83857,#17570);
#11537=LINE('',#83859,#17571);
#11538=LINE('',#83860,#17572);
#11539=LINE('',#83863,#17573);
#11540=LINE('',#83865,#17574);
#11541=LINE('',#83866,#17575);
#11542=LINE('',#83869,#17576);
#11543=LINE('',#83871,#17577);
#11544=LINE('',#83872,#17578);
#11545=LINE('',#83875,#17579);
#11546=LINE('',#83877,#17580);
#11547=LINE('',#83878,#17581);
#11548=LINE('',#83881,#17582);
#11549=LINE('',#83883,#17583);
#11550=LINE('',#83884,#17584);
#11551=LINE('',#83887,#17585);
#11552=LINE('',#83889,#17586);
#11553=LINE('',#83890,#17587);
#11554=LINE('',#83893,#17588);
#11555=LINE('',#83895,#17589);
#11556=LINE('',#83896,#17590);
#11557=LINE('',#83899,#17591);
#11558=LINE('',#83901,#17592);
#11559=LINE('',#83902,#17593);
#11560=LINE('',#83904,#17594);
#11561=LINE('',#83905,#17595);
#11562=LINE('',#83921,#17596);
#11563=LINE('',#83926,#17597);
#11564=LINE('',#83938,#17598);
#11565=LINE('',#83953,#17599);
#11566=LINE('',#83968,#17600);
#11567=LINE('',#83983,#17601);
#11568=LINE('',#83998,#17602);
#11569=LINE('',#84013,#17603);
#11570=LINE('',#84041,#17604);
#11571=LINE('',#84046,#17605);
#11572=LINE('',#84058,#17606);
#11573=LINE('',#84073,#17607);
#11574=LINE('',#84088,#17608);
#11575=LINE('',#84103,#17609);
#11576=LINE('',#84118,#17610);
#11577=LINE('',#84133,#17611);
#11578=LINE('',#84148,#17612);
#11579=LINE('',#84163,#17613);
#11580=LINE('',#84178,#17614);
#11581=LINE('',#84193,#17615);
#11582=LINE('',#84222,#17616);
#11583=LINE('',#84227,#17617);
#11584=LINE('',#84239,#17618);
#11585=LINE('',#84254,#17619);
#11586=LINE('',#84269,#17620);
#11587=LINE('',#84284,#17621);
#11588=LINE('',#84299,#17622);
#11589=LINE('',#84305,#17623);
#11590=LINE('',#84307,#17624);
#11591=LINE('',#84308,#17625);
#11592=LINE('',#84311,#17626);
#11593=LINE('',#84313,#17627);
#11594=LINE('',#84314,#17628);
#11595=LINE('',#84317,#17629);
#11596=LINE('',#84319,#17630);
#11597=LINE('',#84320,#17631);
#11598=LINE('',#84323,#17632);
#11599=LINE('',#84325,#17633);
#11600=LINE('',#84326,#17634);
#11601=LINE('',#84329,#17635);
#11602=LINE('',#84331,#17636);
#11603=LINE('',#84332,#17637);
#11604=LINE('',#84335,#17638);
#11605=LINE('',#84337,#17639);
#11606=LINE('',#84338,#17640);
#11607=LINE('',#84350,#17641);
#11608=LINE('',#84365,#17642);
#11609=LINE('',#84380,#17643);
#11610=LINE('',#84395,#17644);
#11611=LINE('',#84410,#17645);
#11612=LINE('',#84425,#17646);
#11613=LINE('',#84440,#17647);
#11614=LINE('',#84455,#17648);
#11615=LINE('',#84461,#17649);
#11616=LINE('',#84463,#17650);
#11617=LINE('',#84464,#17651);
#11618=LINE('',#84491,#17652);
#11619=LINE('',#84496,#17653);
#11620=LINE('',#84508,#17654);
#11621=LINE('',#84523,#17655);
#11622=LINE('',#84538,#17656);
#11623=LINE('',#84553,#17657);
#11624=LINE('',#84568,#17658);
#11625=LINE('',#84583,#17659);
#11626=LINE('',#84611,#17660);
#11627=LINE('',#84616,#17661);
#11628=LINE('',#84628,#17662);
#11629=LINE('',#84643,#17663);
#11630=LINE('',#84658,#17664);
#11631=LINE('',#84673,#17665);
#11632=LINE('',#84688,#17666);
#11633=LINE('',#84703,#17667);
#11634=LINE('',#84718,#17668);
#11635=LINE('',#84733,#17669);
#11636=LINE('',#84748,#17670);
#11637=LINE('',#84763,#17671);
#11638=LINE('',#84792,#17672);
#11639=LINE('',#84797,#17673);
#11640=LINE('',#84809,#17674);
#11641=LINE('',#84824,#17675);
#11642=LINE('',#84839,#17676);
#11643=LINE('',#84854,#17677);
#11644=LINE('',#84869,#17678);
#11645=LINE('',#84884,#17679);
#11646=LINE('',#84899,#17680);
#11647=LINE('',#84927,#17681);
#11648=LINE('',#84932,#17682);
#11649=LINE('',#84944,#17683);
#11650=LINE('',#84959,#17684);
#11651=LINE('',#84974,#17685);
#11652=LINE('',#84989,#17686);
#11653=LINE('',#85004,#17687);
#11654=LINE('',#85019,#17688);
#11655=LINE('',#85034,#17689);
#11656=LINE('',#85049,#17690);
#11657=LINE('',#85064,#17691);
#11658=LINE('',#85079,#17692);
#11659=LINE('',#85094,#17693);
#11660=LINE('',#85109,#17694);
#11661=LINE('',#85124,#17695);
#11662=LINE('',#85139,#17696);
#11663=LINE('',#85154,#17697);
#11664=LINE('',#85169,#17698);
#11665=LINE('',#85175,#17699);
#11666=LINE('',#85177,#17700);
#11667=LINE('',#85178,#17701);
#11668=LINE('',#85206,#17702);
#11669=LINE('',#85211,#17703);
#11670=LINE('',#85223,#17704);
#11671=LINE('',#85238,#17705);
#11672=LINE('',#85253,#17706);
#11673=LINE('',#85268,#17707);
#11674=LINE('',#85283,#17708);
#11675=LINE('',#85298,#17709);
#11676=LINE('',#85326,#17710);
#11677=LINE('',#85331,#17711);
#11678=LINE('',#85343,#17712);
#11679=LINE('',#85358,#17713);
#11680=LINE('',#85373,#17714);
#11681=LINE('',#85388,#17715);
#11682=LINE('',#85403,#17716);
#11683=LINE('',#85418,#17717);
#11684=LINE('',#85433,#17718);
#11685=LINE('',#85448,#17719);
#11686=LINE('',#85463,#17720);
#11687=LINE('',#85478,#17721);
#11688=LINE('',#85507,#17722);
#11689=LINE('',#85512,#17723);
#11690=LINE('',#85524,#17724);
#11691=LINE('',#85539,#17725);
#11692=LINE('',#85545,#17726);
#11693=LINE('',#85547,#17727);
#11694=LINE('',#85548,#17728);
#11695=LINE('',#85560,#17729);
#11696=LINE('',#85575,#17730);
#11697=LINE('',#85590,#17731);
#11698=LINE('',#85596,#17732);
#11699=LINE('',#85598,#17733);
#11700=LINE('',#85599,#17734);
#11701=LINE('',#85602,#17735);
#11702=LINE('',#85604,#17736);
#11703=LINE('',#85605,#17737);
#11704=LINE('',#85608,#17738);
#11705=LINE('',#85610,#17739);
#11706=LINE('',#85611,#17740);
#11707=LINE('',#85613,#17741);
#11708=LINE('',#85614,#17742);
#11709=LINE('',#85629,#17743);
#11710=LINE('',#85634,#17744);
#11711=LINE('',#85646,#17745);
#11712=LINE('',#85661,#17746);
#11713=LINE('',#85676,#17747);
#11714=LINE('',#85691,#17748);
#11715=LINE('',#85706,#17749);
#11716=LINE('',#85721,#17750);
#11717=LINE('',#85749,#17751);
#11718=LINE('',#85754,#17752);
#11719=LINE('',#85766,#17753);
#11720=LINE('',#85781,#17754);
#11721=LINE('',#85796,#17755);
#11722=LINE('',#85811,#17756);
#11723=LINE('',#85826,#17757);
#11724=LINE('',#85841,#17758);
#11725=LINE('',#85856,#17759);
#11726=LINE('',#85871,#17760);
#11727=LINE('',#85886,#17761);
#11728=LINE('',#85901,#17762);
#11729=LINE('',#85930,#17763);
#11730=LINE('',#85935,#17764);
#11731=LINE('',#85947,#17765);
#11732=LINE('',#85962,#17766);
#11733=LINE('',#85977,#17767);
#11734=LINE('',#85992,#17768);
#11735=LINE('',#86007,#17769);
#11736=LINE('',#86022,#17770);
#11737=LINE('',#86050,#17771);
#11738=LINE('',#86055,#17772);
#11739=LINE('',#86067,#17773);
#11740=LINE('',#86082,#17774);
#11741=LINE('',#86097,#17775);
#11742=LINE('',#86112,#17776);
#11743=LINE('',#86127,#17777);
#11744=LINE('',#86142,#17778);
#11745=LINE('',#86157,#17779);
#11746=LINE('',#86185,#17780);
#11747=LINE('',#86190,#17781);
#11748=LINE('',#86202,#17782);
#11749=LINE('',#86217,#17783);
#11750=LINE('',#86232,#17784);
#11751=LINE('',#86247,#17785);
#11752=LINE('',#86262,#17786);
#11753=LINE('',#86277,#17787);
#11754=LINE('',#86292,#17788);
#11755=LINE('',#86307,#17789);
#11756=LINE('',#86322,#17790);
#11757=LINE('',#86337,#17791);
#11758=LINE('',#86352,#17792);
#11759=LINE('',#86367,#17793);
#11760=LINE('',#86382,#17794);
#11761=LINE('',#86397,#17795);
#11762=LINE('',#86429,#17796);
#11763=LINE('',#86434,#17797);
#11764=LINE('',#86446,#17798);
#11765=LINE('',#86461,#17799);
#11766=LINE('',#86476,#17800);
#11767=LINE('',#86491,#17801);
#11768=LINE('',#86506,#17802);
#11769=LINE('',#86521,#17803);
#11770=LINE('',#86549,#17804);
#11771=LINE('',#86554,#17805);
#11772=LINE('',#86566,#17806);
#11773=LINE('',#86581,#17807);
#11774=LINE('',#86596,#17808);
#11775=LINE('',#86611,#17809);
#11776=LINE('',#86626,#17810);
#11777=LINE('',#86641,#17811);
#11778=LINE('',#86656,#17812);
#11779=LINE('',#86671,#17813);
#11780=LINE('',#86686,#17814);
#11781=LINE('',#86701,#17815);
#11782=LINE('',#86730,#17816);
#11783=LINE('',#86735,#17817);
#11784=LINE('',#86747,#17818);
#11785=LINE('',#86762,#17819);
#11786=LINE('',#86777,#17820);
#11787=LINE('',#86792,#17821);
#11788=LINE('',#86807,#17822);
#11789=LINE('',#86822,#17823);
#11790=LINE('',#86850,#17824);
#11791=LINE('',#86855,#17825);
#11792=LINE('',#86867,#17826);
#11793=LINE('',#86882,#17827);
#11794=LINE('',#86897,#17828);
#11795=LINE('',#86912,#17829);
#11796=LINE('',#86927,#17830);
#11797=LINE('',#86942,#17831);
#11798=LINE('',#86957,#17832);
#11799=LINE('',#86972,#17833);
#11800=LINE('',#86987,#17834);
#11801=LINE('',#87002,#17835);
#11802=LINE('',#87017,#17836);
#11803=LINE('',#87032,#17837);
#11804=LINE('',#87047,#17838);
#11805=LINE('',#87062,#17839);
#11806=LINE('',#87077,#17840);
#11807=LINE('',#87092,#17841);
#11808=LINE('',#87107,#17842);
#11809=LINE('',#87122,#17843);
#11810=LINE('',#87137,#17844);
#11811=LINE('',#87143,#17845);
#11812=LINE('',#87145,#17846);
#11813=LINE('',#87146,#17847);
#11814=LINE('',#87165,#17848);
#11815=LINE('',#87167,#17849);
#11816=LINE('',#87169,#17850);
#11817=LINE('',#87170,#17851);
#11818=LINE('',#87173,#17852);
#11819=LINE('',#87175,#17853);
#11820=LINE('',#87176,#17854);
#11821=LINE('',#87179,#17855);
#11822=LINE('',#87181,#17856);
#11823=LINE('',#87182,#17857);
#11824=LINE('',#87184,#17858);
#11825=LINE('',#87185,#17859);
#11826=LINE('',#87190,#17860);
#11827=LINE('',#87192,#17861);
#11828=LINE('',#87194,#17862);
#11829=LINE('',#87195,#17863);
#11830=LINE('',#87198,#17864);
#11831=LINE('',#87200,#17865);
#11832=LINE('',#87201,#17866);
#11833=LINE('',#87204,#17867);
#11834=LINE('',#87206,#17868);
#11835=LINE('',#87207,#17869);
#11836=LINE('',#87209,#17870);
#11837=LINE('',#87210,#17871);
#11838=LINE('',#87215,#17872);
#11839=LINE('',#87217,#17873);
#11840=LINE('',#87219,#17874);
#11841=LINE('',#87220,#17875);
#11842=LINE('',#87223,#17876);
#11843=LINE('',#87225,#17877);
#11844=LINE('',#87226,#17878);
#11845=LINE('',#87229,#17879);
#11846=LINE('',#87231,#17880);
#11847=LINE('',#87232,#17881);
#11848=LINE('',#87234,#17882);
#11849=LINE('',#87235,#17883);
#11850=LINE('',#87240,#17884);
#11851=LINE('',#87242,#17885);
#11852=LINE('',#87244,#17886);
#11853=LINE('',#87245,#17887);
#11854=LINE('',#87248,#17888);
#11855=LINE('',#87250,#17889);
#11856=LINE('',#87251,#17890);
#11857=LINE('',#87254,#17891);
#11858=LINE('',#87256,#17892);
#11859=LINE('',#87257,#17893);
#11860=LINE('',#87259,#17894);
#11861=LINE('',#87260,#17895);
#11862=LINE('',#87265,#17896);
#11863=LINE('',#87267,#17897);
#11864=LINE('',#87269,#17898);
#11865=LINE('',#87270,#17899);
#11866=LINE('',#87273,#17900);
#11867=LINE('',#87275,#17901);
#11868=LINE('',#87276,#17902);
#11869=LINE('',#87279,#17903);
#11870=LINE('',#87281,#17904);
#11871=LINE('',#87282,#17905);
#11872=LINE('',#87284,#17906);
#11873=LINE('',#87285,#17907);
#11874=LINE('',#87290,#17908);
#11875=LINE('',#87292,#17909);
#11876=LINE('',#87294,#17910);
#11877=LINE('',#87295,#17911);
#11878=LINE('',#87298,#17912);
#11879=LINE('',#87300,#17913);
#11880=LINE('',#87301,#17914);
#11881=LINE('',#87304,#17915);
#11882=LINE('',#87306,#17916);
#11883=LINE('',#87307,#17917);
#11884=LINE('',#87309,#17918);
#11885=LINE('',#87310,#17919);
#11886=LINE('',#87315,#17920);
#11887=LINE('',#87317,#17921);
#11888=LINE('',#87319,#17922);
#11889=LINE('',#87320,#17923);
#11890=LINE('',#87323,#17924);
#11891=LINE('',#87325,#17925);
#11892=LINE('',#87326,#17926);
#11893=LINE('',#87329,#17927);
#11894=LINE('',#87331,#17928);
#11895=LINE('',#87332,#17929);
#11896=LINE('',#87334,#17930);
#11897=LINE('',#87335,#17931);
#11898=LINE('',#87340,#17932);
#11899=LINE('',#87342,#17933);
#11900=LINE('',#87344,#17934);
#11901=LINE('',#87345,#17935);
#11902=LINE('',#87348,#17936);
#11903=LINE('',#87350,#17937);
#11904=LINE('',#87351,#17938);
#11905=LINE('',#87354,#17939);
#11906=LINE('',#87356,#17940);
#11907=LINE('',#87357,#17941);
#11908=LINE('',#87359,#17942);
#11909=LINE('',#87360,#17943);
#11910=LINE('',#87365,#17944);
#11911=LINE('',#87367,#17945);
#11912=LINE('',#87369,#17946);
#11913=LINE('',#87370,#17947);
#11914=LINE('',#87373,#17948);
#11915=LINE('',#87375,#17949);
#11916=LINE('',#87376,#17950);
#11917=LINE('',#87379,#17951);
#11918=LINE('',#87381,#17952);
#11919=LINE('',#87382,#17953);
#11920=LINE('',#87384,#17954);
#11921=LINE('',#87385,#17955);
#11922=LINE('',#87390,#17956);
#11923=LINE('',#87392,#17957);
#11924=LINE('',#87394,#17958);
#11925=LINE('',#87395,#17959);
#11926=LINE('',#87398,#17960);
#11927=LINE('',#87400,#17961);
#11928=LINE('',#87401,#17962);
#11929=LINE('',#87404,#17963);
#11930=LINE('',#87406,#17964);
#11931=LINE('',#87407,#17965);
#11932=LINE('',#87409,#17966);
#11933=LINE('',#87410,#17967);
#11934=LINE('',#87415,#17968);
#11935=LINE('',#87417,#17969);
#11936=LINE('',#87419,#17970);
#11937=LINE('',#87420,#17971);
#11938=LINE('',#87423,#17972);
#11939=LINE('',#87425,#17973);
#11940=LINE('',#87426,#17974);
#11941=LINE('',#87429,#17975);
#11942=LINE('',#87431,#17976);
#11943=LINE('',#87432,#17977);
#11944=LINE('',#87434,#17978);
#11945=LINE('',#87435,#17979);
#11946=LINE('',#87440,#17980);
#11947=LINE('',#87442,#17981);
#11948=LINE('',#87444,#17982);
#11949=LINE('',#87445,#17983);
#11950=LINE('',#87448,#17984);
#11951=LINE('',#87450,#17985);
#11952=LINE('',#87451,#17986);
#11953=LINE('',#87454,#17987);
#11954=LINE('',#87456,#17988);
#11955=LINE('',#87457,#17989);
#11956=LINE('',#87459,#17990);
#11957=LINE('',#87460,#17991);
#11958=LINE('',#87465,#17992);
#11959=LINE('',#87467,#17993);
#11960=LINE('',#87469,#17994);
#11961=LINE('',#87470,#17995);
#11962=LINE('',#87473,#17996);
#11963=LINE('',#87475,#17997);
#11964=LINE('',#87476,#17998);
#11965=LINE('',#87479,#17999);
#11966=LINE('',#87481,#18000);
#11967=LINE('',#87482,#18001);
#11968=LINE('',#87484,#18002);
#11969=LINE('',#87485,#18003);
#11970=LINE('',#87490,#18004);
#11971=LINE('',#87492,#18005);
#11972=LINE('',#87494,#18006);
#11973=LINE('',#87495,#18007);
#11974=LINE('',#87498,#18008);
#11975=LINE('',#87500,#18009);
#11976=LINE('',#87501,#18010);
#11977=LINE('',#87504,#18011);
#11978=LINE('',#87506,#18012);
#11979=LINE('',#87507,#18013);
#11980=LINE('',#87509,#18014);
#11981=LINE('',#87510,#18015);
#11982=LINE('',#87515,#18016);
#11983=LINE('',#87517,#18017);
#11984=LINE('',#87519,#18018);
#11985=LINE('',#87520,#18019);
#11986=LINE('',#87523,#18020);
#11987=LINE('',#87525,#18021);
#11988=LINE('',#87526,#18022);
#11989=LINE('',#87529,#18023);
#11990=LINE('',#87531,#18024);
#11991=LINE('',#87532,#18025);
#11992=LINE('',#87534,#18026);
#11993=LINE('',#87535,#18027);
#11994=LINE('',#87540,#18028);
#11995=LINE('',#87542,#18029);
#11996=LINE('',#87544,#18030);
#11997=LINE('',#87545,#18031);
#11998=LINE('',#87548,#18032);
#11999=LINE('',#87550,#18033);
#12000=LINE('',#87551,#18034);
#12001=LINE('',#87554,#18035);
#12002=LINE('',#87556,#18036);
#12003=LINE('',#87557,#18037);
#12004=LINE('',#87559,#18038);
#12005=LINE('',#87560,#18039);
#12006=LINE('',#87565,#18040);
#12007=LINE('',#87567,#18041);
#12008=LINE('',#87569,#18042);
#12009=LINE('',#87570,#18043);
#12010=LINE('',#87573,#18044);
#12011=LINE('',#87575,#18045);
#12012=LINE('',#87576,#18046);
#12013=LINE('',#87579,#18047);
#12014=LINE('',#87581,#18048);
#12015=LINE('',#87582,#18049);
#12016=LINE('',#87584,#18050);
#12017=LINE('',#87585,#18051);
#12018=LINE('',#87590,#18052);
#12019=LINE('',#87592,#18053);
#12020=LINE('',#87594,#18054);
#12021=LINE('',#87595,#18055);
#12022=LINE('',#87598,#18056);
#12023=LINE('',#87600,#18057);
#12024=LINE('',#87601,#18058);
#12025=LINE('',#87604,#18059);
#12026=LINE('',#87606,#18060);
#12027=LINE('',#87607,#18061);
#12028=LINE('',#87609,#18062);
#12029=LINE('',#87610,#18063);
#12030=LINE('',#87615,#18064);
#12031=LINE('',#87617,#18065);
#12032=LINE('',#87619,#18066);
#12033=LINE('',#87620,#18067);
#12034=LINE('',#87623,#18068);
#12035=LINE('',#87625,#18069);
#12036=LINE('',#87626,#18070);
#12037=LINE('',#87629,#18071);
#12038=LINE('',#87631,#18072);
#12039=LINE('',#87632,#18073);
#12040=LINE('',#87634,#18074);
#12041=LINE('',#87635,#18075);
#12042=LINE('',#87640,#18076);
#12043=LINE('',#87642,#18077);
#12044=LINE('',#87644,#18078);
#12045=LINE('',#87645,#18079);
#12046=LINE('',#87648,#18080);
#12047=LINE('',#87650,#18081);
#12048=LINE('',#87651,#18082);
#12049=LINE('',#87654,#18083);
#12050=LINE('',#87656,#18084);
#12051=LINE('',#87657,#18085);
#12052=LINE('',#87659,#18086);
#12053=LINE('',#87660,#18087);
#12054=LINE('',#87665,#18088);
#12055=LINE('',#87667,#18089);
#12056=LINE('',#87669,#18090);
#12057=LINE('',#87670,#18091);
#12058=LINE('',#87673,#18092);
#12059=LINE('',#87675,#18093);
#12060=LINE('',#87676,#18094);
#12061=LINE('',#87679,#18095);
#12062=LINE('',#87681,#18096);
#12063=LINE('',#87682,#18097);
#12064=LINE('',#87684,#18098);
#12065=LINE('',#87685,#18099);
#12066=LINE('',#87690,#18100);
#12067=LINE('',#87692,#18101);
#12068=LINE('',#87694,#18102);
#12069=LINE('',#87695,#18103);
#12070=LINE('',#87698,#18104);
#12071=LINE('',#87700,#18105);
#12072=LINE('',#87701,#18106);
#12073=LINE('',#87704,#18107);
#12074=LINE('',#87706,#18108);
#12075=LINE('',#87707,#18109);
#12076=LINE('',#87709,#18110);
#12077=LINE('',#87710,#18111);
#12078=LINE('',#87715,#18112);
#12079=LINE('',#87717,#18113);
#12080=LINE('',#87719,#18114);
#12081=LINE('',#87720,#18115);
#12082=LINE('',#87723,#18116);
#12083=LINE('',#87725,#18117);
#12084=LINE('',#87726,#18118);
#12085=LINE('',#87729,#18119);
#12086=LINE('',#87731,#18120);
#12087=LINE('',#87732,#18121);
#12088=LINE('',#87734,#18122);
#12089=LINE('',#87735,#18123);
#12090=LINE('',#87740,#18124);
#12091=LINE('',#87742,#18125);
#12092=LINE('',#87744,#18126);
#12093=LINE('',#87745,#18127);
#12094=LINE('',#87748,#18128);
#12095=LINE('',#87750,#18129);
#12096=LINE('',#87751,#18130);
#12097=LINE('',#87754,#18131);
#12098=LINE('',#87756,#18132);
#12099=LINE('',#87757,#18133);
#12100=LINE('',#87759,#18134);
#12101=LINE('',#87760,#18135);
#12102=LINE('',#87765,#18136);
#12103=LINE('',#87767,#18137);
#12104=LINE('',#87769,#18138);
#12105=LINE('',#87770,#18139);
#12106=LINE('',#87773,#18140);
#12107=LINE('',#87775,#18141);
#12108=LINE('',#87776,#18142);
#12109=LINE('',#87779,#18143);
#12110=LINE('',#87781,#18144);
#12111=LINE('',#87782,#18145);
#12112=LINE('',#87784,#18146);
#12113=LINE('',#87785,#18147);
#12114=LINE('',#87790,#18148);
#12115=LINE('',#87792,#18149);
#12116=LINE('',#87794,#18150);
#12117=LINE('',#87795,#18151);
#12118=LINE('',#87798,#18152);
#12119=LINE('',#87800,#18153);
#12120=LINE('',#87801,#18154);
#12121=LINE('',#87804,#18155);
#12122=LINE('',#87806,#18156);
#12123=LINE('',#87807,#18157);
#12124=LINE('',#87809,#18158);
#12125=LINE('',#87810,#18159);
#12126=LINE('',#87815,#18160);
#12127=LINE('',#87817,#18161);
#12128=LINE('',#87819,#18162);
#12129=LINE('',#87820,#18163);
#12130=LINE('',#87823,#18164);
#12131=LINE('',#87825,#18165);
#12132=LINE('',#87826,#18166);
#12133=LINE('',#87829,#18167);
#12134=LINE('',#87831,#18168);
#12135=LINE('',#87832,#18169);
#12136=LINE('',#87834,#18170);
#12137=LINE('',#87835,#18171);
#12138=LINE('',#87840,#18172);
#12139=LINE('',#87842,#18173);
#12140=LINE('',#87844,#18174);
#12141=LINE('',#87845,#18175);
#12142=LINE('',#87848,#18176);
#12143=LINE('',#87850,#18177);
#12144=LINE('',#87851,#18178);
#12145=LINE('',#87854,#18179);
#12146=LINE('',#87856,#18180);
#12147=LINE('',#87857,#18181);
#12148=LINE('',#87859,#18182);
#12149=LINE('',#87860,#18183);
#12150=LINE('',#87865,#18184);
#12151=LINE('',#87867,#18185);
#12152=LINE('',#87869,#18186);
#12153=LINE('',#87870,#18187);
#12154=LINE('',#87873,#18188);
#12155=LINE('',#87875,#18189);
#12156=LINE('',#87876,#18190);
#12157=LINE('',#87879,#18191);
#12158=LINE('',#87881,#18192);
#12159=LINE('',#87882,#18193);
#12160=LINE('',#87884,#18194);
#12161=LINE('',#87885,#18195);
#12162=LINE('',#87890,#18196);
#12163=LINE('',#87892,#18197);
#12164=LINE('',#87894,#18198);
#12165=LINE('',#87895,#18199);
#12166=LINE('',#87898,#18200);
#12167=LINE('',#87900,#18201);
#12168=LINE('',#87901,#18202);
#12169=LINE('',#87904,#18203);
#12170=LINE('',#87906,#18204);
#12171=LINE('',#87907,#18205);
#12172=LINE('',#87909,#18206);
#12173=LINE('',#87910,#18207);
#12174=LINE('',#87915,#18208);
#12175=LINE('',#87917,#18209);
#12176=LINE('',#87919,#18210);
#12177=LINE('',#87920,#18211);
#12178=LINE('',#87923,#18212);
#12179=LINE('',#87925,#18213);
#12180=LINE('',#87926,#18214);
#12181=LINE('',#87929,#18215);
#12182=LINE('',#87931,#18216);
#12183=LINE('',#87932,#18217);
#12184=LINE('',#87934,#18218);
#12185=LINE('',#87935,#18219);
#12186=LINE('',#87940,#18220);
#12187=LINE('',#87942,#18221);
#12188=LINE('',#87944,#18222);
#12189=LINE('',#87945,#18223);
#12190=LINE('',#87948,#18224);
#12191=LINE('',#87950,#18225);
#12192=LINE('',#87951,#18226);
#12193=LINE('',#87954,#18227);
#12194=LINE('',#87956,#18228);
#12195=LINE('',#87957,#18229);
#12196=LINE('',#87959,#18230);
#12197=LINE('',#87960,#18231);
#12198=LINE('',#87965,#18232);
#12199=LINE('',#87967,#18233);
#12200=LINE('',#87969,#18234);
#12201=LINE('',#87970,#18235);
#12202=LINE('',#87973,#18236);
#12203=LINE('',#87975,#18237);
#12204=LINE('',#87976,#18238);
#12205=LINE('',#87979,#18239);
#12206=LINE('',#87981,#18240);
#12207=LINE('',#87982,#18241);
#12208=LINE('',#87984,#18242);
#12209=LINE('',#87985,#18243);
#12210=LINE('',#87990,#18244);
#12211=LINE('',#87992,#18245);
#12212=LINE('',#87994,#18246);
#12213=LINE('',#87995,#18247);
#12214=LINE('',#87998,#18248);
#12215=LINE('',#88000,#18249);
#12216=LINE('',#88001,#18250);
#12217=LINE('',#88004,#18251);
#12218=LINE('',#88006,#18252);
#12219=LINE('',#88007,#18253);
#12220=LINE('',#88009,#18254);
#12221=LINE('',#88010,#18255);
#12222=LINE('',#88015,#18256);
#12223=LINE('',#88017,#18257);
#12224=LINE('',#88019,#18258);
#12225=LINE('',#88020,#18259);
#12226=LINE('',#88023,#18260);
#12227=LINE('',#88025,#18261);
#12228=LINE('',#88026,#18262);
#12229=LINE('',#88029,#18263);
#12230=LINE('',#88031,#18264);
#12231=LINE('',#88032,#18265);
#12232=LINE('',#88034,#18266);
#12233=LINE('',#88035,#18267);
#12234=LINE('',#88040,#18268);
#12235=LINE('',#88042,#18269);
#12236=LINE('',#88044,#18270);
#12237=LINE('',#88045,#18271);
#12238=LINE('',#88048,#18272);
#12239=LINE('',#88050,#18273);
#12240=LINE('',#88051,#18274);
#12241=LINE('',#88054,#18275);
#12242=LINE('',#88056,#18276);
#12243=LINE('',#88057,#18277);
#12244=LINE('',#88059,#18278);
#12245=LINE('',#88060,#18279);
#12246=LINE('',#88065,#18280);
#12247=LINE('',#88067,#18281);
#12248=LINE('',#88069,#18282);
#12249=LINE('',#88070,#18283);
#12250=LINE('',#88073,#18284);
#12251=LINE('',#88075,#18285);
#12252=LINE('',#88076,#18286);
#12253=LINE('',#88079,#18287);
#12254=LINE('',#88081,#18288);
#12255=LINE('',#88082,#18289);
#12256=LINE('',#88084,#18290);
#12257=LINE('',#88085,#18291);
#12258=LINE('',#88090,#18292);
#12259=LINE('',#88092,#18293);
#12260=LINE('',#88094,#18294);
#12261=LINE('',#88095,#18295);
#12262=LINE('',#88098,#18296);
#12263=LINE('',#88100,#18297);
#12264=LINE('',#88101,#18298);
#12265=LINE('',#88104,#18299);
#12266=LINE('',#88106,#18300);
#12267=LINE('',#88107,#18301);
#12268=LINE('',#88109,#18302);
#12269=LINE('',#88110,#18303);
#12270=LINE('',#88115,#18304);
#12271=LINE('',#88117,#18305);
#12272=LINE('',#88119,#18306);
#12273=LINE('',#88120,#18307);
#12274=LINE('',#88123,#18308);
#12275=LINE('',#88125,#18309);
#12276=LINE('',#88126,#18310);
#12277=LINE('',#88129,#18311);
#12278=LINE('',#88131,#18312);
#12279=LINE('',#88132,#18313);
#12280=LINE('',#88134,#18314);
#12281=LINE('',#88135,#18315);
#12282=LINE('',#88140,#18316);
#12283=LINE('',#88142,#18317);
#12284=LINE('',#88144,#18318);
#12285=LINE('',#88145,#18319);
#12286=LINE('',#88148,#18320);
#12287=LINE('',#88150,#18321);
#12288=LINE('',#88151,#18322);
#12289=LINE('',#88154,#18323);
#12290=LINE('',#88156,#18324);
#12291=LINE('',#88157,#18325);
#12292=LINE('',#88159,#18326);
#12293=LINE('',#88160,#18327);
#12294=LINE('',#88165,#18328);
#12295=LINE('',#88167,#18329);
#12296=LINE('',#88169,#18330);
#12297=LINE('',#88170,#18331);
#12298=LINE('',#88173,#18332);
#12299=LINE('',#88175,#18333);
#12300=LINE('',#88176,#18334);
#12301=LINE('',#88179,#18335);
#12302=LINE('',#88181,#18336);
#12303=LINE('',#88182,#18337);
#12304=LINE('',#88184,#18338);
#12305=LINE('',#88185,#18339);
#12306=LINE('',#88190,#18340);
#12307=LINE('',#88192,#18341);
#12308=LINE('',#88194,#18342);
#12309=LINE('',#88195,#18343);
#12310=LINE('',#88198,#18344);
#12311=LINE('',#88200,#18345);
#12312=LINE('',#88201,#18346);
#12313=LINE('',#88204,#18347);
#12314=LINE('',#88206,#18348);
#12315=LINE('',#88207,#18349);
#12316=LINE('',#88209,#18350);
#12317=LINE('',#88210,#18351);
#12318=LINE('',#88215,#18352);
#12319=LINE('',#88217,#18353);
#12320=LINE('',#88219,#18354);
#12321=LINE('',#88220,#18355);
#12322=LINE('',#88223,#18356);
#12323=LINE('',#88225,#18357);
#12324=LINE('',#88226,#18358);
#12325=LINE('',#88229,#18359);
#12326=LINE('',#88231,#18360);
#12327=LINE('',#88232,#18361);
#12328=LINE('',#88234,#18362);
#12329=LINE('',#88235,#18363);
#12330=LINE('',#88240,#18364);
#12331=LINE('',#88242,#18365);
#12332=LINE('',#88244,#18366);
#12333=LINE('',#88245,#18367);
#12334=LINE('',#88248,#18368);
#12335=LINE('',#88250,#18369);
#12336=LINE('',#88251,#18370);
#12337=LINE('',#88254,#18371);
#12338=LINE('',#88256,#18372);
#12339=LINE('',#88257,#18373);
#12340=LINE('',#88259,#18374);
#12341=LINE('',#88260,#18375);
#12342=LINE('',#88265,#18376);
#12343=LINE('',#88267,#18377);
#12344=LINE('',#88269,#18378);
#12345=LINE('',#88270,#18379);
#12346=LINE('',#88273,#18380);
#12347=LINE('',#88275,#18381);
#12348=LINE('',#88276,#18382);
#12349=LINE('',#88279,#18383);
#12350=LINE('',#88281,#18384);
#12351=LINE('',#88282,#18385);
#12352=LINE('',#88284,#18386);
#12353=LINE('',#88285,#18387);
#12354=LINE('',#88290,#18388);
#12355=LINE('',#88292,#18389);
#12356=LINE('',#88294,#18390);
#12357=LINE('',#88295,#18391);
#12358=LINE('',#88298,#18392);
#12359=LINE('',#88300,#18393);
#12360=LINE('',#88301,#18394);
#12361=LINE('',#88304,#18395);
#12362=LINE('',#88306,#18396);
#12363=LINE('',#88307,#18397);
#12364=LINE('',#88309,#18398);
#12365=LINE('',#88310,#18399);
#12366=LINE('',#88315,#18400);
#12367=LINE('',#88317,#18401);
#12368=LINE('',#88319,#18402);
#12369=LINE('',#88320,#18403);
#12370=LINE('',#88323,#18404);
#12371=LINE('',#88325,#18405);
#12372=LINE('',#88326,#18406);
#12373=LINE('',#88329,#18407);
#12374=LINE('',#88331,#18408);
#12375=LINE('',#88332,#18409);
#12376=LINE('',#88334,#18410);
#12377=LINE('',#88335,#18411);
#12378=LINE('',#88340,#18412);
#12379=LINE('',#88342,#18413);
#12380=LINE('',#88344,#18414);
#12381=LINE('',#88345,#18415);
#12382=LINE('',#88348,#18416);
#12383=LINE('',#88350,#18417);
#12384=LINE('',#88351,#18418);
#12385=LINE('',#88354,#18419);
#12386=LINE('',#88356,#18420);
#12387=LINE('',#88357,#18421);
#12388=LINE('',#88359,#18422);
#12389=LINE('',#88360,#18423);
#12390=LINE('',#88365,#18424);
#12391=LINE('',#88367,#18425);
#12392=LINE('',#88369,#18426);
#12393=LINE('',#88370,#18427);
#12394=LINE('',#88373,#18428);
#12395=LINE('',#88375,#18429);
#12396=LINE('',#88376,#18430);
#12397=LINE('',#88379,#18431);
#12398=LINE('',#88381,#18432);
#12399=LINE('',#88382,#18433);
#12400=LINE('',#88384,#18434);
#12401=LINE('',#88385,#18435);
#12402=LINE('',#88390,#18436);
#12403=LINE('',#88392,#18437);
#12404=LINE('',#88394,#18438);
#12405=LINE('',#88395,#18439);
#12406=LINE('',#88398,#18440);
#12407=LINE('',#88400,#18441);
#12408=LINE('',#88401,#18442);
#12409=LINE('',#88404,#18443);
#12410=LINE('',#88406,#18444);
#12411=LINE('',#88407,#18445);
#12412=LINE('',#88409,#18446);
#12413=LINE('',#88410,#18447);
#12414=LINE('',#88415,#18448);
#12415=LINE('',#88417,#18449);
#12416=LINE('',#88419,#18450);
#12417=LINE('',#88420,#18451);
#12418=LINE('',#88423,#18452);
#12419=LINE('',#88425,#18453);
#12420=LINE('',#88426,#18454);
#12421=LINE('',#88429,#18455);
#12422=LINE('',#88431,#18456);
#12423=LINE('',#88432,#18457);
#12424=LINE('',#88434,#18458);
#12425=LINE('',#88435,#18459);
#12426=LINE('',#88440,#18460);
#12427=LINE('',#88442,#18461);
#12428=LINE('',#88444,#18462);
#12429=LINE('',#88445,#18463);
#12430=LINE('',#88448,#18464);
#12431=LINE('',#88450,#18465);
#12432=LINE('',#88451,#18466);
#12433=LINE('',#88454,#18467);
#12434=LINE('',#88456,#18468);
#12435=LINE('',#88457,#18469);
#12436=LINE('',#88459,#18470);
#12437=LINE('',#88460,#18471);
#12438=LINE('',#88465,#18472);
#12439=LINE('',#88467,#18473);
#12440=LINE('',#88469,#18474);
#12441=LINE('',#88470,#18475);
#12442=LINE('',#88473,#18476);
#12443=LINE('',#88475,#18477);
#12444=LINE('',#88476,#18478);
#12445=LINE('',#88479,#18479);
#12446=LINE('',#88481,#18480);
#12447=LINE('',#88482,#18481);
#12448=LINE('',#88484,#18482);
#12449=LINE('',#88485,#18483);
#12450=LINE('',#88490,#18484);
#12451=LINE('',#88492,#18485);
#12452=LINE('',#88494,#18486);
#12453=LINE('',#88495,#18487);
#12454=LINE('',#88498,#18488);
#12455=LINE('',#88500,#18489);
#12456=LINE('',#88501,#18490);
#12457=LINE('',#88504,#18491);
#12458=LINE('',#88506,#18492);
#12459=LINE('',#88507,#18493);
#12460=LINE('',#88509,#18494);
#12461=LINE('',#88510,#18495);
#12462=LINE('',#88515,#18496);
#12463=LINE('',#88517,#18497);
#12464=LINE('',#88519,#18498);
#12465=LINE('',#88520,#18499);
#12466=LINE('',#88523,#18500);
#12467=LINE('',#88525,#18501);
#12468=LINE('',#88526,#18502);
#12469=LINE('',#88529,#18503);
#12470=LINE('',#88531,#18504);
#12471=LINE('',#88532,#18505);
#12472=LINE('',#88534,#18506);
#12473=LINE('',#88535,#18507);
#12474=LINE('',#88540,#18508);
#12475=LINE('',#88542,#18509);
#12476=LINE('',#88544,#18510);
#12477=LINE('',#88545,#18511);
#12478=LINE('',#88548,#18512);
#12479=LINE('',#88550,#18513);
#12480=LINE('',#88551,#18514);
#12481=LINE('',#88554,#18515);
#12482=LINE('',#88556,#18516);
#12483=LINE('',#88557,#18517);
#12484=LINE('',#88559,#18518);
#12485=LINE('',#88560,#18519);
#12486=LINE('',#88565,#18520);
#12487=LINE('',#88567,#18521);
#12488=LINE('',#88569,#18522);
#12489=LINE('',#88570,#18523);
#12490=LINE('',#88573,#18524);
#12491=LINE('',#88575,#18525);
#12492=LINE('',#88576,#18526);
#12493=LINE('',#88579,#18527);
#12494=LINE('',#88581,#18528);
#12495=LINE('',#88582,#18529);
#12496=LINE('',#88584,#18530);
#12497=LINE('',#88585,#18531);
#12498=LINE('',#88590,#18532);
#12499=LINE('',#88592,#18533);
#12500=LINE('',#88594,#18534);
#12501=LINE('',#88595,#18535);
#12502=LINE('',#88598,#18536);
#12503=LINE('',#88600,#18537);
#12504=LINE('',#88601,#18538);
#12505=LINE('',#88604,#18539);
#12506=LINE('',#88606,#18540);
#12507=LINE('',#88607,#18541);
#12508=LINE('',#88609,#18542);
#12509=LINE('',#88610,#18543);
#12510=LINE('',#88615,#18544);
#12511=LINE('',#88617,#18545);
#12512=LINE('',#88619,#18546);
#12513=LINE('',#88620,#18547);
#12514=LINE('',#88623,#18548);
#12515=LINE('',#88625,#18549);
#12516=LINE('',#88626,#18550);
#12517=LINE('',#88629,#18551);
#12518=LINE('',#88631,#18552);
#12519=LINE('',#88632,#18553);
#12520=LINE('',#88634,#18554);
#12521=LINE('',#88635,#18555);
#12522=LINE('',#88640,#18556);
#12523=LINE('',#88642,#18557);
#12524=LINE('',#88644,#18558);
#12525=LINE('',#88645,#18559);
#12526=LINE('',#88648,#18560);
#12527=LINE('',#88650,#18561);
#12528=LINE('',#88651,#18562);
#12529=LINE('',#88654,#18563);
#12530=LINE('',#88656,#18564);
#12531=LINE('',#88657,#18565);
#12532=LINE('',#88659,#18566);
#12533=LINE('',#88660,#18567);
#12534=LINE('',#88665,#18568);
#12535=LINE('',#88667,#18569);
#12536=LINE('',#88669,#18570);
#12537=LINE('',#88670,#18571);
#12538=LINE('',#88673,#18572);
#12539=LINE('',#88675,#18573);
#12540=LINE('',#88676,#18574);
#12541=LINE('',#88679,#18575);
#12542=LINE('',#88681,#18576);
#12543=LINE('',#88682,#18577);
#12544=LINE('',#88684,#18578);
#12545=LINE('',#88685,#18579);
#12546=LINE('',#88690,#18580);
#12547=LINE('',#88692,#18581);
#12548=LINE('',#88694,#18582);
#12549=LINE('',#88695,#18583);
#12550=LINE('',#88698,#18584);
#12551=LINE('',#88700,#18585);
#12552=LINE('',#88701,#18586);
#12553=LINE('',#88704,#18587);
#12554=LINE('',#88706,#18588);
#12555=LINE('',#88707,#18589);
#12556=LINE('',#88709,#18590);
#12557=LINE('',#88710,#18591);
#12558=LINE('',#88715,#18592);
#12559=LINE('',#88717,#18593);
#12560=LINE('',#88719,#18594);
#12561=LINE('',#88720,#18595);
#12562=LINE('',#88723,#18596);
#12563=LINE('',#88725,#18597);
#12564=LINE('',#88726,#18598);
#12565=LINE('',#88729,#18599);
#12566=LINE('',#88731,#18600);
#12567=LINE('',#88732,#18601);
#12568=LINE('',#88734,#18602);
#12569=LINE('',#88735,#18603);
#12570=LINE('',#88740,#18604);
#12571=LINE('',#88742,#18605);
#12572=LINE('',#88744,#18606);
#12573=LINE('',#88745,#18607);
#12574=LINE('',#88748,#18608);
#12575=LINE('',#88750,#18609);
#12576=LINE('',#88751,#18610);
#12577=LINE('',#88754,#18611);
#12578=LINE('',#88756,#18612);
#12579=LINE('',#88757,#18613);
#12580=LINE('',#88759,#18614);
#12581=LINE('',#88760,#18615);
#12582=LINE('',#88765,#18616);
#12583=LINE('',#88767,#18617);
#12584=LINE('',#88769,#18618);
#12585=LINE('',#88770,#18619);
#12586=LINE('',#88773,#18620);
#12587=LINE('',#88775,#18621);
#12588=LINE('',#88776,#18622);
#12589=LINE('',#88779,#18623);
#12590=LINE('',#88781,#18624);
#12591=LINE('',#88782,#18625);
#12592=LINE('',#88784,#18626);
#12593=LINE('',#88785,#18627);
#12594=LINE('',#88790,#18628);
#12595=LINE('',#88792,#18629);
#12596=LINE('',#88794,#18630);
#12597=LINE('',#88795,#18631);
#12598=LINE('',#88798,#18632);
#12599=LINE('',#88800,#18633);
#12600=LINE('',#88801,#18634);
#12601=LINE('',#88804,#18635);
#12602=LINE('',#88806,#18636);
#12603=LINE('',#88807,#18637);
#12604=LINE('',#88809,#18638);
#12605=LINE('',#88810,#18639);
#12606=LINE('',#88815,#18640);
#12607=LINE('',#88817,#18641);
#12608=LINE('',#88819,#18642);
#12609=LINE('',#88820,#18643);
#12610=LINE('',#88823,#18644);
#12611=LINE('',#88825,#18645);
#12612=LINE('',#88826,#18646);
#12613=LINE('',#88829,#18647);
#12614=LINE('',#88831,#18648);
#12615=LINE('',#88832,#18649);
#12616=LINE('',#88834,#18650);
#12617=LINE('',#88835,#18651);
#12618=LINE('',#88840,#18652);
#12619=LINE('',#88842,#18653);
#12620=LINE('',#88844,#18654);
#12621=LINE('',#88845,#18655);
#12622=LINE('',#88848,#18656);
#12623=LINE('',#88850,#18657);
#12624=LINE('',#88851,#18658);
#12625=LINE('',#88854,#18659);
#12626=LINE('',#88856,#18660);
#12627=LINE('',#88857,#18661);
#12628=LINE('',#88859,#18662);
#12629=LINE('',#88860,#18663);
#12630=LINE('',#88865,#18664);
#12631=LINE('',#88867,#18665);
#12632=LINE('',#88869,#18666);
#12633=LINE('',#88870,#18667);
#12634=LINE('',#88873,#18668);
#12635=LINE('',#88875,#18669);
#12636=LINE('',#88876,#18670);
#12637=LINE('',#88879,#18671);
#12638=LINE('',#88881,#18672);
#12639=LINE('',#88882,#18673);
#12640=LINE('',#88884,#18674);
#12641=LINE('',#88885,#18675);
#12642=LINE('',#88890,#18676);
#12643=LINE('',#88892,#18677);
#12644=LINE('',#88894,#18678);
#12645=LINE('',#88895,#18679);
#12646=LINE('',#88898,#18680);
#12647=LINE('',#88900,#18681);
#12648=LINE('',#88901,#18682);
#12649=LINE('',#88904,#18683);
#12650=LINE('',#88906,#18684);
#12651=LINE('',#88907,#18685);
#12652=LINE('',#88909,#18686);
#12653=LINE('',#88910,#18687);
#12654=LINE('',#88915,#18688);
#12655=LINE('',#88917,#18689);
#12656=LINE('',#88919,#18690);
#12657=LINE('',#88920,#18691);
#12658=LINE('',#88923,#18692);
#12659=LINE('',#88925,#18693);
#12660=LINE('',#88926,#18694);
#12661=LINE('',#88929,#18695);
#12662=LINE('',#88931,#18696);
#12663=LINE('',#88932,#18697);
#12664=LINE('',#88934,#18698);
#12665=LINE('',#88935,#18699);
#12666=LINE('',#88940,#18700);
#12667=LINE('',#88942,#18701);
#12668=LINE('',#88944,#18702);
#12669=LINE('',#88945,#18703);
#12670=LINE('',#88948,#18704);
#12671=LINE('',#88950,#18705);
#12672=LINE('',#88951,#18706);
#12673=LINE('',#88954,#18707);
#12674=LINE('',#88956,#18708);
#12675=LINE('',#88957,#18709);
#12676=LINE('',#88959,#18710);
#12677=LINE('',#88960,#18711);
#12678=LINE('',#88965,#18712);
#12679=LINE('',#88967,#18713);
#12680=LINE('',#88969,#18714);
#12681=LINE('',#88970,#18715);
#12682=LINE('',#88973,#18716);
#12683=LINE('',#88975,#18717);
#12684=LINE('',#88976,#18718);
#12685=LINE('',#88979,#18719);
#12686=LINE('',#88981,#18720);
#12687=LINE('',#88982,#18721);
#12688=LINE('',#88984,#18722);
#12689=LINE('',#88985,#18723);
#12690=LINE('',#88990,#18724);
#12691=LINE('',#88992,#18725);
#12692=LINE('',#88994,#18726);
#12693=LINE('',#88995,#18727);
#12694=LINE('',#88998,#18728);
#12695=LINE('',#89000,#18729);
#12696=LINE('',#89001,#18730);
#12697=LINE('',#89004,#18731);
#12698=LINE('',#89006,#18732);
#12699=LINE('',#89007,#18733);
#12700=LINE('',#89009,#18734);
#12701=LINE('',#89010,#18735);
#12702=LINE('',#89015,#18736);
#12703=LINE('',#89017,#18737);
#12704=LINE('',#89019,#18738);
#12705=LINE('',#89020,#18739);
#12706=LINE('',#89023,#18740);
#12707=LINE('',#89025,#18741);
#12708=LINE('',#89026,#18742);
#12709=LINE('',#89029,#18743);
#12710=LINE('',#89031,#18744);
#12711=LINE('',#89032,#18745);
#12712=LINE('',#89034,#18746);
#12713=LINE('',#89035,#18747);
#12714=LINE('',#89040,#18748);
#12715=LINE('',#89042,#18749);
#12716=LINE('',#89044,#18750);
#12717=LINE('',#89045,#18751);
#12718=LINE('',#89048,#18752);
#12719=LINE('',#89050,#18753);
#12720=LINE('',#89051,#18754);
#12721=LINE('',#89054,#18755);
#12722=LINE('',#89056,#18756);
#12723=LINE('',#89057,#18757);
#12724=LINE('',#89059,#18758);
#12725=LINE('',#89060,#18759);
#12726=LINE('',#89065,#18760);
#12727=LINE('',#89067,#18761);
#12728=LINE('',#89069,#18762);
#12729=LINE('',#89070,#18763);
#12730=LINE('',#89073,#18764);
#12731=LINE('',#89075,#18765);
#12732=LINE('',#89076,#18766);
#12733=LINE('',#89079,#18767);
#12734=LINE('',#89081,#18768);
#12735=LINE('',#89082,#18769);
#12736=LINE('',#89084,#18770);
#12737=LINE('',#89085,#18771);
#12738=LINE('',#89090,#18772);
#12739=LINE('',#89092,#18773);
#12740=LINE('',#89094,#18774);
#12741=LINE('',#89095,#18775);
#12742=LINE('',#89098,#18776);
#12743=LINE('',#89100,#18777);
#12744=LINE('',#89101,#18778);
#12745=LINE('',#89104,#18779);
#12746=LINE('',#89106,#18780);
#12747=LINE('',#89107,#18781);
#12748=LINE('',#89109,#18782);
#12749=LINE('',#89110,#18783);
#12750=LINE('',#89115,#18784);
#12751=LINE('',#89117,#18785);
#12752=LINE('',#89119,#18786);
#12753=LINE('',#89120,#18787);
#12754=LINE('',#89123,#18788);
#12755=LINE('',#89125,#18789);
#12756=LINE('',#89126,#18790);
#12757=LINE('',#89129,#18791);
#12758=LINE('',#89131,#18792);
#12759=LINE('',#89132,#18793);
#12760=LINE('',#89134,#18794);
#12761=LINE('',#89135,#18795);
#12762=LINE('',#89140,#18796);
#12763=LINE('',#89142,#18797);
#12764=LINE('',#89144,#18798);
#12765=LINE('',#89145,#18799);
#12766=LINE('',#89148,#18800);
#12767=LINE('',#89150,#18801);
#12768=LINE('',#89151,#18802);
#12769=LINE('',#89154,#18803);
#12770=LINE('',#89156,#18804);
#12771=LINE('',#89157,#18805);
#12772=LINE('',#89159,#18806);
#12773=LINE('',#89160,#18807);
#12774=LINE('',#89165,#18808);
#12775=LINE('',#89167,#18809);
#12776=LINE('',#89169,#18810);
#12777=LINE('',#89170,#18811);
#12778=LINE('',#89173,#18812);
#12779=LINE('',#89175,#18813);
#12780=LINE('',#89176,#18814);
#12781=LINE('',#89179,#18815);
#12782=LINE('',#89181,#18816);
#12783=LINE('',#89182,#18817);
#12784=LINE('',#89184,#18818);
#12785=LINE('',#89185,#18819);
#12786=LINE('',#89190,#18820);
#12787=LINE('',#89192,#18821);
#12788=LINE('',#89194,#18822);
#12789=LINE('',#89195,#18823);
#12790=LINE('',#89198,#18824);
#12791=LINE('',#89200,#18825);
#12792=LINE('',#89201,#18826);
#12793=LINE('',#89204,#18827);
#12794=LINE('',#89206,#18828);
#12795=LINE('',#89207,#18829);
#12796=LINE('',#89209,#18830);
#12797=LINE('',#89210,#18831);
#12798=LINE('',#89215,#18832);
#12799=LINE('',#89217,#18833);
#12800=LINE('',#89219,#18834);
#12801=LINE('',#89220,#18835);
#12802=LINE('',#89223,#18836);
#12803=LINE('',#89225,#18837);
#12804=LINE('',#89226,#18838);
#12805=LINE('',#89229,#18839);
#12806=LINE('',#89231,#18840);
#12807=LINE('',#89232,#18841);
#12808=LINE('',#89234,#18842);
#12809=LINE('',#89235,#18843);
#12810=LINE('',#89240,#18844);
#12811=LINE('',#89242,#18845);
#12812=LINE('',#89244,#18846);
#12813=LINE('',#89245,#18847);
#12814=LINE('',#89248,#18848);
#12815=LINE('',#89250,#18849);
#12816=LINE('',#89251,#18850);
#12817=LINE('',#89254,#18851);
#12818=LINE('',#89256,#18852);
#12819=LINE('',#89257,#18853);
#12820=LINE('',#89259,#18854);
#12821=LINE('',#89260,#18855);
#12822=LINE('',#89265,#18856);
#12823=LINE('',#89267,#18857);
#12824=LINE('',#89269,#18858);
#12825=LINE('',#89270,#18859);
#12826=LINE('',#89273,#18860);
#12827=LINE('',#89275,#18861);
#12828=LINE('',#89276,#18862);
#12829=LINE('',#89279,#18863);
#12830=LINE('',#89281,#18864);
#12831=LINE('',#89282,#18865);
#12832=LINE('',#89284,#18866);
#12833=LINE('',#89285,#18867);
#12834=LINE('',#89290,#18868);
#12835=LINE('',#89292,#18869);
#12836=LINE('',#89294,#18870);
#12837=LINE('',#89295,#18871);
#12838=LINE('',#89298,#18872);
#12839=LINE('',#89300,#18873);
#12840=LINE('',#89301,#18874);
#12841=LINE('',#89304,#18875);
#12842=LINE('',#89306,#18876);
#12843=LINE('',#89307,#18877);
#12844=LINE('',#89309,#18878);
#12845=LINE('',#89310,#18879);
#12846=LINE('',#89315,#18880);
#12847=LINE('',#89317,#18881);
#12848=LINE('',#89319,#18882);
#12849=LINE('',#89320,#18883);
#12850=LINE('',#89323,#18884);
#12851=LINE('',#89325,#18885);
#12852=LINE('',#89326,#18886);
#12853=LINE('',#89329,#18887);
#12854=LINE('',#89331,#18888);
#12855=LINE('',#89332,#18889);
#12856=LINE('',#89334,#18890);
#12857=LINE('',#89335,#18891);
#12858=LINE('',#89340,#18892);
#12859=LINE('',#89342,#18893);
#12860=LINE('',#89344,#18894);
#12861=LINE('',#89345,#18895);
#12862=LINE('',#89348,#18896);
#12863=LINE('',#89350,#18897);
#12864=LINE('',#89351,#18898);
#12865=LINE('',#89354,#18899);
#12866=LINE('',#89356,#18900);
#12867=LINE('',#89357,#18901);
#12868=LINE('',#89359,#18902);
#12869=LINE('',#89360,#18903);
#12870=LINE('',#89365,#18904);
#12871=LINE('',#89367,#18905);
#12872=LINE('',#89369,#18906);
#12873=LINE('',#89370,#18907);
#12874=LINE('',#89373,#18908);
#12875=LINE('',#89375,#18909);
#12876=LINE('',#89376,#18910);
#12877=LINE('',#89379,#18911);
#12878=LINE('',#89381,#18912);
#12879=LINE('',#89382,#18913);
#12880=LINE('',#89384,#18914);
#12881=LINE('',#89385,#18915);
#12882=LINE('',#89390,#18916);
#12883=LINE('',#89392,#18917);
#12884=LINE('',#89394,#18918);
#12885=LINE('',#89395,#18919);
#12886=LINE('',#89398,#18920);
#12887=LINE('',#89400,#18921);
#12888=LINE('',#89401,#18922);
#12889=LINE('',#89404,#18923);
#12890=LINE('',#89406,#18924);
#12891=LINE('',#89407,#18925);
#12892=LINE('',#89409,#18926);
#12893=LINE('',#89410,#18927);
#12894=LINE('',#89415,#18928);
#12895=LINE('',#89417,#18929);
#12896=LINE('',#89419,#18930);
#12897=LINE('',#89420,#18931);
#12898=LINE('',#89423,#18932);
#12899=LINE('',#89425,#18933);
#12900=LINE('',#89426,#18934);
#12901=LINE('',#89429,#18935);
#12902=LINE('',#89431,#18936);
#12903=LINE('',#89432,#18937);
#12904=LINE('',#89434,#18938);
#12905=LINE('',#89435,#18939);
#12906=LINE('',#89440,#18940);
#12907=LINE('',#89442,#18941);
#12908=LINE('',#89444,#18942);
#12909=LINE('',#89445,#18943);
#12910=LINE('',#89448,#18944);
#12911=LINE('',#89450,#18945);
#12912=LINE('',#89451,#18946);
#12913=LINE('',#89454,#18947);
#12914=LINE('',#89456,#18948);
#12915=LINE('',#89457,#18949);
#12916=LINE('',#89459,#18950);
#12917=LINE('',#89460,#18951);
#12918=LINE('',#89465,#18952);
#12919=LINE('',#89467,#18953);
#12920=LINE('',#89469,#18954);
#12921=LINE('',#89470,#18955);
#12922=LINE('',#89473,#18956);
#12923=LINE('',#89475,#18957);
#12924=LINE('',#89476,#18958);
#12925=LINE('',#89479,#18959);
#12926=LINE('',#89481,#18960);
#12927=LINE('',#89482,#18961);
#12928=LINE('',#89484,#18962);
#12929=LINE('',#89485,#18963);
#12930=LINE('',#89490,#18964);
#12931=LINE('',#89492,#18965);
#12932=LINE('',#89494,#18966);
#12933=LINE('',#89495,#18967);
#12934=LINE('',#89498,#18968);
#12935=LINE('',#89500,#18969);
#12936=LINE('',#89501,#18970);
#12937=LINE('',#89504,#18971);
#12938=LINE('',#89506,#18972);
#12939=LINE('',#89507,#18973);
#12940=LINE('',#89509,#18974);
#12941=LINE('',#89510,#18975);
#12942=LINE('',#89515,#18976);
#12943=LINE('',#89517,#18977);
#12944=LINE('',#89519,#18978);
#12945=LINE('',#89520,#18979);
#12946=LINE('',#89523,#18980);
#12947=LINE('',#89525,#18981);
#12948=LINE('',#89526,#18982);
#12949=LINE('',#89529,#18983);
#12950=LINE('',#89531,#18984);
#12951=LINE('',#89532,#18985);
#12952=LINE('',#89534,#18986);
#12953=LINE('',#89535,#18987);
#12954=LINE('',#89540,#18988);
#12955=LINE('',#89542,#18989);
#12956=LINE('',#89544,#18990);
#12957=LINE('',#89545,#18991);
#12958=LINE('',#89548,#18992);
#12959=LINE('',#89550,#18993);
#12960=LINE('',#89551,#18994);
#12961=LINE('',#89554,#18995);
#12962=LINE('',#89556,#18996);
#12963=LINE('',#89557,#18997);
#12964=LINE('',#89559,#18998);
#12965=LINE('',#89560,#18999);
#12966=LINE('',#89565,#19000);
#12967=LINE('',#89567,#19001);
#12968=LINE('',#89569,#19002);
#12969=LINE('',#89570,#19003);
#12970=LINE('',#89573,#19004);
#12971=LINE('',#89575,#19005);
#12972=LINE('',#89576,#19006);
#12973=LINE('',#89579,#19007);
#12974=LINE('',#89581,#19008);
#12975=LINE('',#89582,#19009);
#12976=LINE('',#89584,#19010);
#12977=LINE('',#89585,#19011);
#12978=LINE('',#89590,#19012);
#12979=LINE('',#89592,#19013);
#12980=LINE('',#89594,#19014);
#12981=LINE('',#89595,#19015);
#12982=LINE('',#89598,#19016);
#12983=LINE('',#89600,#19017);
#12984=LINE('',#89601,#19018);
#12985=LINE('',#89604,#19019);
#12986=LINE('',#89606,#19020);
#12987=LINE('',#89607,#19021);
#12988=LINE('',#89609,#19022);
#12989=LINE('',#89610,#19023);
#12990=LINE('',#89615,#19024);
#12991=LINE('',#89617,#19025);
#12992=LINE('',#89619,#19026);
#12993=LINE('',#89620,#19027);
#12994=LINE('',#89623,#19028);
#12995=LINE('',#89625,#19029);
#12996=LINE('',#89626,#19030);
#12997=LINE('',#89629,#19031);
#12998=LINE('',#89631,#19032);
#12999=LINE('',#89632,#19033);
#13000=LINE('',#89634,#19034);
#13001=LINE('',#89635,#19035);
#13002=LINE('',#89640,#19036);
#13003=LINE('',#89642,#19037);
#13004=LINE('',#89644,#19038);
#13005=LINE('',#89645,#19039);
#13006=LINE('',#89648,#19040);
#13007=LINE('',#89650,#19041);
#13008=LINE('',#89651,#19042);
#13009=LINE('',#89654,#19043);
#13010=LINE('',#89656,#19044);
#13011=LINE('',#89657,#19045);
#13012=LINE('',#89659,#19046);
#13013=LINE('',#89660,#19047);
#13014=LINE('',#89665,#19048);
#13015=LINE('',#89667,#19049);
#13016=LINE('',#89669,#19050);
#13017=LINE('',#89670,#19051);
#13018=LINE('',#89673,#19052);
#13019=LINE('',#89675,#19053);
#13020=LINE('',#89676,#19054);
#13021=LINE('',#89679,#19055);
#13022=LINE('',#89681,#19056);
#13023=LINE('',#89682,#19057);
#13024=LINE('',#89684,#19058);
#13025=LINE('',#89685,#19059);
#13026=LINE('',#89690,#19060);
#13027=LINE('',#89692,#19061);
#13028=LINE('',#89694,#19062);
#13029=LINE('',#89695,#19063);
#13030=LINE('',#89698,#19064);
#13031=LINE('',#89700,#19065);
#13032=LINE('',#89701,#19066);
#13033=LINE('',#89704,#19067);
#13034=LINE('',#89706,#19068);
#13035=LINE('',#89707,#19069);
#13036=LINE('',#89709,#19070);
#13037=LINE('',#89710,#19071);
#13038=LINE('',#89715,#19072);
#13039=LINE('',#89717,#19073);
#13040=LINE('',#89719,#19074);
#13041=LINE('',#89720,#19075);
#13042=LINE('',#89723,#19076);
#13043=LINE('',#89725,#19077);
#13044=LINE('',#89726,#19078);
#13045=LINE('',#89729,#19079);
#13046=LINE('',#89731,#19080);
#13047=LINE('',#89732,#19081);
#13048=LINE('',#89734,#19082);
#13049=LINE('',#89735,#19083);
#13050=LINE('',#89740,#19084);
#13051=LINE('',#89742,#19085);
#13052=LINE('',#89744,#19086);
#13053=LINE('',#89745,#19087);
#13054=LINE('',#89748,#19088);
#13055=LINE('',#89750,#19089);
#13056=LINE('',#89751,#19090);
#13057=LINE('',#89754,#19091);
#13058=LINE('',#89756,#19092);
#13059=LINE('',#89757,#19093);
#13060=LINE('',#89759,#19094);
#13061=LINE('',#89760,#19095);
#13062=LINE('',#89765,#19096);
#13063=LINE('',#89767,#19097);
#13064=LINE('',#89769,#19098);
#13065=LINE('',#89770,#19099);
#13066=LINE('',#89773,#19100);
#13067=LINE('',#89775,#19101);
#13068=LINE('',#89776,#19102);
#13069=LINE('',#89779,#19103);
#13070=LINE('',#89781,#19104);
#13071=LINE('',#89782,#19105);
#13072=LINE('',#89784,#19106);
#13073=LINE('',#89785,#19107);
#13074=LINE('',#89790,#19108);
#13075=LINE('',#89792,#19109);
#13076=LINE('',#89794,#19110);
#13077=LINE('',#89795,#19111);
#13078=LINE('',#89798,#19112);
#13079=LINE('',#89800,#19113);
#13080=LINE('',#89801,#19114);
#13081=LINE('',#89804,#19115);
#13082=LINE('',#89806,#19116);
#13083=LINE('',#89807,#19117);
#13084=LINE('',#89809,#19118);
#13085=LINE('',#89810,#19119);
#13086=LINE('',#89815,#19120);
#13087=LINE('',#89817,#19121);
#13088=LINE('',#89819,#19122);
#13089=LINE('',#89820,#19123);
#13090=LINE('',#89823,#19124);
#13091=LINE('',#89825,#19125);
#13092=LINE('',#89826,#19126);
#13093=LINE('',#89829,#19127);
#13094=LINE('',#89831,#19128);
#13095=LINE('',#89832,#19129);
#13096=LINE('',#89834,#19130);
#13097=LINE('',#89835,#19131);
#13098=LINE('',#89840,#19132);
#13099=LINE('',#89842,#19133);
#13100=LINE('',#89844,#19134);
#13101=LINE('',#89845,#19135);
#13102=LINE('',#89848,#19136);
#13103=LINE('',#89850,#19137);
#13104=LINE('',#89851,#19138);
#13105=LINE('',#89854,#19139);
#13106=LINE('',#89856,#19140);
#13107=LINE('',#89857,#19141);
#13108=LINE('',#89859,#19142);
#13109=LINE('',#89860,#19143);
#13110=LINE('',#89865,#19144);
#13111=LINE('',#89867,#19145);
#13112=LINE('',#89869,#19146);
#13113=LINE('',#89870,#19147);
#13114=LINE('',#89873,#19148);
#13115=LINE('',#89875,#19149);
#13116=LINE('',#89876,#19150);
#13117=LINE('',#89879,#19151);
#13118=LINE('',#89881,#19152);
#13119=LINE('',#89882,#19153);
#13120=LINE('',#89884,#19154);
#13121=LINE('',#89885,#19155);
#13122=LINE('',#89890,#19156);
#13123=LINE('',#89892,#19157);
#13124=LINE('',#89894,#19158);
#13125=LINE('',#89895,#19159);
#13126=LINE('',#89898,#19160);
#13127=LINE('',#89900,#19161);
#13128=LINE('',#89901,#19162);
#13129=LINE('',#89904,#19163);
#13130=LINE('',#89906,#19164);
#13131=LINE('',#89907,#19165);
#13132=LINE('',#89909,#19166);
#13133=LINE('',#89910,#19167);
#13134=LINE('',#89915,#19168);
#13135=LINE('',#89917,#19169);
#13136=LINE('',#89919,#19170);
#13137=LINE('',#89920,#19171);
#13138=LINE('',#89923,#19172);
#13139=LINE('',#89925,#19173);
#13140=LINE('',#89926,#19174);
#13141=LINE('',#89929,#19175);
#13142=LINE('',#89931,#19176);
#13143=LINE('',#89932,#19177);
#13144=LINE('',#89934,#19178);
#13145=LINE('',#89935,#19179);
#13146=LINE('',#89940,#19180);
#13147=LINE('',#89942,#19181);
#13148=LINE('',#89944,#19182);
#13149=LINE('',#89945,#19183);
#13150=LINE('',#89948,#19184);
#13151=LINE('',#89950,#19185);
#13152=LINE('',#89951,#19186);
#13153=LINE('',#89954,#19187);
#13154=LINE('',#89956,#19188);
#13155=LINE('',#89957,#19189);
#13156=LINE('',#89959,#19190);
#13157=LINE('',#89960,#19191);
#13158=LINE('',#89965,#19192);
#13159=LINE('',#89967,#19193);
#13160=LINE('',#89969,#19194);
#13161=LINE('',#89970,#19195);
#13162=LINE('',#89973,#19196);
#13163=LINE('',#89975,#19197);
#13164=LINE('',#89976,#19198);
#13165=LINE('',#89979,#19199);
#13166=LINE('',#89981,#19200);
#13167=LINE('',#89982,#19201);
#13168=LINE('',#89984,#19202);
#13169=LINE('',#89985,#19203);
#13170=LINE('',#89990,#19204);
#13171=LINE('',#89992,#19205);
#13172=LINE('',#89994,#19206);
#13173=LINE('',#89995,#19207);
#13174=LINE('',#89998,#19208);
#13175=LINE('',#90000,#19209);
#13176=LINE('',#90001,#19210);
#13177=LINE('',#90004,#19211);
#13178=LINE('',#90006,#19212);
#13179=LINE('',#90007,#19213);
#13180=LINE('',#90009,#19214);
#13181=LINE('',#90010,#19215);
#13182=LINE('',#90015,#19216);
#13183=LINE('',#90017,#19217);
#13184=LINE('',#90019,#19218);
#13185=LINE('',#90020,#19219);
#13186=LINE('',#90023,#19220);
#13187=LINE('',#90025,#19221);
#13188=LINE('',#90026,#19222);
#13189=LINE('',#90029,#19223);
#13190=LINE('',#90031,#19224);
#13191=LINE('',#90032,#19225);
#13192=LINE('',#90034,#19226);
#13193=LINE('',#90035,#19227);
#13194=LINE('',#90040,#19228);
#13195=LINE('',#90042,#19229);
#13196=LINE('',#90044,#19230);
#13197=LINE('',#90045,#19231);
#13198=LINE('',#90048,#19232);
#13199=LINE('',#90050,#19233);
#13200=LINE('',#90051,#19234);
#13201=LINE('',#90054,#19235);
#13202=LINE('',#90056,#19236);
#13203=LINE('',#90057,#19237);
#13204=LINE('',#90059,#19238);
#13205=LINE('',#90060,#19239);
#13206=LINE('',#90065,#19240);
#13207=LINE('',#90067,#19241);
#13208=LINE('',#90069,#19242);
#13209=LINE('',#90070,#19243);
#13210=LINE('',#90073,#19244);
#13211=LINE('',#90075,#19245);
#13212=LINE('',#90076,#19246);
#13213=LINE('',#90079,#19247);
#13214=LINE('',#90081,#19248);
#13215=LINE('',#90082,#19249);
#13216=LINE('',#90084,#19250);
#13217=LINE('',#90085,#19251);
#13218=LINE('',#90090,#19252);
#13219=LINE('',#90092,#19253);
#13220=LINE('',#90094,#19254);
#13221=LINE('',#90095,#19255);
#13222=LINE('',#90098,#19256);
#13223=LINE('',#90100,#19257);
#13224=LINE('',#90101,#19258);
#13225=LINE('',#90104,#19259);
#13226=LINE('',#90106,#19260);
#13227=LINE('',#90107,#19261);
#13228=LINE('',#90109,#19262);
#13229=LINE('',#90110,#19263);
#13230=LINE('',#90115,#19264);
#13231=LINE('',#90117,#19265);
#13232=LINE('',#90119,#19266);
#13233=LINE('',#90120,#19267);
#13234=LINE('',#90123,#19268);
#13235=LINE('',#90125,#19269);
#13236=LINE('',#90126,#19270);
#13237=LINE('',#90129,#19271);
#13238=LINE('',#90131,#19272);
#13239=LINE('',#90132,#19273);
#13240=LINE('',#90134,#19274);
#13241=LINE('',#90135,#19275);
#13242=LINE('',#90140,#19276);
#13243=LINE('',#90142,#19277);
#13244=LINE('',#90144,#19278);
#13245=LINE('',#90145,#19279);
#13246=LINE('',#90148,#19280);
#13247=LINE('',#90150,#19281);
#13248=LINE('',#90151,#19282);
#13249=LINE('',#90154,#19283);
#13250=LINE('',#90156,#19284);
#13251=LINE('',#90157,#19285);
#13252=LINE('',#90159,#19286);
#13253=LINE('',#90160,#19287);
#13254=LINE('',#90165,#19288);
#13255=LINE('',#90167,#19289);
#13256=LINE('',#90169,#19290);
#13257=LINE('',#90170,#19291);
#13258=LINE('',#90173,#19292);
#13259=LINE('',#90175,#19293);
#13260=LINE('',#90176,#19294);
#13261=LINE('',#90179,#19295);
#13262=LINE('',#90181,#19296);
#13263=LINE('',#90182,#19297);
#13264=LINE('',#90184,#19298);
#13265=LINE('',#90185,#19299);
#13266=LINE('',#90190,#19300);
#13267=LINE('',#90192,#19301);
#13268=LINE('',#90194,#19302);
#13269=LINE('',#90195,#19303);
#13270=LINE('',#90198,#19304);
#13271=LINE('',#90200,#19305);
#13272=LINE('',#90201,#19306);
#13273=LINE('',#90204,#19307);
#13274=LINE('',#90206,#19308);
#13275=LINE('',#90207,#19309);
#13276=LINE('',#90209,#19310);
#13277=LINE('',#90210,#19311);
#13278=LINE('',#90215,#19312);
#13279=LINE('',#90217,#19313);
#13280=LINE('',#90219,#19314);
#13281=LINE('',#90220,#19315);
#13282=LINE('',#90223,#19316);
#13283=LINE('',#90225,#19317);
#13284=LINE('',#90226,#19318);
#13285=LINE('',#90229,#19319);
#13286=LINE('',#90231,#19320);
#13287=LINE('',#90232,#19321);
#13288=LINE('',#90234,#19322);
#13289=LINE('',#90235,#19323);
#13290=LINE('',#90240,#19324);
#13291=LINE('',#90242,#19325);
#13292=LINE('',#90244,#19326);
#13293=LINE('',#90245,#19327);
#13294=LINE('',#90248,#19328);
#13295=LINE('',#90250,#19329);
#13296=LINE('',#90251,#19330);
#13297=LINE('',#90254,#19331);
#13298=LINE('',#90256,#19332);
#13299=LINE('',#90257,#19333);
#13300=LINE('',#90259,#19334);
#13301=LINE('',#90260,#19335);
#13302=LINE('',#90265,#19336);
#13303=LINE('',#90267,#19337);
#13304=LINE('',#90269,#19338);
#13305=LINE('',#90270,#19339);
#13306=LINE('',#90273,#19340);
#13307=LINE('',#90275,#19341);
#13308=LINE('',#90276,#19342);
#13309=LINE('',#90279,#19343);
#13310=LINE('',#90281,#19344);
#13311=LINE('',#90282,#19345);
#13312=LINE('',#90284,#19346);
#13313=LINE('',#90285,#19347);
#13314=LINE('',#90290,#19348);
#13315=LINE('',#90292,#19349);
#13316=LINE('',#90294,#19350);
#13317=LINE('',#90295,#19351);
#13318=LINE('',#90298,#19352);
#13319=LINE('',#90300,#19353);
#13320=LINE('',#90301,#19354);
#13321=LINE('',#90304,#19355);
#13322=LINE('',#90306,#19356);
#13323=LINE('',#90307,#19357);
#13324=LINE('',#90309,#19358);
#13325=LINE('',#90310,#19359);
#13326=LINE('',#90315,#19360);
#13327=LINE('',#90317,#19361);
#13328=LINE('',#90319,#19362);
#13329=LINE('',#90320,#19363);
#13330=LINE('',#90323,#19364);
#13331=LINE('',#90325,#19365);
#13332=LINE('',#90326,#19366);
#13333=LINE('',#90329,#19367);
#13334=LINE('',#90331,#19368);
#13335=LINE('',#90332,#19369);
#13336=LINE('',#90334,#19370);
#13337=LINE('',#90335,#19371);
#13338=LINE('',#90340,#19372);
#13339=LINE('',#90342,#19373);
#13340=LINE('',#90344,#19374);
#13341=LINE('',#90345,#19375);
#13342=LINE('',#90348,#19376);
#13343=LINE('',#90350,#19377);
#13344=LINE('',#90351,#19378);
#13345=LINE('',#90354,#19379);
#13346=LINE('',#90356,#19380);
#13347=LINE('',#90357,#19381);
#13348=LINE('',#90359,#19382);
#13349=LINE('',#90360,#19383);
#13350=LINE('',#90365,#19384);
#13351=LINE('',#90367,#19385);
#13352=LINE('',#90369,#19386);
#13353=LINE('',#90370,#19387);
#13354=LINE('',#90373,#19388);
#13355=LINE('',#90375,#19389);
#13356=LINE('',#90376,#19390);
#13357=LINE('',#90379,#19391);
#13358=LINE('',#90381,#19392);
#13359=LINE('',#90382,#19393);
#13360=LINE('',#90384,#19394);
#13361=LINE('',#90385,#19395);
#13362=LINE('',#90390,#19396);
#13363=LINE('',#90392,#19397);
#13364=LINE('',#90394,#19398);
#13365=LINE('',#90395,#19399);
#13366=LINE('',#90398,#19400);
#13367=LINE('',#90400,#19401);
#13368=LINE('',#90401,#19402);
#13369=LINE('',#90404,#19403);
#13370=LINE('',#90406,#19404);
#13371=LINE('',#90407,#19405);
#13372=LINE('',#90409,#19406);
#13373=LINE('',#90410,#19407);
#13374=LINE('',#90415,#19408);
#13375=LINE('',#90417,#19409);
#13376=LINE('',#90419,#19410);
#13377=LINE('',#90420,#19411);
#13378=LINE('',#90423,#19412);
#13379=LINE('',#90425,#19413);
#13380=LINE('',#90426,#19414);
#13381=LINE('',#90429,#19415);
#13382=LINE('',#90431,#19416);
#13383=LINE('',#90432,#19417);
#13384=LINE('',#90434,#19418);
#13385=LINE('',#90435,#19419);
#13386=LINE('',#90440,#19420);
#13387=LINE('',#90442,#19421);
#13388=LINE('',#90444,#19422);
#13389=LINE('',#90445,#19423);
#13390=LINE('',#90448,#19424);
#13391=LINE('',#90450,#19425);
#13392=LINE('',#90451,#19426);
#13393=LINE('',#90454,#19427);
#13394=LINE('',#90456,#19428);
#13395=LINE('',#90457,#19429);
#13396=LINE('',#90459,#19430);
#13397=LINE('',#90460,#19431);
#13398=LINE('',#90465,#19432);
#13399=LINE('',#90467,#19433);
#13400=LINE('',#90469,#19434);
#13401=LINE('',#90470,#19435);
#13402=LINE('',#90473,#19436);
#13403=LINE('',#90475,#19437);
#13404=LINE('',#90476,#19438);
#13405=LINE('',#90479,#19439);
#13406=LINE('',#90481,#19440);
#13407=LINE('',#90482,#19441);
#13408=LINE('',#90484,#19442);
#13409=LINE('',#90485,#19443);
#13410=LINE('',#90490,#19444);
#13411=LINE('',#90492,#19445);
#13412=LINE('',#90494,#19446);
#13413=LINE('',#90495,#19447);
#13414=LINE('',#90498,#19448);
#13415=LINE('',#90500,#19449);
#13416=LINE('',#90501,#19450);
#13417=LINE('',#90504,#19451);
#13418=LINE('',#90506,#19452);
#13419=LINE('',#90507,#19453);
#13420=LINE('',#90509,#19454);
#13421=LINE('',#90510,#19455);
#13422=LINE('',#90515,#19456);
#13423=LINE('',#90517,#19457);
#13424=LINE('',#90519,#19458);
#13425=LINE('',#90520,#19459);
#13426=LINE('',#90523,#19460);
#13427=LINE('',#90525,#19461);
#13428=LINE('',#90526,#19462);
#13429=LINE('',#90529,#19463);
#13430=LINE('',#90531,#19464);
#13431=LINE('',#90532,#19465);
#13432=LINE('',#90534,#19466);
#13433=LINE('',#90535,#19467);
#13434=LINE('',#90540,#19468);
#13435=LINE('',#90542,#19469);
#13436=LINE('',#90544,#19470);
#13437=LINE('',#90545,#19471);
#13438=LINE('',#90548,#19472);
#13439=LINE('',#90550,#19473);
#13440=LINE('',#90551,#19474);
#13441=LINE('',#90554,#19475);
#13442=LINE('',#90556,#19476);
#13443=LINE('',#90557,#19477);
#13444=LINE('',#90559,#19478);
#13445=LINE('',#90560,#19479);
#13446=LINE('',#90565,#19480);
#13447=LINE('',#90567,#19481);
#13448=LINE('',#90569,#19482);
#13449=LINE('',#90570,#19483);
#13450=LINE('',#90573,#19484);
#13451=LINE('',#90575,#19485);
#13452=LINE('',#90576,#19486);
#13453=LINE('',#90579,#19487);
#13454=LINE('',#90581,#19488);
#13455=LINE('',#90582,#19489);
#13456=LINE('',#90584,#19490);
#13457=LINE('',#90585,#19491);
#13458=LINE('',#90590,#19492);
#13459=LINE('',#90592,#19493);
#13460=LINE('',#90594,#19494);
#13461=LINE('',#90595,#19495);
#13462=LINE('',#90598,#19496);
#13463=LINE('',#90600,#19497);
#13464=LINE('',#90601,#19498);
#13465=LINE('',#90604,#19499);
#13466=LINE('',#90606,#19500);
#13467=LINE('',#90607,#19501);
#13468=LINE('',#90609,#19502);
#13469=LINE('',#90610,#19503);
#13470=LINE('',#90615,#19504);
#13471=LINE('',#90617,#19505);
#13472=LINE('',#90619,#19506);
#13473=LINE('',#90620,#19507);
#13474=LINE('',#90623,#19508);
#13475=LINE('',#90625,#19509);
#13476=LINE('',#90626,#19510);
#13477=LINE('',#90629,#19511);
#13478=LINE('',#90631,#19512);
#13479=LINE('',#90632,#19513);
#13480=LINE('',#90634,#19514);
#13481=LINE('',#90635,#19515);
#13482=LINE('',#90640,#19516);
#13483=LINE('',#90642,#19517);
#13484=LINE('',#90644,#19518);
#13485=LINE('',#90645,#19519);
#13486=LINE('',#90648,#19520);
#13487=LINE('',#90650,#19521);
#13488=LINE('',#90651,#19522);
#13489=LINE('',#90654,#19523);
#13490=LINE('',#90656,#19524);
#13491=LINE('',#90657,#19525);
#13492=LINE('',#90659,#19526);
#13493=LINE('',#90660,#19527);
#13494=LINE('',#90665,#19528);
#13495=LINE('',#90667,#19529);
#13496=LINE('',#90669,#19530);
#13497=LINE('',#90670,#19531);
#13498=LINE('',#90673,#19532);
#13499=LINE('',#90675,#19533);
#13500=LINE('',#90676,#19534);
#13501=LINE('',#90679,#19535);
#13502=LINE('',#90681,#19536);
#13503=LINE('',#90682,#19537);
#13504=LINE('',#90684,#19538);
#13505=LINE('',#90685,#19539);
#13506=LINE('',#90690,#19540);
#13507=LINE('',#90692,#19541);
#13508=LINE('',#90694,#19542);
#13509=LINE('',#90695,#19543);
#13510=LINE('',#90698,#19544);
#13511=LINE('',#90700,#19545);
#13512=LINE('',#90701,#19546);
#13513=LINE('',#90704,#19547);
#13514=LINE('',#90706,#19548);
#13515=LINE('',#90707,#19549);
#13516=LINE('',#90709,#19550);
#13517=LINE('',#90710,#19551);
#13518=LINE('',#90715,#19552);
#13519=LINE('',#90717,#19553);
#13520=LINE('',#90719,#19554);
#13521=LINE('',#90720,#19555);
#13522=LINE('',#90723,#19556);
#13523=LINE('',#90725,#19557);
#13524=LINE('',#90726,#19558);
#13525=LINE('',#90729,#19559);
#13526=LINE('',#90731,#19560);
#13527=LINE('',#90732,#19561);
#13528=LINE('',#90734,#19562);
#13529=LINE('',#90735,#19563);
#13530=LINE('',#90740,#19564);
#13531=LINE('',#90742,#19565);
#13532=LINE('',#90744,#19566);
#13533=LINE('',#90745,#19567);
#13534=LINE('',#90748,#19568);
#13535=LINE('',#90750,#19569);
#13536=LINE('',#90751,#19570);
#13537=LINE('',#90754,#19571);
#13538=LINE('',#90756,#19572);
#13539=LINE('',#90757,#19573);
#13540=LINE('',#90759,#19574);
#13541=LINE('',#90760,#19575);
#13542=LINE('',#90765,#19576);
#13543=LINE('',#90767,#19577);
#13544=LINE('',#90769,#19578);
#13545=LINE('',#90770,#19579);
#13546=LINE('',#90773,#19580);
#13547=LINE('',#90775,#19581);
#13548=LINE('',#90776,#19582);
#13549=LINE('',#90779,#19583);
#13550=LINE('',#90781,#19584);
#13551=LINE('',#90782,#19585);
#13552=LINE('',#90784,#19586);
#13553=LINE('',#90785,#19587);
#13554=LINE('',#90790,#19588);
#13555=LINE('',#90792,#19589);
#13556=LINE('',#90794,#19590);
#13557=LINE('',#90795,#19591);
#13558=LINE('',#90798,#19592);
#13559=LINE('',#90800,#19593);
#13560=LINE('',#90801,#19594);
#13561=LINE('',#90804,#19595);
#13562=LINE('',#90806,#19596);
#13563=LINE('',#90807,#19597);
#13564=LINE('',#90809,#19598);
#13565=LINE('',#90810,#19599);
#13566=LINE('',#90815,#19600);
#13567=LINE('',#90817,#19601);
#13568=LINE('',#90819,#19602);
#13569=LINE('',#90820,#19603);
#13570=LINE('',#90823,#19604);
#13571=LINE('',#90825,#19605);
#13572=LINE('',#90826,#19606);
#13573=LINE('',#90829,#19607);
#13574=LINE('',#90831,#19608);
#13575=LINE('',#90832,#19609);
#13576=LINE('',#90834,#19610);
#13577=LINE('',#90835,#19611);
#13578=LINE('',#90840,#19612);
#13579=LINE('',#90842,#19613);
#13580=LINE('',#90844,#19614);
#13581=LINE('',#90845,#19615);
#13582=LINE('',#90848,#19616);
#13583=LINE('',#90850,#19617);
#13584=LINE('',#90851,#19618);
#13585=LINE('',#90854,#19619);
#13586=LINE('',#90856,#19620);
#13587=LINE('',#90857,#19621);
#13588=LINE('',#90859,#19622);
#13589=LINE('',#90860,#19623);
#13590=LINE('',#90865,#19624);
#13591=LINE('',#90867,#19625);
#13592=LINE('',#90869,#19626);
#13593=LINE('',#90870,#19627);
#13594=LINE('',#90873,#19628);
#13595=LINE('',#90875,#19629);
#13596=LINE('',#90876,#19630);
#13597=LINE('',#90879,#19631);
#13598=LINE('',#90881,#19632);
#13599=LINE('',#90882,#19633);
#13600=LINE('',#90884,#19634);
#13601=LINE('',#90885,#19635);
#13602=LINE('',#90890,#19636);
#13603=LINE('',#90892,#19637);
#13604=LINE('',#90894,#19638);
#13605=LINE('',#90895,#19639);
#13606=LINE('',#90898,#19640);
#13607=LINE('',#90900,#19641);
#13608=LINE('',#90901,#19642);
#13609=LINE('',#90904,#19643);
#13610=LINE('',#90906,#19644);
#13611=LINE('',#90907,#19645);
#13612=LINE('',#90909,#19646);
#13613=LINE('',#90910,#19647);
#13614=LINE('',#90915,#19648);
#13615=LINE('',#90917,#19649);
#13616=LINE('',#90919,#19650);
#13617=LINE('',#90920,#19651);
#13618=LINE('',#90923,#19652);
#13619=LINE('',#90925,#19653);
#13620=LINE('',#90926,#19654);
#13621=LINE('',#90929,#19655);
#13622=LINE('',#90931,#19656);
#13623=LINE('',#90932,#19657);
#13624=LINE('',#90934,#19658);
#13625=LINE('',#90935,#19659);
#13626=LINE('',#90940,#19660);
#13627=LINE('',#90942,#19661);
#13628=LINE('',#90944,#19662);
#13629=LINE('',#90945,#19663);
#13630=LINE('',#90948,#19664);
#13631=LINE('',#90950,#19665);
#13632=LINE('',#90951,#19666);
#13633=LINE('',#90954,#19667);
#13634=LINE('',#90956,#19668);
#13635=LINE('',#90957,#19669);
#13636=LINE('',#90959,#19670);
#13637=LINE('',#90960,#19671);
#13638=LINE('',#90965,#19672);
#13639=LINE('',#90967,#19673);
#13640=LINE('',#90969,#19674);
#13641=LINE('',#90970,#19675);
#13642=LINE('',#90973,#19676);
#13643=LINE('',#90975,#19677);
#13644=LINE('',#90976,#19678);
#13645=LINE('',#90979,#19679);
#13646=LINE('',#90981,#19680);
#13647=LINE('',#90982,#19681);
#13648=LINE('',#90984,#19682);
#13649=LINE('',#90985,#19683);
#13650=LINE('',#90990,#19684);
#13651=LINE('',#90992,#19685);
#13652=LINE('',#90994,#19686);
#13653=LINE('',#90995,#19687);
#13654=LINE('',#90998,#19688);
#13655=LINE('',#91000,#19689);
#13656=LINE('',#91001,#19690);
#13657=LINE('',#91004,#19691);
#13658=LINE('',#91006,#19692);
#13659=LINE('',#91007,#19693);
#13660=LINE('',#91009,#19694);
#13661=LINE('',#91010,#19695);
#13662=LINE('',#91015,#19696);
#13663=LINE('',#91017,#19697);
#13664=LINE('',#91019,#19698);
#13665=LINE('',#91020,#19699);
#13666=LINE('',#91023,#19700);
#13667=LINE('',#91025,#19701);
#13668=LINE('',#91026,#19702);
#13669=LINE('',#91029,#19703);
#13670=LINE('',#91031,#19704);
#13671=LINE('',#91032,#19705);
#13672=LINE('',#91034,#19706);
#13673=LINE('',#91035,#19707);
#13674=LINE('',#91040,#19708);
#13675=LINE('',#91042,#19709);
#13676=LINE('',#91044,#19710);
#13677=LINE('',#91045,#19711);
#13678=LINE('',#91048,#19712);
#13679=LINE('',#91050,#19713);
#13680=LINE('',#91051,#19714);
#13681=LINE('',#91054,#19715);
#13682=LINE('',#91056,#19716);
#13683=LINE('',#91057,#19717);
#13684=LINE('',#91059,#19718);
#13685=LINE('',#91060,#19719);
#13686=LINE('',#91065,#19720);
#13687=LINE('',#91067,#19721);
#13688=LINE('',#91069,#19722);
#13689=LINE('',#91070,#19723);
#13690=LINE('',#91073,#19724);
#13691=LINE('',#91075,#19725);
#13692=LINE('',#91076,#19726);
#13693=LINE('',#91079,#19727);
#13694=LINE('',#91081,#19728);
#13695=LINE('',#91082,#19729);
#13696=LINE('',#91084,#19730);
#13697=LINE('',#91085,#19731);
#13698=LINE('',#91090,#19732);
#13699=LINE('',#91092,#19733);
#13700=LINE('',#91094,#19734);
#13701=LINE('',#91095,#19735);
#13702=LINE('',#91098,#19736);
#13703=LINE('',#91100,#19737);
#13704=LINE('',#91101,#19738);
#13705=LINE('',#91104,#19739);
#13706=LINE('',#91106,#19740);
#13707=LINE('',#91107,#19741);
#13708=LINE('',#91109,#19742);
#13709=LINE('',#91110,#19743);
#13710=LINE('',#91115,#19744);
#13711=LINE('',#91117,#19745);
#13712=LINE('',#91119,#19746);
#13713=LINE('',#91120,#19747);
#13714=LINE('',#91123,#19748);
#13715=LINE('',#91125,#19749);
#13716=LINE('',#91126,#19750);
#13717=LINE('',#91129,#19751);
#13718=LINE('',#91131,#19752);
#13719=LINE('',#91132,#19753);
#13720=LINE('',#91134,#19754);
#13721=LINE('',#91135,#19755);
#13722=LINE('',#91140,#19756);
#13723=LINE('',#91142,#19757);
#13724=LINE('',#91144,#19758);
#13725=LINE('',#91145,#19759);
#13726=LINE('',#91148,#19760);
#13727=LINE('',#91150,#19761);
#13728=LINE('',#91151,#19762);
#13729=LINE('',#91154,#19763);
#13730=LINE('',#91156,#19764);
#13731=LINE('',#91157,#19765);
#13732=LINE('',#91159,#19766);
#13733=LINE('',#91160,#19767);
#13734=LINE('',#91165,#19768);
#13735=LINE('',#91167,#19769);
#13736=LINE('',#91169,#19770);
#13737=LINE('',#91170,#19771);
#13738=LINE('',#91173,#19772);
#13739=LINE('',#91175,#19773);
#13740=LINE('',#91176,#19774);
#13741=LINE('',#91179,#19775);
#13742=LINE('',#91181,#19776);
#13743=LINE('',#91182,#19777);
#13744=LINE('',#91184,#19778);
#13745=LINE('',#91185,#19779);
#13746=LINE('',#91190,#19780);
#13747=LINE('',#91192,#19781);
#13748=LINE('',#91194,#19782);
#13749=LINE('',#91195,#19783);
#13750=LINE('',#91198,#19784);
#13751=LINE('',#91200,#19785);
#13752=LINE('',#91201,#19786);
#13753=LINE('',#91204,#19787);
#13754=LINE('',#91206,#19788);
#13755=LINE('',#91207,#19789);
#13756=LINE('',#91209,#19790);
#13757=LINE('',#91210,#19791);
#13758=LINE('',#91215,#19792);
#13759=LINE('',#91217,#19793);
#13760=LINE('',#91219,#19794);
#13761=LINE('',#91220,#19795);
#13762=LINE('',#91223,#19796);
#13763=LINE('',#91225,#19797);
#13764=LINE('',#91226,#19798);
#13765=LINE('',#91229,#19799);
#13766=LINE('',#91231,#19800);
#13767=LINE('',#91232,#19801);
#13768=LINE('',#91234,#19802);
#13769=LINE('',#91235,#19803);
#13770=LINE('',#91240,#19804);
#13771=LINE('',#91242,#19805);
#13772=LINE('',#91244,#19806);
#13773=LINE('',#91245,#19807);
#13774=LINE('',#91248,#19808);
#13775=LINE('',#91250,#19809);
#13776=LINE('',#91251,#19810);
#13777=LINE('',#91254,#19811);
#13778=LINE('',#91256,#19812);
#13779=LINE('',#91257,#19813);
#13780=LINE('',#91259,#19814);
#13781=LINE('',#91260,#19815);
#13782=LINE('',#91265,#19816);
#13783=LINE('',#91267,#19817);
#13784=LINE('',#91269,#19818);
#13785=LINE('',#91270,#19819);
#13786=LINE('',#91273,#19820);
#13787=LINE('',#91275,#19821);
#13788=LINE('',#91276,#19822);
#13789=LINE('',#91279,#19823);
#13790=LINE('',#91281,#19824);
#13791=LINE('',#91282,#19825);
#13792=LINE('',#91284,#19826);
#13793=LINE('',#91285,#19827);
#13794=LINE('',#91290,#19828);
#13795=LINE('',#91292,#19829);
#13796=LINE('',#91294,#19830);
#13797=LINE('',#91295,#19831);
#13798=LINE('',#91298,#19832);
#13799=LINE('',#91300,#19833);
#13800=LINE('',#91301,#19834);
#13801=LINE('',#91304,#19835);
#13802=LINE('',#91306,#19836);
#13803=LINE('',#91307,#19837);
#13804=LINE('',#91309,#19838);
#13805=LINE('',#91310,#19839);
#13806=LINE('',#91315,#19840);
#13807=LINE('',#91317,#19841);
#13808=LINE('',#91319,#19842);
#13809=LINE('',#91320,#19843);
#13810=LINE('',#91323,#19844);
#13811=LINE('',#91325,#19845);
#13812=LINE('',#91326,#19846);
#13813=LINE('',#91329,#19847);
#13814=LINE('',#91331,#19848);
#13815=LINE('',#91332,#19849);
#13816=LINE('',#91334,#19850);
#13817=LINE('',#91335,#19851);
#13818=LINE('',#91340,#19852);
#13819=LINE('',#91342,#19853);
#13820=LINE('',#91344,#19854);
#13821=LINE('',#91345,#19855);
#13822=LINE('',#91348,#19856);
#13823=LINE('',#91350,#19857);
#13824=LINE('',#91351,#19858);
#13825=LINE('',#91354,#19859);
#13826=LINE('',#91356,#19860);
#13827=LINE('',#91357,#19861);
#13828=LINE('',#91359,#19862);
#13829=LINE('',#91360,#19863);
#13830=LINE('',#91365,#19864);
#13831=LINE('',#91367,#19865);
#13832=LINE('',#91369,#19866);
#13833=LINE('',#91370,#19867);
#13834=LINE('',#91373,#19868);
#13835=LINE('',#91375,#19869);
#13836=LINE('',#91376,#19870);
#13837=LINE('',#91379,#19871);
#13838=LINE('',#91381,#19872);
#13839=LINE('',#91382,#19873);
#13840=LINE('',#91384,#19874);
#13841=LINE('',#91385,#19875);
#13842=LINE('',#91390,#19876);
#13843=LINE('',#91392,#19877);
#13844=LINE('',#91394,#19878);
#13845=LINE('',#91395,#19879);
#13846=LINE('',#91398,#19880);
#13847=LINE('',#91400,#19881);
#13848=LINE('',#91401,#19882);
#13849=LINE('',#91404,#19883);
#13850=LINE('',#91406,#19884);
#13851=LINE('',#91407,#19885);
#13852=LINE('',#91409,#19886);
#13853=LINE('',#91410,#19887);
#13854=LINE('',#91415,#19888);
#13855=LINE('',#91417,#19889);
#13856=LINE('',#91419,#19890);
#13857=LINE('',#91420,#19891);
#13858=LINE('',#91423,#19892);
#13859=LINE('',#91425,#19893);
#13860=LINE('',#91426,#19894);
#13861=LINE('',#91429,#19895);
#13862=LINE('',#91431,#19896);
#13863=LINE('',#91432,#19897);
#13864=LINE('',#91434,#19898);
#13865=LINE('',#91435,#19899);
#13866=LINE('',#91440,#19900);
#13867=LINE('',#91442,#19901);
#13868=LINE('',#91444,#19902);
#13869=LINE('',#91445,#19903);
#13870=LINE('',#91448,#19904);
#13871=LINE('',#91450,#19905);
#13872=LINE('',#91451,#19906);
#13873=LINE('',#91454,#19907);
#13874=LINE('',#91456,#19908);
#13875=LINE('',#91457,#19909);
#13876=LINE('',#91459,#19910);
#13877=LINE('',#91460,#19911);
#13878=LINE('',#91465,#19912);
#13879=LINE('',#91467,#19913);
#13880=LINE('',#91469,#19914);
#13881=LINE('',#91470,#19915);
#13882=LINE('',#91473,#19916);
#13883=LINE('',#91475,#19917);
#13884=LINE('',#91476,#19918);
#13885=LINE('',#91479,#19919);
#13886=LINE('',#91481,#19920);
#13887=LINE('',#91482,#19921);
#13888=LINE('',#91484,#19922);
#13889=LINE('',#91485,#19923);
#13890=LINE('',#91490,#19924);
#13891=LINE('',#91492,#19925);
#13892=LINE('',#91494,#19926);
#13893=LINE('',#91495,#19927);
#13894=LINE('',#91498,#19928);
#13895=LINE('',#91500,#19929);
#13896=LINE('',#91501,#19930);
#13897=LINE('',#91504,#19931);
#13898=LINE('',#91506,#19932);
#13899=LINE('',#91507,#19933);
#13900=LINE('',#91509,#19934);
#13901=LINE('',#91510,#19935);
#13902=LINE('',#91515,#19936);
#13903=LINE('',#91517,#19937);
#13904=LINE('',#91519,#19938);
#13905=LINE('',#91520,#19939);
#13906=LINE('',#91523,#19940);
#13907=LINE('',#91525,#19941);
#13908=LINE('',#91526,#19942);
#13909=LINE('',#91529,#19943);
#13910=LINE('',#91531,#19944);
#13911=LINE('',#91532,#19945);
#13912=LINE('',#91534,#19946);
#13913=LINE('',#91535,#19947);
#13914=LINE('',#91540,#19948);
#13915=LINE('',#91542,#19949);
#13916=LINE('',#91544,#19950);
#13917=LINE('',#91545,#19951);
#13918=LINE('',#91548,#19952);
#13919=LINE('',#91550,#19953);
#13920=LINE('',#91551,#19954);
#13921=LINE('',#91554,#19955);
#13922=LINE('',#91556,#19956);
#13923=LINE('',#91557,#19957);
#13924=LINE('',#91559,#19958);
#13925=LINE('',#91560,#19959);
#13926=LINE('',#91565,#19960);
#13927=LINE('',#91567,#19961);
#13928=LINE('',#91569,#19962);
#13929=LINE('',#91570,#19963);
#13930=LINE('',#91573,#19964);
#13931=LINE('',#91575,#19965);
#13932=LINE('',#91576,#19966);
#13933=LINE('',#91579,#19967);
#13934=LINE('',#91581,#19968);
#13935=LINE('',#91582,#19969);
#13936=LINE('',#91584,#19970);
#13937=LINE('',#91585,#19971);
#13938=LINE('',#91590,#19972);
#13939=LINE('',#91592,#19973);
#13940=LINE('',#91594,#19974);
#13941=LINE('',#91595,#19975);
#13942=LINE('',#91598,#19976);
#13943=LINE('',#91600,#19977);
#13944=LINE('',#91601,#19978);
#13945=LINE('',#91604,#19979);
#13946=LINE('',#91606,#19980);
#13947=LINE('',#91607,#19981);
#13948=LINE('',#91609,#19982);
#13949=LINE('',#91610,#19983);
#13950=LINE('',#91615,#19984);
#13951=LINE('',#91617,#19985);
#13952=LINE('',#91619,#19986);
#13953=LINE('',#91620,#19987);
#13954=LINE('',#91623,#19988);
#13955=LINE('',#91625,#19989);
#13956=LINE('',#91626,#19990);
#13957=LINE('',#91629,#19991);
#13958=LINE('',#91631,#19992);
#13959=LINE('',#91632,#19993);
#13960=LINE('',#91634,#19994);
#13961=LINE('',#91635,#19995);
#13962=LINE('',#91640,#19996);
#13963=LINE('',#91642,#19997);
#13964=LINE('',#91644,#19998);
#13965=LINE('',#91645,#19999);
#13966=LINE('',#91648,#20000);
#13967=LINE('',#91650,#20001);
#13968=LINE('',#91651,#20002);
#13969=LINE('',#91654,#20003);
#13970=LINE('',#91656,#20004);
#13971=LINE('',#91657,#20005);
#13972=LINE('',#91659,#20006);
#13973=LINE('',#91660,#20007);
#13974=LINE('',#91665,#20008);
#13975=LINE('',#91667,#20009);
#13976=LINE('',#91669,#20010);
#13977=LINE('',#91670,#20011);
#13978=LINE('',#91673,#20012);
#13979=LINE('',#91675,#20013);
#13980=LINE('',#91676,#20014);
#13981=LINE('',#91679,#20015);
#13982=LINE('',#91681,#20016);
#13983=LINE('',#91682,#20017);
#13984=LINE('',#91684,#20018);
#13985=LINE('',#91685,#20019);
#13986=LINE('',#91690,#20020);
#13987=LINE('',#91692,#20021);
#13988=LINE('',#91694,#20022);
#13989=LINE('',#91696,#20023);
#13990=LINE('',#91698,#20024);
#13991=LINE('',#91699,#20025);
#13992=LINE('',#91703,#20026);
#13993=LINE('',#91705,#20027);
#13994=LINE('',#91707,#20028);
#13995=LINE('',#91709,#20029);
#13996=LINE('',#91711,#20030);
#13997=LINE('',#91712,#20031);
#13998=LINE('',#91714,#20032);
#13999=LINE('',#91715,#20033);
#14000=LINE('',#91718,#20034);
#14001=LINE('',#91720,#20035);
#14002=LINE('',#91722,#20036);
#14003=LINE('',#91724,#20037);
#14004=LINE('',#91726,#20038);
#14005=LINE('',#91730,#20039);
#14006=LINE('',#91732,#20040);
#14007=LINE('',#91734,#20041);
#14008=LINE('',#91736,#20042);
#14009=LINE('',#91738,#20043);
#14010=LINE('',#91740,#20044);
#14011=LINE('',#91742,#20045);
#14012=LINE('',#91744,#20046);
#14013=LINE('',#91746,#20047);
#14014=LINE('',#91750,#20048);
#14015=LINE('',#91752,#20049);
#14016=LINE('',#91754,#20050);
#14017=LINE('',#91756,#20051);
#14018=LINE('',#91757,#20052);
#14019=LINE('',#91760,#20053);
#14020=LINE('',#91762,#20054);
#14021=LINE('',#91763,#20055);
#14022=LINE('',#91766,#20056);
#14023=LINE('',#91768,#20057);
#14024=LINE('',#91769,#20058);
#14025=LINE('',#91772,#20059);
#14026=LINE('',#91773,#20060);
#14027=LINE('',#91775,#20061);
#14028=LINE('',#91786,#20062);
#14029=LINE('',#91791,#20063);
#14030=LINE('',#91795,#20064);
#14031=LINE('',#91799,#20065);
#14032=LINE('',#91804,#20066);
#14033=LINE('',#91808,#20067);
#14034=LINE('',#91813,#20068);
#14035=LINE('',#91815,#20069);
#14036=LINE('',#91817,#20070);
#14037=LINE('',#91818,#20071);
#14038=LINE('',#91823,#20072);
#14039=LINE('',#91826,#20073);
#14040=LINE('',#91830,#20074);
#14041=LINE('',#91834,#20075);
#14042=LINE('',#91839,#20076);
#14043=LINE('',#91848,#20077);
#14044=LINE('',#91857,#20078);
#14045=LINE('',#91866,#20079);
#14046=LINE('',#91875,#20080);
#14047=LINE('',#91884,#20081);
#14048=LINE('',#91891,#20082);
#14049=LINE('',#91895,#20083);
#14050=LINE('',#91896,#20084);
#14051=LINE('',#91904,#20085);
#14052=LINE('',#91907,#20086);
#14053=LINE('',#91910,#20087);
#14054=LINE('',#91913,#20088);
#14055=LINE('',#91916,#20089);
#14056=LINE('',#91919,#20090);
#14057=LINE('',#91922,#20091);
#14058=LINE('',#91925,#20092);
#14059=LINE('',#91928,#20093);
#14060=LINE('',#91931,#20094);
#14061=LINE('',#91934,#20095);
#14062=LINE('',#91938,#20096);
#14063=LINE('',#91942,#20097);
#14064=LINE('',#91943,#20098);
#14065=LINE('',#91946,#20099);
#14066=LINE('',#91948,#20100);
#14067=LINE('',#91949,#20101);
#14068=LINE('',#91952,#20102);
#14069=LINE('',#91954,#20103);
#14070=LINE('',#91955,#20104);
#14071=LINE('',#91959,#20105);
#14072=LINE('',#91961,#20106);
#14073=LINE('',#91962,#20107);
#14074=LINE('',#91963,#20108);
#14075=LINE('',#91966,#20109);
#14076=LINE('',#91968,#20110);
#14077=LINE('',#91969,#20111);
#14078=LINE('',#91972,#20112);
#14079=LINE('',#91974,#20113);
#14080=LINE('',#91975,#20114);
#14081=LINE('',#91978,#20115);
#14082=LINE('',#91981,#20116);
#14083=LINE('',#91984,#20117);
#14084=LINE('',#91985,#20118);
#14085=LINE('',#91987,#20119);
#14086=LINE('',#91988,#20120);
#14087=LINE('',#91991,#20121);
#14088=LINE('',#91996,#20122);
#14089=LINE('',#92002,#20123);
#14090=LINE('',#92003,#20124);
#14091=LINE('',#92006,#20125);
#14092=LINE('',#92007,#20126);
#14093=LINE('',#92010,#20127);
#14094=LINE('',#92011,#20128);
#14095=LINE('',#92013,#20129);
#14096=LINE('',#92016,#20130);
#14097=LINE('',#92017,#20131);
#14098=LINE('',#92021,#20132);
#14099=LINE('',#92025,#20133);
#14100=LINE('',#92026,#20134);
#14101=LINE('',#92029,#20135);
#14102=LINE('',#92031,#20136);
#14103=LINE('',#92032,#20137);
#14104=LINE('',#92035,#20138);
#14105=LINE('',#92037,#20139);
#14106=LINE('',#92038,#20140);
#14107=LINE('',#92040,#20141);
#14108=LINE('',#92041,#20142);
#14109=LINE('',#92044,#20143);
#14110=LINE('',#92046,#20144);
#14111=LINE('',#92047,#20145);
#14112=LINE('',#92050,#20146);
#14113=LINE('',#92052,#20147);
#14114=LINE('',#92053,#20148);
#14115=LINE('',#92056,#20149);
#14116=LINE('',#92058,#20150);
#14117=LINE('',#92059,#20151);
#14118=LINE('',#92061,#20152);
#14119=LINE('',#92062,#20153);
#14120=LINE('',#92065,#20154);
#14121=LINE('',#92067,#20155);
#14122=LINE('',#92068,#20156);
#14123=LINE('',#92071,#20157);
#14124=LINE('',#92072,#20158);
#14125=LINE('',#92075,#20159);
#14126=LINE('',#92076,#20160);
#14127=LINE('',#92078,#20161);
#14128=LINE('',#92081,#20162);
#14129=LINE('',#92082,#20163);
#14130=LINE('',#92085,#20164);
#14131=LINE('',#92086,#20165);
#14132=LINE('',#92089,#20166);
#14133=LINE('',#92090,#20167);
#14134=LINE('',#92092,#20168);
#14135=LINE('',#92096,#20169);
#14136=LINE('',#92098,#20170);
#14137=LINE('',#92101,#20171);
#14138=LINE('',#92102,#20172);
#14139=LINE('',#92104,#20173);
#14140=LINE('',#92105,#20174);
#14141=LINE('',#92107,#20175);
#14142=LINE('',#92109,#20176);
#14143=LINE('',#92111,#20177);
#14144=LINE('',#92113,#20178);
#14145=LINE('',#92115,#20179);
#14146=LINE('',#92118,#20180);
#14147=LINE('',#92120,#20181);
#14148=LINE('',#92122,#20182);
#14149=LINE('',#92125,#20183);
#14150=LINE('',#92127,#20184);
#14151=LINE('',#92129,#20185);
#14152=LINE('',#92131,#20186);
#14153=LINE('',#92137,#20187);
#14154=LINE('',#92139,#20188);
#14155=LINE('',#92141,#20189);
#14156=LINE('',#92147,#20190);
#14157=LINE('',#92160,#20191);
#14158=LINE('',#92166,#20192);
#14159=LINE('',#92168,#20193);
#14160=LINE('',#92172,#20194);
#14161=LINE('',#92174,#20195);
#14162=LINE('',#92176,#20196);
#14163=LINE('',#92177,#20197);
#14164=LINE('',#92182,#20198);
#14165=LINE('',#92186,#20199);
#14166=LINE('',#92190,#20200);
#14167=LINE('',#92194,#20201);
#14168=LINE('',#92197,#20202);
#14169=LINE('',#92207,#20203);
#14170=LINE('',#92212,#20204);
#14171=LINE('',#92214,#20205);
#14172=LINE('',#92216,#20206);
#14173=LINE('',#92218,#20207);
#14174=LINE('',#92220,#20208);
#14175=LINE('',#92226,#20209);
#14176=LINE('',#92230,#20210);
#14177=LINE('',#92233,#20211);
#14178=LINE('',#92239,#20212);
#14179=LINE('',#92244,#20213);
#14180=LINE('',#92251,#20214);
#14181=LINE('',#92255,#20215);
#14182=LINE('',#92257,#20216);
#14183=LINE('',#92258,#20217);
#14184=LINE('',#92268,#20218);
#14185=LINE('',#92273,#20219);
#14186=LINE('',#92274,#20220);
#14187=LINE('',#92276,#20221);
#14188=LINE('',#92277,#20222);
#14189=LINE('',#92280,#20223);
#14190=LINE('',#92290,#20224);
#14191=LINE('',#92294,#20225);
#14192=LINE('',#92296,#20226);
#14193=LINE('',#92297,#20227);
#14194=LINE('',#92310,#20228);
#14195=LINE('',#92318,#20229);
#14196=LINE('',#92322,#20230);
#14197=LINE('',#92329,#20231);
#14198=LINE('',#92331,#20232);
#14199=LINE('',#92333,#20233);
#14200=LINE('',#92335,#20234);
#14201=LINE('',#92337,#20235);
#14202=LINE('',#92339,#20236);
#14203=LINE('',#92342,#20237);
#14204=LINE('',#92346,#20238);
#14205=LINE('',#92350,#20239);
#14206=LINE('',#92354,#20240);
#14207=LINE('',#92358,#20241);
#14208=LINE('',#92362,#20242);
#14209=LINE('',#92366,#20243);
#14210=LINE('',#92370,#20244);
#14211=LINE('',#92374,#20245);
#14212=LINE('',#92377,#20246);
#14213=LINE('',#92380,#20247);
#14214=LINE('',#92383,#20248);
#14215=LINE('',#92386,#20249);
#14216=LINE('',#92391,#20250);
#14217=LINE('',#92392,#20251);
#14218=LINE('',#92393,#20252);
#14219=LINE('',#92395,#20253);
#14220=LINE('',#92399,#20254);
#14221=LINE('',#92403,#20255);
#14222=LINE('',#92408,#20256);
#14223=LINE('',#92413,#20257);
#14224=LINE('',#92415,#20258);
#14225=LINE('',#92418,#20259);
#14226=LINE('',#92420,#20260);
#14227=LINE('',#92422,#20261);
#14228=LINE('',#92424,#20262);
#14229=LINE('',#92425,#20263);
#14230=LINE('',#92429,#20264);
#14231=LINE('',#92430,#20265);
#14232=LINE('',#92431,#20266);
#14233=LINE('',#92434,#20267);
#14234=LINE('',#92436,#20268);
#14235=LINE('',#92437,#20269);
#14236=LINE('',#92440,#20270);
#14237=LINE('',#92442,#20271);
#14238=LINE('',#92444,#20272);
#14239=LINE('',#92446,#20273);
#14240=LINE('',#92448,#20274);
#14241=LINE('',#92450,#20275);
#14242=LINE('',#92452,#20276);
#14243=LINE('',#92454,#20277);
#14244=LINE('',#92455,#20278);
#14245=LINE('',#92458,#20279);
#14246=LINE('',#92459,#20280);
#14247=LINE('',#92462,#20281);
#14248=LINE('',#92464,#20282);
#14249=LINE('',#92466,#20283);
#14250=LINE('',#92467,#20284);
#14251=LINE('',#92470,#20285);
#14252=LINE('',#92472,#20286);
#14253=LINE('',#92474,#20287);
#14254=LINE('',#92476,#20288);
#14255=LINE('',#92477,#20289);
#14256=LINE('',#92479,#20290);
#14257=LINE('',#92482,#20291);
#14258=LINE('',#92483,#20292);
#14259=LINE('',#92485,#20293);
#14260=LINE('',#92486,#20294);
#14261=LINE('',#92489,#20295);
#14262=LINE('',#92490,#20296);
#14263=LINE('',#92493,#20297);
#14264=LINE('',#92494,#20298);
#14265=LINE('',#92496,#20299);
#14266=LINE('',#92497,#20300);
#14267=LINE('',#92500,#20301);
#14268=LINE('',#92501,#20302);
#14269=LINE('',#92503,#20303);
#14270=LINE('',#92504,#20304);
#14271=LINE('',#92507,#20305);
#14272=LINE('',#92508,#20306);
#14273=LINE('',#92510,#20307);
#14274=LINE('',#92511,#20308);
#14275=LINE('',#92514,#20309);
#14276=LINE('',#92515,#20310);
#14277=LINE('',#92516,#20311);
#14278=LINE('',#92518,#20312);
#14279=LINE('',#92520,#20313);
#14280=LINE('',#92521,#20314);
#14281=LINE('',#92522,#20315);
#14282=LINE('',#92527,#20316);
#14283=LINE('',#92529,#20317);
#14284=LINE('',#92532,#20318);
#14285=LINE('',#92533,#20319);
#14286=LINE('',#92536,#20320);
#14287=LINE('',#92544,#20321);
#14288=LINE('',#92549,#20322);
#14289=LINE('',#92554,#20323);
#14290=LINE('',#92558,#20324);
#14291=LINE('',#92560,#20325);
#14292=LINE('',#92562,#20326);
#14293=LINE('',#92563,#20327);
#14294=LINE('',#92566,#20328);
#14295=LINE('',#92568,#20329);
#14296=LINE('',#92569,#20330);
#14297=LINE('',#92572,#20331);
#14298=LINE('',#92574,#20332);
#14299=LINE('',#92575,#20333);
#14300=LINE('',#92577,#20334);
#14301=LINE('',#92578,#20335);
#14302=LINE('',#92581,#20336);
#14303=LINE('',#92583,#20337);
#14304=LINE('',#92584,#20338);
#14305=LINE('',#92587,#20339);
#14306=LINE('',#92588,#20340);
#14307=LINE('',#92593,#20341);
#14308=LINE('',#92594,#20342);
#14309=LINE('',#92595,#20343);
#14310=LINE('',#92598,#20344);
#14311=LINE('',#92599,#20345);
#14312=LINE('',#92602,#20346);
#14313=LINE('',#92604,#20347);
#14314=LINE('',#92605,#20348);
#14315=LINE('',#92607,#20349);
#14316=LINE('',#92608,#20350);
#14317=LINE('',#92610,#20351);
#14318=LINE('',#92618,#20352);
#14319=LINE('',#92623,#20353);
#14320=LINE('',#92625,#20354);
#14321=LINE('',#92626,#20355);
#14322=LINE('',#92631,#20356);
#14323=LINE('',#92636,#20357);
#14324=LINE('',#92638,#20358);
#14325=LINE('',#92639,#20359);
#14326=LINE('',#92646,#20360);
#14327=LINE('',#92650,#20361);
#14328=LINE('',#92654,#20362);
#14329=LINE('',#92660,#20363);
#14330=LINE('',#92706,#20364);
#14331=LINE('',#92732,#20365);
#14332=LINE('',#92736,#20366);
#14333=LINE('',#92738,#20367);
#14334=LINE('',#92740,#20368);
#14335=LINE('',#92741,#20369);
#14336=LINE('',#92745,#20370);
#14337=LINE('',#92747,#20371);
#14338=LINE('',#92749,#20372);
#14339=LINE('',#92750,#20373);
#14340=LINE('',#92893,#20374);
#14341=LINE('',#92899,#20375);
#14342=LINE('',#93046,#20376);
#14343=LINE('',#93050,#20377);
#14344=LINE('',#93054,#20378);
#14345=LINE('',#93058,#20379);
#14346=LINE('',#93062,#20380);
#14347=LINE('',#93066,#20381);
#14348=LINE('',#93071,#20382);
#14349=LINE('',#93075,#20383);
#14350=LINE('',#93079,#20384);
#14351=LINE('',#93083,#20385);
#14352=LINE('',#93087,#20386);
#14353=LINE('',#93091,#20387);
#14354=LINE('',#93095,#20388);
#14355=LINE('',#93099,#20389);
#14356=LINE('',#93103,#20390);
#14357=LINE('',#93107,#20391);
#14358=LINE('',#93111,#20392);
#14359=LINE('',#93115,#20393);
#14360=LINE('',#93119,#20394);
#14361=LINE('',#93123,#20395);
#14362=LINE('',#93127,#20396);
#14363=LINE('',#93131,#20397);
#14364=LINE('',#93135,#20398);
#14365=LINE('',#93139,#20399);
#14366=LINE('',#93143,#20400);
#14367=LINE('',#93147,#20401);
#14368=LINE('',#93151,#20402);
#14369=LINE('',#93155,#20403);
#14370=LINE('',#93159,#20404);
#14371=LINE('',#93163,#20405);
#14372=LINE('',#93167,#20406);
#14373=LINE('',#93171,#20407);
#14374=LINE('',#93173,#20408);
#14375=LINE('',#93174,#20409);
#14376=LINE('',#93177,#20410);
#14377=LINE('',#93179,#20411);
#14378=LINE('',#93180,#20412);
#14379=LINE('',#93323,#20413);
#14380=LINE('',#93329,#20414);
#14381=LINE('',#93473,#20415);
#14382=LINE('',#93475,#20416);
#14383=LINE('',#93476,#20417);
#14384=LINE('',#93479,#20418);
#14385=LINE('',#93481,#20419);
#14386=LINE('',#93482,#20420);
#14387=LINE('',#93625,#20421);
#14388=LINE('',#93631,#20422);
#14389=LINE('',#93775,#20423);
#14390=LINE('',#93777,#20424);
#14391=LINE('',#93778,#20425);
#14392=LINE('',#93781,#20426);
#14393=LINE('',#93783,#20427);
#14394=LINE('',#93784,#20428);
#14395=LINE('',#93927,#20429);
#14396=LINE('',#93933,#20430);
#14397=LINE('',#94077,#20431);
#14398=LINE('',#94079,#20432);
#14399=LINE('',#94080,#20433);
#14400=LINE('',#94083,#20434);
#14401=LINE('',#94085,#20435);
#14402=LINE('',#94086,#20436);
#14403=LINE('',#94229,#20437);
#14404=LINE('',#94235,#20438);
#14405=LINE('',#94379,#20439);
#14406=LINE('',#94381,#20440);
#14407=LINE('',#94382,#20441);
#14408=LINE('',#94385,#20442);
#14409=LINE('',#94387,#20443);
#14410=LINE('',#94388,#20444);
#14411=LINE('',#94531,#20445);
#14412=LINE('',#94537,#20446);
#14413=LINE('',#94681,#20447);
#14414=LINE('',#94683,#20448);
#14415=LINE('',#94684,#20449);
#14416=LINE('',#94687,#20450);
#14417=LINE('',#94689,#20451);
#14418=LINE('',#94690,#20452);
#14419=LINE('',#94833,#20453);
#14420=LINE('',#94839,#20454);
#14421=LINE('',#94983,#20455);
#14422=LINE('',#94985,#20456);
#14423=LINE('',#94986,#20457);
#14424=LINE('',#94989,#20458);
#14425=LINE('',#94991,#20459);
#14426=LINE('',#94992,#20460);
#14427=LINE('',#95135,#20461);
#14428=LINE('',#95141,#20462);
#14429=LINE('',#95285,#20463);
#14430=LINE('',#95287,#20464);
#14431=LINE('',#95288,#20465);
#14432=LINE('',#95291,#20466);
#14433=LINE('',#95293,#20467);
#14434=LINE('',#95294,#20468);
#14435=LINE('',#95437,#20469);
#14436=LINE('',#95443,#20470);
#14437=LINE('',#95587,#20471);
#14438=LINE('',#95589,#20472);
#14439=LINE('',#95590,#20473);
#14440=LINE('',#95593,#20474);
#14441=LINE('',#95595,#20475);
#14442=LINE('',#95596,#20476);
#14443=LINE('',#95739,#20477);
#14444=LINE('',#95745,#20478);
#14445=LINE('',#95889,#20479);
#14446=LINE('',#95891,#20480);
#14447=LINE('',#95892,#20481);
#14448=LINE('',#95895,#20482);
#14449=LINE('',#95897,#20483);
#14450=LINE('',#95898,#20484);
#14451=LINE('',#96041,#20485);
#14452=LINE('',#96047,#20486);
#14453=LINE('',#96191,#20487);
#14454=LINE('',#96193,#20488);
#14455=LINE('',#96194,#20489);
#14456=LINE('',#96197,#20490);
#14457=LINE('',#96199,#20491);
#14458=LINE('',#96200,#20492);
#14459=LINE('',#96343,#20493);
#14460=LINE('',#96349,#20494);
#14461=LINE('',#96493,#20495);
#14462=LINE('',#96495,#20496);
#14463=LINE('',#96496,#20497);
#14464=LINE('',#96499,#20498);
#14465=LINE('',#96501,#20499);
#14466=LINE('',#96502,#20500);
#14467=LINE('',#96645,#20501);
#14468=LINE('',#96651,#20502);
#14469=LINE('',#96795,#20503);
#14470=LINE('',#96797,#20504);
#14471=LINE('',#96798,#20505);
#14472=LINE('',#96801,#20506);
#14473=LINE('',#96803,#20507);
#14474=LINE('',#96804,#20508);
#14475=LINE('',#96947,#20509);
#14476=LINE('',#96953,#20510);
#14477=LINE('',#97097,#20511);
#14478=LINE('',#97099,#20512);
#14479=LINE('',#97100,#20513);
#14480=LINE('',#97103,#20514);
#14481=LINE('',#97105,#20515);
#14482=LINE('',#97106,#20516);
#14483=LINE('',#97249,#20517);
#14484=LINE('',#97255,#20518);
#14485=LINE('',#97399,#20519);
#14486=LINE('',#97401,#20520);
#14487=LINE('',#97402,#20521);
#14488=LINE('',#97545,#20522);
#14489=LINE('',#97551,#20523);
#14490=LINE('',#97694,#20524);
#14491=LINE('',#97696,#20525);
#14492=LINE('',#97697,#20526);
#14493=LINE('',#97703,#20527);
#14494=LINE('',#97712,#20528);
#14495=LINE('',#97716,#20529);
#14496=LINE('',#97722,#20530);
#14497=LINE('',#97769,#20531);
#14498=LINE('',#97810,#20532);
#14499=LINE('',#97818,#20533);
#14500=LINE('',#97823,#20534);
#14501=LINE('',#97830,#20535);
#14502=LINE('',#98022,#20536);
#14503=LINE('',#98232,#20537);
#14504=LINE('',#98235,#20538);
#14505=LINE('',#98239,#20539);
#14506=LINE('',#98244,#20540);
#14507=LINE('',#98252,#20541);
#14508=LINE('',#98257,#20542);
#14509=LINE('',#98635,#20543);
#14510=LINE('',#98637,#20544);
#14511=LINE('',#98639,#20545);
#14512=LINE('',#98640,#20546);
#14513=LINE('',#98642,#20547);
#14514=LINE('',#98644,#20548);
#14515=LINE('',#98647,#20549);
#14516=LINE('',#98648,#20550);
#14517=LINE('',#98651,#20551);
#14518=LINE('',#98653,#20552);
#14519=LINE('',#98655,#20553);
#14520=LINE('',#98657,#20554);
#14521=LINE('',#98658,#20555);
#14522=LINE('',#98660,#20556);
#14523=LINE('',#98662,#20557);
#14524=LINE('',#98665,#20558);
#14525=LINE('',#98666,#20559);
#14526=LINE('',#98669,#20560);
#14527=LINE('',#98671,#20561);
#14528=LINE('',#98673,#20562);
#14529=LINE('',#98675,#20563);
#14530=LINE('',#98676,#20564);
#14531=LINE('',#98678,#20565);
#14532=LINE('',#98680,#20566);
#14533=LINE('',#98683,#20567);
#14534=LINE('',#98684,#20568);
#14535=LINE('',#98687,#20569);
#14536=LINE('',#98689,#20570);
#14537=LINE('',#98691,#20571);
#14538=LINE('',#98693,#20572);
#14539=LINE('',#98694,#20573);
#14540=LINE('',#98696,#20574);
#14541=LINE('',#98698,#20575);
#14542=LINE('',#98701,#20576);
#14543=LINE('',#98702,#20577);
#14544=LINE('',#98705,#20578);
#14545=LINE('',#98707,#20579);
#14546=LINE('',#98709,#20580);
#14547=LINE('',#98711,#20581);
#14548=LINE('',#98712,#20582);
#14549=LINE('',#98714,#20583);
#14550=LINE('',#98716,#20584);
#14551=LINE('',#98719,#20585);
#14552=LINE('',#98720,#20586);
#14553=LINE('',#98723,#20587);
#14554=LINE('',#98725,#20588);
#14555=LINE('',#98727,#20589);
#14556=LINE('',#98729,#20590);
#14557=LINE('',#98730,#20591);
#14558=LINE('',#98732,#20592);
#14559=LINE('',#98734,#20593);
#14560=LINE('',#98737,#20594);
#14561=LINE('',#98738,#20595);
#14562=LINE('',#98741,#20596);
#14563=LINE('',#98743,#20597);
#14564=LINE('',#98745,#20598);
#14565=LINE('',#98747,#20599);
#14566=LINE('',#98748,#20600);
#14567=LINE('',#98750,#20601);
#14568=LINE('',#98752,#20602);
#14569=LINE('',#98755,#20603);
#14570=LINE('',#98756,#20604);
#14571=LINE('',#98759,#20605);
#14572=LINE('',#98761,#20606);
#14573=LINE('',#98763,#20607);
#14574=LINE('',#98765,#20608);
#14575=LINE('',#98766,#20609);
#14576=LINE('',#98768,#20610);
#14577=LINE('',#98770,#20611);
#14578=LINE('',#98773,#20612);
#14579=LINE('',#98774,#20613);
#14580=LINE('',#98777,#20614);
#14581=LINE('',#98779,#20615);
#14582=LINE('',#98781,#20616);
#14583=LINE('',#98783,#20617);
#14584=LINE('',#98784,#20618);
#14585=LINE('',#98786,#20619);
#14586=LINE('',#98788,#20620);
#14587=LINE('',#98791,#20621);
#14588=LINE('',#98792,#20622);
#14589=LINE('',#98795,#20623);
#14590=LINE('',#98797,#20624);
#14591=LINE('',#98799,#20625);
#14592=LINE('',#98801,#20626);
#14593=LINE('',#98802,#20627);
#14594=LINE('',#98804,#20628);
#14595=LINE('',#98806,#20629);
#14596=LINE('',#98809,#20630);
#14597=LINE('',#98810,#20631);
#14598=LINE('',#98813,#20632);
#14599=LINE('',#98815,#20633);
#14600=LINE('',#98817,#20634);
#14601=LINE('',#98819,#20635);
#14602=LINE('',#98820,#20636);
#14603=LINE('',#98822,#20637);
#14604=LINE('',#98824,#20638);
#14605=LINE('',#98827,#20639);
#14606=LINE('',#98828,#20640);
#14607=LINE('',#98831,#20641);
#14608=LINE('',#98833,#20642);
#14609=LINE('',#98835,#20643);
#14610=LINE('',#98837,#20644);
#14611=LINE('',#98838,#20645);
#14612=LINE('',#98840,#20646);
#14613=LINE('',#98842,#20647);
#14614=LINE('',#98845,#20648);
#14615=LINE('',#98846,#20649);
#14616=LINE('',#98849,#20650);
#14617=LINE('',#98851,#20651);
#14618=LINE('',#98853,#20652);
#14619=LINE('',#98855,#20653);
#14620=LINE('',#98856,#20654);
#14621=LINE('',#98862,#20655);
#14622=LINE('',#98870,#20656);
#14623=LINE('',#98874,#20657);
#14624=LINE('',#98878,#20658);
#14625=LINE('',#98885,#20659);
#14626=LINE('',#98889,#20660);
#14627=LINE('',#98897,#20661);
#14628=LINE('',#98903,#20662);
#14629=LINE('',#98906,#20663);
#14630=LINE('',#98912,#20664);
#14631=LINE('',#98920,#20665);
#14632=LINE('',#98924,#20666);
#14633=LINE('',#98931,#20667);
#14634=LINE('',#98935,#20668);
#14635=LINE('',#98941,#20669);
#14636=LINE('',#98944,#20670);
#14637=LINE('',#98950,#20671);
#14638=LINE('',#98954,#20672);
#14639=LINE('',#98959,#20673);
#14640=LINE('',#98961,#20674);
#14641=LINE('',#98963,#20675);
#14642=LINE('',#98964,#20676);
#14643=LINE('',#98969,#20677);
#14644=LINE('',#98973,#20678);
#14645=LINE('',#98978,#20679);
#14646=LINE('',#98980,#20680);
#14647=LINE('',#98982,#20681);
#14648=LINE('',#98983,#20682);
#14649=LINE('',#98992,#20683);
#14650=LINE('',#98996,#20684);
#14651=LINE('',#99001,#20685);
#14652=LINE('',#99003,#20686);
#14653=LINE('',#99005,#20687);
#14654=LINE('',#99006,#20688);
#14655=LINE('',#99009,#20689);
#14656=LINE('',#99011,#20690);
#14657=LINE('',#99012,#20691);
#14658=LINE('',#99013,#20692);
#14659=LINE('',#99016,#20693);
#14660=LINE('',#99017,#20694);
#14661=LINE('',#99020,#20695);
#14662=LINE('',#99021,#20696);
#14663=LINE('',#99024,#20697);
#14664=LINE('',#99026,#20698);
#14665=LINE('',#99027,#20699);
#14666=LINE('',#99030,#20700);
#14667=LINE('',#99032,#20701);
#14668=LINE('',#99033,#20702);
#14669=LINE('',#99036,#20703);
#14670=LINE('',#99038,#20704);
#14671=LINE('',#99039,#20705);
#14672=LINE('',#99042,#20706);
#14673=LINE('',#99044,#20707);
#14674=LINE('',#99045,#20708);
#14675=LINE('',#99048,#20709);
#14676=LINE('',#99050,#20710);
#14677=LINE('',#99051,#20711);
#14678=LINE('',#99054,#20712);
#14679=LINE('',#99056,#20713);
#14680=LINE('',#99057,#20714);
#14681=LINE('',#99060,#20715);
#14682=LINE('',#99062,#20716);
#14683=LINE('',#99063,#20717);
#14684=LINE('',#99066,#20718);
#14685=LINE('',#99068,#20719);
#14686=LINE('',#99069,#20720);
#14687=LINE('',#99072,#20721);
#14688=LINE('',#99074,#20722);
#14689=LINE('',#99075,#20723);
#14690=LINE('',#99078,#20724);
#14691=LINE('',#99080,#20725);
#14692=LINE('',#99081,#20726);
#14693=LINE('',#99084,#20727);
#14694=LINE('',#99086,#20728);
#14695=LINE('',#99087,#20729);
#14696=LINE('',#99090,#20730);
#14697=LINE('',#99092,#20731);
#14698=LINE('',#99093,#20732);
#14699=LINE('',#99096,#20733);
#14700=LINE('',#99098,#20734);
#14701=LINE('',#99099,#20735);
#14702=LINE('',#99102,#20736);
#14703=LINE('',#99104,#20737);
#14704=LINE('',#99105,#20738);
#14705=LINE('',#99108,#20739);
#14706=LINE('',#99110,#20740);
#14707=LINE('',#99111,#20741);
#14708=LINE('',#99114,#20742);
#14709=LINE('',#99116,#20743);
#14710=LINE('',#99117,#20744);
#14711=LINE('',#99120,#20745);
#14712=LINE('',#99122,#20746);
#14713=LINE('',#99123,#20747);
#14714=LINE('',#99126,#20748);
#14715=LINE('',#99128,#20749);
#14716=LINE('',#99129,#20750);
#14717=LINE('',#99132,#20751);
#14718=LINE('',#99134,#20752);
#14719=LINE('',#99135,#20753);
#14720=LINE('',#99138,#20754);
#14721=LINE('',#99140,#20755);
#14722=LINE('',#99141,#20756);
#14723=LINE('',#99144,#20757);
#14724=LINE('',#99146,#20758);
#14725=LINE('',#99147,#20759);
#14726=LINE('',#99150,#20760);
#14727=LINE('',#99152,#20761);
#14728=LINE('',#99153,#20762);
#14729=LINE('',#99156,#20763);
#14730=LINE('',#99158,#20764);
#14731=LINE('',#99159,#20765);
#14732=LINE('',#99162,#20766);
#14733=LINE('',#99164,#20767);
#14734=LINE('',#99165,#20768);
#14735=LINE('',#99168,#20769);
#14736=LINE('',#99170,#20770);
#14737=LINE('',#99171,#20771);
#14738=LINE('',#99174,#20772);
#14739=LINE('',#99176,#20773);
#14740=LINE('',#99177,#20774);
#14741=LINE('',#99180,#20775);
#14742=LINE('',#99182,#20776);
#14743=LINE('',#99183,#20777);
#14744=LINE('',#99186,#20778);
#14745=LINE('',#99188,#20779);
#14746=LINE('',#99189,#20780);
#14747=LINE('',#99192,#20781);
#14748=LINE('',#99194,#20782);
#14749=LINE('',#99195,#20783);
#14750=LINE('',#99198,#20784);
#14751=LINE('',#99200,#20785);
#14752=LINE('',#99201,#20786);
#14753=LINE('',#99204,#20787);
#14754=LINE('',#99206,#20788);
#14755=LINE('',#99207,#20789);
#14756=LINE('',#99210,#20790);
#14757=LINE('',#99212,#20791);
#14758=LINE('',#99213,#20792);
#14759=LINE('',#99216,#20793);
#14760=LINE('',#99218,#20794);
#14761=LINE('',#99219,#20795);
#14762=LINE('',#99222,#20796);
#14763=LINE('',#99224,#20797);
#14764=LINE('',#99225,#20798);
#14765=LINE('',#99228,#20799);
#14766=LINE('',#99230,#20800);
#14767=LINE('',#99231,#20801);
#14768=LINE('',#99234,#20802);
#14769=LINE('',#99236,#20803);
#14770=LINE('',#99237,#20804);
#14771=LINE('',#99240,#20805);
#14772=LINE('',#99242,#20806);
#14773=LINE('',#99243,#20807);
#14774=LINE('',#99246,#20808);
#14775=LINE('',#99248,#20809);
#14776=LINE('',#99249,#20810);
#14777=LINE('',#99252,#20811);
#14778=LINE('',#99254,#20812);
#14779=LINE('',#99255,#20813);
#14780=LINE('',#99258,#20814);
#14781=LINE('',#99260,#20815);
#14782=LINE('',#99261,#20816);
#14783=LINE('',#99264,#20817);
#14784=LINE('',#99266,#20818);
#14785=LINE('',#99267,#20819);
#14786=LINE('',#99270,#20820);
#14787=LINE('',#99272,#20821);
#14788=LINE('',#99273,#20822);
#14789=LINE('',#99276,#20823);
#14790=LINE('',#99278,#20824);
#14791=LINE('',#99279,#20825);
#14792=LINE('',#99282,#20826);
#14793=LINE('',#99284,#20827);
#14794=LINE('',#99285,#20828);
#14795=LINE('',#99288,#20829);
#14796=LINE('',#99290,#20830);
#14797=LINE('',#99291,#20831);
#14798=LINE('',#99294,#20832);
#14799=LINE('',#99296,#20833);
#14800=LINE('',#99297,#20834);
#14801=LINE('',#99300,#20835);
#14802=LINE('',#99302,#20836);
#14803=LINE('',#99303,#20837);
#14804=LINE('',#99306,#20838);
#14805=LINE('',#99308,#20839);
#14806=LINE('',#99309,#20840);
#14807=LINE('',#99312,#20841);
#14808=LINE('',#99314,#20842);
#14809=LINE('',#99315,#20843);
#14810=LINE('',#99318,#20844);
#14811=LINE('',#99320,#20845);
#14812=LINE('',#99321,#20846);
#14813=LINE('',#99324,#20847);
#14814=LINE('',#99326,#20848);
#14815=LINE('',#99327,#20849);
#14816=LINE('',#99330,#20850);
#14817=LINE('',#99332,#20851);
#14818=LINE('',#99333,#20852);
#14819=LINE('',#99336,#20853);
#14820=LINE('',#99338,#20854);
#14821=LINE('',#99339,#20855);
#14822=LINE('',#99342,#20856);
#14823=LINE('',#99344,#20857);
#14824=LINE('',#99345,#20858);
#14825=LINE('',#99348,#20859);
#14826=LINE('',#99350,#20860);
#14827=LINE('',#99351,#20861);
#14828=LINE('',#99354,#20862);
#14829=LINE('',#99356,#20863);
#14830=LINE('',#99357,#20864);
#14831=LINE('',#99360,#20865);
#14832=LINE('',#99362,#20866);
#14833=LINE('',#99363,#20867);
#14834=LINE('',#99366,#20868);
#14835=LINE('',#99368,#20869);
#14836=LINE('',#99369,#20870);
#14837=LINE('',#99372,#20871);
#14838=LINE('',#99374,#20872);
#14839=LINE('',#99375,#20873);
#14840=LINE('',#99378,#20874);
#14841=LINE('',#99380,#20875);
#14842=LINE('',#99381,#20876);
#14843=LINE('',#99384,#20877);
#14844=LINE('',#99386,#20878);
#14845=LINE('',#99387,#20879);
#14846=LINE('',#99390,#20880);
#14847=LINE('',#99392,#20881);
#14848=LINE('',#99393,#20882);
#14849=LINE('',#99396,#20883);
#14850=LINE('',#99398,#20884);
#14851=LINE('',#99399,#20885);
#14852=LINE('',#99402,#20886);
#14853=LINE('',#99404,#20887);
#14854=LINE('',#99405,#20888);
#14855=LINE('',#99408,#20889);
#14856=LINE('',#99410,#20890);
#14857=LINE('',#99411,#20891);
#14858=LINE('',#99414,#20892);
#14859=LINE('',#99416,#20893);
#14860=LINE('',#99417,#20894);
#14861=LINE('',#99420,#20895);
#14862=LINE('',#99422,#20896);
#14863=LINE('',#99423,#20897);
#14864=LINE('',#99426,#20898);
#14865=LINE('',#99428,#20899);
#14866=LINE('',#99429,#20900);
#14867=LINE('',#99432,#20901);
#14868=LINE('',#99434,#20902);
#14869=LINE('',#99435,#20903);
#14870=LINE('',#99438,#20904);
#14871=LINE('',#99440,#20905);
#14872=LINE('',#99441,#20906);
#14873=LINE('',#99444,#20907);
#14874=LINE('',#99446,#20908);
#14875=LINE('',#99447,#20909);
#14876=LINE('',#99450,#20910);
#14877=LINE('',#99452,#20911);
#14878=LINE('',#99453,#20912);
#14879=LINE('',#99456,#20913);
#14880=LINE('',#99458,#20914);
#14881=LINE('',#99459,#20915);
#14882=LINE('',#99462,#20916);
#14883=LINE('',#99464,#20917);
#14884=LINE('',#99465,#20918);
#14885=LINE('',#99468,#20919);
#14886=LINE('',#99470,#20920);
#14887=LINE('',#99471,#20921);
#14888=LINE('',#99474,#20922);
#14889=LINE('',#99476,#20923);
#14890=LINE('',#99477,#20924);
#14891=LINE('',#99480,#20925);
#14892=LINE('',#99482,#20926);
#14893=LINE('',#99483,#20927);
#14894=LINE('',#99486,#20928);
#14895=LINE('',#99488,#20929);
#14896=LINE('',#99489,#20930);
#14897=LINE('',#99492,#20931);
#14898=LINE('',#99494,#20932);
#14899=LINE('',#99495,#20933);
#14900=LINE('',#99498,#20934);
#14901=LINE('',#99500,#20935);
#14902=LINE('',#99501,#20936);
#14903=LINE('',#99504,#20937);
#14904=LINE('',#99506,#20938);
#14905=LINE('',#99507,#20939);
#14906=LINE('',#99510,#20940);
#14907=LINE('',#99512,#20941);
#14908=LINE('',#99513,#20942);
#14909=LINE('',#99516,#20943);
#14910=LINE('',#99518,#20944);
#14911=LINE('',#99519,#20945);
#14912=LINE('',#99522,#20946);
#14913=LINE('',#99524,#20947);
#14914=LINE('',#99525,#20948);
#14915=LINE('',#99528,#20949);
#14916=LINE('',#99530,#20950);
#14917=LINE('',#99531,#20951);
#14918=LINE('',#99534,#20952);
#14919=LINE('',#99536,#20953);
#14920=LINE('',#99537,#20954);
#14921=LINE('',#99540,#20955);
#14922=LINE('',#99542,#20956);
#14923=LINE('',#99543,#20957);
#14924=LINE('',#99546,#20958);
#14925=LINE('',#99548,#20959);
#14926=LINE('',#99549,#20960);
#14927=LINE('',#99552,#20961);
#14928=LINE('',#99554,#20962);
#14929=LINE('',#99555,#20963);
#14930=LINE('',#99558,#20964);
#14931=LINE('',#99560,#20965);
#14932=LINE('',#99561,#20966);
#14933=LINE('',#99564,#20967);
#14934=LINE('',#99566,#20968);
#14935=LINE('',#99567,#20969);
#14936=LINE('',#99570,#20970);
#14937=LINE('',#99572,#20971);
#14938=LINE('',#99573,#20972);
#14939=LINE('',#99576,#20973);
#14940=LINE('',#99578,#20974);
#14941=LINE('',#99579,#20975);
#14942=LINE('',#99582,#20976);
#14943=LINE('',#99584,#20977);
#14944=LINE('',#99585,#20978);
#14945=LINE('',#99588,#20979);
#14946=LINE('',#99590,#20980);
#14947=LINE('',#99591,#20981);
#14948=LINE('',#99594,#20982);
#14949=LINE('',#99596,#20983);
#14950=LINE('',#99597,#20984);
#14951=LINE('',#99600,#20985);
#14952=LINE('',#99602,#20986);
#14953=LINE('',#99603,#20987);
#14954=LINE('',#99606,#20988);
#14955=LINE('',#99608,#20989);
#14956=LINE('',#99609,#20990);
#14957=LINE('',#99612,#20991);
#14958=LINE('',#99614,#20992);
#14959=LINE('',#99615,#20993);
#14960=LINE('',#99618,#20994);
#14961=LINE('',#99620,#20995);
#14962=LINE('',#99621,#20996);
#14963=LINE('',#99624,#20997);
#14964=LINE('',#99626,#20998);
#14965=LINE('',#99627,#20999);
#14966=LINE('',#99630,#21000);
#14967=LINE('',#99632,#21001);
#14968=LINE('',#99633,#21002);
#14969=LINE('',#99636,#21003);
#14970=LINE('',#99638,#21004);
#14971=LINE('',#99639,#21005);
#14972=LINE('',#99642,#21006);
#14973=LINE('',#99644,#21007);
#14974=LINE('',#99645,#21008);
#14975=LINE('',#99648,#21009);
#14976=LINE('',#99650,#21010);
#14977=LINE('',#99651,#21011);
#14978=LINE('',#99654,#21012);
#14979=LINE('',#99656,#21013);
#14980=LINE('',#99657,#21014);
#14981=LINE('',#99660,#21015);
#14982=LINE('',#99662,#21016);
#14983=LINE('',#99663,#21017);
#14984=LINE('',#99666,#21018);
#14985=LINE('',#99668,#21019);
#14986=LINE('',#99669,#21020);
#14987=LINE('',#99672,#21021);
#14988=LINE('',#99674,#21022);
#14989=LINE('',#99675,#21023);
#14990=LINE('',#99678,#21024);
#14991=LINE('',#99680,#21025);
#14992=LINE('',#99681,#21026);
#14993=LINE('',#99684,#21027);
#14994=LINE('',#99686,#21028);
#14995=LINE('',#99687,#21029);
#14996=LINE('',#99690,#21030);
#14997=LINE('',#99692,#21031);
#14998=LINE('',#99693,#21032);
#14999=LINE('',#99696,#21033);
#15000=LINE('',#99698,#21034);
#15001=LINE('',#99699,#21035);
#15002=LINE('',#99702,#21036);
#15003=LINE('',#99704,#21037);
#15004=LINE('',#99705,#21038);
#15005=LINE('',#99708,#21039);
#15006=LINE('',#99710,#21040);
#15007=LINE('',#99711,#21041);
#15008=LINE('',#99714,#21042);
#15009=LINE('',#99716,#21043);
#15010=LINE('',#99717,#21044);
#15011=LINE('',#99720,#21045);
#15012=LINE('',#99722,#21046);
#15013=LINE('',#99723,#21047);
#15014=LINE('',#99726,#21048);
#15015=LINE('',#99728,#21049);
#15016=LINE('',#99729,#21050);
#15017=LINE('',#99732,#21051);
#15018=LINE('',#99734,#21052);
#15019=LINE('',#99735,#21053);
#15020=LINE('',#99738,#21054);
#15021=LINE('',#99740,#21055);
#15022=LINE('',#99741,#21056);
#15023=LINE('',#99744,#21057);
#15024=LINE('',#99746,#21058);
#15025=LINE('',#99747,#21059);
#15026=LINE('',#99750,#21060);
#15027=LINE('',#99752,#21061);
#15028=LINE('',#99753,#21062);
#15029=LINE('',#99756,#21063);
#15030=LINE('',#99758,#21064);
#15031=LINE('',#99759,#21065);
#15032=LINE('',#99762,#21066);
#15033=LINE('',#99764,#21067);
#15034=LINE('',#99765,#21068);
#15035=LINE('',#99768,#21069);
#15036=LINE('',#99770,#21070);
#15037=LINE('',#99771,#21071);
#15038=LINE('',#99774,#21072);
#15039=LINE('',#99776,#21073);
#15040=LINE('',#99777,#21074);
#15041=LINE('',#99780,#21075);
#15042=LINE('',#99782,#21076);
#15043=LINE('',#99783,#21077);
#15044=LINE('',#99786,#21078);
#15045=LINE('',#99788,#21079);
#15046=LINE('',#99789,#21080);
#15047=LINE('',#99792,#21081);
#15048=LINE('',#99794,#21082);
#15049=LINE('',#99795,#21083);
#15050=LINE('',#99798,#21084);
#15051=LINE('',#99800,#21085);
#15052=LINE('',#99801,#21086);
#15053=LINE('',#99804,#21087);
#15054=LINE('',#99806,#21088);
#15055=LINE('',#99807,#21089);
#15056=LINE('',#99810,#21090);
#15057=LINE('',#99812,#21091);
#15058=LINE('',#99813,#21092);
#15059=LINE('',#99816,#21093);
#15060=LINE('',#99818,#21094);
#15061=LINE('',#99819,#21095);
#15062=LINE('',#99822,#21096);
#15063=LINE('',#99824,#21097);
#15064=LINE('',#99825,#21098);
#15065=LINE('',#99828,#21099);
#15066=LINE('',#99830,#21100);
#15067=LINE('',#99831,#21101);
#15068=LINE('',#99834,#21102);
#15069=LINE('',#99836,#21103);
#15070=LINE('',#99837,#21104);
#15071=LINE('',#99840,#21105);
#15072=LINE('',#99842,#21106);
#15073=LINE('',#99843,#21107);
#15074=LINE('',#99846,#21108);
#15075=LINE('',#99848,#21109);
#15076=LINE('',#99849,#21110);
#15077=LINE('',#99852,#21111);
#15078=LINE('',#99854,#21112);
#15079=LINE('',#99855,#21113);
#15080=LINE('',#99858,#21114);
#15081=LINE('',#99860,#21115);
#15082=LINE('',#99861,#21116);
#15083=LINE('',#99864,#21117);
#15084=LINE('',#99866,#21118);
#15085=LINE('',#99867,#21119);
#15086=LINE('',#99870,#21120);
#15087=LINE('',#99872,#21121);
#15088=LINE('',#99873,#21122);
#15089=LINE('',#99876,#21123);
#15090=LINE('',#99878,#21124);
#15091=LINE('',#99879,#21125);
#15092=LINE('',#99882,#21126);
#15093=LINE('',#99884,#21127);
#15094=LINE('',#99885,#21128);
#15095=LINE('',#99888,#21129);
#15096=LINE('',#99890,#21130);
#15097=LINE('',#99891,#21131);
#15098=LINE('',#99894,#21132);
#15099=LINE('',#99896,#21133);
#15100=LINE('',#99897,#21134);
#15101=LINE('',#99900,#21135);
#15102=LINE('',#99902,#21136);
#15103=LINE('',#99903,#21137);
#15104=LINE('',#99906,#21138);
#15105=LINE('',#99908,#21139);
#15106=LINE('',#99909,#21140);
#15107=LINE('',#99912,#21141);
#15108=LINE('',#99914,#21142);
#15109=LINE('',#99915,#21143);
#15110=LINE('',#99918,#21144);
#15111=LINE('',#99920,#21145);
#15112=LINE('',#99921,#21146);
#15113=LINE('',#99924,#21147);
#15114=LINE('',#99926,#21148);
#15115=LINE('',#99927,#21149);
#15116=LINE('',#99930,#21150);
#15117=LINE('',#99932,#21151);
#15118=LINE('',#99933,#21152);
#15119=LINE('',#99936,#21153);
#15120=LINE('',#99938,#21154);
#15121=LINE('',#99939,#21155);
#15122=LINE('',#99942,#21156);
#15123=LINE('',#99944,#21157);
#15124=LINE('',#99945,#21158);
#15125=LINE('',#99948,#21159);
#15126=LINE('',#99950,#21160);
#15127=LINE('',#99951,#21161);
#15128=LINE('',#99954,#21162);
#15129=LINE('',#99956,#21163);
#15130=LINE('',#99957,#21164);
#15131=LINE('',#99960,#21165);
#15132=LINE('',#99962,#21166);
#15133=LINE('',#99963,#21167);
#15134=LINE('',#99966,#21168);
#15135=LINE('',#99968,#21169);
#15136=LINE('',#99969,#21170);
#15137=LINE('',#99972,#21171);
#15138=LINE('',#99974,#21172);
#15139=LINE('',#99975,#21173);
#15140=LINE('',#99978,#21174);
#15141=LINE('',#99980,#21175);
#15142=LINE('',#99981,#21176);
#15143=LINE('',#99984,#21177);
#15144=LINE('',#99986,#21178);
#15145=LINE('',#99987,#21179);
#15146=LINE('',#99990,#21180);
#15147=LINE('',#99992,#21181);
#15148=LINE('',#99993,#21182);
#15149=LINE('',#99996,#21183);
#15150=LINE('',#99998,#21184);
#15151=LINE('',#99999,#21185);
#15152=LINE('',#100002,#21186);
#15153=LINE('',#100004,#21187);
#15154=LINE('',#100005,#21188);
#15155=LINE('',#100008,#21189);
#15156=LINE('',#100010,#21190);
#15157=LINE('',#100011,#21191);
#15158=LINE('',#100014,#21192);
#15159=LINE('',#100016,#21193);
#15160=LINE('',#100017,#21194);
#15161=LINE('',#100020,#21195);
#15162=LINE('',#100022,#21196);
#15163=LINE('',#100023,#21197);
#15164=LINE('',#100026,#21198);
#15165=LINE('',#100028,#21199);
#15166=LINE('',#100029,#21200);
#15167=LINE('',#100032,#21201);
#15168=LINE('',#100034,#21202);
#15169=LINE('',#100035,#21203);
#15170=LINE('',#100038,#21204);
#15171=LINE('',#100040,#21205);
#15172=LINE('',#100041,#21206);
#15173=LINE('',#100044,#21207);
#15174=LINE('',#100046,#21208);
#15175=LINE('',#100047,#21209);
#15176=LINE('',#100050,#21210);
#15177=LINE('',#100052,#21211);
#15178=LINE('',#100053,#21212);
#15179=LINE('',#100056,#21213);
#15180=LINE('',#100058,#21214);
#15181=LINE('',#100059,#21215);
#15182=LINE('',#100062,#21216);
#15183=LINE('',#100064,#21217);
#15184=LINE('',#100065,#21218);
#15185=LINE('',#100068,#21219);
#15186=LINE('',#100070,#21220);
#15187=LINE('',#100071,#21221);
#15188=LINE('',#100074,#21222);
#15189=LINE('',#100076,#21223);
#15190=LINE('',#100077,#21224);
#15191=LINE('',#100080,#21225);
#15192=LINE('',#100082,#21226);
#15193=LINE('',#100083,#21227);
#15194=LINE('',#100086,#21228);
#15195=LINE('',#100088,#21229);
#15196=LINE('',#100089,#21230);
#15197=LINE('',#100092,#21231);
#15198=LINE('',#100094,#21232);
#15199=LINE('',#100095,#21233);
#15200=LINE('',#100098,#21234);
#15201=LINE('',#100100,#21235);
#15202=LINE('',#100101,#21236);
#15203=LINE('',#100104,#21237);
#15204=LINE('',#100106,#21238);
#15205=LINE('',#100107,#21239);
#15206=LINE('',#100110,#21240);
#15207=LINE('',#100112,#21241);
#15208=LINE('',#100113,#21242);
#15209=LINE('',#100116,#21243);
#15210=LINE('',#100118,#21244);
#15211=LINE('',#100119,#21245);
#15212=LINE('',#100122,#21246);
#15213=LINE('',#100124,#21247);
#15214=LINE('',#100125,#21248);
#15215=LINE('',#100128,#21249);
#15216=LINE('',#100130,#21250);
#15217=LINE('',#100131,#21251);
#15218=LINE('',#100134,#21252);
#15219=LINE('',#100136,#21253);
#15220=LINE('',#100137,#21254);
#15221=LINE('',#100140,#21255);
#15222=LINE('',#100142,#21256);
#15223=LINE('',#100143,#21257);
#15224=LINE('',#100146,#21258);
#15225=LINE('',#100148,#21259);
#15226=LINE('',#100149,#21260);
#15227=LINE('',#100152,#21261);
#15228=LINE('',#100154,#21262);
#15229=LINE('',#100155,#21263);
#15230=LINE('',#100158,#21264);
#15231=LINE('',#100160,#21265);
#15232=LINE('',#100161,#21266);
#15233=LINE('',#100164,#21267);
#15234=LINE('',#100166,#21268);
#15235=LINE('',#100167,#21269);
#15236=LINE('',#100170,#21270);
#15237=LINE('',#100172,#21271);
#15238=LINE('',#100173,#21272);
#15239=LINE('',#100176,#21273);
#15240=LINE('',#100178,#21274);
#15241=LINE('',#100179,#21275);
#15242=LINE('',#100182,#21276);
#15243=LINE('',#100184,#21277);
#15244=LINE('',#100185,#21278);
#15245=LINE('',#100188,#21279);
#15246=LINE('',#100190,#21280);
#15247=LINE('',#100191,#21281);
#15248=LINE('',#100194,#21282);
#15249=LINE('',#100196,#21283);
#15250=LINE('',#100197,#21284);
#15251=LINE('',#100200,#21285);
#15252=LINE('',#100202,#21286);
#15253=LINE('',#100203,#21287);
#15254=LINE('',#100206,#21288);
#15255=LINE('',#100208,#21289);
#15256=LINE('',#100209,#21290);
#15257=LINE('',#100212,#21291);
#15258=LINE('',#100214,#21292);
#15259=LINE('',#100215,#21293);
#15260=LINE('',#100218,#21294);
#15261=LINE('',#100220,#21295);
#15262=LINE('',#100221,#21296);
#15263=LINE('',#100224,#21297);
#15264=LINE('',#100226,#21298);
#15265=LINE('',#100227,#21299);
#15266=LINE('',#100230,#21300);
#15267=LINE('',#100232,#21301);
#15268=LINE('',#100233,#21302);
#15269=LINE('',#100236,#21303);
#15270=LINE('',#100238,#21304);
#15271=LINE('',#100239,#21305);
#15272=LINE('',#100242,#21306);
#15273=LINE('',#100244,#21307);
#15274=LINE('',#100245,#21308);
#15275=LINE('',#100248,#21309);
#15276=LINE('',#100250,#21310);
#15277=LINE('',#100251,#21311);
#15278=LINE('',#100254,#21312);
#15279=LINE('',#100256,#21313);
#15280=LINE('',#100257,#21314);
#15281=LINE('',#100260,#21315);
#15282=LINE('',#100262,#21316);
#15283=LINE('',#100263,#21317);
#15284=LINE('',#100266,#21318);
#15285=LINE('',#100268,#21319);
#15286=LINE('',#100269,#21320);
#15287=LINE('',#100272,#21321);
#15288=LINE('',#100274,#21322);
#15289=LINE('',#100275,#21323);
#15290=LINE('',#100278,#21324);
#15291=LINE('',#100280,#21325);
#15292=LINE('',#100281,#21326);
#15293=LINE('',#100284,#21327);
#15294=LINE('',#100286,#21328);
#15295=LINE('',#100287,#21329);
#15296=LINE('',#100290,#21330);
#15297=LINE('',#100292,#21331);
#15298=LINE('',#100293,#21332);
#15299=LINE('',#100296,#21333);
#15300=LINE('',#100298,#21334);
#15301=LINE('',#100299,#21335);
#15302=LINE('',#100302,#21336);
#15303=LINE('',#100304,#21337);
#15304=LINE('',#100305,#21338);
#15305=LINE('',#100308,#21339);
#15306=LINE('',#100310,#21340);
#15307=LINE('',#100311,#21341);
#15308=LINE('',#100314,#21342);
#15309=LINE('',#100316,#21343);
#15310=LINE('',#100317,#21344);
#15311=LINE('',#100320,#21345);
#15312=LINE('',#100322,#21346);
#15313=LINE('',#100323,#21347);
#15314=LINE('',#100326,#21348);
#15315=LINE('',#100328,#21349);
#15316=LINE('',#100329,#21350);
#15317=LINE('',#100332,#21351);
#15318=LINE('',#100334,#21352);
#15319=LINE('',#100335,#21353);
#15320=LINE('',#100338,#21354);
#15321=LINE('',#100340,#21355);
#15322=LINE('',#100341,#21356);
#15323=LINE('',#100344,#21357);
#15324=LINE('',#100346,#21358);
#15325=LINE('',#100347,#21359);
#15326=LINE('',#100350,#21360);
#15327=LINE('',#100352,#21361);
#15328=LINE('',#100353,#21362);
#15329=LINE('',#100356,#21363);
#15330=LINE('',#100358,#21364);
#15331=LINE('',#100359,#21365);
#15332=LINE('',#100362,#21366);
#15333=LINE('',#100364,#21367);
#15334=LINE('',#100365,#21368);
#15335=LINE('',#100368,#21369);
#15336=LINE('',#100370,#21370);
#15337=LINE('',#100371,#21371);
#15338=LINE('',#100374,#21372);
#15339=LINE('',#100376,#21373);
#15340=LINE('',#100377,#21374);
#15341=LINE('',#100380,#21375);
#15342=LINE('',#100382,#21376);
#15343=LINE('',#100383,#21377);
#15344=LINE('',#100386,#21378);
#15345=LINE('',#100388,#21379);
#15346=LINE('',#100389,#21380);
#15347=LINE('',#100392,#21381);
#15348=LINE('',#100394,#21382);
#15349=LINE('',#100395,#21383);
#15350=LINE('',#100398,#21384);
#15351=LINE('',#100400,#21385);
#15352=LINE('',#100401,#21386);
#15353=LINE('',#100404,#21387);
#15354=LINE('',#100406,#21388);
#15355=LINE('',#100407,#21389);
#15356=LINE('',#100410,#21390);
#15357=LINE('',#100412,#21391);
#15358=LINE('',#100413,#21392);
#15359=LINE('',#100416,#21393);
#15360=LINE('',#100418,#21394);
#15361=LINE('',#100419,#21395);
#15362=LINE('',#100422,#21396);
#15363=LINE('',#100424,#21397);
#15364=LINE('',#100425,#21398);
#15365=LINE('',#100428,#21399);
#15366=LINE('',#100430,#21400);
#15367=LINE('',#100431,#21401);
#15368=LINE('',#100434,#21402);
#15369=LINE('',#100436,#21403);
#15370=LINE('',#100437,#21404);
#15371=LINE('',#100440,#21405);
#15372=LINE('',#100442,#21406);
#15373=LINE('',#100443,#21407);
#15374=LINE('',#100446,#21408);
#15375=LINE('',#100448,#21409);
#15376=LINE('',#100449,#21410);
#15377=LINE('',#100452,#21411);
#15378=LINE('',#100454,#21412);
#15379=LINE('',#100455,#21413);
#15380=LINE('',#100458,#21414);
#15381=LINE('',#100460,#21415);
#15382=LINE('',#100461,#21416);
#15383=LINE('',#100464,#21417);
#15384=LINE('',#100466,#21418);
#15385=LINE('',#100467,#21419);
#15386=LINE('',#100470,#21420);
#15387=LINE('',#100472,#21421);
#15388=LINE('',#100473,#21422);
#15389=LINE('',#100476,#21423);
#15390=LINE('',#100478,#21424);
#15391=LINE('',#100479,#21425);
#15392=LINE('',#100482,#21426);
#15393=LINE('',#100484,#21427);
#15394=LINE('',#100485,#21428);
#15395=LINE('',#100488,#21429);
#15396=LINE('',#100490,#21430);
#15397=LINE('',#100491,#21431);
#15398=LINE('',#100494,#21432);
#15399=LINE('',#100496,#21433);
#15400=LINE('',#100497,#21434);
#15401=LINE('',#100500,#21435);
#15402=LINE('',#100502,#21436);
#15403=LINE('',#100503,#21437);
#15404=LINE('',#100506,#21438);
#15405=LINE('',#100508,#21439);
#15406=LINE('',#100509,#21440);
#15407=LINE('',#100512,#21441);
#15408=LINE('',#100514,#21442);
#15409=LINE('',#100515,#21443);
#15410=LINE('',#100518,#21444);
#15411=LINE('',#100520,#21445);
#15412=LINE('',#100521,#21446);
#15413=LINE('',#100524,#21447);
#15414=LINE('',#100526,#21448);
#15415=LINE('',#100527,#21449);
#15416=LINE('',#100530,#21450);
#15417=LINE('',#100532,#21451);
#15418=LINE('',#100533,#21452);
#15419=LINE('',#100536,#21453);
#15420=LINE('',#100538,#21454);
#15421=LINE('',#100539,#21455);
#15422=LINE('',#100542,#21456);
#15423=LINE('',#100544,#21457);
#15424=LINE('',#100545,#21458);
#15425=LINE('',#100548,#21459);
#15426=LINE('',#100550,#21460);
#15427=LINE('',#100551,#21461);
#15428=LINE('',#100554,#21462);
#15429=LINE('',#100556,#21463);
#15430=LINE('',#100557,#21464);
#15431=LINE('',#100560,#21465);
#15432=LINE('',#100562,#21466);
#15433=LINE('',#100563,#21467);
#15434=LINE('',#100566,#21468);
#15435=LINE('',#100568,#21469);
#15436=LINE('',#100569,#21470);
#15437=LINE('',#100572,#21471);
#15438=LINE('',#100574,#21472);
#15439=LINE('',#100575,#21473);
#15440=LINE('',#100578,#21474);
#15441=LINE('',#100580,#21475);
#15442=LINE('',#100581,#21476);
#15443=LINE('',#100584,#21477);
#15444=LINE('',#100586,#21478);
#15445=LINE('',#100587,#21479);
#15446=LINE('',#100590,#21480);
#15447=LINE('',#100592,#21481);
#15448=LINE('',#100593,#21482);
#15449=LINE('',#100596,#21483);
#15450=LINE('',#100598,#21484);
#15451=LINE('',#100599,#21485);
#15452=LINE('',#100602,#21486);
#15453=LINE('',#100604,#21487);
#15454=LINE('',#100605,#21488);
#15455=LINE('',#100608,#21489);
#15456=LINE('',#100610,#21490);
#15457=LINE('',#100611,#21491);
#15458=LINE('',#100614,#21492);
#15459=LINE('',#100616,#21493);
#15460=LINE('',#100617,#21494);
#15461=LINE('',#100620,#21495);
#15462=LINE('',#100622,#21496);
#15463=LINE('',#100623,#21497);
#15464=LINE('',#100626,#21498);
#15465=LINE('',#100628,#21499);
#15466=LINE('',#100629,#21500);
#15467=LINE('',#100632,#21501);
#15468=LINE('',#100634,#21502);
#15469=LINE('',#100635,#21503);
#15470=LINE('',#100638,#21504);
#15471=LINE('',#100640,#21505);
#15472=LINE('',#100641,#21506);
#15473=LINE('',#100644,#21507);
#15474=LINE('',#100646,#21508);
#15475=LINE('',#100647,#21509);
#15476=LINE('',#100650,#21510);
#15477=LINE('',#100652,#21511);
#15478=LINE('',#100653,#21512);
#15479=LINE('',#100656,#21513);
#15480=LINE('',#100658,#21514);
#15481=LINE('',#100659,#21515);
#15482=LINE('',#100662,#21516);
#15483=LINE('',#100664,#21517);
#15484=LINE('',#100665,#21518);
#15485=LINE('',#100668,#21519);
#15486=LINE('',#100670,#21520);
#15487=LINE('',#100671,#21521);
#15488=LINE('',#100674,#21522);
#15489=LINE('',#100676,#21523);
#15490=LINE('',#100677,#21524);
#15491=LINE('',#100680,#21525);
#15492=LINE('',#100682,#21526);
#15493=LINE('',#100683,#21527);
#15494=LINE('',#100686,#21528);
#15495=LINE('',#100688,#21529);
#15496=LINE('',#100689,#21530);
#15497=LINE('',#100692,#21531);
#15498=LINE('',#100694,#21532);
#15499=LINE('',#100695,#21533);
#15500=LINE('',#100698,#21534);
#15501=LINE('',#100700,#21535);
#15502=LINE('',#100701,#21536);
#15503=LINE('',#100704,#21537);
#15504=LINE('',#100706,#21538);
#15505=LINE('',#100707,#21539);
#15506=LINE('',#100710,#21540);
#15507=LINE('',#100712,#21541);
#15508=LINE('',#100713,#21542);
#15509=LINE('',#100716,#21543);
#15510=LINE('',#100718,#21544);
#15511=LINE('',#100719,#21545);
#15512=LINE('',#100722,#21546);
#15513=LINE('',#100724,#21547);
#15514=LINE('',#100725,#21548);
#15515=LINE('',#100728,#21549);
#15516=LINE('',#100730,#21550);
#15517=LINE('',#100731,#21551);
#15518=LINE('',#100734,#21552);
#15519=LINE('',#100736,#21553);
#15520=LINE('',#100737,#21554);
#15521=LINE('',#100740,#21555);
#15522=LINE('',#100742,#21556);
#15523=LINE('',#100743,#21557);
#15524=LINE('',#100746,#21558);
#15525=LINE('',#100748,#21559);
#15526=LINE('',#100749,#21560);
#15527=LINE('',#100752,#21561);
#15528=LINE('',#100754,#21562);
#15529=LINE('',#100755,#21563);
#15530=LINE('',#100758,#21564);
#15531=LINE('',#100760,#21565);
#15532=LINE('',#100761,#21566);
#15533=LINE('',#100764,#21567);
#15534=LINE('',#100766,#21568);
#15535=LINE('',#100767,#21569);
#15536=LINE('',#100770,#21570);
#15537=LINE('',#100772,#21571);
#15538=LINE('',#100773,#21572);
#15539=LINE('',#100776,#21573);
#15540=LINE('',#100778,#21574);
#15541=LINE('',#100779,#21575);
#15542=LINE('',#100782,#21576);
#15543=LINE('',#100784,#21577);
#15544=LINE('',#100785,#21578);
#15545=LINE('',#100788,#21579);
#15546=LINE('',#100790,#21580);
#15547=LINE('',#100791,#21581);
#15548=LINE('',#100794,#21582);
#15549=LINE('',#100796,#21583);
#15550=LINE('',#100797,#21584);
#15551=LINE('',#100800,#21585);
#15552=LINE('',#100802,#21586);
#15553=LINE('',#100803,#21587);
#15554=LINE('',#100806,#21588);
#15555=LINE('',#100808,#21589);
#15556=LINE('',#100809,#21590);
#15557=LINE('',#100812,#21591);
#15558=LINE('',#100814,#21592);
#15559=LINE('',#100815,#21593);
#15560=LINE('',#100818,#21594);
#15561=LINE('',#100820,#21595);
#15562=LINE('',#100821,#21596);
#15563=LINE('',#100824,#21597);
#15564=LINE('',#100826,#21598);
#15565=LINE('',#100827,#21599);
#15566=LINE('',#100830,#21600);
#15567=LINE('',#100832,#21601);
#15568=LINE('',#100833,#21602);
#15569=LINE('',#100836,#21603);
#15570=LINE('',#100838,#21604);
#15571=LINE('',#100839,#21605);
#15572=LINE('',#100842,#21606);
#15573=LINE('',#100844,#21607);
#15574=LINE('',#100845,#21608);
#15575=LINE('',#100848,#21609);
#15576=LINE('',#100850,#21610);
#15577=LINE('',#100851,#21611);
#15578=LINE('',#100854,#21612);
#15579=LINE('',#100856,#21613);
#15580=LINE('',#100857,#21614);
#15581=LINE('',#100860,#21615);
#15582=LINE('',#100862,#21616);
#15583=LINE('',#100863,#21617);
#15584=LINE('',#100866,#21618);
#15585=LINE('',#100868,#21619);
#15586=LINE('',#100869,#21620);
#15587=LINE('',#100872,#21621);
#15588=LINE('',#100874,#21622);
#15589=LINE('',#100875,#21623);
#15590=LINE('',#100878,#21624);
#15591=LINE('',#100880,#21625);
#15592=LINE('',#100881,#21626);
#15593=LINE('',#100884,#21627);
#15594=LINE('',#100886,#21628);
#15595=LINE('',#100887,#21629);
#15596=LINE('',#100890,#21630);
#15597=LINE('',#100892,#21631);
#15598=LINE('',#100893,#21632);
#15599=LINE('',#100896,#21633);
#15600=LINE('',#100898,#21634);
#15601=LINE('',#100899,#21635);
#15602=LINE('',#100902,#21636);
#15603=LINE('',#100904,#21637);
#15604=LINE('',#100905,#21638);
#15605=LINE('',#100908,#21639);
#15606=LINE('',#100910,#21640);
#15607=LINE('',#100911,#21641);
#15608=LINE('',#100914,#21642);
#15609=LINE('',#100916,#21643);
#15610=LINE('',#100917,#21644);
#15611=LINE('',#100920,#21645);
#15612=LINE('',#100922,#21646);
#15613=LINE('',#100923,#21647);
#15614=LINE('',#100926,#21648);
#15615=LINE('',#100928,#21649);
#15616=LINE('',#100929,#21650);
#15617=LINE('',#100932,#21651);
#15618=LINE('',#100934,#21652);
#15619=LINE('',#100935,#21653);
#15620=LINE('',#100938,#21654);
#15621=LINE('',#100940,#21655);
#15622=LINE('',#100941,#21656);
#15623=LINE('',#100944,#21657);
#15624=LINE('',#100946,#21658);
#15625=LINE('',#100947,#21659);
#15626=LINE('',#100950,#21660);
#15627=LINE('',#100952,#21661);
#15628=LINE('',#100953,#21662);
#15629=LINE('',#100956,#21663);
#15630=LINE('',#100958,#21664);
#15631=LINE('',#100959,#21665);
#15632=LINE('',#100962,#21666);
#15633=LINE('',#100964,#21667);
#15634=LINE('',#100965,#21668);
#15635=LINE('',#100968,#21669);
#15636=LINE('',#100970,#21670);
#15637=LINE('',#100971,#21671);
#15638=LINE('',#100974,#21672);
#15639=LINE('',#100976,#21673);
#15640=LINE('',#100977,#21674);
#15641=LINE('',#100980,#21675);
#15642=LINE('',#100982,#21676);
#15643=LINE('',#100983,#21677);
#15644=LINE('',#100986,#21678);
#15645=LINE('',#100988,#21679);
#15646=LINE('',#100989,#21680);
#15647=LINE('',#100992,#21681);
#15648=LINE('',#100994,#21682);
#15649=LINE('',#100995,#21683);
#15650=LINE('',#100998,#21684);
#15651=LINE('',#101000,#21685);
#15652=LINE('',#101001,#21686);
#15653=LINE('',#101004,#21687);
#15654=LINE('',#101006,#21688);
#15655=LINE('',#101007,#21689);
#15656=LINE('',#101010,#21690);
#15657=LINE('',#101012,#21691);
#15658=LINE('',#101013,#21692);
#15659=LINE('',#101016,#21693);
#15660=LINE('',#101018,#21694);
#15661=LINE('',#101019,#21695);
#15662=LINE('',#101022,#21696);
#15663=LINE('',#101024,#21697);
#15664=LINE('',#101025,#21698);
#15665=LINE('',#101028,#21699);
#15666=LINE('',#101030,#21700);
#15667=LINE('',#101031,#21701);
#15668=LINE('',#101034,#21702);
#15669=LINE('',#101036,#21703);
#15670=LINE('',#101037,#21704);
#15671=LINE('',#101040,#21705);
#15672=LINE('',#101042,#21706);
#15673=LINE('',#101043,#21707);
#15674=LINE('',#101046,#21708);
#15675=LINE('',#101048,#21709);
#15676=LINE('',#101049,#21710);
#15677=LINE('',#101052,#21711);
#15678=LINE('',#101054,#21712);
#15679=LINE('',#101055,#21713);
#15680=LINE('',#101058,#21714);
#15681=LINE('',#101060,#21715);
#15682=LINE('',#101061,#21716);
#15683=LINE('',#101064,#21717);
#15684=LINE('',#101066,#21718);
#15685=LINE('',#101067,#21719);
#15686=LINE('',#101070,#21720);
#15687=LINE('',#101072,#21721);
#15688=LINE('',#101073,#21722);
#15689=LINE('',#101076,#21723);
#15690=LINE('',#101078,#21724);
#15691=LINE('',#101079,#21725);
#15692=LINE('',#101082,#21726);
#15693=LINE('',#101084,#21727);
#15694=LINE('',#101085,#21728);
#15695=LINE('',#101088,#21729);
#15696=LINE('',#101090,#21730);
#15697=LINE('',#101091,#21731);
#15698=LINE('',#101094,#21732);
#15699=LINE('',#101096,#21733);
#15700=LINE('',#101097,#21734);
#15701=LINE('',#101100,#21735);
#15702=LINE('',#101102,#21736);
#15703=LINE('',#101103,#21737);
#15704=LINE('',#101106,#21738);
#15705=LINE('',#101108,#21739);
#15706=LINE('',#101109,#21740);
#15707=LINE('',#101112,#21741);
#15708=LINE('',#101114,#21742);
#15709=LINE('',#101115,#21743);
#15710=LINE('',#101118,#21744);
#15711=LINE('',#101120,#21745);
#15712=LINE('',#101121,#21746);
#15713=LINE('',#101124,#21747);
#15714=LINE('',#101126,#21748);
#15715=LINE('',#101127,#21749);
#15716=LINE('',#101130,#21750);
#15717=LINE('',#101132,#21751);
#15718=LINE('',#101133,#21752);
#15719=LINE('',#101136,#21753);
#15720=LINE('',#101138,#21754);
#15721=LINE('',#101139,#21755);
#15722=LINE('',#101142,#21756);
#15723=LINE('',#101144,#21757);
#15724=LINE('',#101145,#21758);
#15725=LINE('',#101148,#21759);
#15726=LINE('',#101150,#21760);
#15727=LINE('',#101151,#21761);
#15728=LINE('',#101154,#21762);
#15729=LINE('',#101156,#21763);
#15730=LINE('',#101157,#21764);
#15731=LINE('',#101160,#21765);
#15732=LINE('',#101162,#21766);
#15733=LINE('',#101163,#21767);
#15734=LINE('',#101166,#21768);
#15735=LINE('',#101168,#21769);
#15736=LINE('',#101169,#21770);
#15737=LINE('',#101172,#21771);
#15738=LINE('',#101174,#21772);
#15739=LINE('',#101175,#21773);
#15740=LINE('',#101178,#21774);
#15741=LINE('',#101180,#21775);
#15742=LINE('',#101181,#21776);
#15743=LINE('',#101184,#21777);
#15744=LINE('',#101186,#21778);
#15745=LINE('',#101187,#21779);
#15746=LINE('',#101190,#21780);
#15747=LINE('',#101192,#21781);
#15748=LINE('',#101193,#21782);
#15749=LINE('',#101196,#21783);
#15750=LINE('',#101198,#21784);
#15751=LINE('',#101199,#21785);
#15752=LINE('',#101202,#21786);
#15753=LINE('',#101204,#21787);
#15754=LINE('',#101205,#21788);
#15755=LINE('',#101208,#21789);
#15756=LINE('',#101210,#21790);
#15757=LINE('',#101211,#21791);
#15758=LINE('',#101214,#21792);
#15759=LINE('',#101216,#21793);
#15760=LINE('',#101217,#21794);
#15761=LINE('',#101220,#21795);
#15762=LINE('',#101222,#21796);
#15763=LINE('',#101223,#21797);
#15764=LINE('',#101226,#21798);
#15765=LINE('',#101228,#21799);
#15766=LINE('',#101229,#21800);
#15767=LINE('',#101232,#21801);
#15768=LINE('',#101234,#21802);
#15769=LINE('',#101235,#21803);
#15770=LINE('',#101238,#21804);
#15771=LINE('',#101240,#21805);
#15772=LINE('',#101241,#21806);
#15773=LINE('',#101244,#21807);
#15774=LINE('',#101246,#21808);
#15775=LINE('',#101247,#21809);
#15776=LINE('',#101250,#21810);
#15777=LINE('',#101252,#21811);
#15778=LINE('',#101253,#21812);
#15779=LINE('',#101256,#21813);
#15780=LINE('',#101258,#21814);
#15781=LINE('',#101259,#21815);
#15782=LINE('',#101262,#21816);
#15783=LINE('',#101264,#21817);
#15784=LINE('',#101265,#21818);
#15785=LINE('',#101268,#21819);
#15786=LINE('',#101270,#21820);
#15787=LINE('',#101271,#21821);
#15788=LINE('',#101274,#21822);
#15789=LINE('',#101276,#21823);
#15790=LINE('',#101277,#21824);
#15791=LINE('',#101280,#21825);
#15792=LINE('',#101282,#21826);
#15793=LINE('',#101283,#21827);
#15794=LINE('',#101286,#21828);
#15795=LINE('',#101288,#21829);
#15796=LINE('',#101289,#21830);
#15797=LINE('',#101292,#21831);
#15798=LINE('',#101294,#21832);
#15799=LINE('',#101295,#21833);
#15800=LINE('',#101298,#21834);
#15801=LINE('',#101300,#21835);
#15802=LINE('',#101301,#21836);
#15803=LINE('',#101304,#21837);
#15804=LINE('',#101306,#21838);
#15805=LINE('',#101307,#21839);
#15806=LINE('',#101310,#21840);
#15807=LINE('',#101312,#21841);
#15808=LINE('',#101313,#21842);
#15809=LINE('',#101316,#21843);
#15810=LINE('',#101318,#21844);
#15811=LINE('',#101319,#21845);
#15812=LINE('',#101322,#21846);
#15813=LINE('',#101324,#21847);
#15814=LINE('',#101325,#21848);
#15815=LINE('',#101328,#21849);
#15816=LINE('',#101330,#21850);
#15817=LINE('',#101331,#21851);
#15818=LINE('',#101334,#21852);
#15819=LINE('',#101336,#21853);
#15820=LINE('',#101337,#21854);
#15821=LINE('',#101340,#21855);
#15822=LINE('',#101342,#21856);
#15823=LINE('',#101343,#21857);
#15824=LINE('',#101346,#21858);
#15825=LINE('',#101348,#21859);
#15826=LINE('',#101349,#21860);
#15827=LINE('',#101352,#21861);
#15828=LINE('',#101354,#21862);
#15829=LINE('',#101355,#21863);
#15830=LINE('',#101358,#21864);
#15831=LINE('',#101360,#21865);
#15832=LINE('',#101361,#21866);
#15833=LINE('',#101364,#21867);
#15834=LINE('',#101366,#21868);
#15835=LINE('',#101367,#21869);
#15836=LINE('',#101370,#21870);
#15837=LINE('',#101372,#21871);
#15838=LINE('',#101373,#21872);
#15839=LINE('',#101376,#21873);
#15840=LINE('',#101378,#21874);
#15841=LINE('',#101379,#21875);
#15842=LINE('',#101382,#21876);
#15843=LINE('',#101384,#21877);
#15844=LINE('',#101385,#21878);
#15845=LINE('',#101388,#21879);
#15846=LINE('',#101390,#21880);
#15847=LINE('',#101391,#21881);
#15848=LINE('',#101394,#21882);
#15849=LINE('',#101396,#21883);
#15850=LINE('',#101397,#21884);
#15851=LINE('',#101400,#21885);
#15852=LINE('',#101402,#21886);
#15853=LINE('',#101403,#21887);
#15854=LINE('',#101406,#21888);
#15855=LINE('',#101408,#21889);
#15856=LINE('',#101409,#21890);
#15857=LINE('',#101412,#21891);
#15858=LINE('',#101414,#21892);
#15859=LINE('',#101415,#21893);
#15860=LINE('',#101418,#21894);
#15861=LINE('',#101420,#21895);
#15862=LINE('',#101421,#21896);
#15863=LINE('',#101424,#21897);
#15864=LINE('',#101426,#21898);
#15865=LINE('',#101427,#21899);
#15866=LINE('',#101430,#21900);
#15867=LINE('',#101432,#21901);
#15868=LINE('',#101433,#21902);
#15869=LINE('',#101436,#21903);
#15870=LINE('',#101438,#21904);
#15871=LINE('',#101439,#21905);
#15872=LINE('',#101442,#21906);
#15873=LINE('',#101444,#21907);
#15874=LINE('',#101445,#21908);
#15875=LINE('',#101448,#21909);
#15876=LINE('',#101450,#21910);
#15877=LINE('',#101451,#21911);
#15878=LINE('',#101454,#21912);
#15879=LINE('',#101456,#21913);
#15880=LINE('',#101457,#21914);
#15881=LINE('',#101460,#21915);
#15882=LINE('',#101462,#21916);
#15883=LINE('',#101463,#21917);
#15884=LINE('',#101466,#21918);
#15885=LINE('',#101468,#21919);
#15886=LINE('',#101469,#21920);
#15887=LINE('',#101472,#21921);
#15888=LINE('',#101474,#21922);
#15889=LINE('',#101475,#21923);
#15890=LINE('',#101478,#21924);
#15891=LINE('',#101480,#21925);
#15892=LINE('',#101481,#21926);
#15893=LINE('',#101484,#21927);
#15894=LINE('',#101486,#21928);
#15895=LINE('',#101487,#21929);
#15896=LINE('',#101490,#21930);
#15897=LINE('',#101492,#21931);
#15898=LINE('',#101493,#21932);
#15899=LINE('',#101496,#21933);
#15900=LINE('',#101498,#21934);
#15901=LINE('',#101499,#21935);
#15902=LINE('',#101502,#21936);
#15903=LINE('',#101504,#21937);
#15904=LINE('',#101505,#21938);
#15905=LINE('',#101508,#21939);
#15906=LINE('',#101510,#21940);
#15907=LINE('',#101511,#21941);
#15908=LINE('',#101514,#21942);
#15909=LINE('',#101516,#21943);
#15910=LINE('',#101517,#21944);
#15911=LINE('',#101520,#21945);
#15912=LINE('',#101522,#21946);
#15913=LINE('',#101523,#21947);
#15914=LINE('',#101526,#21948);
#15915=LINE('',#101528,#21949);
#15916=LINE('',#101529,#21950);
#15917=LINE('',#101532,#21951);
#15918=LINE('',#101534,#21952);
#15919=LINE('',#101535,#21953);
#15920=LINE('',#101538,#21954);
#15921=LINE('',#101540,#21955);
#15922=LINE('',#101541,#21956);
#15923=LINE('',#101544,#21957);
#15924=LINE('',#101546,#21958);
#15925=LINE('',#101547,#21959);
#15926=LINE('',#101550,#21960);
#15927=LINE('',#101552,#21961);
#15928=LINE('',#101553,#21962);
#15929=LINE('',#101556,#21963);
#15930=LINE('',#101558,#21964);
#15931=LINE('',#101559,#21965);
#15932=LINE('',#101562,#21966);
#15933=LINE('',#101564,#21967);
#15934=LINE('',#101565,#21968);
#15935=LINE('',#101568,#21969);
#15936=LINE('',#101570,#21970);
#15937=LINE('',#101571,#21971);
#15938=LINE('',#101574,#21972);
#15939=LINE('',#101576,#21973);
#15940=LINE('',#101577,#21974);
#15941=LINE('',#101580,#21975);
#15942=LINE('',#101582,#21976);
#15943=LINE('',#101583,#21977);
#15944=LINE('',#101586,#21978);
#15945=LINE('',#101588,#21979);
#15946=LINE('',#101589,#21980);
#15947=LINE('',#101592,#21981);
#15948=LINE('',#101594,#21982);
#15949=LINE('',#101595,#21983);
#15950=LINE('',#101598,#21984);
#15951=LINE('',#101600,#21985);
#15952=LINE('',#101601,#21986);
#15953=LINE('',#101604,#21987);
#15954=LINE('',#101606,#21988);
#15955=LINE('',#101607,#21989);
#15956=LINE('',#101610,#21990);
#15957=LINE('',#101612,#21991);
#15958=LINE('',#101613,#21992);
#15959=LINE('',#101616,#21993);
#15960=LINE('',#101618,#21994);
#15961=LINE('',#101619,#21995);
#15962=LINE('',#101622,#21996);
#15963=LINE('',#101624,#21997);
#15964=LINE('',#101625,#21998);
#15965=LINE('',#101628,#21999);
#15966=LINE('',#101630,#22000);
#15967=LINE('',#101631,#22001);
#15968=LINE('',#101634,#22002);
#15969=LINE('',#101636,#22003);
#15970=LINE('',#101637,#22004);
#15971=LINE('',#101640,#22005);
#15972=LINE('',#101642,#22006);
#15973=LINE('',#101643,#22007);
#15974=LINE('',#101646,#22008);
#15975=LINE('',#101648,#22009);
#15976=LINE('',#101649,#22010);
#15977=LINE('',#101652,#22011);
#15978=LINE('',#101654,#22012);
#15979=LINE('',#101655,#22013);
#15980=LINE('',#101658,#22014);
#15981=LINE('',#101660,#22015);
#15982=LINE('',#101661,#22016);
#15983=LINE('',#101664,#22017);
#15984=LINE('',#101666,#22018);
#15985=LINE('',#101667,#22019);
#15986=LINE('',#101670,#22020);
#15987=LINE('',#101672,#22021);
#15988=LINE('',#101673,#22022);
#15989=LINE('',#101676,#22023);
#15990=LINE('',#101678,#22024);
#15991=LINE('',#101679,#22025);
#15992=LINE('',#101682,#22026);
#15993=LINE('',#101684,#22027);
#15994=LINE('',#101685,#22028);
#15995=LINE('',#101688,#22029);
#15996=LINE('',#101690,#22030);
#15997=LINE('',#101691,#22031);
#15998=LINE('',#101694,#22032);
#15999=LINE('',#101696,#22033);
#16000=LINE('',#101697,#22034);
#16001=LINE('',#101700,#22035);
#16002=LINE('',#101702,#22036);
#16003=LINE('',#101703,#22037);
#16004=LINE('',#101706,#22038);
#16005=LINE('',#101708,#22039);
#16006=LINE('',#101709,#22040);
#16007=LINE('',#101712,#22041);
#16008=LINE('',#101714,#22042);
#16009=LINE('',#101715,#22043);
#16010=LINE('',#101718,#22044);
#16011=LINE('',#101720,#22045);
#16012=LINE('',#101721,#22046);
#16013=LINE('',#101724,#22047);
#16014=LINE('',#101726,#22048);
#16015=LINE('',#101727,#22049);
#16016=LINE('',#101730,#22050);
#16017=LINE('',#101732,#22051);
#16018=LINE('',#101733,#22052);
#16019=LINE('',#101736,#22053);
#16020=LINE('',#101738,#22054);
#16021=LINE('',#101739,#22055);
#16022=LINE('',#101742,#22056);
#16023=LINE('',#101744,#22057);
#16024=LINE('',#101745,#22058);
#16025=LINE('',#101748,#22059);
#16026=LINE('',#101750,#22060);
#16027=LINE('',#101751,#22061);
#16028=LINE('',#101754,#22062);
#16029=LINE('',#101756,#22063);
#16030=LINE('',#101757,#22064);
#16031=LINE('',#101760,#22065);
#16032=LINE('',#101762,#22066);
#16033=LINE('',#101763,#22067);
#16034=LINE('',#101766,#22068);
#16035=LINE('',#101768,#22069);
#16036=LINE('',#101769,#22070);
#16037=LINE('',#101772,#22071);
#16038=LINE('',#101774,#22072);
#16039=LINE('',#101775,#22073);
#16040=LINE('',#101778,#22074);
#16041=LINE('',#101780,#22075);
#16042=LINE('',#101781,#22076);
#16043=LINE('',#101784,#22077);
#16044=LINE('',#101786,#22078);
#16045=LINE('',#101787,#22079);
#16046=LINE('',#101790,#22080);
#16047=LINE('',#101792,#22081);
#16048=LINE('',#101793,#22082);
#16049=LINE('',#101796,#22083);
#16050=LINE('',#101798,#22084);
#16051=LINE('',#101799,#22085);
#16052=LINE('',#101802,#22086);
#16053=LINE('',#101804,#22087);
#16054=LINE('',#101805,#22088);
#16055=LINE('',#101808,#22089);
#16056=LINE('',#101810,#22090);
#16057=LINE('',#101811,#22091);
#16058=LINE('',#101814,#22092);
#16059=LINE('',#101816,#22093);
#16060=LINE('',#101817,#22094);
#16061=LINE('',#101820,#22095);
#16062=LINE('',#101822,#22096);
#16063=LINE('',#101823,#22097);
#16064=LINE('',#101826,#22098);
#16065=LINE('',#101828,#22099);
#16066=LINE('',#101829,#22100);
#16067=LINE('',#101832,#22101);
#16068=LINE('',#101834,#22102);
#16069=LINE('',#101835,#22103);
#16070=LINE('',#101838,#22104);
#16071=LINE('',#101840,#22105);
#16072=LINE('',#101841,#22106);
#16073=LINE('',#101844,#22107);
#16074=LINE('',#101846,#22108);
#16075=LINE('',#101847,#22109);
#16076=LINE('',#101850,#22110);
#16077=LINE('',#101852,#22111);
#16078=LINE('',#101853,#22112);
#16079=LINE('',#101856,#22113);
#16080=LINE('',#101858,#22114);
#16081=LINE('',#101859,#22115);
#16082=LINE('',#101862,#22116);
#16083=LINE('',#101864,#22117);
#16084=LINE('',#101865,#22118);
#16085=LINE('',#101868,#22119);
#16086=LINE('',#101870,#22120);
#16087=LINE('',#101871,#22121);
#16088=LINE('',#101874,#22122);
#16089=LINE('',#101876,#22123);
#16090=LINE('',#101877,#22124);
#16091=LINE('',#101880,#22125);
#16092=LINE('',#101882,#22126);
#16093=LINE('',#101883,#22127);
#16094=LINE('',#101886,#22128);
#16095=LINE('',#101888,#22129);
#16096=LINE('',#101889,#22130);
#16097=LINE('',#101892,#22131);
#16098=LINE('',#101894,#22132);
#16099=LINE('',#101895,#22133);
#16100=LINE('',#101898,#22134);
#16101=LINE('',#101900,#22135);
#16102=LINE('',#101901,#22136);
#16103=LINE('',#101904,#22137);
#16104=LINE('',#101906,#22138);
#16105=LINE('',#101907,#22139);
#16106=LINE('',#101910,#22140);
#16107=LINE('',#101912,#22141);
#16108=LINE('',#101913,#22142);
#16109=LINE('',#101916,#22143);
#16110=LINE('',#101918,#22144);
#16111=LINE('',#101919,#22145);
#16112=LINE('',#101922,#22146);
#16113=LINE('',#101924,#22147);
#16114=LINE('',#101925,#22148);
#16115=LINE('',#101928,#22149);
#16116=LINE('',#101930,#22150);
#16117=LINE('',#101931,#22151);
#16118=LINE('',#101934,#22152);
#16119=LINE('',#101936,#22153);
#16120=LINE('',#101937,#22154);
#16121=LINE('',#101940,#22155);
#16122=LINE('',#101942,#22156);
#16123=LINE('',#101943,#22157);
#16124=LINE('',#101946,#22158);
#16125=LINE('',#101948,#22159);
#16126=LINE('',#101949,#22160);
#16127=LINE('',#101952,#22161);
#16128=LINE('',#101954,#22162);
#16129=LINE('',#101955,#22163);
#16130=LINE('',#101958,#22164);
#16131=LINE('',#101960,#22165);
#16132=LINE('',#101961,#22166);
#16133=LINE('',#101964,#22167);
#16134=LINE('',#101966,#22168);
#16135=LINE('',#101967,#22169);
#16136=LINE('',#101970,#22170);
#16137=LINE('',#101972,#22171);
#16138=LINE('',#101973,#22172);
#16139=LINE('',#101976,#22173);
#16140=LINE('',#101978,#22174);
#16141=LINE('',#101979,#22175);
#16142=LINE('',#101982,#22176);
#16143=LINE('',#101984,#22177);
#16144=LINE('',#101985,#22178);
#16145=LINE('',#101988,#22179);
#16146=LINE('',#101990,#22180);
#16147=LINE('',#101991,#22181);
#16148=LINE('',#101994,#22182);
#16149=LINE('',#101996,#22183);
#16150=LINE('',#101997,#22184);
#16151=LINE('',#102000,#22185);
#16152=LINE('',#102002,#22186);
#16153=LINE('',#102003,#22187);
#16154=LINE('',#102006,#22188);
#16155=LINE('',#102008,#22189);
#16156=LINE('',#102009,#22190);
#16157=LINE('',#102011,#22191);
#16158=LINE('',#102012,#22192);
#16159=LINE('',#102014,#22193);
#16160=LINE('',#102015,#22194);
#16161=LINE('',#102024,#22195);
#16162=LINE('',#102027,#22196);
#16163=LINE('',#102032,#22197);
#16164=LINE('',#102038,#22198);
#16165=LINE('',#102042,#22199);
#16166=LINE('',#102044,#22200);
#16167=LINE('',#102046,#22201);
#16168=LINE('',#102048,#22202);
#16169=LINE('',#102049,#22203);
#16170=LINE('',#102055,#22204);
#16171=LINE('',#102058,#22205);
#16172=LINE('',#102060,#22206);
#16173=LINE('',#102061,#22207);
#16174=LINE('',#102064,#22208);
#16175=LINE('',#102066,#22209);
#16176=LINE('',#102068,#22210);
#16177=LINE('',#102070,#22211);
#16178=LINE('',#102072,#22212);
#16179=LINE('',#102073,#22213);
#16180=LINE('',#102079,#22214);
#16181=LINE('',#102082,#22215);
#16182=LINE('',#102084,#22216);
#16183=LINE('',#102086,#22217);
#16184=LINE('',#102092,#22218);
#16185=LINE('',#102095,#22219);
#16186=LINE('',#102097,#22220);
#16187=LINE('',#102099,#22221);
#16188=LINE('',#102100,#22222);
#16189=LINE('',#102103,#22223);
#16190=LINE('',#102104,#22224);
#16191=LINE('',#102107,#22225);
#16192=LINE('',#102109,#22226);
#16193=LINE('',#102110,#22227);
#16194=LINE('',#102112,#22228);
#16195=LINE('',#102113,#22229);
#16196=LINE('',#102118,#22230);
#16197=LINE('',#102121,#22231);
#16198=LINE('',#102127,#22232);
#16199=LINE('',#102129,#22233);
#16200=LINE('',#102131,#22234);
#16201=LINE('',#102132,#22235);
#16202=LINE('',#102135,#22236);
#16203=LINE('',#102137,#22237);
#16204=LINE('',#102138,#22238);
#16205=LINE('',#102141,#22239);
#16206=LINE('',#102142,#22240);
#16207=LINE('',#102145,#22241);
#16208=LINE('',#102146,#22242);
#16209=LINE('',#102150,#22243);
#16210=LINE('',#102152,#22244);
#16211=LINE('',#102154,#22245);
#16212=LINE('',#102155,#22246);
#16213=LINE('',#102158,#22247);
#16214=LINE('',#102160,#22248);
#16215=LINE('',#102161,#22249);
#16216=LINE('',#102164,#22250);
#16217=LINE('',#102165,#22251);
#16218=LINE('',#102168,#22252);
#16219=LINE('',#102169,#22253);
#16220=LINE('',#102173,#22254);
#16221=LINE('',#102175,#22255);
#16222=LINE('',#102177,#22256);
#16223=LINE('',#102178,#22257);
#16224=LINE('',#102181,#22258);
#16225=LINE('',#102183,#22259);
#16226=LINE('',#102184,#22260);
#16227=LINE('',#102187,#22261);
#16228=LINE('',#102188,#22262);
#16229=LINE('',#102191,#22263);
#16230=LINE('',#102192,#22264);
#16231=LINE('',#102196,#22265);
#16232=LINE('',#102198,#22266);
#16233=LINE('',#102200,#22267);
#16234=LINE('',#102201,#22268);
#16235=LINE('',#102204,#22269);
#16236=LINE('',#102206,#22270);
#16237=LINE('',#102207,#22271);
#16238=LINE('',#102210,#22272);
#16239=LINE('',#102211,#22273);
#16240=LINE('',#102214,#22274);
#16241=LINE('',#102215,#22275);
#16242=LINE('',#102219,#22276);
#16243=LINE('',#102221,#22277);
#16244=LINE('',#102223,#22278);
#16245=LINE('',#102224,#22279);
#16246=LINE('',#102227,#22280);
#16247=LINE('',#102229,#22281);
#16248=LINE('',#102230,#22282);
#16249=LINE('',#102233,#22283);
#16250=LINE('',#102234,#22284);
#16251=LINE('',#102237,#22285);
#16252=LINE('',#102238,#22286);
#16253=LINE('',#102242,#22287);
#16254=LINE('',#102244,#22288);
#16255=LINE('',#102246,#22289);
#16256=LINE('',#102247,#22290);
#16257=LINE('',#102250,#22291);
#16258=LINE('',#102252,#22292);
#16259=LINE('',#102253,#22293);
#16260=LINE('',#102256,#22294);
#16261=LINE('',#102257,#22295);
#16262=LINE('',#102260,#22296);
#16263=LINE('',#102261,#22297);
#16264=LINE('',#102265,#22298);
#16265=LINE('',#102267,#22299);
#16266=LINE('',#102269,#22300);
#16267=LINE('',#102270,#22301);
#16268=LINE('',#102273,#22302);
#16269=LINE('',#102275,#22303);
#16270=LINE('',#102276,#22304);
#16271=LINE('',#102279,#22305);
#16272=LINE('',#102280,#22306);
#16273=LINE('',#102283,#22307);
#16274=LINE('',#102284,#22308);
#16275=LINE('',#102288,#22309);
#16276=LINE('',#102290,#22310);
#16277=LINE('',#102292,#22311);
#16278=LINE('',#102293,#22312);
#16279=LINE('',#102296,#22313);
#16280=LINE('',#102298,#22314);
#16281=LINE('',#102299,#22315);
#16282=LINE('',#102302,#22316);
#16283=LINE('',#102303,#22317);
#16284=LINE('',#102306,#22318);
#16285=LINE('',#102307,#22319);
#16286=LINE('',#102315,#22320);
#16287=LINE('',#102317,#22321);
#16288=LINE('',#102318,#22322);
#16289=LINE('',#102326,#22323);
#16290=LINE('',#102328,#22324);
#16291=LINE('',#102329,#22325);
#16292=LINE('',#102332,#22326);
#16293=LINE('',#102336,#22327);
#16294=LINE('',#102338,#22328);
#16295=LINE('',#102340,#22329);
#16296=LINE('',#102341,#22330);
#16297=LINE('',#102344,#22331);
#16298=LINE('',#102346,#22332);
#16299=LINE('',#102347,#22333);
#16300=LINE('',#102350,#22334);
#16301=LINE('',#102351,#22335);
#16302=LINE('',#102354,#22336);
#16303=LINE('',#102355,#22337);
#16304=LINE('',#102359,#22338);
#16305=LINE('',#102361,#22339);
#16306=LINE('',#102363,#22340);
#16307=LINE('',#102364,#22341);
#16308=LINE('',#102367,#22342);
#16309=LINE('',#102369,#22343);
#16310=LINE('',#102370,#22344);
#16311=LINE('',#102373,#22345);
#16312=LINE('',#102374,#22346);
#16313=LINE('',#102377,#22347);
#16314=LINE('',#102378,#22348);
#16315=LINE('',#102382,#22349);
#16316=LINE('',#102384,#22350);
#16317=LINE('',#102386,#22351);
#16318=LINE('',#102387,#22352);
#16319=LINE('',#102390,#22353);
#16320=LINE('',#102392,#22354);
#16321=LINE('',#102393,#22355);
#16322=LINE('',#102396,#22356);
#16323=LINE('',#102397,#22357);
#16324=LINE('',#102400,#22358);
#16325=LINE('',#102401,#22359);
#16326=LINE('',#102405,#22360);
#16327=LINE('',#102407,#22361);
#16328=LINE('',#102409,#22362);
#16329=LINE('',#102410,#22363);
#16330=LINE('',#102413,#22364);
#16331=LINE('',#102415,#22365);
#16332=LINE('',#102416,#22366);
#16333=LINE('',#102419,#22367);
#16334=LINE('',#102420,#22368);
#16335=LINE('',#102423,#22369);
#16336=LINE('',#102424,#22370);
#16337=LINE('',#102428,#22371);
#16338=LINE('',#102430,#22372);
#16339=LINE('',#102432,#22373);
#16340=LINE('',#102433,#22374);
#16341=LINE('',#102436,#22375);
#16342=LINE('',#102438,#22376);
#16343=LINE('',#102439,#22377);
#16344=LINE('',#102442,#22378);
#16345=LINE('',#102443,#22379);
#16346=LINE('',#102446,#22380);
#16347=LINE('',#102447,#22381);
#16348=LINE('',#102451,#22382);
#16349=LINE('',#102453,#22383);
#16350=LINE('',#102455,#22384);
#16351=LINE('',#102456,#22385);
#16352=LINE('',#102459,#22386);
#16353=LINE('',#102461,#22387);
#16354=LINE('',#102462,#22388);
#16355=LINE('',#102465,#22389);
#16356=LINE('',#102466,#22390);
#16357=LINE('',#102469,#22391);
#16358=LINE('',#102470,#22392);
#16359=LINE('',#102474,#22393);
#16360=LINE('',#102476,#22394);
#16361=LINE('',#102478,#22395);
#16362=LINE('',#102479,#22396);
#16363=LINE('',#102482,#22397);
#16364=LINE('',#102484,#22398);
#16365=LINE('',#102485,#22399);
#16366=LINE('',#102488,#22400);
#16367=LINE('',#102489,#22401);
#16368=LINE('',#102492,#22402);
#16369=LINE('',#102493,#22403);
#16370=LINE('',#102501,#22404);
#16371=LINE('',#102503,#22405);
#16372=LINE('',#102504,#22406);
#16373=LINE('',#102512,#22407);
#16374=LINE('',#102514,#22408);
#16375=LINE('',#102515,#22409);
#16376=LINE('',#102518,#22410);
#16377=LINE('',#102521,#22411);
#16378=LINE('',#102526,#22412);
#16379=LINE('',#102528,#22413);
#16380=LINE('',#102529,#22414);
#16381=LINE('',#102530,#22415);
#16382=LINE('',#102531,#22416);
#16383=LINE('',#102532,#22417);
#16384=LINE('',#102533,#22418);
#16385=LINE('',#102534,#22419);
#16386=LINE('',#102535,#22420);
#16387=LINE('',#102536,#22421);
#16388=LINE('',#102537,#22422);
#16389=LINE('',#102538,#22423);
#16390=LINE('',#102539,#22424);
#16391=LINE('',#102540,#22425);
#16392=LINE('',#102541,#22426);
#16393=LINE('',#102542,#22427);
#16394=LINE('',#102548,#22428);
#16395=LINE('',#102550,#22429);
#16396=LINE('',#102552,#22430);
#16397=LINE('',#102554,#22431);
#16398=LINE('',#102556,#22432);
#16399=LINE('',#102560,#22433);
#16400=LINE('',#102565,#22434);
#16401=LINE('',#102569,#22435);
#16402=LINE('',#102580,#22436);
#16403=LINE('',#102584,#22437);
#16404=LINE('',#102587,#22438);
#16405=LINE('',#102592,#22439);
#16406=LINE('',#102596,#22440);
#16407=LINE('',#102605,#22441);
#16408=LINE('',#102608,#22442);
#16409=LINE('',#102613,#22443);
#16410=LINE('',#102614,#22444);
#16411=LINE('',#102617,#22445);
#16412=LINE('',#102618,#22446);
#16413=LINE('',#102622,#22447);
#16414=LINE('',#102624,#22448);
#16415=LINE('',#102626,#22449);
#16416=LINE('',#102632,#22450);
#16417=LINE('',#102656,#22451);
#16418=LINE('',#102704,#22452);
#16419=LINE('',#102752,#22453);
#16420=LINE('',#102806,#22454);
#16421=LINE('',#102854,#22455);
#16422=LINE('',#102908,#22456);
#16423=LINE('',#102956,#22457);
#16424=LINE('',#103004,#22458);
#16425=LINE('',#103058,#22459);
#16426=LINE('',#103106,#22460);
#16427=LINE('',#103154,#22461);
#16428=LINE('',#103178,#22462);
#16429=LINE('',#103202,#22463);
#16430=LINE('',#103227,#22464);
#16431=LINE('',#103252,#22465);
#16432=LINE('',#103276,#22466);
#16433=LINE('',#103301,#22467);
#16434=LINE('',#103326,#22468);
#16435=LINE('',#103351,#22469);
#16436=LINE('',#103376,#22470);
#16437=LINE('',#104373,#22471);
#16438=LINE('',#104375,#22472);
#16439=LINE('',#104377,#22473);
#16440=LINE('',#104383,#22474);
#16441=LINE('',#104390,#22475);
#16442=LINE('',#104396,#22476);
#16443=LINE('',#104402,#22477);
#16444=LINE('',#104403,#22478);
#16445=LINE('',#104418,#22479);
#16446=LINE('',#104422,#22480);
#16447=LINE('',#104428,#22481);
#16448=LINE('',#104452,#22482);
#16449=LINE('',#104500,#22483);
#16450=LINE('',#104548,#22484);
#16451=LINE('',#104602,#22485);
#16452=LINE('',#104650,#22486);
#16453=LINE('',#104674,#22487);
#16454=LINE('',#104699,#22488);
#16455=LINE('',#104724,#22489);
#16456=LINE('',#105403,#22490);
#16457=LINE('',#105465,#22491);
#16458=LINE('',#105467,#22492);
#16459=LINE('',#105471,#22493);
#16460=LINE('',#105473,#22494);
#16461=LINE('',#105477,#22495);
#16462=LINE('',#105480,#22496);
#16463=LINE('',#105483,#22497);
#16464=LINE('',#105485,#22498);
#16465=LINE('',#105489,#22499);
#16466=LINE('',#105492,#22500);
#16467=LINE('',#105495,#22501);
#16468=LINE('',#105498,#22502);
#16469=LINE('',#105500,#22503);
#16470=LINE('',#105502,#22504);
#16471=LINE('',#105504,#22505);
#16472=LINE('',#105505,#22506);
#16473=LINE('',#105507,#22507);
#16474=LINE('',#105509,#22508);
#16475=LINE('',#105510,#22509);
#16476=LINE('',#105512,#22510);
#16477=LINE('',#105514,#22511);
#16478=LINE('',#105515,#22512);
#16479=LINE('',#105519,#22513);
#16480=LINE('',#105522,#22514);
#16481=LINE('',#105524,#22515);
#16482=LINE('',#105527,#22516);
#16483=LINE('',#105537,#22517);
#16484=LINE('',#105540,#22518);
#16485=LINE('',#105544,#22519);
#16486=LINE('',#105546,#22520);
#16487=LINE('',#105548,#22521);
#16488=LINE('',#105554,#22522);
#16489=LINE('',#105560,#22523);
#16490=LINE('',#105566,#22524);
#16491=LINE('',#105590,#22525);
#16492=LINE('',#105638,#22526);
#16493=LINE('',#105686,#22527);
#16494=LINE('',#105739,#22528);
#16495=LINE('',#105760,#22529);
#16496=LINE('',#105785,#22530);
#16497=LINE('',#106348,#22531);
#16498=LINE('',#106410,#22532);
#16499=LINE('',#106412,#22533);
#16500=LINE('',#106416,#22534);
#16501=LINE('',#106418,#22535);
#16502=LINE('',#106422,#22536);
#16503=LINE('',#106425,#22537);
#16504=LINE('',#106428,#22538);
#16505=LINE('',#106430,#22539);
#16506=LINE('',#106434,#22540);
#16507=LINE('',#106437,#22541);
#16508=LINE('',#106440,#22542);
#16509=LINE('',#106443,#22543);
#16510=LINE('',#106445,#22544);
#16511=LINE('',#106447,#22545);
#16512=LINE('',#106449,#22546);
#16513=LINE('',#106450,#22547);
#16514=LINE('',#106452,#22548);
#16515=LINE('',#106454,#22549);
#16516=LINE('',#106455,#22550);
#16517=LINE('',#106457,#22551);
#16518=LINE('',#106459,#22552);
#16519=LINE('',#106460,#22553);
#16520=LINE('',#106464,#22554);
#16521=LINE('',#106467,#22555);
#16522=LINE('',#106469,#22556);
#16523=LINE('',#106472,#22557);
#16524=LINE('',#106482,#22558);
#16525=LINE('',#106485,#22559);
#16526=LINE('',#106489,#22560);
#16527=LINE('',#106491,#22561);
#16528=LINE('',#106493,#22562);
#16529=LINE('',#106499,#22563);
#16530=LINE('',#106505,#22564);
#16531=LINE('',#106511,#22565);
#16532=LINE('',#106535,#22566);
#16533=LINE('',#106583,#22567);
#16534=LINE('',#106631,#22568);
#16535=LINE('',#106685,#22569);
#16536=LINE('',#106733,#22570);
#16537=LINE('',#106781,#22571);
#16538=LINE('',#106835,#22572);
#16539=LINE('',#106883,#22573);
#16540=LINE('',#106931,#22574);
#16541=LINE('',#106985,#22575);
#16542=LINE('',#107033,#22576);
#16543=LINE('',#107057,#22577);
#16544=LINE('',#107082,#22578);
#16545=LINE('',#107107,#22579);
#16546=LINE('',#107131,#22580);
#16547=LINE('',#107156,#22581);
#16548=LINE('',#107181,#22582);
#16549=LINE('',#107205,#22583);
#16550=LINE('',#107230,#22584);
#16551=LINE('',#107255,#22585);
#16552=LINE('',#108238,#22586);
#16553=LINE('',#108300,#22587);
#16554=LINE('',#108302,#22588);
#16555=LINE('',#108306,#22589);
#16556=LINE('',#108308,#22590);
#16557=LINE('',#108312,#22591);
#16558=LINE('',#108315,#22592);
#16559=LINE('',#108318,#22593);
#16560=LINE('',#108320,#22594);
#16561=LINE('',#108324,#22595);
#16562=LINE('',#108327,#22596);
#16563=LINE('',#108330,#22597);
#16564=LINE('',#108333,#22598);
#16565=LINE('',#108335,#22599);
#16566=LINE('',#108337,#22600);
#16567=LINE('',#108339,#22601);
#16568=LINE('',#108340,#22602);
#16569=LINE('',#108342,#22603);
#16570=LINE('',#108344,#22604);
#16571=LINE('',#108345,#22605);
#16572=LINE('',#108347,#22606);
#16573=LINE('',#108349,#22607);
#16574=LINE('',#108350,#22608);
#16575=LINE('',#108354,#22609);
#16576=LINE('',#108357,#22610);
#16577=LINE('',#108359,#22611);
#16578=LINE('',#108362,#22612);
#16579=LINE('',#108372,#22613);
#16580=LINE('',#108375,#22614);
#16581=LINE('',#108379,#22615);
#16582=LINE('',#108381,#22616);
#16583=LINE('',#108383,#22617);
#16584=LINE('',#108389,#22618);
#16585=LINE('',#108395,#22619);
#16586=LINE('',#108401,#22620);
#16587=LINE('',#108425,#22621);
#16588=LINE('',#108473,#22622);
#16589=LINE('',#108521,#22623);
#16590=LINE('',#108575,#22624);
#16591=LINE('',#108623,#22625);
#16592=LINE('',#108671,#22626);
#16593=LINE('',#108682,#22627);
#16594=LINE('',#108708,#22628);
#16595=LINE('',#108732,#22629);
#16596=LINE('',#108757,#22630);
#16597=LINE('',#108782,#22631);
#16598=LINE('',#109501,#22632);
#16599=LINE('',#109563,#22633);
#16600=LINE('',#109565,#22634);
#16601=LINE('',#109569,#22635);
#16602=LINE('',#109571,#22636);
#16603=LINE('',#109575,#22637);
#16604=LINE('',#109578,#22638);
#16605=LINE('',#109581,#22639);
#16606=LINE('',#109583,#22640);
#16607=LINE('',#109587,#22641);
#16608=LINE('',#109590,#22642);
#16609=LINE('',#109593,#22643);
#16610=LINE('',#109596,#22644);
#16611=LINE('',#109598,#22645);
#16612=LINE('',#109600,#22646);
#16613=LINE('',#109602,#22647);
#16614=LINE('',#109603,#22648);
#16615=LINE('',#109605,#22649);
#16616=LINE('',#109607,#22650);
#16617=LINE('',#109608,#22651);
#16618=LINE('',#109610,#22652);
#16619=LINE('',#109612,#22653);
#16620=LINE('',#109613,#22654);
#16621=LINE('',#109617,#22655);
#16622=LINE('',#109620,#22656);
#16623=LINE('',#109622,#22657);
#16624=LINE('',#109625,#22658);
#16625=LINE('',#109635,#22659);
#16626=LINE('',#109638,#22660);
#16627=LINE('',#109642,#22661);
#16628=LINE('',#109644,#22662);
#16629=LINE('',#109646,#22663);
#16630=LINE('',#109652,#22664);
#16631=LINE('',#109658,#22665);
#16632=LINE('',#109664,#22666);
#16633=LINE('',#109688,#22667);
#16634=LINE('',#109736,#22668);
#16635=LINE('',#109784,#22669);
#16636=LINE('',#109838,#22670);
#16637=LINE('',#109886,#22671);
#16638=LINE('',#109934,#22672);
#16639=LINE('',#109988,#22673);
#16640=LINE('',#110035,#22674);
#16641=LINE('',#110055,#22675);
#16642=LINE('',#110080,#22676);
#16643=LINE('',#110105,#22677);
#16644=LINE('',#110129,#22678);
#16645=LINE('',#110154,#22679);
#16646=LINE('',#110179,#22680);
#16647=LINE('',#110941,#22681);
#16648=LINE('',#110943,#22682);
#16649=LINE('',#110945,#22683);
#16650=LINE('',#110946,#22684);
#16651=LINE('',#110949,#22685);
#16652=LINE('',#110951,#22686);
#16653=LINE('',#110952,#22687);
#16654=LINE('',#110955,#22688);
#16655=LINE('',#110957,#22689);
#16656=LINE('',#110958,#22690);
#16657=LINE('',#110961,#22691);
#16658=LINE('',#110963,#22692);
#16659=LINE('',#110964,#22693);
#16660=LINE('',#110967,#22694);
#16661=LINE('',#110969,#22695);
#16662=LINE('',#110970,#22696);
#16663=LINE('',#110972,#22697);
#16664=LINE('',#110973,#22698);
#16665=LINE('',#110979,#22699);
#16666=LINE('',#110985,#22700);
#16667=LINE('',#110991,#22701);
#16668=LINE('',#111015,#22702);
#16669=LINE('',#111063,#22703);
#16670=LINE('',#111111,#22704);
#16671=LINE('',#111165,#22705);
#16672=LINE('',#111213,#22706);
#16673=LINE('',#111261,#22707);
#16674=LINE('',#111315,#22708);
#16675=LINE('',#111363,#22709);
#16676=LINE('',#111411,#22710);
#16677=LINE('',#111459,#22711);
#16678=LINE('',#111513,#22712);
#16679=LINE('',#111561,#22713);
#16680=LINE('',#111609,#22714);
#16681=LINE('',#111631,#22715);
#16682=LINE('',#111655,#22716);
#16683=LINE('',#111680,#22717);
#16684=LINE('',#111705,#22718);
#16685=LINE('',#111729,#22719);
#16686=LINE('',#111753,#22720);
#16687=LINE('',#111778,#22721);
#16688=LINE('',#111803,#22722);
#16689=LINE('',#111827,#22723);
#16690=LINE('',#111852,#22724);
#16691=LINE('',#111877,#22725);
#16692=LINE('',#112943,#22726);
#16693=LINE('',#112953,#22727);
#16694=LINE('',#112955,#22728);
#16695=LINE('',#112956,#22729);
#16696=LINE('',#112960,#22730);
#16697=LINE('',#112966,#22731);
#16698=LINE('',#112971,#22732);
#16699=LINE('',#112975,#22733);
#16700=LINE('',#112979,#22734);
#16701=LINE('',#112983,#22735);
#16702=LINE('',#112987,#22736);
#16703=LINE('',#112991,#22737);
#16704=LINE('',#112995,#22738);
#16705=LINE('',#112999,#22739);
#16706=LINE('',#113003,#22740);
#16707=LINE('',#113007,#22741);
#16708=LINE('',#113011,#22742);
#16709=LINE('',#113015,#22743);
#16710=LINE('',#113019,#22744);
#16711=LINE('',#113023,#22745);
#16712=LINE('',#113027,#22746);
#16713=LINE('',#113031,#22747);
#16714=LINE('',#113035,#22748);
#16715=LINE('',#113039,#22749);
#16716=LINE('',#113043,#22750);
#16717=LINE('',#113047,#22751);
#16718=LINE('',#113051,#22752);
#16719=LINE('',#113055,#22753);
#16720=LINE('',#113059,#22754);
#16721=LINE('',#113063,#22755);
#16722=LINE('',#113067,#22756);
#16723=LINE('',#113071,#22757);
#16724=LINE('',#113075,#22758);
#16725=LINE('',#113079,#22759);
#16726=LINE('',#113083,#22760);
#16727=LINE('',#113087,#22761);
#16728=LINE('',#113091,#22762);
#16729=LINE('',#113095,#22763);
#16730=LINE('',#113099,#22764);
#16731=LINE('',#113103,#22765);
#16732=LINE('',#113107,#22766);
#16733=LINE('',#113111,#22767);
#16734=LINE('',#113115,#22768);
#16735=LINE('',#113119,#22769);
#16736=LINE('',#113126,#22770);
#16737=LINE('',#113130,#22771);
#16738=LINE('',#113134,#22772);
#16739=LINE('',#113138,#22773);
#16740=LINE('',#113142,#22774);
#16741=LINE('',#113146,#22775);
#16742=LINE('',#113150,#22776);
#16743=LINE('',#113154,#22777);
#16744=LINE('',#113158,#22778);
#16745=LINE('',#113162,#22779);
#16746=LINE('',#113166,#22780);
#16747=LINE('',#113170,#22781);
#16748=LINE('',#113174,#22782);
#16749=LINE('',#113178,#22783);
#16750=LINE('',#113182,#22784);
#16751=LINE('',#113186,#22785);
#16752=LINE('',#113190,#22786);
#16753=LINE('',#113194,#22787);
#16754=LINE('',#113198,#22788);
#16755=LINE('',#113202,#22789);
#16756=LINE('',#113206,#22790);
#16757=LINE('',#113210,#22791);
#16758=LINE('',#113214,#22792);
#16759=LINE('',#113218,#22793);
#16760=LINE('',#113222,#22794);
#16761=LINE('',#113226,#22795);
#16762=LINE('',#113230,#22796);
#16763=LINE('',#113234,#22797);
#16764=LINE('',#113238,#22798);
#16765=LINE('',#113242,#22799);
#16766=LINE('',#113246,#22800);
#16767=LINE('',#113250,#22801);
#16768=LINE('',#113254,#22802);
#16769=LINE('',#113262,#22803);
#16770=LINE('',#113263,#22804);
#16771=LINE('',#113265,#22805);
#16772=LINE('',#113276,#22806);
#16773=LINE('',#113277,#22807);
#16774=LINE('',#113279,#22808);
#16775=LINE('',#113290,#22809);
#16776=LINE('',#113291,#22810);
#16777=LINE('',#113293,#22811);
#16778=LINE('',#113304,#22812);
#16779=LINE('',#113305,#22813);
#16780=LINE('',#113307,#22814);
#16781=LINE('',#113318,#22815);
#16782=LINE('',#113319,#22816);
#16783=LINE('',#113321,#22817);
#16784=LINE('',#113332,#22818);
#16785=LINE('',#113333,#22819);
#16786=LINE('',#113335,#22820);
#16787=LINE('',#113346,#22821);
#16788=LINE('',#113347,#22822);
#16789=LINE('',#113349,#22823);
#16790=LINE('',#113360,#22824);
#16791=LINE('',#113361,#22825);
#16792=LINE('',#113363,#22826);
#16793=LINE('',#113374,#22827);
#16794=LINE('',#113375,#22828);
#16795=LINE('',#113377,#22829);
#16796=LINE('',#113388,#22830);
#16797=LINE('',#113389,#22831);
#16798=LINE('',#113391,#22832);
#16799=LINE('',#113402,#22833);
#16800=LINE('',#113403,#22834);
#16801=LINE('',#113405,#22835);
#16802=LINE('',#113416,#22836);
#16803=LINE('',#113417,#22837);
#16804=LINE('',#113419,#22838);
#16805=LINE('',#113430,#22839);
#16806=LINE('',#113431,#22840);
#16807=LINE('',#113433,#22841);
#16808=LINE('',#113444,#22842);
#16809=LINE('',#113445,#22843);
#16810=LINE('',#113447,#22844);
#16811=LINE('',#113458,#22845);
#16812=LINE('',#113459,#22846);
#16813=LINE('',#113461,#22847);
#16814=LINE('',#113472,#22848);
#16815=LINE('',#113473,#22849);
#16816=LINE('',#113475,#22850);
#16817=LINE('',#113486,#22851);
#16818=LINE('',#113487,#22852);
#16819=LINE('',#113489,#22853);
#16820=LINE('',#113500,#22854);
#16821=LINE('',#113501,#22855);
#16822=LINE('',#113503,#22856);
#16823=LINE('',#113514,#22857);
#16824=LINE('',#113515,#22858);
#16825=LINE('',#113517,#22859);
#16826=LINE('',#113528,#22860);
#16827=LINE('',#113529,#22861);
#16828=LINE('',#113531,#22862);
#16829=LINE('',#113542,#22863);
#16830=LINE('',#113543,#22864);
#16831=LINE('',#113545,#22865);
#16832=LINE('',#113556,#22866);
#16833=LINE('',#113557,#22867);
#16834=LINE('',#113559,#22868);
#16835=LINE('',#113570,#22869);
#16836=LINE('',#113571,#22870);
#16837=LINE('',#113573,#22871);
#16838=LINE('',#113584,#22872);
#16839=LINE('',#113585,#22873);
#16840=LINE('',#113587,#22874);
#16841=LINE('',#113598,#22875);
#16842=LINE('',#113599,#22876);
#16843=LINE('',#113601,#22877);
#16844=LINE('',#113612,#22878);
#16845=LINE('',#113613,#22879);
#16846=LINE('',#113615,#22880);
#16847=LINE('',#113626,#22881);
#16848=LINE('',#113627,#22882);
#16849=LINE('',#113629,#22883);
#16850=LINE('',#113640,#22884);
#16851=LINE('',#113641,#22885);
#16852=LINE('',#113643,#22886);
#16853=LINE('',#113654,#22887);
#16854=LINE('',#113655,#22888);
#16855=LINE('',#113657,#22889);
#16856=LINE('',#113668,#22890);
#16857=LINE('',#113669,#22891);
#16858=LINE('',#113671,#22892);
#16859=LINE('',#113682,#22893);
#16860=LINE('',#113683,#22894);
#16861=LINE('',#113685,#22895);
#16862=LINE('',#113696,#22896);
#16863=LINE('',#113697,#22897);
#16864=LINE('',#113699,#22898);
#16865=LINE('',#113710,#22899);
#16866=LINE('',#113711,#22900);
#16867=LINE('',#113713,#22901);
#16868=LINE('',#113724,#22902);
#16869=LINE('',#113725,#22903);
#16870=LINE('',#113727,#22904);
#16871=LINE('',#113738,#22905);
#16872=LINE('',#113739,#22906);
#16873=LINE('',#113741,#22907);
#16874=LINE('',#113751,#22908);
#16875=LINE('',#113757,#22909);
#16876=LINE('',#113819,#22910);
#16877=LINE('',#113821,#22911);
#16878=LINE('',#113825,#22912);
#16879=LINE('',#113827,#22913);
#16880=LINE('',#113831,#22914);
#16881=LINE('',#113834,#22915);
#16882=LINE('',#113837,#22916);
#16883=LINE('',#113839,#22917);
#16884=LINE('',#113843,#22918);
#16885=LINE('',#113846,#22919);
#16886=LINE('',#113849,#22920);
#16887=LINE('',#113852,#22921);
#16888=LINE('',#113854,#22922);
#16889=LINE('',#113856,#22923);
#16890=LINE('',#113858,#22924);
#16891=LINE('',#113859,#22925);
#16892=LINE('',#113861,#22926);
#16893=LINE('',#113863,#22927);
#16894=LINE('',#113864,#22928);
#16895=LINE('',#113866,#22929);
#16896=LINE('',#113868,#22930);
#16897=LINE('',#113869,#22931);
#16898=LINE('',#113873,#22932);
#16899=LINE('',#113876,#22933);
#16900=LINE('',#113878,#22934);
#16901=LINE('',#113881,#22935);
#16902=LINE('',#113891,#22936);
#16903=LINE('',#113894,#22937);
#16904=LINE('',#113898,#22938);
#16905=LINE('',#113900,#22939);
#16906=LINE('',#113902,#22940);
#16907=LINE('',#113911,#22941);
#16908=LINE('',#113915,#22942);
#16909=LINE('',#113919,#22943);
#16910=VECTOR('',#63780,10.);
#16911=VECTOR('',#63781,10.);
#16912=VECTOR('',#63782,10.);
#16913=VECTOR('',#63783,10.);
#16914=VECTOR('',#63784,10.);
#16915=VECTOR('',#63785,10.);
#16916=VECTOR('',#63786,10.);
#16917=VECTOR('',#63787,10.);
#16918=VECTOR('',#63788,10.);
#16919=VECTOR('',#63789,10.);
#16920=VECTOR('',#63790,10.);
#16921=VECTOR('',#63791,10.);
#16922=VECTOR('',#63792,10.);
#16923=VECTOR('',#63793,10.);
#16924=VECTOR('',#63794,10.);
#16925=VECTOR('',#63795,10.);
#16926=VECTOR('',#63796,10.);
#16927=VECTOR('',#63797,10.);
#16928=VECTOR('',#63798,10.);
#16929=VECTOR('',#63799,10.);
#16930=VECTOR('',#63802,10.);
#16931=VECTOR('',#63803,10.);
#16932=VECTOR('',#63804,10.);
#16933=VECTOR('',#63805,10.);
#16934=VECTOR('',#63806,10.);
#16935=VECTOR('',#63807,10.);
#16936=VECTOR('',#63808,10.);
#16937=VECTOR('',#63809,10.);
#16938=VECTOR('',#63810,10.);
#16939=VECTOR('',#63811,10.);
#16940=VECTOR('',#63812,10.);
#16941=VECTOR('',#63813,10.);
#16942=VECTOR('',#63814,10.);
#16943=VECTOR('',#63815,10.);
#16944=VECTOR('',#63816,10.);
#16945=VECTOR('',#63817,10.);
#16946=VECTOR('',#63818,10.);
#16947=VECTOR('',#63819,10.);
#16948=VECTOR('',#63820,10.);
#16949=VECTOR('',#63821,10.);
#16950=VECTOR('',#63822,10.);
#16951=VECTOR('',#63823,10.);
#16952=VECTOR('',#63824,10.);
#16953=VECTOR('',#63825,10.);
#16954=VECTOR('',#63826,10.);
#16955=VECTOR('',#63827,10.);
#16956=VECTOR('',#63828,10.);
#16957=VECTOR('',#63829,10.);
#16958=VECTOR('',#63830,10.);
#16959=VECTOR('',#63833,10.);
#16960=VECTOR('',#63834,10.);
#16961=VECTOR('',#63835,10.);
#16962=VECTOR('',#63842,10.);
#16963=VECTOR('',#63843,10.);
#16964=VECTOR('',#63844,10.);
#16965=VECTOR('',#63845,10.);
#16966=VECTOR('',#63846,10.);
#16967=VECTOR('',#63847,10.);
#16968=VECTOR('',#63848,10.);
#16969=VECTOR('',#63849,10.);
#16970=VECTOR('',#63850,10.);
#16971=VECTOR('',#63851,10.);
#16972=VECTOR('',#63852,10.);
#16973=VECTOR('',#63853,10.);
#16974=VECTOR('',#63854,10.);
#16975=VECTOR('',#63855,10.);
#16976=VECTOR('',#63856,10.);
#16977=VECTOR('',#63857,10.);
#16978=VECTOR('',#63858,10.);
#16979=VECTOR('',#63859,10.);
#16980=VECTOR('',#63860,10.);
#16981=VECTOR('',#63861,10.);
#16982=VECTOR('',#63864,10.);
#16983=VECTOR('',#63865,10.);
#16984=VECTOR('',#63866,10.);
#16985=VECTOR('',#63867,10.);
#16986=VECTOR('',#63868,10.);
#16987=VECTOR('',#63869,10.);
#16988=VECTOR('',#63870,10.);
#16989=VECTOR('',#63871,10.);
#16990=VECTOR('',#63872,10.);
#16991=VECTOR('',#63873,10.);
#16992=VECTOR('',#63874,10.);
#16993=VECTOR('',#63875,10.);
#16994=VECTOR('',#63876,10.);
#16995=VECTOR('',#63877,10.);
#16996=VECTOR('',#63878,10.);
#16997=VECTOR('',#63879,10.);
#16998=VECTOR('',#63880,10.);
#16999=VECTOR('',#63881,10.);
#17000=VECTOR('',#63882,10.);
#17001=VECTOR('',#63883,10.);
#17002=VECTOR('',#63884,10.);
#17003=VECTOR('',#63885,10.);
#17004=VECTOR('',#63886,10.);
#17005=VECTOR('',#63887,10.);
#17006=VECTOR('',#63888,10.);
#17007=VECTOR('',#63889,10.);
#17008=VECTOR('',#63890,10.);
#17009=VECTOR('',#63891,10.);
#17010=VECTOR('',#63892,10.);
#17011=VECTOR('',#63893,10.);
#17012=VECTOR('',#63894,10.);
#17013=VECTOR('',#63895,10.);
#17014=VECTOR('',#63896,10.);
#17015=VECTOR('',#63905,10.);
#17016=VECTOR('',#63906,10.);
#17017=VECTOR('',#63907,10.);
#17018=VECTOR('',#63908,10.);
#17019=VECTOR('',#63909,10.);
#17020=VECTOR('',#63910,10.);
#17021=VECTOR('',#63911,10.);
#17022=VECTOR('',#63912,10.);
#17023=VECTOR('',#63913,10.);
#17024=VECTOR('',#63914,10.);
#17025=VECTOR('',#63915,10.);
#17026=VECTOR('',#63916,10.);
#17027=VECTOR('',#63917,10.);
#17028=VECTOR('',#63918,10.);
#17029=VECTOR('',#63919,10.);
#17030=VECTOR('',#63920,10.);
#17031=VECTOR('',#63921,10.);
#17032=VECTOR('',#63922,10.);
#17033=VECTOR('',#63923,10.);
#17034=VECTOR('',#63924,10.);
#17035=VECTOR('',#63927,10.);
#17036=VECTOR('',#63928,10.);
#17037=VECTOR('',#63929,10.);
#17038=VECTOR('',#63930,10.);
#17039=VECTOR('',#63933,10.);
#17040=VECTOR('',#63934,10.);
#17041=VECTOR('',#63935,10.);
#17042=VECTOR('',#63936,10.);
#17043=VECTOR('',#63937,10.);
#17044=VECTOR('',#63938,10.);
#17045=VECTOR('',#63941,10.);
#17046=VECTOR('',#63942,10.);
#17047=VECTOR('',#63943,10.);
#17048=VECTOR('',#63946,10.);
#17049=VECTOR('',#63947,10.);
#17050=VECTOR('',#63948,10.);
#17051=VECTOR('',#63951,10.);
#17052=VECTOR('',#63952,10.);
#17053=VECTOR('',#63953,10.);
#17054=VECTOR('',#63956,10.);
#17055=VECTOR('',#63957,10.);
#17056=VECTOR('',#63962,10.);
#17057=VECTOR('',#63963,10.);
#17058=VECTOR('',#63964,10.);
#17059=VECTOR('',#63965,10.);
#17060=VECTOR('',#63966,10.);
#17061=VECTOR('',#63967,10.);
#17062=VECTOR('',#63968,10.);
#17063=VECTOR('',#63969,10.);
#17064=VECTOR('',#63970,10.);
#17065=VECTOR('',#63971,10.);
#17066=VECTOR('',#63972,10.);
#17067=VECTOR('',#63973,10.);
#17068=VECTOR('',#63974,10.);
#17069=VECTOR('',#63975,10.);
#17070=VECTOR('',#63976,10.);
#17071=VECTOR('',#63977,10.);
#17072=VECTOR('',#63978,10.);
#17073=VECTOR('',#63979,10.);
#17074=VECTOR('',#63980,10.);
#17075=VECTOR('',#63981,10.);
#17076=VECTOR('',#63984,10.);
#17077=VECTOR('',#63985,10.);
#17078=VECTOR('',#63986,10.);
#17079=VECTOR('',#63987,10.);
#17080=VECTOR('',#63988,10.);
#17081=VECTOR('',#63989,10.);
#17082=VECTOR('',#63990,10.);
#17083=VECTOR('',#63991,10.);
#17084=VECTOR('',#63992,10.);
#17085=VECTOR('',#63993,10.);
#17086=VECTOR('',#63994,10.);
#17087=VECTOR('',#63995,10.);
#17088=VECTOR('',#63996,10.);
#17089=VECTOR('',#63997,10.);
#17090=VECTOR('',#63998,10.);
#17091=VECTOR('',#63999,10.);
#17092=VECTOR('',#64000,10.);
#17093=VECTOR('',#64001,10.);
#17094=VECTOR('',#64002,10.);
#17095=VECTOR('',#64003,10.);
#17096=VECTOR('',#64004,10.);
#17097=VECTOR('',#64005,10.);
#17098=VECTOR('',#64006,10.);
#17099=VECTOR('',#64007,10.);
#17100=VECTOR('',#64008,10.);
#17101=VECTOR('',#64009,10.);
#17102=VECTOR('',#64010,10.);
#17103=VECTOR('',#64013,10.);
#17104=VECTOR('',#64014,10.);
#17105=VECTOR('',#64015,10.);
#17106=VECTOR('',#64022,10.);
#17107=VECTOR('',#64023,10.);
#17108=VECTOR('',#64024,10.);
#17109=VECTOR('',#64025,10.);
#17110=VECTOR('',#64026,10.);
#17111=VECTOR('',#64027,10.);
#17112=VECTOR('',#64028,10.);
#17113=VECTOR('',#64029,10.);
#17114=VECTOR('',#64030,10.);
#17115=VECTOR('',#64031,10.);
#17116=VECTOR('',#64032,10.);
#17117=VECTOR('',#64033,10.);
#17118=VECTOR('',#64034,10.);
#17119=VECTOR('',#64035,10.);
#17120=VECTOR('',#64036,10.);
#17121=VECTOR('',#64037,10.);
#17122=VECTOR('',#64038,10.);
#17123=VECTOR('',#64039,10.);
#17124=VECTOR('',#64040,10.);
#17125=VECTOR('',#64041,10.);
#17126=VECTOR('',#64044,10.);
#17127=VECTOR('',#64045,10.);
#17128=VECTOR('',#64046,10.);
#17129=VECTOR('',#64047,10.);
#17130=VECTOR('',#64048,10.);
#17131=VECTOR('',#64049,10.);
#17132=VECTOR('',#64050,10.);
#17133=VECTOR('',#64053,10.);
#17134=VECTOR('',#64054,10.);
#17135=VECTOR('',#64055,10.);
#17136=VECTOR('',#64058,10.);
#17137=VECTOR('',#64059,10.);
#17138=VECTOR('',#64060,10.);
#17139=VECTOR('',#64063,10.);
#17140=VECTOR('',#64064,10.);
#17141=VECTOR('',#64065,10.);
#17142=VECTOR('',#64068,10.);
#17143=VECTOR('',#64069,10.);
#17144=VECTOR('',#64070,10.);
#17145=VECTOR('',#64073,10.);
#17146=VECTOR('',#64074,10.);
#17147=VECTOR('',#64075,10.);
#17148=VECTOR('',#64078,10.);
#17149=VECTOR('',#64079,10.);
#17150=VECTOR('',#64080,10.);
#17151=VECTOR('',#64081,10.);
#17152=VECTOR('',#64082,10.);
#17153=VECTOR('',#64083,10.);
#17154=VECTOR('',#64084,10.);
#17155=VECTOR('',#64085,10.);
#17156=VECTOR('',#64086,10.);
#17157=VECTOR('',#64087,10.);
#17158=VECTOR('',#64088,10.);
#17159=VECTOR('',#64091,10.);
#17160=VECTOR('',#64092,10.);
#17161=VECTOR('',#64093,10.);
#17162=VECTOR('',#64098,10.);
#17163=VECTOR('',#64099,10.);
#17164=VECTOR('',#64100,10.);
#17165=VECTOR('',#64101,10.);
#17166=VECTOR('',#64102,10.);
#17167=VECTOR('',#64103,10.);
#17168=VECTOR('',#64104,10.);
#17169=VECTOR('',#64105,10.);
#17170=VECTOR('',#64106,10.);
#17171=VECTOR('',#64107,10.);
#17172=VECTOR('',#64108,10.);
#17173=VECTOR('',#64109,10.);
#17174=VECTOR('',#64110,10.);
#17175=VECTOR('',#64111,10.);
#17176=VECTOR('',#64112,10.);
#17177=VECTOR('',#64113,10.);
#17178=VECTOR('',#64114,10.);
#17179=VECTOR('',#64115,10.);
#17180=VECTOR('',#64116,10.);
#17181=VECTOR('',#64117,10.);
#17182=VECTOR('',#64122,10.);
#17183=VECTOR('',#64123,10.);
#17184=VECTOR('',#64124,10.);
#17185=VECTOR('',#64125,10.);
#17186=VECTOR('',#64128,10.);
#17187=VECTOR('',#64129,10.);
#17188=VECTOR('',#64130,10.);
#17189=VECTOR('',#64133,10.);
#17190=VECTOR('',#64134,10.);
#17191=VECTOR('',#64137,10.);
#17192=VECTOR('',#64138,10.);
#17193=VECTOR('',#64139,10.);
#17194=VECTOR('',#64140,10.);
#17195=VECTOR('',#64143,10.);
#17196=VECTOR('',#64144,10.);
#17197=VECTOR('',#64145,10.);
#17198=VECTOR('',#64148,10.);
#17199=VECTOR('',#64149,10.);
#17200=VECTOR('',#64150,10.);
#17201=VECTOR('',#64153,10.);
#17202=VECTOR('',#64154,10.);
#17203=VECTOR('',#64155,10.);
#17204=VECTOR('',#64158,10.);
#17205=VECTOR('',#64159,10.);
#17206=VECTOR('',#64160,10.);
#17207=VECTOR('',#64163,10.);
#17208=VECTOR('',#64164,10.);
#17209=VECTOR('',#64165,10.);
#17210=VECTOR('',#64168,10.);
#17211=VECTOR('',#64169,10.);
#17212=VECTOR('',#64170,10.);
#17213=VECTOR('',#64173,10.);
#17214=VECTOR('',#64174,10.);
#17215=VECTOR('',#64175,10.);
#17216=VECTOR('',#64178,10.);
#17217=VECTOR('',#64179,10.);
#17218=VECTOR('',#64180,10.);
#17219=VECTOR('',#64183,10.);
#17220=VECTOR('',#64184,10.);
#17221=VECTOR('',#64185,10.);
#17222=VECTOR('',#64188,10.);
#17223=VECTOR('',#64189,10.);
#17224=VECTOR('',#64196,10.);
#17225=VECTOR('',#64197,10.);
#17226=VECTOR('',#64198,10.);
#17227=VECTOR('',#64199,10.);
#17228=VECTOR('',#64200,10.);
#17229=VECTOR('',#64201,10.);
#17230=VECTOR('',#64202,10.);
#17231=VECTOR('',#64203,10.);
#17232=VECTOR('',#64204,10.);
#17233=VECTOR('',#64205,10.);
#17234=VECTOR('',#64206,10.);
#17235=VECTOR('',#64207,10.);
#17236=VECTOR('',#64208,10.);
#17237=VECTOR('',#64209,10.);
#17238=VECTOR('',#64210,10.);
#17239=VECTOR('',#64211,10.);
#17240=VECTOR('',#64212,10.);
#17241=VECTOR('',#64213,10.);
#17242=VECTOR('',#64214,10.);
#17243=VECTOR('',#64215,10.);
#17244=VECTOR('',#64218,10.);
#17245=VECTOR('',#64219,10.);
#17246=VECTOR('',#64220,10.);
#17247=VECTOR('',#64221,10.);
#17248=VECTOR('',#64222,10.);
#17249=VECTOR('',#64223,10.);
#17250=VECTOR('',#64224,10.);
#17251=VECTOR('',#64225,10.);
#17252=VECTOR('',#64226,10.);
#17253=VECTOR('',#64227,10.);
#17254=VECTOR('',#64228,10.);
#17255=VECTOR('',#64229,10.);
#17256=VECTOR('',#64230,10.);
#17257=VECTOR('',#64233,10.);
#17258=VECTOR('',#64234,10.);
#17259=VECTOR('',#64235,10.);
#17260=VECTOR('',#64236,10.);
#17261=VECTOR('',#64237,10.);
#17262=VECTOR('',#64238,10.);
#17263=VECTOR('',#64239,10.);
#17264=VECTOR('',#64240,10.);
#17265=VECTOR('',#64241,10.);
#17266=VECTOR('',#64242,10.);
#17267=VECTOR('',#64245,10.);
#17268=VECTOR('',#64246,10.);
#17269=VECTOR('',#64247,10.);
#17270=VECTOR('',#64248,10.);
#17271=VECTOR('',#64249,10.);
#17272=VECTOR('',#64250,10.);
#17273=VECTOR('',#64251,10.);
#17274=VECTOR('',#64252,10.);
#17275=VECTOR('',#64253,10.);
#17276=VECTOR('',#64254,10.);
#17277=VECTOR('',#64257,10.);
#17278=VECTOR('',#64258,10.);
#17279=VECTOR('',#64259,10.);
#17280=VECTOR('',#64264,10.);
#17281=VECTOR('',#64265,10.);
#17282=VECTOR('',#64266,10.);
#17283=VECTOR('',#64267,10.);
#17284=VECTOR('',#64268,10.);
#17285=VECTOR('',#64269,10.);
#17286=VECTOR('',#64270,10.);
#17287=VECTOR('',#64271,10.);
#17288=VECTOR('',#64272,10.);
#17289=VECTOR('',#64273,10.);
#17290=VECTOR('',#64274,10.);
#17291=VECTOR('',#64275,10.);
#17292=VECTOR('',#64276,10.);
#17293=VECTOR('',#64277,10.);
#17294=VECTOR('',#64278,10.);
#17295=VECTOR('',#64279,10.);
#17296=VECTOR('',#64280,10.);
#17297=VECTOR('',#64281,10.);
#17298=VECTOR('',#64282,10.);
#17299=VECTOR('',#64283,10.);
#17300=VECTOR('',#64286,10.);
#17301=VECTOR('',#64287,10.);
#17302=VECTOR('',#64288,10.);
#17303=VECTOR('',#64289,10.);
#17304=VECTOR('',#64290,10.);
#17305=VECTOR('',#64291,10.);
#17306=VECTOR('',#64292,10.);
#17307=VECTOR('',#64293,10.);
#17308=VECTOR('',#64294,10.);
#17309=VECTOR('',#64295,10.);
#17310=VECTOR('',#64298,10.);
#17311=VECTOR('',#64299,10.);
#17312=VECTOR('',#64300,10.);
#17313=VECTOR('',#64301,10.);
#17314=VECTOR('',#64302,10.);
#17315=VECTOR('',#64303,10.);
#17316=VECTOR('',#64304,10.);
#17317=VECTOR('',#64305,10.);
#17318=VECTOR('',#64306,10.);
#17319=VECTOR('',#64307,10.);
#17320=VECTOR('',#64308,10.);
#17321=VECTOR('',#64309,10.);
#17322=VECTOR('',#64312,10.);
#17323=VECTOR('',#64313,10.);
#17324=VECTOR('',#64314,10.);
#17325=VECTOR('',#64317,10.);
#17326=VECTOR('',#64318,10.);
#17327=VECTOR('',#64319,10.);
#17328=VECTOR('',#64322,10.);
#17329=VECTOR('',#64323,10.);
#17330=VECTOR('',#64328,10.);
#17331=VECTOR('',#64329,10.);
#17332=VECTOR('',#64330,10.);
#17333=VECTOR('',#64331,10.);
#17334=VECTOR('',#64332,10.);
#17335=VECTOR('',#64333,10.);
#17336=VECTOR('',#64334,10.);
#17337=VECTOR('',#64335,10.);
#17338=VECTOR('',#64336,10.);
#17339=VECTOR('',#64337,10.);
#17340=VECTOR('',#64338,10.);
#17341=VECTOR('',#64339,10.);
#17342=VECTOR('',#64340,10.);
#17343=VECTOR('',#64341,10.);
#17344=VECTOR('',#64342,10.);
#17345=VECTOR('',#64343,10.);
#17346=VECTOR('',#64344,10.);
#17347=VECTOR('',#64345,10.);
#17348=VECTOR('',#64346,10.);
#17349=VECTOR('',#64347,10.);
#17350=VECTOR('',#64352,10.);
#17351=VECTOR('',#64353,10.);
#17352=VECTOR('',#64354,10.);
#17353=VECTOR('',#64355,10.);
#17354=VECTOR('',#64356,10.);
#17355=VECTOR('',#64357,10.);
#17356=VECTOR('',#64360,10.);
#17357=VECTOR('',#64361,10.);
#17358=VECTOR('',#64362,10.);
#17359=VECTOR('',#64363,10.);
#17360=VECTOR('',#64364,10.);
#17361=VECTOR('',#64367,10.);
#17362=VECTOR('',#64368,10.);
#17363=VECTOR('',#64369,10.);
#17364=VECTOR('',#64372,10.);
#17365=VECTOR('',#64373,10.);
#17366=VECTOR('',#64374,10.);
#17367=VECTOR('',#64377,10.);
#17368=VECTOR('',#64378,10.);
#17369=VECTOR('',#64383,10.);
#17370=VECTOR('',#64384,10.);
#17371=VECTOR('',#64385,10.);
#17372=VECTOR('',#64386,10.);
#17373=VECTOR('',#64387,10.);
#17374=VECTOR('',#64388,10.);
#17375=VECTOR('',#64389,10.);
#17376=VECTOR('',#64390,10.);
#17377=VECTOR('',#64391,10.);
#17378=VECTOR('',#64392,10.);
#17379=VECTOR('',#64393,10.);
#17380=VECTOR('',#64394,10.);
#17381=VECTOR('',#64395,10.);
#17382=VECTOR('',#64396,10.);
#17383=VECTOR('',#64397,10.);
#17384=VECTOR('',#64398,10.);
#17385=VECTOR('',#64399,10.);
#17386=VECTOR('',#64400,10.);
#17387=VECTOR('',#64401,10.);
#17388=VECTOR('',#64402,10.);
#17389=VECTOR('',#64407,10.);
#17390=VECTOR('',#64408,10.);
#17391=VECTOR('',#64409,10.);
#17392=VECTOR('',#64410,10.);
#17393=VECTOR('',#64411,10.);
#17394=VECTOR('',#64412,10.);
#17395=VECTOR('',#64413,10.);
#17396=VECTOR('',#64414,10.);
#17397=VECTOR('',#64415,10.);
#17398=VECTOR('',#64416,10.);
#17399=VECTOR('',#64417,10.);
#17400=VECTOR('',#64418,10.);
#17401=VECTOR('',#64419,10.);
#17402=VECTOR('',#64420,10.);
#17403=VECTOR('',#64421,10.);
#17404=VECTOR('',#64422,10.);
#17405=VECTOR('',#64423,10.);
#17406=VECTOR('',#64424,10.);
#17407=VECTOR('',#64425,10.);
#17408=VECTOR('',#64426,10.);
#17409=VECTOR('',#64431,10.);
#17410=VECTOR('',#64432,10.);
#17411=VECTOR('',#64433,10.);
#17412=VECTOR('',#64434,10.);
#17413=VECTOR('',#64435,10.);
#17414=VECTOR('',#64436,10.);
#17415=VECTOR('',#64439,10.);
#17416=VECTOR('',#64440,10.);
#17417=VECTOR('',#64441,10.);
#17418=VECTOR('',#64442,10.);
#17419=VECTOR('',#64443,10.);
#17420=VECTOR('',#64446,10.);
#17421=VECTOR('',#64447,10.);
#17422=VECTOR('',#64448,10.);
#17423=VECTOR('',#64451,10.);
#17424=VECTOR('',#64452,10.);
#17425=VECTOR('',#64453,10.);
#17426=VECTOR('',#64456,10.);
#17427=VECTOR('',#64457,10.);
#17428=VECTOR('',#64462,10.);
#17429=VECTOR('',#64463,10.);
#17430=VECTOR('',#64464,10.);
#17431=VECTOR('',#64465,10.);
#17432=VECTOR('',#64466,10.);
#17433=VECTOR('',#64467,10.);
#17434=VECTOR('',#64468,10.);
#17435=VECTOR('',#64469,10.);
#17436=VECTOR('',#64470,10.);
#17437=VECTOR('',#64471,10.);
#17438=VECTOR('',#64472,10.);
#17439=VECTOR('',#64473,10.);
#17440=VECTOR('',#64474,10.);
#17441=VECTOR('',#64475,10.);
#17442=VECTOR('',#64476,10.);
#17443=VECTOR('',#64477,10.);
#17444=VECTOR('',#64478,10.);
#17445=VECTOR('',#64479,10.);
#17446=VECTOR('',#64480,10.);
#17447=VECTOR('',#64481,10.);
#17448=VECTOR('',#64484,10.);
#17449=VECTOR('',#64485,10.);
#17450=VECTOR('',#64486,10.);
#17451=VECTOR('',#64487,10.);
#17452=VECTOR('',#64488,10.);
#17453=VECTOR('',#64489,10.);
#17454=VECTOR('',#64490,10.);
#17455=VECTOR('',#64491,10.);
#17456=VECTOR('',#64492,10.);
#17457=VECTOR('',#64493,10.);
#17458=VECTOR('',#64496,10.);
#17459=VECTOR('',#64497,10.);
#17460=VECTOR('',#64498,10.);
#17461=VECTOR('',#64499,10.);
#17462=VECTOR('',#64500,10.);
#17463=VECTOR('',#64501,10.);
#17464=VECTOR('',#64502,10.);
#17465=VECTOR('',#64503,10.);
#17466=VECTOR('',#64504,10.);
#17467=VECTOR('',#64505,10.);
#17468=VECTOR('',#64506,10.);
#17469=VECTOR('',#64507,10.);
#17470=VECTOR('',#64510,10.);
#17471=VECTOR('',#64511,10.);
#17472=VECTOR('',#64512,10.);
#17473=VECTOR('',#64515,10.);
#17474=VECTOR('',#64516,10.);
#17475=VECTOR('',#64517,10.);
#17476=VECTOR('',#64520,10.);
#17477=VECTOR('',#64521,10.);
#17478=VECTOR('',#64526,10.);
#17479=VECTOR('',#64527,10.);
#17480=VECTOR('',#64528,10.);
#17481=VECTOR('',#64529,10.);
#17482=VECTOR('',#64530,10.);
#17483=VECTOR('',#64531,10.);
#17484=VECTOR('',#64532,10.);
#17485=VECTOR('',#64533,10.);
#17486=VECTOR('',#64534,10.);
#17487=VECTOR('',#64535,10.);
#17488=VECTOR('',#64536,10.);
#17489=VECTOR('',#64537,10.);
#17490=VECTOR('',#64538,10.);
#17491=VECTOR('',#64539,10.);
#17492=VECTOR('',#64540,10.);
#17493=VECTOR('',#64541,10.);
#17494=VECTOR('',#64542,10.);
#17495=VECTOR('',#64543,10.);
#17496=VECTOR('',#64544,10.);
#17497=VECTOR('',#64545,10.);
#17498=VECTOR('',#64548,10.);
#17499=VECTOR('',#64549,10.);
#17500=VECTOR('',#64550,10.);
#17501=VECTOR('',#64551,10.);
#17502=VECTOR('',#64552,10.);
#17503=VECTOR('',#64553,10.);
#17504=VECTOR('',#64554,10.);
#17505=VECTOR('',#64555,10.);
#17506=VECTOR('',#64556,10.);
#17507=VECTOR('',#64557,10.);
#17508=VECTOR('',#64558,10.);
#17509=VECTOR('',#64559,10.);
#17510=VECTOR('',#64560,10.);
#17511=VECTOR('',#64563,10.);
#17512=VECTOR('',#64564,10.);
#17513=VECTOR('',#64565,10.);
#17514=VECTOR('',#64566,10.);
#17515=VECTOR('',#64567,10.);
#17516=VECTOR('',#64568,10.);
#17517=VECTOR('',#64569,10.);
#17518=VECTOR('',#64570,10.);
#17519=VECTOR('',#64571,10.);
#17520=VECTOR('',#64572,10.);
#17521=VECTOR('',#64575,10.);
#17522=VECTOR('',#64576,10.);
#17523=VECTOR('',#64577,10.);
#17524=VECTOR('',#64578,10.);
#17525=VECTOR('',#64579,10.);
#17526=VECTOR('',#64580,10.);
#17527=VECTOR('',#64581,10.);
#17528=VECTOR('',#64582,10.);
#17529=VECTOR('',#64583,10.);
#17530=VECTOR('',#64584,10.);
#17531=VECTOR('',#64587,10.);
#17532=VECTOR('',#64588,10.);
#17533=VECTOR('',#64589,10.);
#17534=VECTOR('',#64594,10.);
#17535=VECTOR('',#64595,10.);
#17536=VECTOR('',#64596,10.);
#17537=VECTOR('',#64597,10.);
#17538=VECTOR('',#64598,10.);
#17539=VECTOR('',#64599,10.);
#17540=VECTOR('',#64600,10.);
#17541=VECTOR('',#64601,10.);
#17542=VECTOR('',#64602,10.);
#17543=VECTOR('',#64603,10.);
#17544=VECTOR('',#64604,10.);
#17545=VECTOR('',#64605,10.);
#17546=VECTOR('',#64606,10.);
#17547=VECTOR('',#64607,10.);
#17548=VECTOR('',#64608,10.);
#17549=VECTOR('',#64609,10.);
#17550=VECTOR('',#64610,10.);
#17551=VECTOR('',#64611,10.);
#17552=VECTOR('',#64612,10.);
#17553=VECTOR('',#64613,10.);
#17554=VECTOR('',#64618,10.);
#17555=VECTOR('',#64619,10.);
#17556=VECTOR('',#64620,10.);
#17557=VECTOR('',#64621,10.);
#17558=VECTOR('',#64624,10.);
#17559=VECTOR('',#64625,10.);
#17560=VECTOR('',#64626,10.);
#17561=VECTOR('',#64629,10.);
#17562=VECTOR('',#64630,10.);
#17563=VECTOR('',#64633,10.);
#17564=VECTOR('',#64634,10.);
#17565=VECTOR('',#64635,10.);
#17566=VECTOR('',#64636,10.);
#17567=VECTOR('',#64639,10.);
#17568=VECTOR('',#64640,10.);
#17569=VECTOR('',#64641,10.);
#17570=VECTOR('',#64644,10.);
#17571=VECTOR('',#64645,10.);
#17572=VECTOR('',#64646,10.);
#17573=VECTOR('',#64649,10.);
#17574=VECTOR('',#64650,10.);
#17575=VECTOR('',#64651,10.);
#17576=VECTOR('',#64654,10.);
#17577=VECTOR('',#64655,10.);
#17578=VECTOR('',#64656,10.);
#17579=VECTOR('',#64659,10.);
#17580=VECTOR('',#64660,10.);
#17581=VECTOR('',#64661,10.);
#17582=VECTOR('',#64664,10.);
#17583=VECTOR('',#64665,10.);
#17584=VECTOR('',#64666,10.);
#17585=VECTOR('',#64669,10.);
#17586=VECTOR('',#64670,10.);
#17587=VECTOR('',#64671,10.);
#17588=VECTOR('',#64674,10.);
#17589=VECTOR('',#64675,10.);
#17590=VECTOR('',#64676,10.);
#17591=VECTOR('',#64679,10.);
#17592=VECTOR('',#64680,10.);
#17593=VECTOR('',#64681,10.);
#17594=VECTOR('',#64684,10.);
#17595=VECTOR('',#64685,10.);
#17596=VECTOR('',#64692,10.);
#17597=VECTOR('',#64693,10.);
#17598=VECTOR('',#64694,10.);
#17599=VECTOR('',#64695,10.);
#17600=VECTOR('',#64696,10.);
#17601=VECTOR('',#64697,10.);
#17602=VECTOR('',#64698,10.);
#17603=VECTOR('',#64699,10.);
#17604=VECTOR('',#64700,10.);
#17605=VECTOR('',#64701,10.);
#17606=VECTOR('',#64702,10.);
#17607=VECTOR('',#64703,10.);
#17608=VECTOR('',#64704,10.);
#17609=VECTOR('',#64705,10.);
#17610=VECTOR('',#64706,10.);
#17611=VECTOR('',#64707,10.);
#17612=VECTOR('',#64708,10.);
#17613=VECTOR('',#64709,10.);
#17614=VECTOR('',#64710,10.);
#17615=VECTOR('',#64711,10.);
#17616=VECTOR('',#64714,10.);
#17617=VECTOR('',#64715,10.);
#17618=VECTOR('',#64716,10.);
#17619=VECTOR('',#64717,10.);
#17620=VECTOR('',#64718,10.);
#17621=VECTOR('',#64719,10.);
#17622=VECTOR('',#64720,10.);
#17623=VECTOR('',#64723,10.);
#17624=VECTOR('',#64724,10.);
#17625=VECTOR('',#64725,10.);
#17626=VECTOR('',#64728,10.);
#17627=VECTOR('',#64729,10.);
#17628=VECTOR('',#64730,10.);
#17629=VECTOR('',#64733,10.);
#17630=VECTOR('',#64734,10.);
#17631=VECTOR('',#64735,10.);
#17632=VECTOR('',#64738,10.);
#17633=VECTOR('',#64739,10.);
#17634=VECTOR('',#64740,10.);
#17635=VECTOR('',#64743,10.);
#17636=VECTOR('',#64744,10.);
#17637=VECTOR('',#64745,10.);
#17638=VECTOR('',#64748,10.);
#17639=VECTOR('',#64749,10.);
#17640=VECTOR('',#64750,10.);
#17641=VECTOR('',#64751,10.);
#17642=VECTOR('',#64752,10.);
#17643=VECTOR('',#64753,10.);
#17644=VECTOR('',#64754,10.);
#17645=VECTOR('',#64755,10.);
#17646=VECTOR('',#64756,10.);
#17647=VECTOR('',#64757,10.);
#17648=VECTOR('',#64758,10.);
#17649=VECTOR('',#64761,10.);
#17650=VECTOR('',#64762,10.);
#17651=VECTOR('',#64763,10.);
#17652=VECTOR('',#64768,10.);
#17653=VECTOR('',#64769,10.);
#17654=VECTOR('',#64770,10.);
#17655=VECTOR('',#64771,10.);
#17656=VECTOR('',#64772,10.);
#17657=VECTOR('',#64773,10.);
#17658=VECTOR('',#64774,10.);
#17659=VECTOR('',#64775,10.);
#17660=VECTOR('',#64776,10.);
#17661=VECTOR('',#64777,10.);
#17662=VECTOR('',#64778,10.);
#17663=VECTOR('',#64779,10.);
#17664=VECTOR('',#64780,10.);
#17665=VECTOR('',#64781,10.);
#17666=VECTOR('',#64782,10.);
#17667=VECTOR('',#64783,10.);
#17668=VECTOR('',#64784,10.);
#17669=VECTOR('',#64785,10.);
#17670=VECTOR('',#64786,10.);
#17671=VECTOR('',#64787,10.);
#17672=VECTOR('',#64790,10.);
#17673=VECTOR('',#64791,10.);
#17674=VECTOR('',#64792,10.);
#17675=VECTOR('',#64793,10.);
#17676=VECTOR('',#64794,10.);
#17677=VECTOR('',#64795,10.);
#17678=VECTOR('',#64796,10.);
#17679=VECTOR('',#64797,10.);
#17680=VECTOR('',#64798,10.);
#17681=VECTOR('',#64799,10.);
#17682=VECTOR('',#64800,10.);
#17683=VECTOR('',#64801,10.);
#17684=VECTOR('',#64802,10.);
#17685=VECTOR('',#64803,10.);
#17686=VECTOR('',#64804,10.);
#17687=VECTOR('',#64805,10.);
#17688=VECTOR('',#64806,10.);
#17689=VECTOR('',#64807,10.);
#17690=VECTOR('',#64808,10.);
#17691=VECTOR('',#64809,10.);
#17692=VECTOR('',#64810,10.);
#17693=VECTOR('',#64811,10.);
#17694=VECTOR('',#64812,10.);
#17695=VECTOR('',#64813,10.);
#17696=VECTOR('',#64814,10.);
#17697=VECTOR('',#64815,10.);
#17698=VECTOR('',#64816,10.);
#17699=VECTOR('',#64819,10.);
#17700=VECTOR('',#64820,10.);
#17701=VECTOR('',#64821,10.);
#17702=VECTOR('',#64828,10.);
#17703=VECTOR('',#64829,10.);
#17704=VECTOR('',#64830,10.);
#17705=VECTOR('',#64831,10.);
#17706=VECTOR('',#64832,10.);
#17707=VECTOR('',#64833,10.);
#17708=VECTOR('',#64834,10.);
#17709=VECTOR('',#64835,10.);
#17710=VECTOR('',#64836,10.);
#17711=VECTOR('',#64837,10.);
#17712=VECTOR('',#64838,10.);
#17713=VECTOR('',#64839,10.);
#17714=VECTOR('',#64840,10.);
#17715=VECTOR('',#64841,10.);
#17716=VECTOR('',#64842,10.);
#17717=VECTOR('',#64843,10.);
#17718=VECTOR('',#64844,10.);
#17719=VECTOR('',#64845,10.);
#17720=VECTOR('',#64846,10.);
#17721=VECTOR('',#64847,10.);
#17722=VECTOR('',#64850,10.);
#17723=VECTOR('',#64851,10.);
#17724=VECTOR('',#64852,10.);
#17725=VECTOR('',#64853,10.);
#17726=VECTOR('',#64856,10.);
#17727=VECTOR('',#64857,10.);
#17728=VECTOR('',#64858,10.);
#17729=VECTOR('',#64859,10.);
#17730=VECTOR('',#64860,10.);
#17731=VECTOR('',#64861,10.);
#17732=VECTOR('',#64864,10.);
#17733=VECTOR('',#64865,10.);
#17734=VECTOR('',#64866,10.);
#17735=VECTOR('',#64869,10.);
#17736=VECTOR('',#64870,10.);
#17737=VECTOR('',#64871,10.);
#17738=VECTOR('',#64874,10.);
#17739=VECTOR('',#64875,10.);
#17740=VECTOR('',#64876,10.);
#17741=VECTOR('',#64879,10.);
#17742=VECTOR('',#64880,10.);
#17743=VECTOR('',#64885,10.);
#17744=VECTOR('',#64886,10.);
#17745=VECTOR('',#64887,10.);
#17746=VECTOR('',#64888,10.);
#17747=VECTOR('',#64889,10.);
#17748=VECTOR('',#64890,10.);
#17749=VECTOR('',#64891,10.);
#17750=VECTOR('',#64892,10.);
#17751=VECTOR('',#64893,10.);
#17752=VECTOR('',#64894,10.);
#17753=VECTOR('',#64895,10.);
#17754=VECTOR('',#64896,10.);
#17755=VECTOR('',#64897,10.);
#17756=VECTOR('',#64898,10.);
#17757=VECTOR('',#64899,10.);
#17758=VECTOR('',#64900,10.);
#17759=VECTOR('',#64901,10.);
#17760=VECTOR('',#64902,10.);
#17761=VECTOR('',#64903,10.);
#17762=VECTOR('',#64904,10.);
#17763=VECTOR('',#64907,10.);
#17764=VECTOR('',#64908,10.);
#17765=VECTOR('',#64909,10.);
#17766=VECTOR('',#64910,10.);
#17767=VECTOR('',#64911,10.);
#17768=VECTOR('',#64912,10.);
#17769=VECTOR('',#64913,10.);
#17770=VECTOR('',#64914,10.);
#17771=VECTOR('',#64915,10.);
#17772=VECTOR('',#64916,10.);
#17773=VECTOR('',#64917,10.);
#17774=VECTOR('',#64918,10.);
#17775=VECTOR('',#64919,10.);
#17776=VECTOR('',#64920,10.);
#17777=VECTOR('',#64921,10.);
#17778=VECTOR('',#64922,10.);
#17779=VECTOR('',#64923,10.);
#17780=VECTOR('',#64924,10.);
#17781=VECTOR('',#64925,10.);
#17782=VECTOR('',#64926,10.);
#17783=VECTOR('',#64927,10.);
#17784=VECTOR('',#64928,10.);
#17785=VECTOR('',#64929,10.);
#17786=VECTOR('',#64930,10.);
#17787=VECTOR('',#64931,10.);
#17788=VECTOR('',#64932,10.);
#17789=VECTOR('',#64933,10.);
#17790=VECTOR('',#64934,10.);
#17791=VECTOR('',#64935,10.);
#17792=VECTOR('',#64936,10.);
#17793=VECTOR('',#64937,10.);
#17794=VECTOR('',#64938,10.);
#17795=VECTOR('',#64939,10.);
#17796=VECTOR('',#64948,10.);
#17797=VECTOR('',#64949,10.);
#17798=VECTOR('',#64950,10.);
#17799=VECTOR('',#64951,10.);
#17800=VECTOR('',#64952,10.);
#17801=VECTOR('',#64953,10.);
#17802=VECTOR('',#64954,10.);
#17803=VECTOR('',#64955,10.);
#17804=VECTOR('',#64956,10.);
#17805=VECTOR('',#64957,10.);
#17806=VECTOR('',#64958,10.);
#17807=VECTOR('',#64959,10.);
#17808=VECTOR('',#64960,10.);
#17809=VECTOR('',#64961,10.);
#17810=VECTOR('',#64962,10.);
#17811=VECTOR('',#64963,10.);
#17812=VECTOR('',#64964,10.);
#17813=VECTOR('',#64965,10.);
#17814=VECTOR('',#64966,10.);
#17815=VECTOR('',#64967,10.);
#17816=VECTOR('',#64970,10.);
#17817=VECTOR('',#64971,10.);
#17818=VECTOR('',#64972,10.);
#17819=VECTOR('',#64973,10.);
#17820=VECTOR('',#64974,10.);
#17821=VECTOR('',#64975,10.);
#17822=VECTOR('',#64976,10.);
#17823=VECTOR('',#64977,10.);
#17824=VECTOR('',#64978,10.);
#17825=VECTOR('',#64979,10.);
#17826=VECTOR('',#64980,10.);
#17827=VECTOR('',#64981,10.);
#17828=VECTOR('',#64982,10.);
#17829=VECTOR('',#64983,10.);
#17830=VECTOR('',#64984,10.);
#17831=VECTOR('',#64985,10.);
#17832=VECTOR('',#64986,10.);
#17833=VECTOR('',#64987,10.);
#17834=VECTOR('',#64988,10.);
#17835=VECTOR('',#64989,10.);
#17836=VECTOR('',#64990,10.);
#17837=VECTOR('',#64991,10.);
#17838=VECTOR('',#64992,10.);
#17839=VECTOR('',#64993,10.);
#17840=VECTOR('',#64994,10.);
#17841=VECTOR('',#64995,10.);
#17842=VECTOR('',#64996,10.);
#17843=VECTOR('',#64997,10.);
#17844=VECTOR('',#64998,10.);
#17845=VECTOR('',#65001,10.);
#17846=VECTOR('',#65002,10.);
#17847=VECTOR('',#65003,10.);
#17848=VECTOR('',#65012,10.);
#17849=VECTOR('',#65013,10.);
#17850=VECTOR('',#65014,10.);
#17851=VECTOR('',#65015,10.);
#17852=VECTOR('',#65018,10.);
#17853=VECTOR('',#65019,10.);
#17854=VECTOR('',#65020,10.);
#17855=VECTOR('',#65023,10.);
#17856=VECTOR('',#65024,10.);
#17857=VECTOR('',#65025,10.);
#17858=VECTOR('',#65028,10.);
#17859=VECTOR('',#65029,10.);
#17860=VECTOR('',#65034,10.);
#17861=VECTOR('',#65035,10.);
#17862=VECTOR('',#65036,10.);
#17863=VECTOR('',#65037,10.);
#17864=VECTOR('',#65040,10.);
#17865=VECTOR('',#65041,10.);
#17866=VECTOR('',#65042,10.);
#17867=VECTOR('',#65045,10.);
#17868=VECTOR('',#65046,10.);
#17869=VECTOR('',#65047,10.);
#17870=VECTOR('',#65050,10.);
#17871=VECTOR('',#65051,10.);
#17872=VECTOR('',#65056,10.);
#17873=VECTOR('',#65057,10.);
#17874=VECTOR('',#65058,10.);
#17875=VECTOR('',#65059,10.);
#17876=VECTOR('',#65062,10.);
#17877=VECTOR('',#65063,10.);
#17878=VECTOR('',#65064,10.);
#17879=VECTOR('',#65067,10.);
#17880=VECTOR('',#65068,10.);
#17881=VECTOR('',#65069,10.);
#17882=VECTOR('',#65072,10.);
#17883=VECTOR('',#65073,10.);
#17884=VECTOR('',#65078,10.);
#17885=VECTOR('',#65079,10.);
#17886=VECTOR('',#65080,10.);
#17887=VECTOR('',#65081,10.);
#17888=VECTOR('',#65084,10.);
#17889=VECTOR('',#65085,10.);
#17890=VECTOR('',#65086,10.);
#17891=VECTOR('',#65089,10.);
#17892=VECTOR('',#65090,10.);
#17893=VECTOR('',#65091,10.);
#17894=VECTOR('',#65094,10.);
#17895=VECTOR('',#65095,10.);
#17896=VECTOR('',#65100,10.);
#17897=VECTOR('',#65101,10.);
#17898=VECTOR('',#65102,10.);
#17899=VECTOR('',#65103,10.);
#17900=VECTOR('',#65106,10.);
#17901=VECTOR('',#65107,10.);
#17902=VECTOR('',#65108,10.);
#17903=VECTOR('',#65111,10.);
#17904=VECTOR('',#65112,10.);
#17905=VECTOR('',#65113,10.);
#17906=VECTOR('',#65116,10.);
#17907=VECTOR('',#65117,10.);
#17908=VECTOR('',#65122,10.);
#17909=VECTOR('',#65123,10.);
#17910=VECTOR('',#65124,10.);
#17911=VECTOR('',#65125,10.);
#17912=VECTOR('',#65128,10.);
#17913=VECTOR('',#65129,10.);
#17914=VECTOR('',#65130,10.);
#17915=VECTOR('',#65133,10.);
#17916=VECTOR('',#65134,10.);
#17917=VECTOR('',#65135,10.);
#17918=VECTOR('',#65138,10.);
#17919=VECTOR('',#65139,10.);
#17920=VECTOR('',#65144,10.);
#17921=VECTOR('',#65145,10.);
#17922=VECTOR('',#65146,10.);
#17923=VECTOR('',#65147,10.);
#17924=VECTOR('',#65150,10.);
#17925=VECTOR('',#65151,10.);
#17926=VECTOR('',#65152,10.);
#17927=VECTOR('',#65155,10.);
#17928=VECTOR('',#65156,10.);
#17929=VECTOR('',#65157,10.);
#17930=VECTOR('',#65160,10.);
#17931=VECTOR('',#65161,10.);
#17932=VECTOR('',#65166,10.);
#17933=VECTOR('',#65167,10.);
#17934=VECTOR('',#65168,10.);
#17935=VECTOR('',#65169,10.);
#17936=VECTOR('',#65172,10.);
#17937=VECTOR('',#65173,10.);
#17938=VECTOR('',#65174,10.);
#17939=VECTOR('',#65177,10.);
#17940=VECTOR('',#65178,10.);
#17941=VECTOR('',#65179,10.);
#17942=VECTOR('',#65182,10.);
#17943=VECTOR('',#65183,10.);
#17944=VECTOR('',#65188,10.);
#17945=VECTOR('',#65189,10.);
#17946=VECTOR('',#65190,10.);
#17947=VECTOR('',#65191,10.);
#17948=VECTOR('',#65194,10.);
#17949=VECTOR('',#65195,10.);
#17950=VECTOR('',#65196,10.);
#17951=VECTOR('',#65199,10.);
#17952=VECTOR('',#65200,10.);
#17953=VECTOR('',#65201,10.);
#17954=VECTOR('',#65204,10.);
#17955=VECTOR('',#65205,10.);
#17956=VECTOR('',#65210,10.);
#17957=VECTOR('',#65211,10.);
#17958=VECTOR('',#65212,10.);
#17959=VECTOR('',#65213,10.);
#17960=VECTOR('',#65216,10.);
#17961=VECTOR('',#65217,10.);
#17962=VECTOR('',#65218,10.);
#17963=VECTOR('',#65221,10.);
#17964=VECTOR('',#65222,10.);
#17965=VECTOR('',#65223,10.);
#17966=VECTOR('',#65226,10.);
#17967=VECTOR('',#65227,10.);
#17968=VECTOR('',#65232,10.);
#17969=VECTOR('',#65233,10.);
#17970=VECTOR('',#65234,10.);
#17971=VECTOR('',#65235,10.);
#17972=VECTOR('',#65238,10.);
#17973=VECTOR('',#65239,10.);
#17974=VECTOR('',#65240,10.);
#17975=VECTOR('',#65243,10.);
#17976=VECTOR('',#65244,10.);
#17977=VECTOR('',#65245,10.);
#17978=VECTOR('',#65248,10.);
#17979=VECTOR('',#65249,10.);
#17980=VECTOR('',#65254,10.);
#17981=VECTOR('',#65255,10.);
#17982=VECTOR('',#65256,10.);
#17983=VECTOR('',#65257,10.);
#17984=VECTOR('',#65260,10.);
#17985=VECTOR('',#65261,10.);
#17986=VECTOR('',#65262,10.);
#17987=VECTOR('',#65265,10.);
#17988=VECTOR('',#65266,10.);
#17989=VECTOR('',#65267,10.);
#17990=VECTOR('',#65270,10.);
#17991=VECTOR('',#65271,10.);
#17992=VECTOR('',#65276,10.);
#17993=VECTOR('',#65277,10.);
#17994=VECTOR('',#65278,10.);
#17995=VECTOR('',#65279,10.);
#17996=VECTOR('',#65282,10.);
#17997=VECTOR('',#65283,10.);
#17998=VECTOR('',#65284,10.);
#17999=VECTOR('',#65287,10.);
#18000=VECTOR('',#65288,10.);
#18001=VECTOR('',#65289,10.);
#18002=VECTOR('',#65292,10.);
#18003=VECTOR('',#65293,10.);
#18004=VECTOR('',#65298,10.);
#18005=VECTOR('',#65299,10.);
#18006=VECTOR('',#65300,10.);
#18007=VECTOR('',#65301,10.);
#18008=VECTOR('',#65304,10.);
#18009=VECTOR('',#65305,10.);
#18010=VECTOR('',#65306,10.);
#18011=VECTOR('',#65309,10.);
#18012=VECTOR('',#65310,10.);
#18013=VECTOR('',#65311,10.);
#18014=VECTOR('',#65314,10.);
#18015=VECTOR('',#65315,10.);
#18016=VECTOR('',#65320,10.);
#18017=VECTOR('',#65321,10.);
#18018=VECTOR('',#65322,10.);
#18019=VECTOR('',#65323,10.);
#18020=VECTOR('',#65326,10.);
#18021=VECTOR('',#65327,10.);
#18022=VECTOR('',#65328,10.);
#18023=VECTOR('',#65331,10.);
#18024=VECTOR('',#65332,10.);
#18025=VECTOR('',#65333,10.);
#18026=VECTOR('',#65336,10.);
#18027=VECTOR('',#65337,10.);
#18028=VECTOR('',#65342,10.);
#18029=VECTOR('',#65343,10.);
#18030=VECTOR('',#65344,10.);
#18031=VECTOR('',#65345,10.);
#18032=VECTOR('',#65348,10.);
#18033=VECTOR('',#65349,10.);
#18034=VECTOR('',#65350,10.);
#18035=VECTOR('',#65353,10.);
#18036=VECTOR('',#65354,10.);
#18037=VECTOR('',#65355,10.);
#18038=VECTOR('',#65358,10.);
#18039=VECTOR('',#65359,10.);
#18040=VECTOR('',#65364,10.);
#18041=VECTOR('',#65365,10.);
#18042=VECTOR('',#65366,10.);
#18043=VECTOR('',#65367,10.);
#18044=VECTOR('',#65370,10.);
#18045=VECTOR('',#65371,10.);
#18046=VECTOR('',#65372,10.);
#18047=VECTOR('',#65375,10.);
#18048=VECTOR('',#65376,10.);
#18049=VECTOR('',#65377,10.);
#18050=VECTOR('',#65380,10.);
#18051=VECTOR('',#65381,10.);
#18052=VECTOR('',#65386,10.);
#18053=VECTOR('',#65387,10.);
#18054=VECTOR('',#65388,10.);
#18055=VECTOR('',#65389,10.);
#18056=VECTOR('',#65392,10.);
#18057=VECTOR('',#65393,10.);
#18058=VECTOR('',#65394,10.);
#18059=VECTOR('',#65397,10.);
#18060=VECTOR('',#65398,10.);
#18061=VECTOR('',#65399,10.);
#18062=VECTOR('',#65402,10.);
#18063=VECTOR('',#65403,10.);
#18064=VECTOR('',#65408,10.);
#18065=VECTOR('',#65409,10.);
#18066=VECTOR('',#65410,10.);
#18067=VECTOR('',#65411,10.);
#18068=VECTOR('',#65414,10.);
#18069=VECTOR('',#65415,10.);
#18070=VECTOR('',#65416,10.);
#18071=VECTOR('',#65419,10.);
#18072=VECTOR('',#65420,10.);
#18073=VECTOR('',#65421,10.);
#18074=VECTOR('',#65424,10.);
#18075=VECTOR('',#65425,10.);
#18076=VECTOR('',#65430,10.);
#18077=VECTOR('',#65431,10.);
#18078=VECTOR('',#65432,10.);
#18079=VECTOR('',#65433,10.);
#18080=VECTOR('',#65436,10.);
#18081=VECTOR('',#65437,10.);
#18082=VECTOR('',#65438,10.);
#18083=VECTOR('',#65441,10.);
#18084=VECTOR('',#65442,10.);
#18085=VECTOR('',#65443,10.);
#18086=VECTOR('',#65446,10.);
#18087=VECTOR('',#65447,10.);
#18088=VECTOR('',#65452,10.);
#18089=VECTOR('',#65453,10.);
#18090=VECTOR('',#65454,10.);
#18091=VECTOR('',#65455,10.);
#18092=VECTOR('',#65458,10.);
#18093=VECTOR('',#65459,10.);
#18094=VECTOR('',#65460,10.);
#18095=VECTOR('',#65463,10.);
#18096=VECTOR('',#65464,10.);
#18097=VECTOR('',#65465,10.);
#18098=VECTOR('',#65468,10.);
#18099=VECTOR('',#65469,10.);
#18100=VECTOR('',#65474,10.);
#18101=VECTOR('',#65475,10.);
#18102=VECTOR('',#65476,10.);
#18103=VECTOR('',#65477,10.);
#18104=VECTOR('',#65480,10.);
#18105=VECTOR('',#65481,10.);
#18106=VECTOR('',#65482,10.);
#18107=VECTOR('',#65485,10.);
#18108=VECTOR('',#65486,10.);
#18109=VECTOR('',#65487,10.);
#18110=VECTOR('',#65490,10.);
#18111=VECTOR('',#65491,10.);
#18112=VECTOR('',#65496,10.);
#18113=VECTOR('',#65497,10.);
#18114=VECTOR('',#65498,10.);
#18115=VECTOR('',#65499,10.);
#18116=VECTOR('',#65502,10.);
#18117=VECTOR('',#65503,10.);
#18118=VECTOR('',#65504,10.);
#18119=VECTOR('',#65507,10.);
#18120=VECTOR('',#65508,10.);
#18121=VECTOR('',#65509,10.);
#18122=VECTOR('',#65512,10.);
#18123=VECTOR('',#65513,10.);
#18124=VECTOR('',#65518,10.);
#18125=VECTOR('',#65519,10.);
#18126=VECTOR('',#65520,10.);
#18127=VECTOR('',#65521,10.);
#18128=VECTOR('',#65524,10.);
#18129=VECTOR('',#65525,10.);
#18130=VECTOR('',#65526,10.);
#18131=VECTOR('',#65529,10.);
#18132=VECTOR('',#65530,10.);
#18133=VECTOR('',#65531,10.);
#18134=VECTOR('',#65534,10.);
#18135=VECTOR('',#65535,10.);
#18136=VECTOR('',#65540,10.);
#18137=VECTOR('',#65541,10.);
#18138=VECTOR('',#65542,10.);
#18139=VECTOR('',#65543,10.);
#18140=VECTOR('',#65546,10.);
#18141=VECTOR('',#65547,10.);
#18142=VECTOR('',#65548,10.);
#18143=VECTOR('',#65551,10.);
#18144=VECTOR('',#65552,10.);
#18145=VECTOR('',#65553,10.);
#18146=VECTOR('',#65556,10.);
#18147=VECTOR('',#65557,10.);
#18148=VECTOR('',#65562,10.);
#18149=VECTOR('',#65563,10.);
#18150=VECTOR('',#65564,10.);
#18151=VECTOR('',#65565,10.);
#18152=VECTOR('',#65568,10.);
#18153=VECTOR('',#65569,10.);
#18154=VECTOR('',#65570,10.);
#18155=VECTOR('',#65573,10.);
#18156=VECTOR('',#65574,10.);
#18157=VECTOR('',#65575,10.);
#18158=VECTOR('',#65578,10.);
#18159=VECTOR('',#65579,10.);
#18160=VECTOR('',#65584,10.);
#18161=VECTOR('',#65585,10.);
#18162=VECTOR('',#65586,10.);
#18163=VECTOR('',#65587,10.);
#18164=VECTOR('',#65590,10.);
#18165=VECTOR('',#65591,10.);
#18166=VECTOR('',#65592,10.);
#18167=VECTOR('',#65595,10.);
#18168=VECTOR('',#65596,10.);
#18169=VECTOR('',#65597,10.);
#18170=VECTOR('',#65600,10.);
#18171=VECTOR('',#65601,10.);
#18172=VECTOR('',#65606,10.);
#18173=VECTOR('',#65607,10.);
#18174=VECTOR('',#65608,10.);
#18175=VECTOR('',#65609,10.);
#18176=VECTOR('',#65612,10.);
#18177=VECTOR('',#65613,10.);
#18178=VECTOR('',#65614,10.);
#18179=VECTOR('',#65617,10.);
#18180=VECTOR('',#65618,10.);
#18181=VECTOR('',#65619,10.);
#18182=VECTOR('',#65622,10.);
#18183=VECTOR('',#65623,10.);
#18184=VECTOR('',#65628,10.);
#18185=VECTOR('',#65629,10.);
#18186=VECTOR('',#65630,10.);
#18187=VECTOR('',#65631,10.);
#18188=VECTOR('',#65634,10.);
#18189=VECTOR('',#65635,10.);
#18190=VECTOR('',#65636,10.);
#18191=VECTOR('',#65639,10.);
#18192=VECTOR('',#65640,10.);
#18193=VECTOR('',#65641,10.);
#18194=VECTOR('',#65644,10.);
#18195=VECTOR('',#65645,10.);
#18196=VECTOR('',#65650,10.);
#18197=VECTOR('',#65651,10.);
#18198=VECTOR('',#65652,10.);
#18199=VECTOR('',#65653,10.);
#18200=VECTOR('',#65656,10.);
#18201=VECTOR('',#65657,10.);
#18202=VECTOR('',#65658,10.);
#18203=VECTOR('',#65661,10.);
#18204=VECTOR('',#65662,10.);
#18205=VECTOR('',#65663,10.);
#18206=VECTOR('',#65666,10.);
#18207=VECTOR('',#65667,10.);
#18208=VECTOR('',#65672,10.);
#18209=VECTOR('',#65673,10.);
#18210=VECTOR('',#65674,10.);
#18211=VECTOR('',#65675,10.);
#18212=VECTOR('',#65678,10.);
#18213=VECTOR('',#65679,10.);
#18214=VECTOR('',#65680,10.);
#18215=VECTOR('',#65683,10.);
#18216=VECTOR('',#65684,10.);
#18217=VECTOR('',#65685,10.);
#18218=VECTOR('',#65688,10.);
#18219=VECTOR('',#65689,10.);
#18220=VECTOR('',#65694,10.);
#18221=VECTOR('',#65695,10.);
#18222=VECTOR('',#65696,10.);
#18223=VECTOR('',#65697,10.);
#18224=VECTOR('',#65700,10.);
#18225=VECTOR('',#65701,10.);
#18226=VECTOR('',#65702,10.);
#18227=VECTOR('',#65705,10.);
#18228=VECTOR('',#65706,10.);
#18229=VECTOR('',#65707,10.);
#18230=VECTOR('',#65710,10.);
#18231=VECTOR('',#65711,10.);
#18232=VECTOR('',#65716,10.);
#18233=VECTOR('',#65717,10.);
#18234=VECTOR('',#65718,10.);
#18235=VECTOR('',#65719,10.);
#18236=VECTOR('',#65722,10.);
#18237=VECTOR('',#65723,10.);
#18238=VECTOR('',#65724,10.);
#18239=VECTOR('',#65727,10.);
#18240=VECTOR('',#65728,10.);
#18241=VECTOR('',#65729,10.);
#18242=VECTOR('',#65732,10.);
#18243=VECTOR('',#65733,10.);
#18244=VECTOR('',#65738,10.);
#18245=VECTOR('',#65739,10.);
#18246=VECTOR('',#65740,10.);
#18247=VECTOR('',#65741,10.);
#18248=VECTOR('',#65744,10.);
#18249=VECTOR('',#65745,10.);
#18250=VECTOR('',#65746,10.);
#18251=VECTOR('',#65749,10.);
#18252=VECTOR('',#65750,10.);
#18253=VECTOR('',#65751,10.);
#18254=VECTOR('',#65754,10.);
#18255=VECTOR('',#65755,10.);
#18256=VECTOR('',#65760,10.);
#18257=VECTOR('',#65761,10.);
#18258=VECTOR('',#65762,10.);
#18259=VECTOR('',#65763,10.);
#18260=VECTOR('',#65766,10.);
#18261=VECTOR('',#65767,10.);
#18262=VECTOR('',#65768,10.);
#18263=VECTOR('',#65771,10.);
#18264=VECTOR('',#65772,10.);
#18265=VECTOR('',#65773,10.);
#18266=VECTOR('',#65776,10.);
#18267=VECTOR('',#65777,10.);
#18268=VECTOR('',#65782,10.);
#18269=VECTOR('',#65783,10.);
#18270=VECTOR('',#65784,10.);
#18271=VECTOR('',#65785,10.);
#18272=VECTOR('',#65788,10.);
#18273=VECTOR('',#65789,10.);
#18274=VECTOR('',#65790,10.);
#18275=VECTOR('',#65793,10.);
#18276=VECTOR('',#65794,10.);
#18277=VECTOR('',#65795,10.);
#18278=VECTOR('',#65798,10.);
#18279=VECTOR('',#65799,10.);
#18280=VECTOR('',#65804,10.);
#18281=VECTOR('',#65805,10.);
#18282=VECTOR('',#65806,10.);
#18283=VECTOR('',#65807,10.);
#18284=VECTOR('',#65810,10.);
#18285=VECTOR('',#65811,10.);
#18286=VECTOR('',#65812,10.);
#18287=VECTOR('',#65815,10.);
#18288=VECTOR('',#65816,10.);
#18289=VECTOR('',#65817,10.);
#18290=VECTOR('',#65820,10.);
#18291=VECTOR('',#65821,10.);
#18292=VECTOR('',#65826,10.);
#18293=VECTOR('',#65827,10.);
#18294=VECTOR('',#65828,10.);
#18295=VECTOR('',#65829,10.);
#18296=VECTOR('',#65832,10.);
#18297=VECTOR('',#65833,10.);
#18298=VECTOR('',#65834,10.);
#18299=VECTOR('',#65837,10.);
#18300=VECTOR('',#65838,10.);
#18301=VECTOR('',#65839,10.);
#18302=VECTOR('',#65842,10.);
#18303=VECTOR('',#65843,10.);
#18304=VECTOR('',#65848,10.);
#18305=VECTOR('',#65849,10.);
#18306=VECTOR('',#65850,10.);
#18307=VECTOR('',#65851,10.);
#18308=VECTOR('',#65854,10.);
#18309=VECTOR('',#65855,10.);
#18310=VECTOR('',#65856,10.);
#18311=VECTOR('',#65859,10.);
#18312=VECTOR('',#65860,10.);
#18313=VECTOR('',#65861,10.);
#18314=VECTOR('',#65864,10.);
#18315=VECTOR('',#65865,10.);
#18316=VECTOR('',#65870,10.);
#18317=VECTOR('',#65871,10.);
#18318=VECTOR('',#65872,10.);
#18319=VECTOR('',#65873,10.);
#18320=VECTOR('',#65876,10.);
#18321=VECTOR('',#65877,10.);
#18322=VECTOR('',#65878,10.);
#18323=VECTOR('',#65881,10.);
#18324=VECTOR('',#65882,10.);
#18325=VECTOR('',#65883,10.);
#18326=VECTOR('',#65886,10.);
#18327=VECTOR('',#65887,10.);
#18328=VECTOR('',#65892,10.);
#18329=VECTOR('',#65893,10.);
#18330=VECTOR('',#65894,10.);
#18331=VECTOR('',#65895,10.);
#18332=VECTOR('',#65898,10.);
#18333=VECTOR('',#65899,10.);
#18334=VECTOR('',#65900,10.);
#18335=VECTOR('',#65903,10.);
#18336=VECTOR('',#65904,10.);
#18337=VECTOR('',#65905,10.);
#18338=VECTOR('',#65908,10.);
#18339=VECTOR('',#65909,10.);
#18340=VECTOR('',#65914,10.);
#18341=VECTOR('',#65915,10.);
#18342=VECTOR('',#65916,10.);
#18343=VECTOR('',#65917,10.);
#18344=VECTOR('',#65920,10.);
#18345=VECTOR('',#65921,10.);
#18346=VECTOR('',#65922,10.);
#18347=VECTOR('',#65925,10.);
#18348=VECTOR('',#65926,10.);
#18349=VECTOR('',#65927,10.);
#18350=VECTOR('',#65930,10.);
#18351=VECTOR('',#65931,10.);
#18352=VECTOR('',#65936,10.);
#18353=VECTOR('',#65937,10.);
#18354=VECTOR('',#65938,10.);
#18355=VECTOR('',#65939,10.);
#18356=VECTOR('',#65942,10.);
#18357=VECTOR('',#65943,10.);
#18358=VECTOR('',#65944,10.);
#18359=VECTOR('',#65947,10.);
#18360=VECTOR('',#65948,10.);
#18361=VECTOR('',#65949,10.);
#18362=VECTOR('',#65952,10.);
#18363=VECTOR('',#65953,10.);
#18364=VECTOR('',#65958,10.);
#18365=VECTOR('',#65959,10.);
#18366=VECTOR('',#65960,10.);
#18367=VECTOR('',#65961,10.);
#18368=VECTOR('',#65964,10.);
#18369=VECTOR('',#65965,10.);
#18370=VECTOR('',#65966,10.);
#18371=VECTOR('',#65969,10.);
#18372=VECTOR('',#65970,10.);
#18373=VECTOR('',#65971,10.);
#18374=VECTOR('',#65974,10.);
#18375=VECTOR('',#65975,10.);
#18376=VECTOR('',#65980,10.);
#18377=VECTOR('',#65981,10.);
#18378=VECTOR('',#65982,10.);
#18379=VECTOR('',#65983,10.);
#18380=VECTOR('',#65986,10.);
#18381=VECTOR('',#65987,10.);
#18382=VECTOR('',#65988,10.);
#18383=VECTOR('',#65991,10.);
#18384=VECTOR('',#65992,10.);
#18385=VECTOR('',#65993,10.);
#18386=VECTOR('',#65996,10.);
#18387=VECTOR('',#65997,10.);
#18388=VECTOR('',#66002,10.);
#18389=VECTOR('',#66003,10.);
#18390=VECTOR('',#66004,10.);
#18391=VECTOR('',#66005,10.);
#18392=VECTOR('',#66008,10.);
#18393=VECTOR('',#66009,10.);
#18394=VECTOR('',#66010,10.);
#18395=VECTOR('',#66013,10.);
#18396=VECTOR('',#66014,10.);
#18397=VECTOR('',#66015,10.);
#18398=VECTOR('',#66018,10.);
#18399=VECTOR('',#66019,10.);
#18400=VECTOR('',#66024,10.);
#18401=VECTOR('',#66025,10.);
#18402=VECTOR('',#66026,10.);
#18403=VECTOR('',#66027,10.);
#18404=VECTOR('',#66030,10.);
#18405=VECTOR('',#66031,10.);
#18406=VECTOR('',#66032,10.);
#18407=VECTOR('',#66035,10.);
#18408=VECTOR('',#66036,10.);
#18409=VECTOR('',#66037,10.);
#18410=VECTOR('',#66040,10.);
#18411=VECTOR('',#66041,10.);
#18412=VECTOR('',#66046,10.);
#18413=VECTOR('',#66047,10.);
#18414=VECTOR('',#66048,10.);
#18415=VECTOR('',#66049,10.);
#18416=VECTOR('',#66052,10.);
#18417=VECTOR('',#66053,10.);
#18418=VECTOR('',#66054,10.);
#18419=VECTOR('',#66057,10.);
#18420=VECTOR('',#66058,10.);
#18421=VECTOR('',#66059,10.);
#18422=VECTOR('',#66062,10.);
#18423=VECTOR('',#66063,10.);
#18424=VECTOR('',#66068,10.);
#18425=VECTOR('',#66069,10.);
#18426=VECTOR('',#66070,10.);
#18427=VECTOR('',#66071,10.);
#18428=VECTOR('',#66074,10.);
#18429=VECTOR('',#66075,10.);
#18430=VECTOR('',#66076,10.);
#18431=VECTOR('',#66079,10.);
#18432=VECTOR('',#66080,10.);
#18433=VECTOR('',#66081,10.);
#18434=VECTOR('',#66084,10.);
#18435=VECTOR('',#66085,10.);
#18436=VECTOR('',#66090,10.);
#18437=VECTOR('',#66091,10.);
#18438=VECTOR('',#66092,10.);
#18439=VECTOR('',#66093,10.);
#18440=VECTOR('',#66096,10.);
#18441=VECTOR('',#66097,10.);
#18442=VECTOR('',#66098,10.);
#18443=VECTOR('',#66101,10.);
#18444=VECTOR('',#66102,10.);
#18445=VECTOR('',#66103,10.);
#18446=VECTOR('',#66106,10.);
#18447=VECTOR('',#66107,10.);
#18448=VECTOR('',#66112,10.);
#18449=VECTOR('',#66113,10.);
#18450=VECTOR('',#66114,10.);
#18451=VECTOR('',#66115,10.);
#18452=VECTOR('',#66118,10.);
#18453=VECTOR('',#66119,10.);
#18454=VECTOR('',#66120,10.);
#18455=VECTOR('',#66123,10.);
#18456=VECTOR('',#66124,10.);
#18457=VECTOR('',#66125,10.);
#18458=VECTOR('',#66128,10.);
#18459=VECTOR('',#66129,10.);
#18460=VECTOR('',#66134,10.);
#18461=VECTOR('',#66135,10.);
#18462=VECTOR('',#66136,10.);
#18463=VECTOR('',#66137,10.);
#18464=VECTOR('',#66140,10.);
#18465=VECTOR('',#66141,10.);
#18466=VECTOR('',#66142,10.);
#18467=VECTOR('',#66145,10.);
#18468=VECTOR('',#66146,10.);
#18469=VECTOR('',#66147,10.);
#18470=VECTOR('',#66150,10.);
#18471=VECTOR('',#66151,10.);
#18472=VECTOR('',#66156,10.);
#18473=VECTOR('',#66157,10.);
#18474=VECTOR('',#66158,10.);
#18475=VECTOR('',#66159,10.);
#18476=VECTOR('',#66162,10.);
#18477=VECTOR('',#66163,10.);
#18478=VECTOR('',#66164,10.);
#18479=VECTOR('',#66167,10.);
#18480=VECTOR('',#66168,10.);
#18481=VECTOR('',#66169,10.);
#18482=VECTOR('',#66172,10.);
#18483=VECTOR('',#66173,10.);
#18484=VECTOR('',#66178,10.);
#18485=VECTOR('',#66179,10.);
#18486=VECTOR('',#66180,10.);
#18487=VECTOR('',#66181,10.);
#18488=VECTOR('',#66184,10.);
#18489=VECTOR('',#66185,10.);
#18490=VECTOR('',#66186,10.);
#18491=VECTOR('',#66189,10.);
#18492=VECTOR('',#66190,10.);
#18493=VECTOR('',#66191,10.);
#18494=VECTOR('',#66194,10.);
#18495=VECTOR('',#66195,10.);
#18496=VECTOR('',#66200,10.);
#18497=VECTOR('',#66201,10.);
#18498=VECTOR('',#66202,10.);
#18499=VECTOR('',#66203,10.);
#18500=VECTOR('',#66206,10.);
#18501=VECTOR('',#66207,10.);
#18502=VECTOR('',#66208,10.);
#18503=VECTOR('',#66211,10.);
#18504=VECTOR('',#66212,10.);
#18505=VECTOR('',#66213,10.);
#18506=VECTOR('',#66216,10.);
#18507=VECTOR('',#66217,10.);
#18508=VECTOR('',#66222,10.);
#18509=VECTOR('',#66223,10.);
#18510=VECTOR('',#66224,10.);
#18511=VECTOR('',#66225,10.);
#18512=VECTOR('',#66228,10.);
#18513=VECTOR('',#66229,10.);
#18514=VECTOR('',#66230,10.);
#18515=VECTOR('',#66233,10.);
#18516=VECTOR('',#66234,10.);
#18517=VECTOR('',#66235,10.);
#18518=VECTOR('',#66238,10.);
#18519=VECTOR('',#66239,10.);
#18520=VECTOR('',#66244,10.);
#18521=VECTOR('',#66245,10.);
#18522=VECTOR('',#66246,10.);
#18523=VECTOR('',#66247,10.);
#18524=VECTOR('',#66250,10.);
#18525=VECTOR('',#66251,10.);
#18526=VECTOR('',#66252,10.);
#18527=VECTOR('',#66255,10.);
#18528=VECTOR('',#66256,10.);
#18529=VECTOR('',#66257,10.);
#18530=VECTOR('',#66260,10.);
#18531=VECTOR('',#66261,10.);
#18532=VECTOR('',#66266,10.);
#18533=VECTOR('',#66267,10.);
#18534=VECTOR('',#66268,10.);
#18535=VECTOR('',#66269,10.);
#18536=VECTOR('',#66272,10.);
#18537=VECTOR('',#66273,10.);
#18538=VECTOR('',#66274,10.);
#18539=VECTOR('',#66277,10.);
#18540=VECTOR('',#66278,10.);
#18541=VECTOR('',#66279,10.);
#18542=VECTOR('',#66282,10.);
#18543=VECTOR('',#66283,10.);
#18544=VECTOR('',#66288,10.);
#18545=VECTOR('',#66289,10.);
#18546=VECTOR('',#66290,10.);
#18547=VECTOR('',#66291,10.);
#18548=VECTOR('',#66294,10.);
#18549=VECTOR('',#66295,10.);
#18550=VECTOR('',#66296,10.);
#18551=VECTOR('',#66299,10.);
#18552=VECTOR('',#66300,10.);
#18553=VECTOR('',#66301,10.);
#18554=VECTOR('',#66304,10.);
#18555=VECTOR('',#66305,10.);
#18556=VECTOR('',#66310,10.);
#18557=VECTOR('',#66311,10.);
#18558=VECTOR('',#66312,10.);
#18559=VECTOR('',#66313,10.);
#18560=VECTOR('',#66316,10.);
#18561=VECTOR('',#66317,10.);
#18562=VECTOR('',#66318,10.);
#18563=VECTOR('',#66321,10.);
#18564=VECTOR('',#66322,10.);
#18565=VECTOR('',#66323,10.);
#18566=VECTOR('',#66326,10.);
#18567=VECTOR('',#66327,10.);
#18568=VECTOR('',#66332,10.);
#18569=VECTOR('',#66333,10.);
#18570=VECTOR('',#66334,10.);
#18571=VECTOR('',#66335,10.);
#18572=VECTOR('',#66338,10.);
#18573=VECTOR('',#66339,10.);
#18574=VECTOR('',#66340,10.);
#18575=VECTOR('',#66343,10.);
#18576=VECTOR('',#66344,10.);
#18577=VECTOR('',#66345,10.);
#18578=VECTOR('',#66348,10.);
#18579=VECTOR('',#66349,10.);
#18580=VECTOR('',#66354,10.);
#18581=VECTOR('',#66355,10.);
#18582=VECTOR('',#66356,10.);
#18583=VECTOR('',#66357,10.);
#18584=VECTOR('',#66360,10.);
#18585=VECTOR('',#66361,10.);
#18586=VECTOR('',#66362,10.);
#18587=VECTOR('',#66365,10.);
#18588=VECTOR('',#66366,10.);
#18589=VECTOR('',#66367,10.);
#18590=VECTOR('',#66370,10.);
#18591=VECTOR('',#66371,10.);
#18592=VECTOR('',#66376,10.);
#18593=VECTOR('',#66377,10.);
#18594=VECTOR('',#66378,10.);
#18595=VECTOR('',#66379,10.);
#18596=VECTOR('',#66382,10.);
#18597=VECTOR('',#66383,10.);
#18598=VECTOR('',#66384,10.);
#18599=VECTOR('',#66387,10.);
#18600=VECTOR('',#66388,10.);
#18601=VECTOR('',#66389,10.);
#18602=VECTOR('',#66392,10.);
#18603=VECTOR('',#66393,10.);
#18604=VECTOR('',#66398,10.);
#18605=VECTOR('',#66399,10.);
#18606=VECTOR('',#66400,10.);
#18607=VECTOR('',#66401,10.);
#18608=VECTOR('',#66404,10.);
#18609=VECTOR('',#66405,10.);
#18610=VECTOR('',#66406,10.);
#18611=VECTOR('',#66409,10.);
#18612=VECTOR('',#66410,10.);
#18613=VECTOR('',#66411,10.);
#18614=VECTOR('',#66414,10.);
#18615=VECTOR('',#66415,10.);
#18616=VECTOR('',#66420,10.);
#18617=VECTOR('',#66421,10.);
#18618=VECTOR('',#66422,10.);
#18619=VECTOR('',#66423,10.);
#18620=VECTOR('',#66426,10.);
#18621=VECTOR('',#66427,10.);
#18622=VECTOR('',#66428,10.);
#18623=VECTOR('',#66431,10.);
#18624=VECTOR('',#66432,10.);
#18625=VECTOR('',#66433,10.);
#18626=VECTOR('',#66436,10.);
#18627=VECTOR('',#66437,10.);
#18628=VECTOR('',#66442,10.);
#18629=VECTOR('',#66443,10.);
#18630=VECTOR('',#66444,10.);
#18631=VECTOR('',#66445,10.);
#18632=VECTOR('',#66448,10.);
#18633=VECTOR('',#66449,10.);
#18634=VECTOR('',#66450,10.);
#18635=VECTOR('',#66453,10.);
#18636=VECTOR('',#66454,10.);
#18637=VECTOR('',#66455,10.);
#18638=VECTOR('',#66458,10.);
#18639=VECTOR('',#66459,10.);
#18640=VECTOR('',#66464,10.);
#18641=VECTOR('',#66465,10.);
#18642=VECTOR('',#66466,10.);
#18643=VECTOR('',#66467,10.);
#18644=VECTOR('',#66470,10.);
#18645=VECTOR('',#66471,10.);
#18646=VECTOR('',#66472,10.);
#18647=VECTOR('',#66475,10.);
#18648=VECTOR('',#66476,10.);
#18649=VECTOR('',#66477,10.);
#18650=VECTOR('',#66480,10.);
#18651=VECTOR('',#66481,10.);
#18652=VECTOR('',#66486,10.);
#18653=VECTOR('',#66487,10.);
#18654=VECTOR('',#66488,10.);
#18655=VECTOR('',#66489,10.);
#18656=VECTOR('',#66492,10.);
#18657=VECTOR('',#66493,10.);
#18658=VECTOR('',#66494,10.);
#18659=VECTOR('',#66497,10.);
#18660=VECTOR('',#66498,10.);
#18661=VECTOR('',#66499,10.);
#18662=VECTOR('',#66502,10.);
#18663=VECTOR('',#66503,10.);
#18664=VECTOR('',#66508,10.);
#18665=VECTOR('',#66509,10.);
#18666=VECTOR('',#66510,10.);
#18667=VECTOR('',#66511,10.);
#18668=VECTOR('',#66514,10.);
#18669=VECTOR('',#66515,10.);
#18670=VECTOR('',#66516,10.);
#18671=VECTOR('',#66519,10.);
#18672=VECTOR('',#66520,10.);
#18673=VECTOR('',#66521,10.);
#18674=VECTOR('',#66524,10.);
#18675=VECTOR('',#66525,10.);
#18676=VECTOR('',#66530,10.);
#18677=VECTOR('',#66531,10.);
#18678=VECTOR('',#66532,10.);
#18679=VECTOR('',#66533,10.);
#18680=VECTOR('',#66536,10.);
#18681=VECTOR('',#66537,10.);
#18682=VECTOR('',#66538,10.);
#18683=VECTOR('',#66541,10.);
#18684=VECTOR('',#66542,10.);
#18685=VECTOR('',#66543,10.);
#18686=VECTOR('',#66546,10.);
#18687=VECTOR('',#66547,10.);
#18688=VECTOR('',#66552,10.);
#18689=VECTOR('',#66553,10.);
#18690=VECTOR('',#66554,10.);
#18691=VECTOR('',#66555,10.);
#18692=VECTOR('',#66558,10.);
#18693=VECTOR('',#66559,10.);
#18694=VECTOR('',#66560,10.);
#18695=VECTOR('',#66563,10.);
#18696=VECTOR('',#66564,10.);
#18697=VECTOR('',#66565,10.);
#18698=VECTOR('',#66568,10.);
#18699=VECTOR('',#66569,10.);
#18700=VECTOR('',#66574,10.);
#18701=VECTOR('',#66575,10.);
#18702=VECTOR('',#66576,10.);
#18703=VECTOR('',#66577,10.);
#18704=VECTOR('',#66580,10.);
#18705=VECTOR('',#66581,10.);
#18706=VECTOR('',#66582,10.);
#18707=VECTOR('',#66585,10.);
#18708=VECTOR('',#66586,10.);
#18709=VECTOR('',#66587,10.);
#18710=VECTOR('',#66590,10.);
#18711=VECTOR('',#66591,10.);
#18712=VECTOR('',#66596,10.);
#18713=VECTOR('',#66597,10.);
#18714=VECTOR('',#66598,10.);
#18715=VECTOR('',#66599,10.);
#18716=VECTOR('',#66602,10.);
#18717=VECTOR('',#66603,10.);
#18718=VECTOR('',#66604,10.);
#18719=VECTOR('',#66607,10.);
#18720=VECTOR('',#66608,10.);
#18721=VECTOR('',#66609,10.);
#18722=VECTOR('',#66612,10.);
#18723=VECTOR('',#66613,10.);
#18724=VECTOR('',#66618,10.);
#18725=VECTOR('',#66619,10.);
#18726=VECTOR('',#66620,10.);
#18727=VECTOR('',#66621,10.);
#18728=VECTOR('',#66624,10.);
#18729=VECTOR('',#66625,10.);
#18730=VECTOR('',#66626,10.);
#18731=VECTOR('',#66629,10.);
#18732=VECTOR('',#66630,10.);
#18733=VECTOR('',#66631,10.);
#18734=VECTOR('',#66634,10.);
#18735=VECTOR('',#66635,10.);
#18736=VECTOR('',#66640,10.);
#18737=VECTOR('',#66641,10.);
#18738=VECTOR('',#66642,10.);
#18739=VECTOR('',#66643,10.);
#18740=VECTOR('',#66646,10.);
#18741=VECTOR('',#66647,10.);
#18742=VECTOR('',#66648,10.);
#18743=VECTOR('',#66651,10.);
#18744=VECTOR('',#66652,10.);
#18745=VECTOR('',#66653,10.);
#18746=VECTOR('',#66656,10.);
#18747=VECTOR('',#66657,10.);
#18748=VECTOR('',#66662,10.);
#18749=VECTOR('',#66663,10.);
#18750=VECTOR('',#66664,10.);
#18751=VECTOR('',#66665,10.);
#18752=VECTOR('',#66668,10.);
#18753=VECTOR('',#66669,10.);
#18754=VECTOR('',#66670,10.);
#18755=VECTOR('',#66673,10.);
#18756=VECTOR('',#66674,10.);
#18757=VECTOR('',#66675,10.);
#18758=VECTOR('',#66678,10.);
#18759=VECTOR('',#66679,10.);
#18760=VECTOR('',#66684,10.);
#18761=VECTOR('',#66685,10.);
#18762=VECTOR('',#66686,10.);
#18763=VECTOR('',#66687,10.);
#18764=VECTOR('',#66690,10.);
#18765=VECTOR('',#66691,10.);
#18766=VECTOR('',#66692,10.);
#18767=VECTOR('',#66695,10.);
#18768=VECTOR('',#66696,10.);
#18769=VECTOR('',#66697,10.);
#18770=VECTOR('',#66700,10.);
#18771=VECTOR('',#66701,10.);
#18772=VECTOR('',#66706,10.);
#18773=VECTOR('',#66707,10.);
#18774=VECTOR('',#66708,10.);
#18775=VECTOR('',#66709,10.);
#18776=VECTOR('',#66712,10.);
#18777=VECTOR('',#66713,10.);
#18778=VECTOR('',#66714,10.);
#18779=VECTOR('',#66717,10.);
#18780=VECTOR('',#66718,10.);
#18781=VECTOR('',#66719,10.);
#18782=VECTOR('',#66722,10.);
#18783=VECTOR('',#66723,10.);
#18784=VECTOR('',#66728,10.);
#18785=VECTOR('',#66729,10.);
#18786=VECTOR('',#66730,10.);
#18787=VECTOR('',#66731,10.);
#18788=VECTOR('',#66734,10.);
#18789=VECTOR('',#66735,10.);
#18790=VECTOR('',#66736,10.);
#18791=VECTOR('',#66739,10.);
#18792=VECTOR('',#66740,10.);
#18793=VECTOR('',#66741,10.);
#18794=VECTOR('',#66744,10.);
#18795=VECTOR('',#66745,10.);
#18796=VECTOR('',#66750,10.);
#18797=VECTOR('',#66751,10.);
#18798=VECTOR('',#66752,10.);
#18799=VECTOR('',#66753,10.);
#18800=VECTOR('',#66756,10.);
#18801=VECTOR('',#66757,10.);
#18802=VECTOR('',#66758,10.);
#18803=VECTOR('',#66761,10.);
#18804=VECTOR('',#66762,10.);
#18805=VECTOR('',#66763,10.);
#18806=VECTOR('',#66766,10.);
#18807=VECTOR('',#66767,10.);
#18808=VECTOR('',#66772,10.);
#18809=VECTOR('',#66773,10.);
#18810=VECTOR('',#66774,10.);
#18811=VECTOR('',#66775,10.);
#18812=VECTOR('',#66778,10.);
#18813=VECTOR('',#66779,10.);
#18814=VECTOR('',#66780,10.);
#18815=VECTOR('',#66783,10.);
#18816=VECTOR('',#66784,10.);
#18817=VECTOR('',#66785,10.);
#18818=VECTOR('',#66788,10.);
#18819=VECTOR('',#66789,10.);
#18820=VECTOR('',#66794,10.);
#18821=VECTOR('',#66795,10.);
#18822=VECTOR('',#66796,10.);
#18823=VECTOR('',#66797,10.);
#18824=VECTOR('',#66800,10.);
#18825=VECTOR('',#66801,10.);
#18826=VECTOR('',#66802,10.);
#18827=VECTOR('',#66805,10.);
#18828=VECTOR('',#66806,10.);
#18829=VECTOR('',#66807,10.);
#18830=VECTOR('',#66810,10.);
#18831=VECTOR('',#66811,10.);
#18832=VECTOR('',#66816,10.);
#18833=VECTOR('',#66817,10.);
#18834=VECTOR('',#66818,10.);
#18835=VECTOR('',#66819,10.);
#18836=VECTOR('',#66822,10.);
#18837=VECTOR('',#66823,10.);
#18838=VECTOR('',#66824,10.);
#18839=VECTOR('',#66827,10.);
#18840=VECTOR('',#66828,10.);
#18841=VECTOR('',#66829,10.);
#18842=VECTOR('',#66832,10.);
#18843=VECTOR('',#66833,10.);
#18844=VECTOR('',#66838,10.);
#18845=VECTOR('',#66839,10.);
#18846=VECTOR('',#66840,10.);
#18847=VECTOR('',#66841,10.);
#18848=VECTOR('',#66844,10.);
#18849=VECTOR('',#66845,10.);
#18850=VECTOR('',#66846,10.);
#18851=VECTOR('',#66849,10.);
#18852=VECTOR('',#66850,10.);
#18853=VECTOR('',#66851,10.);
#18854=VECTOR('',#66854,10.);
#18855=VECTOR('',#66855,10.);
#18856=VECTOR('',#66860,10.);
#18857=VECTOR('',#66861,10.);
#18858=VECTOR('',#66862,10.);
#18859=VECTOR('',#66863,10.);
#18860=VECTOR('',#66866,10.);
#18861=VECTOR('',#66867,10.);
#18862=VECTOR('',#66868,10.);
#18863=VECTOR('',#66871,10.);
#18864=VECTOR('',#66872,10.);
#18865=VECTOR('',#66873,10.);
#18866=VECTOR('',#66876,10.);
#18867=VECTOR('',#66877,10.);
#18868=VECTOR('',#66882,10.);
#18869=VECTOR('',#66883,10.);
#18870=VECTOR('',#66884,10.);
#18871=VECTOR('',#66885,10.);
#18872=VECTOR('',#66888,10.);
#18873=VECTOR('',#66889,10.);
#18874=VECTOR('',#66890,10.);
#18875=VECTOR('',#66893,10.);
#18876=VECTOR('',#66894,10.);
#18877=VECTOR('',#66895,10.);
#18878=VECTOR('',#66898,10.);
#18879=VECTOR('',#66899,10.);
#18880=VECTOR('',#66904,10.);
#18881=VECTOR('',#66905,10.);
#18882=VECTOR('',#66906,10.);
#18883=VECTOR('',#66907,10.);
#18884=VECTOR('',#66910,10.);
#18885=VECTOR('',#66911,10.);
#18886=VECTOR('',#66912,10.);
#18887=VECTOR('',#66915,10.);
#18888=VECTOR('',#66916,10.);
#18889=VECTOR('',#66917,10.);
#18890=VECTOR('',#66920,10.);
#18891=VECTOR('',#66921,10.);
#18892=VECTOR('',#66926,10.);
#18893=VECTOR('',#66927,10.);
#18894=VECTOR('',#66928,10.);
#18895=VECTOR('',#66929,10.);
#18896=VECTOR('',#66932,10.);
#18897=VECTOR('',#66933,10.);
#18898=VECTOR('',#66934,10.);
#18899=VECTOR('',#66937,10.);
#18900=VECTOR('',#66938,10.);
#18901=VECTOR('',#66939,10.);
#18902=VECTOR('',#66942,10.);
#18903=VECTOR('',#66943,10.);
#18904=VECTOR('',#66948,10.);
#18905=VECTOR('',#66949,10.);
#18906=VECTOR('',#66950,10.);
#18907=VECTOR('',#66951,10.);
#18908=VECTOR('',#66954,10.);
#18909=VECTOR('',#66955,10.);
#18910=VECTOR('',#66956,10.);
#18911=VECTOR('',#66959,10.);
#18912=VECTOR('',#66960,10.);
#18913=VECTOR('',#66961,10.);
#18914=VECTOR('',#66964,10.);
#18915=VECTOR('',#66965,10.);
#18916=VECTOR('',#66970,10.);
#18917=VECTOR('',#66971,10.);
#18918=VECTOR('',#66972,10.);
#18919=VECTOR('',#66973,10.);
#18920=VECTOR('',#66976,10.);
#18921=VECTOR('',#66977,10.);
#18922=VECTOR('',#66978,10.);
#18923=VECTOR('',#66981,10.);
#18924=VECTOR('',#66982,10.);
#18925=VECTOR('',#66983,10.);
#18926=VECTOR('',#66986,10.);
#18927=VECTOR('',#66987,10.);
#18928=VECTOR('',#66992,10.);
#18929=VECTOR('',#66993,10.);
#18930=VECTOR('',#66994,10.);
#18931=VECTOR('',#66995,10.);
#18932=VECTOR('',#66998,10.);
#18933=VECTOR('',#66999,10.);
#18934=VECTOR('',#67000,10.);
#18935=VECTOR('',#67003,10.);
#18936=VECTOR('',#67004,10.);
#18937=VECTOR('',#67005,10.);
#18938=VECTOR('',#67008,10.);
#18939=VECTOR('',#67009,10.);
#18940=VECTOR('',#67014,10.);
#18941=VECTOR('',#67015,10.);
#18942=VECTOR('',#67016,10.);
#18943=VECTOR('',#67017,10.);
#18944=VECTOR('',#67020,10.);
#18945=VECTOR('',#67021,10.);
#18946=VECTOR('',#67022,10.);
#18947=VECTOR('',#67025,10.);
#18948=VECTOR('',#67026,10.);
#18949=VECTOR('',#67027,10.);
#18950=VECTOR('',#67030,10.);
#18951=VECTOR('',#67031,10.);
#18952=VECTOR('',#67036,10.);
#18953=VECTOR('',#67037,10.);
#18954=VECTOR('',#67038,10.);
#18955=VECTOR('',#67039,10.);
#18956=VECTOR('',#67042,10.);
#18957=VECTOR('',#67043,10.);
#18958=VECTOR('',#67044,10.);
#18959=VECTOR('',#67047,10.);
#18960=VECTOR('',#67048,10.);
#18961=VECTOR('',#67049,10.);
#18962=VECTOR('',#67052,10.);
#18963=VECTOR('',#67053,10.);
#18964=VECTOR('',#67058,10.);
#18965=VECTOR('',#67059,10.);
#18966=VECTOR('',#67060,10.);
#18967=VECTOR('',#67061,10.);
#18968=VECTOR('',#67064,10.);
#18969=VECTOR('',#67065,10.);
#18970=VECTOR('',#67066,10.);
#18971=VECTOR('',#67069,10.);
#18972=VECTOR('',#67070,10.);
#18973=VECTOR('',#67071,10.);
#18974=VECTOR('',#67074,10.);
#18975=VECTOR('',#67075,10.);
#18976=VECTOR('',#67080,10.);
#18977=VECTOR('',#67081,10.);
#18978=VECTOR('',#67082,10.);
#18979=VECTOR('',#67083,10.);
#18980=VECTOR('',#67086,10.);
#18981=VECTOR('',#67087,10.);
#18982=VECTOR('',#67088,10.);
#18983=VECTOR('',#67091,10.);
#18984=VECTOR('',#67092,10.);
#18985=VECTOR('',#67093,10.);
#18986=VECTOR('',#67096,10.);
#18987=VECTOR('',#67097,10.);
#18988=VECTOR('',#67102,10.);
#18989=VECTOR('',#67103,10.);
#18990=VECTOR('',#67104,10.);
#18991=VECTOR('',#67105,10.);
#18992=VECTOR('',#67108,10.);
#18993=VECTOR('',#67109,10.);
#18994=VECTOR('',#67110,10.);
#18995=VECTOR('',#67113,10.);
#18996=VECTOR('',#67114,10.);
#18997=VECTOR('',#67115,10.);
#18998=VECTOR('',#67118,10.);
#18999=VECTOR('',#67119,10.);
#19000=VECTOR('',#67124,10.);
#19001=VECTOR('',#67125,10.);
#19002=VECTOR('',#67126,10.);
#19003=VECTOR('',#67127,10.);
#19004=VECTOR('',#67130,10.);
#19005=VECTOR('',#67131,10.);
#19006=VECTOR('',#67132,10.);
#19007=VECTOR('',#67135,10.);
#19008=VECTOR('',#67136,10.);
#19009=VECTOR('',#67137,10.);
#19010=VECTOR('',#67140,10.);
#19011=VECTOR('',#67141,10.);
#19012=VECTOR('',#67146,10.);
#19013=VECTOR('',#67147,10.);
#19014=VECTOR('',#67148,10.);
#19015=VECTOR('',#67149,10.);
#19016=VECTOR('',#67152,10.);
#19017=VECTOR('',#67153,10.);
#19018=VECTOR('',#67154,10.);
#19019=VECTOR('',#67157,10.);
#19020=VECTOR('',#67158,10.);
#19021=VECTOR('',#67159,10.);
#19022=VECTOR('',#67162,10.);
#19023=VECTOR('',#67163,10.);
#19024=VECTOR('',#67168,10.);
#19025=VECTOR('',#67169,10.);
#19026=VECTOR('',#67170,10.);
#19027=VECTOR('',#67171,10.);
#19028=VECTOR('',#67174,10.);
#19029=VECTOR('',#67175,10.);
#19030=VECTOR('',#67176,10.);
#19031=VECTOR('',#67179,10.);
#19032=VECTOR('',#67180,10.);
#19033=VECTOR('',#67181,10.);
#19034=VECTOR('',#67184,10.);
#19035=VECTOR('',#67185,10.);
#19036=VECTOR('',#67190,10.);
#19037=VECTOR('',#67191,10.);
#19038=VECTOR('',#67192,10.);
#19039=VECTOR('',#67193,10.);
#19040=VECTOR('',#67196,10.);
#19041=VECTOR('',#67197,10.);
#19042=VECTOR('',#67198,10.);
#19043=VECTOR('',#67201,10.);
#19044=VECTOR('',#67202,10.);
#19045=VECTOR('',#67203,10.);
#19046=VECTOR('',#67206,10.);
#19047=VECTOR('',#67207,10.);
#19048=VECTOR('',#67212,10.);
#19049=VECTOR('',#67213,10.);
#19050=VECTOR('',#67214,10.);
#19051=VECTOR('',#67215,10.);
#19052=VECTOR('',#67218,10.);
#19053=VECTOR('',#67219,10.);
#19054=VECTOR('',#67220,10.);
#19055=VECTOR('',#67223,10.);
#19056=VECTOR('',#67224,10.);
#19057=VECTOR('',#67225,10.);
#19058=VECTOR('',#67228,10.);
#19059=VECTOR('',#67229,10.);
#19060=VECTOR('',#67234,10.);
#19061=VECTOR('',#67235,10.);
#19062=VECTOR('',#67236,10.);
#19063=VECTOR('',#67237,10.);
#19064=VECTOR('',#67240,10.);
#19065=VECTOR('',#67241,10.);
#19066=VECTOR('',#67242,10.);
#19067=VECTOR('',#67245,10.);
#19068=VECTOR('',#67246,10.);
#19069=VECTOR('',#67247,10.);
#19070=VECTOR('',#67250,10.);
#19071=VECTOR('',#67251,10.);
#19072=VECTOR('',#67256,10.);
#19073=VECTOR('',#67257,10.);
#19074=VECTOR('',#67258,10.);
#19075=VECTOR('',#67259,10.);
#19076=VECTOR('',#67262,10.);
#19077=VECTOR('',#67263,10.);
#19078=VECTOR('',#67264,10.);
#19079=VECTOR('',#67267,10.);
#19080=VECTOR('',#67268,10.);
#19081=VECTOR('',#67269,10.);
#19082=VECTOR('',#67272,10.);
#19083=VECTOR('',#67273,10.);
#19084=VECTOR('',#67278,10.);
#19085=VECTOR('',#67279,10.);
#19086=VECTOR('',#67280,10.);
#19087=VECTOR('',#67281,10.);
#19088=VECTOR('',#67284,10.);
#19089=VECTOR('',#67285,10.);
#19090=VECTOR('',#67286,10.);
#19091=VECTOR('',#67289,10.);
#19092=VECTOR('',#67290,10.);
#19093=VECTOR('',#67291,10.);
#19094=VECTOR('',#67294,10.);
#19095=VECTOR('',#67295,10.);
#19096=VECTOR('',#67300,10.);
#19097=VECTOR('',#67301,10.);
#19098=VECTOR('',#67302,10.);
#19099=VECTOR('',#67303,10.);
#19100=VECTOR('',#67306,10.);
#19101=VECTOR('',#67307,10.);
#19102=VECTOR('',#67308,10.);
#19103=VECTOR('',#67311,10.);
#19104=VECTOR('',#67312,10.);
#19105=VECTOR('',#67313,10.);
#19106=VECTOR('',#67316,10.);
#19107=VECTOR('',#67317,10.);
#19108=VECTOR('',#67322,10.);
#19109=VECTOR('',#67323,10.);
#19110=VECTOR('',#67324,10.);
#19111=VECTOR('',#67325,10.);
#19112=VECTOR('',#67328,10.);
#19113=VECTOR('',#67329,10.);
#19114=VECTOR('',#67330,10.);
#19115=VECTOR('',#67333,10.);
#19116=VECTOR('',#67334,10.);
#19117=VECTOR('',#67335,10.);
#19118=VECTOR('',#67338,10.);
#19119=VECTOR('',#67339,10.);
#19120=VECTOR('',#67344,10.);
#19121=VECTOR('',#67345,10.);
#19122=VECTOR('',#67346,10.);
#19123=VECTOR('',#67347,10.);
#19124=VECTOR('',#67350,10.);
#19125=VECTOR('',#67351,10.);
#19126=VECTOR('',#67352,10.);
#19127=VECTOR('',#67355,10.);
#19128=VECTOR('',#67356,10.);
#19129=VECTOR('',#67357,10.);
#19130=VECTOR('',#67360,10.);
#19131=VECTOR('',#67361,10.);
#19132=VECTOR('',#67366,10.);
#19133=VECTOR('',#67367,10.);
#19134=VECTOR('',#67368,10.);
#19135=VECTOR('',#67369,10.);
#19136=VECTOR('',#67372,10.);
#19137=VECTOR('',#67373,10.);
#19138=VECTOR('',#67374,10.);
#19139=VECTOR('',#67377,10.);
#19140=VECTOR('',#67378,10.);
#19141=VECTOR('',#67379,10.);
#19142=VECTOR('',#67382,10.);
#19143=VECTOR('',#67383,10.);
#19144=VECTOR('',#67388,10.);
#19145=VECTOR('',#67389,10.);
#19146=VECTOR('',#67390,10.);
#19147=VECTOR('',#67391,10.);
#19148=VECTOR('',#67394,10.);
#19149=VECTOR('',#67395,10.);
#19150=VECTOR('',#67396,10.);
#19151=VECTOR('',#67399,10.);
#19152=VECTOR('',#67400,10.);
#19153=VECTOR('',#67401,10.);
#19154=VECTOR('',#67404,10.);
#19155=VECTOR('',#67405,10.);
#19156=VECTOR('',#67410,10.);
#19157=VECTOR('',#67411,10.);
#19158=VECTOR('',#67412,10.);
#19159=VECTOR('',#67413,10.);
#19160=VECTOR('',#67416,10.);
#19161=VECTOR('',#67417,10.);
#19162=VECTOR('',#67418,10.);
#19163=VECTOR('',#67421,10.);
#19164=VECTOR('',#67422,10.);
#19165=VECTOR('',#67423,10.);
#19166=VECTOR('',#67426,10.);
#19167=VECTOR('',#67427,10.);
#19168=VECTOR('',#67432,10.);
#19169=VECTOR('',#67433,10.);
#19170=VECTOR('',#67434,10.);
#19171=VECTOR('',#67435,10.);
#19172=VECTOR('',#67438,10.);
#19173=VECTOR('',#67439,10.);
#19174=VECTOR('',#67440,10.);
#19175=VECTOR('',#67443,10.);
#19176=VECTOR('',#67444,10.);
#19177=VECTOR('',#67445,10.);
#19178=VECTOR('',#67448,10.);
#19179=VECTOR('',#67449,10.);
#19180=VECTOR('',#67454,10.);
#19181=VECTOR('',#67455,10.);
#19182=VECTOR('',#67456,10.);
#19183=VECTOR('',#67457,10.);
#19184=VECTOR('',#67460,10.);
#19185=VECTOR('',#67461,10.);
#19186=VECTOR('',#67462,10.);
#19187=VECTOR('',#67465,10.);
#19188=VECTOR('',#67466,10.);
#19189=VECTOR('',#67467,10.);
#19190=VECTOR('',#67470,10.);
#19191=VECTOR('',#67471,10.);
#19192=VECTOR('',#67476,10.);
#19193=VECTOR('',#67477,10.);
#19194=VECTOR('',#67478,10.);
#19195=VECTOR('',#67479,10.);
#19196=VECTOR('',#67482,10.);
#19197=VECTOR('',#67483,10.);
#19198=VECTOR('',#67484,10.);
#19199=VECTOR('',#67487,10.);
#19200=VECTOR('',#67488,10.);
#19201=VECTOR('',#67489,10.);
#19202=VECTOR('',#67492,10.);
#19203=VECTOR('',#67493,10.);
#19204=VECTOR('',#67498,10.);
#19205=VECTOR('',#67499,10.);
#19206=VECTOR('',#67500,10.);
#19207=VECTOR('',#67501,10.);
#19208=VECTOR('',#67504,10.);
#19209=VECTOR('',#67505,10.);
#19210=VECTOR('',#67506,10.);
#19211=VECTOR('',#67509,10.);
#19212=VECTOR('',#67510,10.);
#19213=VECTOR('',#67511,10.);
#19214=VECTOR('',#67514,10.);
#19215=VECTOR('',#67515,10.);
#19216=VECTOR('',#67520,10.);
#19217=VECTOR('',#67521,10.);
#19218=VECTOR('',#67522,10.);
#19219=VECTOR('',#67523,10.);
#19220=VECTOR('',#67526,10.);
#19221=VECTOR('',#67527,10.);
#19222=VECTOR('',#67528,10.);
#19223=VECTOR('',#67531,10.);
#19224=VECTOR('',#67532,10.);
#19225=VECTOR('',#67533,10.);
#19226=VECTOR('',#67536,10.);
#19227=VECTOR('',#67537,10.);
#19228=VECTOR('',#67542,10.);
#19229=VECTOR('',#67543,10.);
#19230=VECTOR('',#67544,10.);
#19231=VECTOR('',#67545,10.);
#19232=VECTOR('',#67548,10.);
#19233=VECTOR('',#67549,10.);
#19234=VECTOR('',#67550,10.);
#19235=VECTOR('',#67553,10.);
#19236=VECTOR('',#67554,10.);
#19237=VECTOR('',#67555,10.);
#19238=VECTOR('',#67558,10.);
#19239=VECTOR('',#67559,10.);
#19240=VECTOR('',#67564,10.);
#19241=VECTOR('',#67565,10.);
#19242=VECTOR('',#67566,10.);
#19243=VECTOR('',#67567,10.);
#19244=VECTOR('',#67570,10.);
#19245=VECTOR('',#67571,10.);
#19246=VECTOR('',#67572,10.);
#19247=VECTOR('',#67575,10.);
#19248=VECTOR('',#67576,10.);
#19249=VECTOR('',#67577,10.);
#19250=VECTOR('',#67580,10.);
#19251=VECTOR('',#67581,10.);
#19252=VECTOR('',#67586,10.);
#19253=VECTOR('',#67587,10.);
#19254=VECTOR('',#67588,10.);
#19255=VECTOR('',#67589,10.);
#19256=VECTOR('',#67592,10.);
#19257=VECTOR('',#67593,10.);
#19258=VECTOR('',#67594,10.);
#19259=VECTOR('',#67597,10.);
#19260=VECTOR('',#67598,10.);
#19261=VECTOR('',#67599,10.);
#19262=VECTOR('',#67602,10.);
#19263=VECTOR('',#67603,10.);
#19264=VECTOR('',#67608,10.);
#19265=VECTOR('',#67609,10.);
#19266=VECTOR('',#67610,10.);
#19267=VECTOR('',#67611,10.);
#19268=VECTOR('',#67614,10.);
#19269=VECTOR('',#67615,10.);
#19270=VECTOR('',#67616,10.);
#19271=VECTOR('',#67619,10.);
#19272=VECTOR('',#67620,10.);
#19273=VECTOR('',#67621,10.);
#19274=VECTOR('',#67624,10.);
#19275=VECTOR('',#67625,10.);
#19276=VECTOR('',#67630,10.);
#19277=VECTOR('',#67631,10.);
#19278=VECTOR('',#67632,10.);
#19279=VECTOR('',#67633,10.);
#19280=VECTOR('',#67636,10.);
#19281=VECTOR('',#67637,10.);
#19282=VECTOR('',#67638,10.);
#19283=VECTOR('',#67641,10.);
#19284=VECTOR('',#67642,10.);
#19285=VECTOR('',#67643,10.);
#19286=VECTOR('',#67646,10.);
#19287=VECTOR('',#67647,10.);
#19288=VECTOR('',#67652,10.);
#19289=VECTOR('',#67653,10.);
#19290=VECTOR('',#67654,10.);
#19291=VECTOR('',#67655,10.);
#19292=VECTOR('',#67658,10.);
#19293=VECTOR('',#67659,10.);
#19294=VECTOR('',#67660,10.);
#19295=VECTOR('',#67663,10.);
#19296=VECTOR('',#67664,10.);
#19297=VECTOR('',#67665,10.);
#19298=VECTOR('',#67668,10.);
#19299=VECTOR('',#67669,10.);
#19300=VECTOR('',#67674,10.);
#19301=VECTOR('',#67675,10.);
#19302=VECTOR('',#67676,10.);
#19303=VECTOR('',#67677,10.);
#19304=VECTOR('',#67680,10.);
#19305=VECTOR('',#67681,10.);
#19306=VECTOR('',#67682,10.);
#19307=VECTOR('',#67685,10.);
#19308=VECTOR('',#67686,10.);
#19309=VECTOR('',#67687,10.);
#19310=VECTOR('',#67690,10.);
#19311=VECTOR('',#67691,10.);
#19312=VECTOR('',#67696,10.);
#19313=VECTOR('',#67697,10.);
#19314=VECTOR('',#67698,10.);
#19315=VECTOR('',#67699,10.);
#19316=VECTOR('',#67702,10.);
#19317=VECTOR('',#67703,10.);
#19318=VECTOR('',#67704,10.);
#19319=VECTOR('',#67707,10.);
#19320=VECTOR('',#67708,10.);
#19321=VECTOR('',#67709,10.);
#19322=VECTOR('',#67712,10.);
#19323=VECTOR('',#67713,10.);
#19324=VECTOR('',#67718,10.);
#19325=VECTOR('',#67719,10.);
#19326=VECTOR('',#67720,10.);
#19327=VECTOR('',#67721,10.);
#19328=VECTOR('',#67724,10.);
#19329=VECTOR('',#67725,10.);
#19330=VECTOR('',#67726,10.);
#19331=VECTOR('',#67729,10.);
#19332=VECTOR('',#67730,10.);
#19333=VECTOR('',#67731,10.);
#19334=VECTOR('',#67734,10.);
#19335=VECTOR('',#67735,10.);
#19336=VECTOR('',#67740,10.);
#19337=VECTOR('',#67741,10.);
#19338=VECTOR('',#67742,10.);
#19339=VECTOR('',#67743,10.);
#19340=VECTOR('',#67746,10.);
#19341=VECTOR('',#67747,10.);
#19342=VECTOR('',#67748,10.);
#19343=VECTOR('',#67751,10.);
#19344=VECTOR('',#67752,10.);
#19345=VECTOR('',#67753,10.);
#19346=VECTOR('',#67756,10.);
#19347=VECTOR('',#67757,10.);
#19348=VECTOR('',#67762,10.);
#19349=VECTOR('',#67763,10.);
#19350=VECTOR('',#67764,10.);
#19351=VECTOR('',#67765,10.);
#19352=VECTOR('',#67768,10.);
#19353=VECTOR('',#67769,10.);
#19354=VECTOR('',#67770,10.);
#19355=VECTOR('',#67773,10.);
#19356=VECTOR('',#67774,10.);
#19357=VECTOR('',#67775,10.);
#19358=VECTOR('',#67778,10.);
#19359=VECTOR('',#67779,10.);
#19360=VECTOR('',#67784,10.);
#19361=VECTOR('',#67785,10.);
#19362=VECTOR('',#67786,10.);
#19363=VECTOR('',#67787,10.);
#19364=VECTOR('',#67790,10.);
#19365=VECTOR('',#67791,10.);
#19366=VECTOR('',#67792,10.);
#19367=VECTOR('',#67795,10.);
#19368=VECTOR('',#67796,10.);
#19369=VECTOR('',#67797,10.);
#19370=VECTOR('',#67800,10.);
#19371=VECTOR('',#67801,10.);
#19372=VECTOR('',#67806,10.);
#19373=VECTOR('',#67807,10.);
#19374=VECTOR('',#67808,10.);
#19375=VECTOR('',#67809,10.);
#19376=VECTOR('',#67812,10.);
#19377=VECTOR('',#67813,10.);
#19378=VECTOR('',#67814,10.);
#19379=VECTOR('',#67817,10.);
#19380=VECTOR('',#67818,10.);
#19381=VECTOR('',#67819,10.);
#19382=VECTOR('',#67822,10.);
#19383=VECTOR('',#67823,10.);
#19384=VECTOR('',#67828,10.);
#19385=VECTOR('',#67829,10.);
#19386=VECTOR('',#67830,10.);
#19387=VECTOR('',#67831,10.);
#19388=VECTOR('',#67834,10.);
#19389=VECTOR('',#67835,10.);
#19390=VECTOR('',#67836,10.);
#19391=VECTOR('',#67839,10.);
#19392=VECTOR('',#67840,10.);
#19393=VECTOR('',#67841,10.);
#19394=VECTOR('',#67844,10.);
#19395=VECTOR('',#67845,10.);
#19396=VECTOR('',#67850,10.);
#19397=VECTOR('',#67851,10.);
#19398=VECTOR('',#67852,10.);
#19399=VECTOR('',#67853,10.);
#19400=VECTOR('',#67856,10.);
#19401=VECTOR('',#67857,10.);
#19402=VECTOR('',#67858,10.);
#19403=VECTOR('',#67861,10.);
#19404=VECTOR('',#67862,10.);
#19405=VECTOR('',#67863,10.);
#19406=VECTOR('',#67866,10.);
#19407=VECTOR('',#67867,10.);
#19408=VECTOR('',#67872,10.);
#19409=VECTOR('',#67873,10.);
#19410=VECTOR('',#67874,10.);
#19411=VECTOR('',#67875,10.);
#19412=VECTOR('',#67878,10.);
#19413=VECTOR('',#67879,10.);
#19414=VECTOR('',#67880,10.);
#19415=VECTOR('',#67883,10.);
#19416=VECTOR('',#67884,10.);
#19417=VECTOR('',#67885,10.);
#19418=VECTOR('',#67888,10.);
#19419=VECTOR('',#67889,10.);
#19420=VECTOR('',#67894,10.);
#19421=VECTOR('',#67895,10.);
#19422=VECTOR('',#67896,10.);
#19423=VECTOR('',#67897,10.);
#19424=VECTOR('',#67900,10.);
#19425=VECTOR('',#67901,10.);
#19426=VECTOR('',#67902,10.);
#19427=VECTOR('',#67905,10.);
#19428=VECTOR('',#67906,10.);
#19429=VECTOR('',#67907,10.);
#19430=VECTOR('',#67910,10.);
#19431=VECTOR('',#67911,10.);
#19432=VECTOR('',#67916,10.);
#19433=VECTOR('',#67917,10.);
#19434=VECTOR('',#67918,10.);
#19435=VECTOR('',#67919,10.);
#19436=VECTOR('',#67922,10.);
#19437=VECTOR('',#67923,10.);
#19438=VECTOR('',#67924,10.);
#19439=VECTOR('',#67927,10.);
#19440=VECTOR('',#67928,10.);
#19441=VECTOR('',#67929,10.);
#19442=VECTOR('',#67932,10.);
#19443=VECTOR('',#67933,10.);
#19444=VECTOR('',#67938,10.);
#19445=VECTOR('',#67939,10.);
#19446=VECTOR('',#67940,10.);
#19447=VECTOR('',#67941,10.);
#19448=VECTOR('',#67944,10.);
#19449=VECTOR('',#67945,10.);
#19450=VECTOR('',#67946,10.);
#19451=VECTOR('',#67949,10.);
#19452=VECTOR('',#67950,10.);
#19453=VECTOR('',#67951,10.);
#19454=VECTOR('',#67954,10.);
#19455=VECTOR('',#67955,10.);
#19456=VECTOR('',#67960,10.);
#19457=VECTOR('',#67961,10.);
#19458=VECTOR('',#67962,10.);
#19459=VECTOR('',#67963,10.);
#19460=VECTOR('',#67966,10.);
#19461=VECTOR('',#67967,10.);
#19462=VECTOR('',#67968,10.);
#19463=VECTOR('',#67971,10.);
#19464=VECTOR('',#67972,10.);
#19465=VECTOR('',#67973,10.);
#19466=VECTOR('',#67976,10.);
#19467=VECTOR('',#67977,10.);
#19468=VECTOR('',#67982,10.);
#19469=VECTOR('',#67983,10.);
#19470=VECTOR('',#67984,10.);
#19471=VECTOR('',#67985,10.);
#19472=VECTOR('',#67988,10.);
#19473=VECTOR('',#67989,10.);
#19474=VECTOR('',#67990,10.);
#19475=VECTOR('',#67993,10.);
#19476=VECTOR('',#67994,10.);
#19477=VECTOR('',#67995,10.);
#19478=VECTOR('',#67998,10.);
#19479=VECTOR('',#67999,10.);
#19480=VECTOR('',#68004,10.);
#19481=VECTOR('',#68005,10.);
#19482=VECTOR('',#68006,10.);
#19483=VECTOR('',#68007,10.);
#19484=VECTOR('',#68010,10.);
#19485=VECTOR('',#68011,10.);
#19486=VECTOR('',#68012,10.);
#19487=VECTOR('',#68015,10.);
#19488=VECTOR('',#68016,10.);
#19489=VECTOR('',#68017,10.);
#19490=VECTOR('',#68020,10.);
#19491=VECTOR('',#68021,10.);
#19492=VECTOR('',#68026,10.);
#19493=VECTOR('',#68027,10.);
#19494=VECTOR('',#68028,10.);
#19495=VECTOR('',#68029,10.);
#19496=VECTOR('',#68032,10.);
#19497=VECTOR('',#68033,10.);
#19498=VECTOR('',#68034,10.);
#19499=VECTOR('',#68037,10.);
#19500=VECTOR('',#68038,10.);
#19501=VECTOR('',#68039,10.);
#19502=VECTOR('',#68042,10.);
#19503=VECTOR('',#68043,10.);
#19504=VECTOR('',#68048,10.);
#19505=VECTOR('',#68049,10.);
#19506=VECTOR('',#68050,10.);
#19507=VECTOR('',#68051,10.);
#19508=VECTOR('',#68054,10.);
#19509=VECTOR('',#68055,10.);
#19510=VECTOR('',#68056,10.);
#19511=VECTOR('',#68059,10.);
#19512=VECTOR('',#68060,10.);
#19513=VECTOR('',#68061,10.);
#19514=VECTOR('',#68064,10.);
#19515=VECTOR('',#68065,10.);
#19516=VECTOR('',#68070,10.);
#19517=VECTOR('',#68071,10.);
#19518=VECTOR('',#68072,10.);
#19519=VECTOR('',#68073,10.);
#19520=VECTOR('',#68076,10.);
#19521=VECTOR('',#68077,10.);
#19522=VECTOR('',#68078,10.);
#19523=VECTOR('',#68081,10.);
#19524=VECTOR('',#68082,10.);
#19525=VECTOR('',#68083,10.);
#19526=VECTOR('',#68086,10.);
#19527=VECTOR('',#68087,10.);
#19528=VECTOR('',#68092,10.);
#19529=VECTOR('',#68093,10.);
#19530=VECTOR('',#68094,10.);
#19531=VECTOR('',#68095,10.);
#19532=VECTOR('',#68098,10.);
#19533=VECTOR('',#68099,10.);
#19534=VECTOR('',#68100,10.);
#19535=VECTOR('',#68103,10.);
#19536=VECTOR('',#68104,10.);
#19537=VECTOR('',#68105,10.);
#19538=VECTOR('',#68108,10.);
#19539=VECTOR('',#68109,10.);
#19540=VECTOR('',#68114,10.);
#19541=VECTOR('',#68115,10.);
#19542=VECTOR('',#68116,10.);
#19543=VECTOR('',#68117,10.);
#19544=VECTOR('',#68120,10.);
#19545=VECTOR('',#68121,10.);
#19546=VECTOR('',#68122,10.);
#19547=VECTOR('',#68125,10.);
#19548=VECTOR('',#68126,10.);
#19549=VECTOR('',#68127,10.);
#19550=VECTOR('',#68130,10.);
#19551=VECTOR('',#68131,10.);
#19552=VECTOR('',#68136,10.);
#19553=VECTOR('',#68137,10.);
#19554=VECTOR('',#68138,10.);
#19555=VECTOR('',#68139,10.);
#19556=VECTOR('',#68142,10.);
#19557=VECTOR('',#68143,10.);
#19558=VECTOR('',#68144,10.);
#19559=VECTOR('',#68147,10.);
#19560=VECTOR('',#68148,10.);
#19561=VECTOR('',#68149,10.);
#19562=VECTOR('',#68152,10.);
#19563=VECTOR('',#68153,10.);
#19564=VECTOR('',#68158,10.);
#19565=VECTOR('',#68159,10.);
#19566=VECTOR('',#68160,10.);
#19567=VECTOR('',#68161,10.);
#19568=VECTOR('',#68164,10.);
#19569=VECTOR('',#68165,10.);
#19570=VECTOR('',#68166,10.);
#19571=VECTOR('',#68169,10.);
#19572=VECTOR('',#68170,10.);
#19573=VECTOR('',#68171,10.);
#19574=VECTOR('',#68174,10.);
#19575=VECTOR('',#68175,10.);
#19576=VECTOR('',#68180,10.);
#19577=VECTOR('',#68181,10.);
#19578=VECTOR('',#68182,10.);
#19579=VECTOR('',#68183,10.);
#19580=VECTOR('',#68186,10.);
#19581=VECTOR('',#68187,10.);
#19582=VECTOR('',#68188,10.);
#19583=VECTOR('',#68191,10.);
#19584=VECTOR('',#68192,10.);
#19585=VECTOR('',#68193,10.);
#19586=VECTOR('',#68196,10.);
#19587=VECTOR('',#68197,10.);
#19588=VECTOR('',#68202,10.);
#19589=VECTOR('',#68203,10.);
#19590=VECTOR('',#68204,10.);
#19591=VECTOR('',#68205,10.);
#19592=VECTOR('',#68208,10.);
#19593=VECTOR('',#68209,10.);
#19594=VECTOR('',#68210,10.);
#19595=VECTOR('',#68213,10.);
#19596=VECTOR('',#68214,10.);
#19597=VECTOR('',#68215,10.);
#19598=VECTOR('',#68218,10.);
#19599=VECTOR('',#68219,10.);
#19600=VECTOR('',#68224,10.);
#19601=VECTOR('',#68225,10.);
#19602=VECTOR('',#68226,10.);
#19603=VECTOR('',#68227,10.);
#19604=VECTOR('',#68230,10.);
#19605=VECTOR('',#68231,10.);
#19606=VECTOR('',#68232,10.);
#19607=VECTOR('',#68235,10.);
#19608=VECTOR('',#68236,10.);
#19609=VECTOR('',#68237,10.);
#19610=VECTOR('',#68240,10.);
#19611=VECTOR('',#68241,10.);
#19612=VECTOR('',#68246,10.);
#19613=VECTOR('',#68247,10.);
#19614=VECTOR('',#68248,10.);
#19615=VECTOR('',#68249,10.);
#19616=VECTOR('',#68252,10.);
#19617=VECTOR('',#68253,10.);
#19618=VECTOR('',#68254,10.);
#19619=VECTOR('',#68257,10.);
#19620=VECTOR('',#68258,10.);
#19621=VECTOR('',#68259,10.);
#19622=VECTOR('',#68262,10.);
#19623=VECTOR('',#68263,10.);
#19624=VECTOR('',#68268,10.);
#19625=VECTOR('',#68269,10.);
#19626=VECTOR('',#68270,10.);
#19627=VECTOR('',#68271,10.);
#19628=VECTOR('',#68274,10.);
#19629=VECTOR('',#68275,10.);
#19630=VECTOR('',#68276,10.);
#19631=VECTOR('',#68279,10.);
#19632=VECTOR('',#68280,10.);
#19633=VECTOR('',#68281,10.);
#19634=VECTOR('',#68284,10.);
#19635=VECTOR('',#68285,10.);
#19636=VECTOR('',#68290,10.);
#19637=VECTOR('',#68291,10.);
#19638=VECTOR('',#68292,10.);
#19639=VECTOR('',#68293,10.);
#19640=VECTOR('',#68296,10.);
#19641=VECTOR('',#68297,10.);
#19642=VECTOR('',#68298,10.);
#19643=VECTOR('',#68301,10.);
#19644=VECTOR('',#68302,10.);
#19645=VECTOR('',#68303,10.);
#19646=VECTOR('',#68306,10.);
#19647=VECTOR('',#68307,10.);
#19648=VECTOR('',#68312,10.);
#19649=VECTOR('',#68313,10.);
#19650=VECTOR('',#68314,10.);
#19651=VECTOR('',#68315,10.);
#19652=VECTOR('',#68318,10.);
#19653=VECTOR('',#68319,10.);
#19654=VECTOR('',#68320,10.);
#19655=VECTOR('',#68323,10.);
#19656=VECTOR('',#68324,10.);
#19657=VECTOR('',#68325,10.);
#19658=VECTOR('',#68328,10.);
#19659=VECTOR('',#68329,10.);
#19660=VECTOR('',#68334,10.);
#19661=VECTOR('',#68335,10.);
#19662=VECTOR('',#68336,10.);
#19663=VECTOR('',#68337,10.);
#19664=VECTOR('',#68340,10.);
#19665=VECTOR('',#68341,10.);
#19666=VECTOR('',#68342,10.);
#19667=VECTOR('',#68345,10.);
#19668=VECTOR('',#68346,10.);
#19669=VECTOR('',#68347,10.);
#19670=VECTOR('',#68350,10.);
#19671=VECTOR('',#68351,10.);
#19672=VECTOR('',#68356,10.);
#19673=VECTOR('',#68357,10.);
#19674=VECTOR('',#68358,10.);
#19675=VECTOR('',#68359,10.);
#19676=VECTOR('',#68362,10.);
#19677=VECTOR('',#68363,10.);
#19678=VECTOR('',#68364,10.);
#19679=VECTOR('',#68367,10.);
#19680=VECTOR('',#68368,10.);
#19681=VECTOR('',#68369,10.);
#19682=VECTOR('',#68372,10.);
#19683=VECTOR('',#68373,10.);
#19684=VECTOR('',#68378,10.);
#19685=VECTOR('',#68379,10.);
#19686=VECTOR('',#68380,10.);
#19687=VECTOR('',#68381,10.);
#19688=VECTOR('',#68384,10.);
#19689=VECTOR('',#68385,10.);
#19690=VECTOR('',#68386,10.);
#19691=VECTOR('',#68389,10.);
#19692=VECTOR('',#68390,10.);
#19693=VECTOR('',#68391,10.);
#19694=VECTOR('',#68394,10.);
#19695=VECTOR('',#68395,10.);
#19696=VECTOR('',#68400,10.);
#19697=VECTOR('',#68401,10.);
#19698=VECTOR('',#68402,10.);
#19699=VECTOR('',#68403,10.);
#19700=VECTOR('',#68406,10.);
#19701=VECTOR('',#68407,10.);
#19702=VECTOR('',#68408,10.);
#19703=VECTOR('',#68411,10.);
#19704=VECTOR('',#68412,10.);
#19705=VECTOR('',#68413,10.);
#19706=VECTOR('',#68416,10.);
#19707=VECTOR('',#68417,10.);
#19708=VECTOR('',#68422,10.);
#19709=VECTOR('',#68423,10.);
#19710=VECTOR('',#68424,10.);
#19711=VECTOR('',#68425,10.);
#19712=VECTOR('',#68428,10.);
#19713=VECTOR('',#68429,10.);
#19714=VECTOR('',#68430,10.);
#19715=VECTOR('',#68433,10.);
#19716=VECTOR('',#68434,10.);
#19717=VECTOR('',#68435,10.);
#19718=VECTOR('',#68438,10.);
#19719=VECTOR('',#68439,10.);
#19720=VECTOR('',#68444,10.);
#19721=VECTOR('',#68445,10.);
#19722=VECTOR('',#68446,10.);
#19723=VECTOR('',#68447,10.);
#19724=VECTOR('',#68450,10.);
#19725=VECTOR('',#68451,10.);
#19726=VECTOR('',#68452,10.);
#19727=VECTOR('',#68455,10.);
#19728=VECTOR('',#68456,10.);
#19729=VECTOR('',#68457,10.);
#19730=VECTOR('',#68460,10.);
#19731=VECTOR('',#68461,10.);
#19732=VECTOR('',#68466,10.);
#19733=VECTOR('',#68467,10.);
#19734=VECTOR('',#68468,10.);
#19735=VECTOR('',#68469,10.);
#19736=VECTOR('',#68472,10.);
#19737=VECTOR('',#68473,10.);
#19738=VECTOR('',#68474,10.);
#19739=VECTOR('',#68477,10.);
#19740=VECTOR('',#68478,10.);
#19741=VECTOR('',#68479,10.);
#19742=VECTOR('',#68482,10.);
#19743=VECTOR('',#68483,10.);
#19744=VECTOR('',#68488,10.);
#19745=VECTOR('',#68489,10.);
#19746=VECTOR('',#68490,10.);
#19747=VECTOR('',#68491,10.);
#19748=VECTOR('',#68494,10.);
#19749=VECTOR('',#68495,10.);
#19750=VECTOR('',#68496,10.);
#19751=VECTOR('',#68499,10.);
#19752=VECTOR('',#68500,10.);
#19753=VECTOR('',#68501,10.);
#19754=VECTOR('',#68504,10.);
#19755=VECTOR('',#68505,10.);
#19756=VECTOR('',#68510,10.);
#19757=VECTOR('',#68511,10.);
#19758=VECTOR('',#68512,10.);
#19759=VECTOR('',#68513,10.);
#19760=VECTOR('',#68516,10.);
#19761=VECTOR('',#68517,10.);
#19762=VECTOR('',#68518,10.);
#19763=VECTOR('',#68521,10.);
#19764=VECTOR('',#68522,10.);
#19765=VECTOR('',#68523,10.);
#19766=VECTOR('',#68526,10.);
#19767=VECTOR('',#68527,10.);
#19768=VECTOR('',#68532,10.);
#19769=VECTOR('',#68533,10.);
#19770=VECTOR('',#68534,10.);
#19771=VECTOR('',#68535,10.);
#19772=VECTOR('',#68538,10.);
#19773=VECTOR('',#68539,10.);
#19774=VECTOR('',#68540,10.);
#19775=VECTOR('',#68543,10.);
#19776=VECTOR('',#68544,10.);
#19777=VECTOR('',#68545,10.);
#19778=VECTOR('',#68548,10.);
#19779=VECTOR('',#68549,10.);
#19780=VECTOR('',#68554,10.);
#19781=VECTOR('',#68555,10.);
#19782=VECTOR('',#68556,10.);
#19783=VECTOR('',#68557,10.);
#19784=VECTOR('',#68560,10.);
#19785=VECTOR('',#68561,10.);
#19786=VECTOR('',#68562,10.);
#19787=VECTOR('',#68565,10.);
#19788=VECTOR('',#68566,10.);
#19789=VECTOR('',#68567,10.);
#19790=VECTOR('',#68570,10.);
#19791=VECTOR('',#68571,10.);
#19792=VECTOR('',#68576,10.);
#19793=VECTOR('',#68577,10.);
#19794=VECTOR('',#68578,10.);
#19795=VECTOR('',#68579,10.);
#19796=VECTOR('',#68582,10.);
#19797=VECTOR('',#68583,10.);
#19798=VECTOR('',#68584,10.);
#19799=VECTOR('',#68587,10.);
#19800=VECTOR('',#68588,10.);
#19801=VECTOR('',#68589,10.);
#19802=VECTOR('',#68592,10.);
#19803=VECTOR('',#68593,10.);
#19804=VECTOR('',#68598,10.);
#19805=VECTOR('',#68599,10.);
#19806=VECTOR('',#68600,10.);
#19807=VECTOR('',#68601,10.);
#19808=VECTOR('',#68604,10.);
#19809=VECTOR('',#68605,10.);
#19810=VECTOR('',#68606,10.);
#19811=VECTOR('',#68609,10.);
#19812=VECTOR('',#68610,10.);
#19813=VECTOR('',#68611,10.);
#19814=VECTOR('',#68614,10.);
#19815=VECTOR('',#68615,10.);
#19816=VECTOR('',#68620,10.);
#19817=VECTOR('',#68621,10.);
#19818=VECTOR('',#68622,10.);
#19819=VECTOR('',#68623,10.);
#19820=VECTOR('',#68626,10.);
#19821=VECTOR('',#68627,10.);
#19822=VECTOR('',#68628,10.);
#19823=VECTOR('',#68631,10.);
#19824=VECTOR('',#68632,10.);
#19825=VECTOR('',#68633,10.);
#19826=VECTOR('',#68636,10.);
#19827=VECTOR('',#68637,10.);
#19828=VECTOR('',#68642,10.);
#19829=VECTOR('',#68643,10.);
#19830=VECTOR('',#68644,10.);
#19831=VECTOR('',#68645,10.);
#19832=VECTOR('',#68648,10.);
#19833=VECTOR('',#68649,10.);
#19834=VECTOR('',#68650,10.);
#19835=VECTOR('',#68653,10.);
#19836=VECTOR('',#68654,10.);
#19837=VECTOR('',#68655,10.);
#19838=VECTOR('',#68658,10.);
#19839=VECTOR('',#68659,10.);
#19840=VECTOR('',#68664,10.);
#19841=VECTOR('',#68665,10.);
#19842=VECTOR('',#68666,10.);
#19843=VECTOR('',#68667,10.);
#19844=VECTOR('',#68670,10.);
#19845=VECTOR('',#68671,10.);
#19846=VECTOR('',#68672,10.);
#19847=VECTOR('',#68675,10.);
#19848=VECTOR('',#68676,10.);
#19849=VECTOR('',#68677,10.);
#19850=VECTOR('',#68680,10.);
#19851=VECTOR('',#68681,10.);
#19852=VECTOR('',#68686,10.);
#19853=VECTOR('',#68687,10.);
#19854=VECTOR('',#68688,10.);
#19855=VECTOR('',#68689,10.);
#19856=VECTOR('',#68692,10.);
#19857=VECTOR('',#68693,10.);
#19858=VECTOR('',#68694,10.);
#19859=VECTOR('',#68697,10.);
#19860=VECTOR('',#68698,10.);
#19861=VECTOR('',#68699,10.);
#19862=VECTOR('',#68702,10.);
#19863=VECTOR('',#68703,10.);
#19864=VECTOR('',#68708,10.);
#19865=VECTOR('',#68709,10.);
#19866=VECTOR('',#68710,10.);
#19867=VECTOR('',#68711,10.);
#19868=VECTOR('',#68714,10.);
#19869=VECTOR('',#68715,10.);
#19870=VECTOR('',#68716,10.);
#19871=VECTOR('',#68719,10.);
#19872=VECTOR('',#68720,10.);
#19873=VECTOR('',#68721,10.);
#19874=VECTOR('',#68724,10.);
#19875=VECTOR('',#68725,10.);
#19876=VECTOR('',#68730,10.);
#19877=VECTOR('',#68731,10.);
#19878=VECTOR('',#68732,10.);
#19879=VECTOR('',#68733,10.);
#19880=VECTOR('',#68736,10.);
#19881=VECTOR('',#68737,10.);
#19882=VECTOR('',#68738,10.);
#19883=VECTOR('',#68741,10.);
#19884=VECTOR('',#68742,10.);
#19885=VECTOR('',#68743,10.);
#19886=VECTOR('',#68746,10.);
#19887=VECTOR('',#68747,10.);
#19888=VECTOR('',#68752,10.);
#19889=VECTOR('',#68753,10.);
#19890=VECTOR('',#68754,10.);
#19891=VECTOR('',#68755,10.);
#19892=VECTOR('',#68758,10.);
#19893=VECTOR('',#68759,10.);
#19894=VECTOR('',#68760,10.);
#19895=VECTOR('',#68763,10.);
#19896=VECTOR('',#68764,10.);
#19897=VECTOR('',#68765,10.);
#19898=VECTOR('',#68768,10.);
#19899=VECTOR('',#68769,10.);
#19900=VECTOR('',#68774,10.);
#19901=VECTOR('',#68775,10.);
#19902=VECTOR('',#68776,10.);
#19903=VECTOR('',#68777,10.);
#19904=VECTOR('',#68780,10.);
#19905=VECTOR('',#68781,10.);
#19906=VECTOR('',#68782,10.);
#19907=VECTOR('',#68785,10.);
#19908=VECTOR('',#68786,10.);
#19909=VECTOR('',#68787,10.);
#19910=VECTOR('',#68790,10.);
#19911=VECTOR('',#68791,10.);
#19912=VECTOR('',#68796,10.);
#19913=VECTOR('',#68797,10.);
#19914=VECTOR('',#68798,10.);
#19915=VECTOR('',#68799,10.);
#19916=VECTOR('',#68802,10.);
#19917=VECTOR('',#68803,10.);
#19918=VECTOR('',#68804,10.);
#19919=VECTOR('',#68807,10.);
#19920=VECTOR('',#68808,10.);
#19921=VECTOR('',#68809,10.);
#19922=VECTOR('',#68812,10.);
#19923=VECTOR('',#68813,10.);
#19924=VECTOR('',#68818,10.);
#19925=VECTOR('',#68819,10.);
#19926=VECTOR('',#68820,10.);
#19927=VECTOR('',#68821,10.);
#19928=VECTOR('',#68824,10.);
#19929=VECTOR('',#68825,10.);
#19930=VECTOR('',#68826,10.);
#19931=VECTOR('',#68829,10.);
#19932=VECTOR('',#68830,10.);
#19933=VECTOR('',#68831,10.);
#19934=VECTOR('',#68834,10.);
#19935=VECTOR('',#68835,10.);
#19936=VECTOR('',#68840,10.);
#19937=VECTOR('',#68841,10.);
#19938=VECTOR('',#68842,10.);
#19939=VECTOR('',#68843,10.);
#19940=VECTOR('',#68846,10.);
#19941=VECTOR('',#68847,10.);
#19942=VECTOR('',#68848,10.);
#19943=VECTOR('',#68851,10.);
#19944=VECTOR('',#68852,10.);
#19945=VECTOR('',#68853,10.);
#19946=VECTOR('',#68856,10.);
#19947=VECTOR('',#68857,10.);
#19948=VECTOR('',#68862,10.);
#19949=VECTOR('',#68863,10.);
#19950=VECTOR('',#68864,10.);
#19951=VECTOR('',#68865,10.);
#19952=VECTOR('',#68868,10.);
#19953=VECTOR('',#68869,10.);
#19954=VECTOR('',#68870,10.);
#19955=VECTOR('',#68873,10.);
#19956=VECTOR('',#68874,10.);
#19957=VECTOR('',#68875,10.);
#19958=VECTOR('',#68878,10.);
#19959=VECTOR('',#68879,10.);
#19960=VECTOR('',#68884,10.);
#19961=VECTOR('',#68885,10.);
#19962=VECTOR('',#68886,10.);
#19963=VECTOR('',#68887,10.);
#19964=VECTOR('',#68890,10.);
#19965=VECTOR('',#68891,10.);
#19966=VECTOR('',#68892,10.);
#19967=VECTOR('',#68895,10.);
#19968=VECTOR('',#68896,10.);
#19969=VECTOR('',#68897,10.);
#19970=VECTOR('',#68900,10.);
#19971=VECTOR('',#68901,10.);
#19972=VECTOR('',#68906,10.);
#19973=VECTOR('',#68907,10.);
#19974=VECTOR('',#68908,10.);
#19975=VECTOR('',#68909,10.);
#19976=VECTOR('',#68912,10.);
#19977=VECTOR('',#68913,10.);
#19978=VECTOR('',#68914,10.);
#19979=VECTOR('',#68917,10.);
#19980=VECTOR('',#68918,10.);
#19981=VECTOR('',#68919,10.);
#19982=VECTOR('',#68922,10.);
#19983=VECTOR('',#68923,10.);
#19984=VECTOR('',#68928,10.);
#19985=VECTOR('',#68929,10.);
#19986=VECTOR('',#68930,10.);
#19987=VECTOR('',#68931,10.);
#19988=VECTOR('',#68934,10.);
#19989=VECTOR('',#68935,10.);
#19990=VECTOR('',#68936,10.);
#19991=VECTOR('',#68939,10.);
#19992=VECTOR('',#68940,10.);
#19993=VECTOR('',#68941,10.);
#19994=VECTOR('',#68944,10.);
#19995=VECTOR('',#68945,10.);
#19996=VECTOR('',#68950,10.);
#19997=VECTOR('',#68951,10.);
#19998=VECTOR('',#68952,10.);
#19999=VECTOR('',#68953,10.);
#20000=VECTOR('',#68956,10.);
#20001=VECTOR('',#68957,10.);
#20002=VECTOR('',#68958,10.);
#20003=VECTOR('',#68961,10.);
#20004=VECTOR('',#68962,10.);
#20005=VECTOR('',#68963,10.);
#20006=VECTOR('',#68966,10.);
#20007=VECTOR('',#68967,10.);
#20008=VECTOR('',#68972,10.);
#20009=VECTOR('',#68973,10.);
#20010=VECTOR('',#68974,10.);
#20011=VECTOR('',#68975,10.);
#20012=VECTOR('',#68978,10.);
#20013=VECTOR('',#68979,10.);
#20014=VECTOR('',#68980,10.);
#20015=VECTOR('',#68983,10.);
#20016=VECTOR('',#68984,10.);
#20017=VECTOR('',#68985,10.);
#20018=VECTOR('',#68988,10.);
#20019=VECTOR('',#68989,10.);
#20020=VECTOR('',#68994,10.);
#20021=VECTOR('',#68995,10.);
#20022=VECTOR('',#68996,10.);
#20023=VECTOR('',#68997,10.);
#20024=VECTOR('',#68998,10.);
#20025=VECTOR('',#68999,10.);
#20026=VECTOR('',#69002,10.);
#20027=VECTOR('',#69003,10.);
#20028=VECTOR('',#69004,10.);
#20029=VECTOR('',#69005,10.);
#20030=VECTOR('',#69006,10.);
#20031=VECTOR('',#69007,10.);
#20032=VECTOR('',#69010,10.);
#20033=VECTOR('',#69011,10.);
#20034=VECTOR('',#69014,10.);
#20035=VECTOR('',#69015,10.);
#20036=VECTOR('',#69016,10.);
#20037=VECTOR('',#69017,10.);
#20038=VECTOR('',#69018,10.);
#20039=VECTOR('',#69021,10.);
#20040=VECTOR('',#69022,10.);
#20041=VECTOR('',#69023,10.);
#20042=VECTOR('',#69024,10.);
#20043=VECTOR('',#69025,10.);
#20044=VECTOR('',#69026,10.);
#20045=VECTOR('',#69027,10.);
#20046=VECTOR('',#69028,10.);
#20047=VECTOR('',#69029,10.);
#20048=VECTOR('',#69032,10.);
#20049=VECTOR('',#69033,10.);
#20050=VECTOR('',#69034,10.);
#20051=VECTOR('',#69035,10.);
#20052=VECTOR('',#69036,10.);
#20053=VECTOR('',#69039,10.);
#20054=VECTOR('',#69040,10.);
#20055=VECTOR('',#69041,10.);
#20056=VECTOR('',#69044,10.);
#20057=VECTOR('',#69045,10.);
#20058=VECTOR('',#69046,10.);
#20059=VECTOR('',#69049,10.);
#20060=VECTOR('',#69050,10.);
#20061=VECTOR('',#69053,10.);
#20062=VECTOR('',#69064,0.999999999999979);
#20063=VECTOR('',#69069,1.);
#20064=VECTOR('',#69074,1.);
#20065=VECTOR('',#69079,1.00000000000001);
#20066=VECTOR('',#69084,1.39999999999999);
#20067=VECTOR('',#69089,1.29999999999999);
#20068=VECTOR('',#69094,10.);
#20069=VECTOR('',#69095,10.);
#20070=VECTOR('',#69096,10.);
#20071=VECTOR('',#69097,10.);
#20072=VECTOR('',#69102,1.30000000000003);
#20073=VECTOR('',#69105,1.4);
#20074=VECTOR('',#69110,1.3);
#20075=VECTOR('',#69115,1.3);
#20076=VECTOR('',#69120,3.00000000000001);
#20077=VECTOR('',#69131,3.);
#20078=VECTOR('',#69142,3.);
#20079=VECTOR('',#69153,3.00000000000001);
#20080=VECTOR('',#69164,3.00000000000001);
#20081=VECTOR('',#69175,3.00000000000001);
#20082=VECTOR('',#69184,2.19999999999999);
#20083=VECTOR('',#69189,10.);
#20084=VECTOR('',#69190,10.);
#20085=VECTOR('',#69199,2.04999999999998);
#20086=VECTOR('',#69202,2.2);
#20087=VECTOR('',#69207,2.05);
#20088=VECTOR('',#69210,2.2);
#20089=VECTOR('',#69215,2.05);
#20090=VECTOR('',#69218,2.2);
#20091=VECTOR('',#69223,2.05);
#20092=VECTOR('',#69226,2.2);
#20093=VECTOR('',#69231,2.05);
#20094=VECTOR('',#69234,2.19999999999999);
#20095=VECTOR('',#69239,2.04999999999998);
#20096=VECTOR('',#69242,10.);
#20097=VECTOR('',#69245,10.);
#20098=VECTOR('',#69246,10.);
#20099=VECTOR('',#69249,10.);
#20100=VECTOR('',#69250,10.);
#20101=VECTOR('',#69251,10.);
#20102=VECTOR('',#69254,10.);
#20103=VECTOR('',#69255,10.);
#20104=VECTOR('',#69256,10.);
#20105=VECTOR('',#69259,10.);
#20106=VECTOR('',#69260,10.);
#20107=VECTOR('',#69261,10.);
#20108=VECTOR('',#69262,10.);
#20109=VECTOR('',#69265,10.);
#20110=VECTOR('',#69266,10.);
#20111=VECTOR('',#69267,10.);
#20112=VECTOR('',#69270,10.);
#20113=VECTOR('',#69271,10.);
#20114=VECTOR('',#69272,10.);
#20115=VECTOR('',#69275,10.);
#20116=VECTOR('',#69278,10.);
#20117=VECTOR('',#69281,10.);
#20118=VECTOR('',#69282,10.);
#20119=VECTOR('',#69285,10.);
#20120=VECTOR('',#69286,10.);
#20121=VECTOR('',#69289,10.);
#20122=VECTOR('',#69294,10.);
#20123=VECTOR('',#69301,10.);
#20124=VECTOR('',#69302,10.);
#20125=VECTOR('',#69305,10.);
#20126=VECTOR('',#69306,10.);
#20127=VECTOR('',#69309,10.);
#20128=VECTOR('',#69310,10.);
#20129=VECTOR('',#69313,10.);
#20130=VECTOR('',#69316,10.);
#20131=VECTOR('',#69317,10.);
#20132=VECTOR('',#69320,10.);
#20133=VECTOR('',#69323,10.);
#20134=VECTOR('',#69324,10.);
#20135=VECTOR('',#69327,10.);
#20136=VECTOR('',#69328,10.);
#20137=VECTOR('',#69329,10.);
#20138=VECTOR('',#69332,10.);
#20139=VECTOR('',#69333,10.);
#20140=VECTOR('',#69334,10.);
#20141=VECTOR('',#69337,10.);
#20142=VECTOR('',#69338,10.);
#20143=VECTOR('',#69341,10.);
#20144=VECTOR('',#69342,10.);
#20145=VECTOR('',#69343,10.);
#20146=VECTOR('',#69346,10.);
#20147=VECTOR('',#69347,10.);
#20148=VECTOR('',#69348,10.);
#20149=VECTOR('',#69351,10.);
#20150=VECTOR('',#69352,10.);
#20151=VECTOR('',#69353,10.);
#20152=VECTOR('',#69356,10.);
#20153=VECTOR('',#69357,10.);
#20154=VECTOR('',#69360,10.);
#20155=VECTOR('',#69361,10.);
#20156=VECTOR('',#69362,10.);
#20157=VECTOR('',#69365,10.);
#20158=VECTOR('',#69366,10.);
#20159=VECTOR('',#69369,10.);
#20160=VECTOR('',#69370,10.);
#20161=VECTOR('',#69373,10.);
#20162=VECTOR('',#69376,10.);
#20163=VECTOR('',#69377,10.);
#20164=VECTOR('',#69380,10.);
#20165=VECTOR('',#69381,10.);
#20166=VECTOR('',#69384,10.);
#20167=VECTOR('',#69385,10.);
#20168=VECTOR('',#69388,10.);
#20169=VECTOR('',#69391,10.);
#20170=VECTOR('',#69394,10.);
#20171=VECTOR('',#69397,10.);
#20172=VECTOR('',#69398,10.);
#20173=VECTOR('',#69401,10.);
#20174=VECTOR('',#69402,10.);
#20175=VECTOR('',#69405,10.);
#20176=VECTOR('',#69408,10.);
#20177=VECTOR('',#69411,10.);
#20178=VECTOR('',#69414,10.);
#20179=VECTOR('',#69417,10.);
#20180=VECTOR('',#69422,10.);
#20181=VECTOR('',#69425,10.);
#20182=VECTOR('',#69428,10.);
#20183=VECTOR('',#69433,10.);
#20184=VECTOR('',#69436,10.);
#20185=VECTOR('',#69439,10.);
#20186=VECTOR('',#69442,10.);
#20187=VECTOR('',#69453,10.);
#20188=VECTOR('',#69456,10.);
#20189=VECTOR('',#69459,10.);
#20190=VECTOR('',#69466,2.2);
#20191=VECTOR('',#69475,1.12500000000001);
#20192=VECTOR('',#69482,10.);
#20193=VECTOR('',#69483,10.);
#20194=VECTOR('',#69488,10.);
#20195=VECTOR('',#69489,10.);
#20196=VECTOR('',#69490,10.);
#20197=VECTOR('',#69491,10.);
#20198=VECTOR('',#69496,1.05);
#20199=VECTOR('',#69501,1.12500000000001);
#20200=VECTOR('',#69506,1.05);
#20201=VECTOR('',#69511,0.525000000000002);
#20202=VECTOR('',#69514,0.525000000000002);
#20203=VECTOR('',#69519,1.675);
#20204=VECTOR('',#69526,10.);
#20205=VECTOR('',#69527,10.);
#20206=VECTOR('',#69528,10.);
#20207=VECTOR('',#69529,10.);
#20208=VECTOR('',#69530,10.);
#20209=VECTOR('',#69531,10.);
#20210=VECTOR('',#69532,10.);
#20211=VECTOR('',#69535,1.54999999999999);
#20212=VECTOR('',#69542,1.675);
#20213=VECTOR('',#69549,1.54999999999999);
#20214=VECTOR('',#69560,2.05);
#20215=VECTOR('',#69565,10.);
#20216=VECTOR('',#69566,10.);
#20217=VECTOR('',#69567,10.);
#20218=VECTOR('',#69572,1.125);
#20219=VECTOR('',#69579,10.);
#20220=VECTOR('',#69580,10.);
#20221=VECTOR('',#69581,10.);
#20222=VECTOR('',#69582,10.);
#20223=VECTOR('',#69585,1.05);
#20224=VECTOR('',#69596,1.12500000000001);
#20225=VECTOR('',#69601,10.);
#20226=VECTOR('',#69602,10.);
#20227=VECTOR('',#69603,10.);
#20228=VECTOR('',#69616,1.05);
#20229=VECTOR('',#69625,1.12500000000001);
#20230=VECTOR('',#69630,1.05);
#20231=VECTOR('',#69639,10.);
#20232=VECTOR('',#69642,10.);
#20233=VECTOR('',#69645,10.);
#20234=VECTOR('',#69648,10.);
#20235=VECTOR('',#69651,10.);
#20236=VECTOR('',#69654,10.);
#20237=VECTOR('',#69657,1.675);
#20238=VECTOR('',#69662,1.54999999999999);
#20239=VECTOR('',#69667,1.675);
#20240=VECTOR('',#69672,1.54999999999999);
#20241=VECTOR('',#69677,1.675);
#20242=VECTOR('',#69682,1.54999999999999);
#20243=VECTOR('',#69687,1.675);
#20244=VECTOR('',#69692,1.54999999999999);
#20245=VECTOR('',#69697,1.54999999999999);
#20246=VECTOR('',#69700,1.54999999999999);
#20247=VECTOR('',#69703,1.54999999999999);
#20248=VECTOR('',#69706,1.54999999999999);
#20249=VECTOR('',#69709,4.95);
#20250=VECTOR('',#69716,4.8);
#20251=VECTOR('',#69717,4.8);
#20252=VECTOR('',#69718,4.8);
#20253=VECTOR('',#69719,4.8);
#20254=VECTOR('',#69722,10.);
#20255=VECTOR('',#69725,10.);
#20256=VECTOR('',#69730,1.26250000000001);
#20257=VECTOR('',#69737,2.525);
#20258=VECTOR('',#69740,10.);
#20259=VECTOR('',#69743,10.);
#20260=VECTOR('',#69744,10.);
#20261=VECTOR('',#69745,10.);
#20262=VECTOR('',#69746,10.);
#20263=VECTOR('',#69747,10.);
#20264=VECTOR('',#69750,10.);
#20265=VECTOR('',#69751,10.);
#20266=VECTOR('',#69752,10.);
#20267=VECTOR('',#69755,10.);
#20268=VECTOR('',#69756,10.);
#20269=VECTOR('',#69757,10.);
#20270=VECTOR('',#69760,10.);
#20271=VECTOR('',#69761,10.);
#20272=VECTOR('',#69762,10.);
#20273=VECTOR('',#69763,10.);
#20274=VECTOR('',#69764,10.);
#20275=VECTOR('',#69765,10.);
#20276=VECTOR('',#69766,10.);
#20277=VECTOR('',#69767,10.);
#20278=VECTOR('',#69768,10.);
#20279=VECTOR('',#69771,10.);
#20280=VECTOR('',#69772,10.);
#20281=VECTOR('',#69775,10.);
#20282=VECTOR('',#69776,10.);
#20283=VECTOR('',#69777,10.);
#20284=VECTOR('',#69778,10.);
#20285=VECTOR('',#69781,10.);
#20286=VECTOR('',#69782,10.);
#20287=VECTOR('',#69783,10.);
#20288=VECTOR('',#69784,10.);
#20289=VECTOR('',#69785,10.);
#20290=VECTOR('',#69788,10.);
#20291=VECTOR('',#69791,10.);
#20292=VECTOR('',#69792,10.);
#20293=VECTOR('',#69795,10.);
#20294=VECTOR('',#69796,10.);
#20295=VECTOR('',#69799,10.);
#20296=VECTOR('',#69800,10.);
#20297=VECTOR('',#69803,10.);
#20298=VECTOR('',#69804,10.);
#20299=VECTOR('',#69807,10.);
#20300=VECTOR('',#69808,10.);
#20301=VECTOR('',#69811,10.);
#20302=VECTOR('',#69812,10.);
#20303=VECTOR('',#69815,10.);
#20304=VECTOR('',#69816,10.);
#20305=VECTOR('',#69819,10.);
#20306=VECTOR('',#69820,10.);
#20307=VECTOR('',#69823,10.);
#20308=VECTOR('',#69824,10.);
#20309=VECTOR('',#69827,10.);
#20310=VECTOR('',#69828,10.);
#20311=VECTOR('',#69829,10.);
#20312=VECTOR('',#69832,10.);
#20313=VECTOR('',#69835,10.);
#20314=VECTOR('',#69836,10.);
#20315=VECTOR('',#69837,10.);
#20316=VECTOR('',#69846,10.);
#20317=VECTOR('',#69849,10.);
#20318=VECTOR('',#69854,10.);
#20319=VECTOR('',#69855,10.);
#20320=VECTOR('',#69860,10.);
#20321=VECTOR('',#69871,1.40000000000001);
#20322=VECTOR('',#69876,1.40000000000001);
#20323=VECTOR('',#69881,1.40000000000001);
#20324=VECTOR('',#69884,10.);
#20325=VECTOR('',#69885,10.);
#20326=VECTOR('',#69886,10.);
#20327=VECTOR('',#69887,10.);
#20328=VECTOR('',#69890,10.);
#20329=VECTOR('',#69891,10.);
#20330=VECTOR('',#69892,10.);
#20331=VECTOR('',#69895,10.);
#20332=VECTOR('',#69896,10.);
#20333=VECTOR('',#69897,10.);
#20334=VECTOR('',#69900,10.);
#20335=VECTOR('',#69901,10.);
#20336=VECTOR('',#69904,10.);
#20337=VECTOR('',#69905,10.);
#20338=VECTOR('',#69906,10.);
#20339=VECTOR('',#69909,10.);
#20340=VECTOR('',#69910,10.);
#20341=VECTOR('',#69915,10.);
#20342=VECTOR('',#69916,10.);
#20343=VECTOR('',#69917,10.);
#20344=VECTOR('',#69920,10.);
#20345=VECTOR('',#69921,10.);
#20346=VECTOR('',#69924,10.);
#20347=VECTOR('',#69925,10.);
#20348=VECTOR('',#69926,10.);
#20349=VECTOR('',#69929,10.);
#20350=VECTOR('',#69930,10.);
#20351=VECTOR('',#69933,10.);
#20352=VECTOR('',#69944,10.);
#20353=VECTOR('',#69949,10.);
#20354=VECTOR('',#69952,10.);
#20355=VECTOR('',#69953,10.);
#20356=VECTOR('',#69958,10.);
#20357=VECTOR('',#69963,10.);
#20358=VECTOR('',#69966,10.);
#20359=VECTOR('',#69967,10.);
#20360=VECTOR('',#69976,2.34999999999999);
#20361=VECTOR('',#69981,2.5);
#20362=VECTOR('',#69986,2.34999999999999);
#20363=VECTOR('',#69993,10.);
#20364=VECTOR('',#69998,1.05);
#20365=VECTOR('',#70005,10.);
#20366=VECTOR('',#70008,10.);
#20367=VECTOR('',#70009,10.);
#20368=VECTOR('',#70010,10.);
#20369=VECTOR('',#70011,10.);
#20370=VECTOR('',#70014,10.);
#20371=VECTOR('',#70015,10.);
#20372=VECTOR('',#70016,10.);
#20373=VECTOR('',#70017,10.);
#20374=VECTOR('',#70018,10.);
#20375=VECTOR('',#70025,10.);
#20376=VECTOR('',#70034,3.375);
#20377=VECTOR('',#70037,10.);
#20378=VECTOR('',#70040,10.);
#20379=VECTOR('',#70043,10.);
#20380=VECTOR('',#70046,10.);
#20381=VECTOR('',#70049,10.);
#20382=VECTOR('',#70054,10.);
#20383=VECTOR('',#70057,10.);
#20384=VECTOR('',#70060,10.);
#20385=VECTOR('',#70063,10.);
#20386=VECTOR('',#70066,10.);
#20387=VECTOR('',#70069,10.);
#20388=VECTOR('',#70072,10.);
#20389=VECTOR('',#70075,10.);
#20390=VECTOR('',#70078,10.);
#20391=VECTOR('',#70081,10.);
#20392=VECTOR('',#70084,10.);
#20393=VECTOR('',#70087,10.);
#20394=VECTOR('',#70090,10.);
#20395=VECTOR('',#70093,10.);
#20396=VECTOR('',#70096,10.);
#20397=VECTOR('',#70099,10.);
#20398=VECTOR('',#70102,10.);
#20399=VECTOR('',#70105,10.);
#20400=VECTOR('',#70108,10.);
#20401=VECTOR('',#70111,10.);
#20402=VECTOR('',#70114,10.);
#20403=VECTOR('',#70117,10.);
#20404=VECTOR('',#70120,10.);
#20405=VECTOR('',#70123,10.);
#20406=VECTOR('',#70126,10.);
#20407=VECTOR('',#70131,10.);
#20408=VECTOR('',#70132,10.);
#20409=VECTOR('',#70133,10.);
#20410=VECTOR('',#70136,10.);
#20411=VECTOR('',#70137,10.);
#20412=VECTOR('',#70138,10.);
#20413=VECTOR('',#70139,10.);
#20414=VECTOR('',#70146,10.);
#20415=VECTOR('',#70151,10.);
#20416=VECTOR('',#70152,10.);
#20417=VECTOR('',#70153,10.);
#20418=VECTOR('',#70156,10.);
#20419=VECTOR('',#70157,10.);
#20420=VECTOR('',#70158,10.);
#20421=VECTOR('',#70159,10.);
#20422=VECTOR('',#70166,10.);
#20423=VECTOR('',#70171,10.);
#20424=VECTOR('',#70172,10.);
#20425=VECTOR('',#70173,10.);
#20426=VECTOR('',#70176,10.);
#20427=VECTOR('',#70177,10.);
#20428=VECTOR('',#70178,10.);
#20429=VECTOR('',#70179,10.);
#20430=VECTOR('',#70186,10.);
#20431=VECTOR('',#70191,10.);
#20432=VECTOR('',#70192,10.);
#20433=VECTOR('',#70193,10.);
#20434=VECTOR('',#70196,10.);
#20435=VECTOR('',#70197,10.);
#20436=VECTOR('',#70198,10.);
#20437=VECTOR('',#70199,10.);
#20438=VECTOR('',#70206,10.);
#20439=VECTOR('',#70211,10.);
#20440=VECTOR('',#70212,10.);
#20441=VECTOR('',#70213,10.);
#20442=VECTOR('',#70216,10.);
#20443=VECTOR('',#70217,10.);
#20444=VECTOR('',#70218,10.);
#20445=VECTOR('',#70219,10.);
#20446=VECTOR('',#70226,10.);
#20447=VECTOR('',#70231,10.);
#20448=VECTOR('',#70232,10.);
#20449=VECTOR('',#70233,10.);
#20450=VECTOR('',#70236,10.);
#20451=VECTOR('',#70237,10.);
#20452=VECTOR('',#70238,10.);
#20453=VECTOR('',#70239,10.);
#20454=VECTOR('',#70246,10.);
#20455=VECTOR('',#70251,10.);
#20456=VECTOR('',#70252,10.);
#20457=VECTOR('',#70253,10.);
#20458=VECTOR('',#70256,10.);
#20459=VECTOR('',#70257,10.);
#20460=VECTOR('',#70258,10.);
#20461=VECTOR('',#70259,10.);
#20462=VECTOR('',#70266,10.);
#20463=VECTOR('',#70271,10.);
#20464=VECTOR('',#70272,10.);
#20465=VECTOR('',#70273,10.);
#20466=VECTOR('',#70276,10.);
#20467=VECTOR('',#70277,10.);
#20468=VECTOR('',#70278,10.);
#20469=VECTOR('',#70279,10.);
#20470=VECTOR('',#70286,10.);
#20471=VECTOR('',#70291,10.);
#20472=VECTOR('',#70292,10.);
#20473=VECTOR('',#70293,10.);
#20474=VECTOR('',#70296,10.);
#20475=VECTOR('',#70297,10.);
#20476=VECTOR('',#70298,10.);
#20477=VECTOR('',#70299,10.);
#20478=VECTOR('',#70306,10.);
#20479=VECTOR('',#70311,10.);
#20480=VECTOR('',#70312,10.);
#20481=VECTOR('',#70313,10.);
#20482=VECTOR('',#70316,10.);
#20483=VECTOR('',#70317,10.);
#20484=VECTOR('',#70318,10.);
#20485=VECTOR('',#70319,10.);
#20486=VECTOR('',#70326,10.);
#20487=VECTOR('',#70331,10.);
#20488=VECTOR('',#70332,10.);
#20489=VECTOR('',#70333,10.);
#20490=VECTOR('',#70336,10.);
#20491=VECTOR('',#70337,10.);
#20492=VECTOR('',#70338,10.);
#20493=VECTOR('',#70339,10.);
#20494=VECTOR('',#70346,10.);
#20495=VECTOR('',#70351,10.);
#20496=VECTOR('',#70352,10.);
#20497=VECTOR('',#70353,10.);
#20498=VECTOR('',#70356,10.);
#20499=VECTOR('',#70357,10.);
#20500=VECTOR('',#70358,10.);
#20501=VECTOR('',#70359,10.);
#20502=VECTOR('',#70366,10.);
#20503=VECTOR('',#70371,10.);
#20504=VECTOR('',#70372,10.);
#20505=VECTOR('',#70373,10.);
#20506=VECTOR('',#70376,10.);
#20507=VECTOR('',#70377,10.);
#20508=VECTOR('',#70378,10.);
#20509=VECTOR('',#70379,10.);
#20510=VECTOR('',#70386,10.);
#20511=VECTOR('',#70391,10.);
#20512=VECTOR('',#70392,10.);
#20513=VECTOR('',#70393,10.);
#20514=VECTOR('',#70396,10.);
#20515=VECTOR('',#70397,10.);
#20516=VECTOR('',#70398,10.);
#20517=VECTOR('',#70399,10.);
#20518=VECTOR('',#70406,10.);
#20519=VECTOR('',#70411,10.);
#20520=VECTOR('',#70412,10.);
#20521=VECTOR('',#70413,10.);
#20522=VECTOR('',#70414,10.);
#20523=VECTOR('',#70421,10.);
#20524=VECTOR('',#70422,10.);
#20525=VECTOR('',#70425,10.);
#20526=VECTOR('',#70426,10.);
#20527=VECTOR('',#70433,2.5);
#20528=VECTOR('',#70446,4.49999999999999);
#20529=VECTOR('',#70451,4.34999999999999);
#20530=VECTOR('',#70458,10.);
#20531=VECTOR('',#70465,1.54999999999999);
#20532=VECTOR('',#70470,10.);
#20533=VECTOR('',#70473,10.);
#20534=VECTOR('',#70474,10.);
#20535=VECTOR('',#70477,10.);
#20536=VECTOR('',#70518,9.60000000000001);
#20537=VECTOR('',#70567,10.);
#20538=VECTOR('',#70570,10.);
#20539=VECTOR('',#70575,10.);
#20540=VECTOR('',#70576,10.);
#20541=VECTOR('',#70583,10.);
#20542=VECTOR('',#70588,9.60000000000001);
#20543=VECTOR('',#70665,10.);
#20544=VECTOR('',#70668,10.);
#20545=VECTOR('',#70671,10.);
#20546=VECTOR('',#70672,10.);
#20547=VECTOR('',#70675,10.);
#20548=VECTOR('',#70678,10.);
#20549=VECTOR('',#70683,10.);
#20550=VECTOR('',#70684,10.);
#20551=VECTOR('',#70689,10.);
#20552=VECTOR('',#70692,10.);
#20553=VECTOR('',#70695,10.);
#20554=VECTOR('',#70698,10.);
#20555=VECTOR('',#70699,10.);
#20556=VECTOR('',#70702,10.);
#20557=VECTOR('',#70705,10.);
#20558=VECTOR('',#70710,10.);
#20559=VECTOR('',#70711,10.);
#20560=VECTOR('',#70716,10.);
#20561=VECTOR('',#70719,10.);
#20562=VECTOR('',#70722,10.);
#20563=VECTOR('',#70725,10.);
#20564=VECTOR('',#70726,10.);
#20565=VECTOR('',#70729,10.);
#20566=VECTOR('',#70732,10.);
#20567=VECTOR('',#70737,10.);
#20568=VECTOR('',#70738,10.);
#20569=VECTOR('',#70743,10.);
#20570=VECTOR('',#70746,10.);
#20571=VECTOR('',#70749,10.);
#20572=VECTOR('',#70752,10.);
#20573=VECTOR('',#70753,10.);
#20574=VECTOR('',#70756,10.);
#20575=VECTOR('',#70759,10.);
#20576=VECTOR('',#70764,10.);
#20577=VECTOR('',#70765,10.);
#20578=VECTOR('',#70770,10.);
#20579=VECTOR('',#70773,10.);
#20580=VECTOR('',#70776,10.);
#20581=VECTOR('',#70779,10.);
#20582=VECTOR('',#70780,10.);
#20583=VECTOR('',#70783,10.);
#20584=VECTOR('',#70786,10.);
#20585=VECTOR('',#70791,10.);
#20586=VECTOR('',#70792,10.);
#20587=VECTOR('',#70797,10.);
#20588=VECTOR('',#70800,10.);
#20589=VECTOR('',#70803,10.);
#20590=VECTOR('',#70806,10.);
#20591=VECTOR('',#70807,10.);
#20592=VECTOR('',#70810,10.);
#20593=VECTOR('',#70813,10.);
#20594=VECTOR('',#70818,10.);
#20595=VECTOR('',#70819,10.);
#20596=VECTOR('',#70824,10.);
#20597=VECTOR('',#70827,10.);
#20598=VECTOR('',#70830,10.);
#20599=VECTOR('',#70833,10.);
#20600=VECTOR('',#70834,10.);
#20601=VECTOR('',#70837,10.);
#20602=VECTOR('',#70840,10.);
#20603=VECTOR('',#70845,10.);
#20604=VECTOR('',#70846,10.);
#20605=VECTOR('',#70851,10.);
#20606=VECTOR('',#70854,10.);
#20607=VECTOR('',#70857,10.);
#20608=VECTOR('',#70860,10.);
#20609=VECTOR('',#70861,10.);
#20610=VECTOR('',#70864,10.);
#20611=VECTOR('',#70867,10.);
#20612=VECTOR('',#70872,10.);
#20613=VECTOR('',#70873,10.);
#20614=VECTOR('',#70878,10.);
#20615=VECTOR('',#70881,10.);
#20616=VECTOR('',#70884,10.);
#20617=VECTOR('',#70887,10.);
#20618=VECTOR('',#70888,10.);
#20619=VECTOR('',#70891,10.);
#20620=VECTOR('',#70894,10.);
#20621=VECTOR('',#70899,10.);
#20622=VECTOR('',#70900,10.);
#20623=VECTOR('',#70905,10.);
#20624=VECTOR('',#70908,10.);
#20625=VECTOR('',#70911,10.);
#20626=VECTOR('',#70914,10.);
#20627=VECTOR('',#70915,10.);
#20628=VECTOR('',#70918,10.);
#20629=VECTOR('',#70921,10.);
#20630=VECTOR('',#70926,10.);
#20631=VECTOR('',#70927,10.);
#20632=VECTOR('',#70932,10.);
#20633=VECTOR('',#70935,10.);
#20634=VECTOR('',#70938,10.);
#20635=VECTOR('',#70941,10.);
#20636=VECTOR('',#70942,10.);
#20637=VECTOR('',#70945,10.);
#20638=VECTOR('',#70948,10.);
#20639=VECTOR('',#70953,10.);
#20640=VECTOR('',#70954,10.);
#20641=VECTOR('',#70959,10.);
#20642=VECTOR('',#70962,10.);
#20643=VECTOR('',#70965,10.);
#20644=VECTOR('',#70968,10.);
#20645=VECTOR('',#70969,10.);
#20646=VECTOR('',#70972,10.);
#20647=VECTOR('',#70975,10.);
#20648=VECTOR('',#70980,10.);
#20649=VECTOR('',#70981,10.);
#20650=VECTOR('',#70986,10.);
#20651=VECTOR('',#70989,10.);
#20652=VECTOR('',#70992,10.);
#20653=VECTOR('',#70995,10.);
#20654=VECTOR('',#70996,10.);
#20655=VECTOR('',#71003,2.66000000000002);
#20656=VECTOR('',#71014,3.85000000000002);
#20657=VECTOR('',#71019,4.);
#20658=VECTOR('',#71024,4.20000000000002);
#20659=VECTOR('',#71033,6.);
#20660=VECTOR('',#71038,6.20000000000001);
#20661=VECTOR('',#71049,7.19999999999999);
#20662=VECTOR('',#71056,1.25500000000001);
#20663=VECTOR('',#71061,2.51000000000001);
#20664=VECTOR('',#71068,2.66000000000002);
#20665=VECTOR('',#71079,4.65);
#20666=VECTOR('',#71084,4.8);
#20667=VECTOR('',#71093,5.85000000000001);
#20668=VECTOR('',#71098,6.);
#20669=VECTOR('',#71105,2.66000000000002);
#20670=VECTOR('',#71110,2.51000000000001);
#20671=VECTOR('',#71117,2.65000000000001);
#20672=VECTOR('',#71122,2.5);
#20673=VECTOR('',#71127,10.);
#20674=VECTOR('',#71128,10.);
#20675=VECTOR('',#71129,10.);
#20676=VECTOR('',#71130,10.);
#20677=VECTOR('',#71135,2.65);
#20678=VECTOR('',#71140,2.5);
#20679=VECTOR('',#71145,10.);
#20680=VECTOR('',#71146,10.);
#20681=VECTOR('',#71147,10.);
#20682=VECTOR('',#71148,10.);
#20683=VECTOR('',#71159,1.45);
#20684=VECTOR('',#71164,1.45);
#20685=VECTOR('',#71169,10.);
#20686=VECTOR('',#71170,10.);
#20687=VECTOR('',#71171,10.);
#20688=VECTOR('',#71172,10.);
#20689=VECTOR('',#71175,10.);
#20690=VECTOR('',#71176,10.);
#20691=VECTOR('',#71177,10.);
#20692=VECTOR('',#71178,10.);
#20693=VECTOR('',#71181,10.);
#20694=VECTOR('',#71182,10.);
#20695=VECTOR('',#71185,10.);
#20696=VECTOR('',#71186,10.);
#20697=VECTOR('',#71189,10.);
#20698=VECTOR('',#71190,10.);
#20699=VECTOR('',#71191,10.);
#20700=VECTOR('',#71194,10.);
#20701=VECTOR('',#71195,10.);
#20702=VECTOR('',#71196,10.);
#20703=VECTOR('',#71199,10.);
#20704=VECTOR('',#71200,10.);
#20705=VECTOR('',#71201,10.);
#20706=VECTOR('',#71204,10.);
#20707=VECTOR('',#71205,10.);
#20708=VECTOR('',#71206,10.);
#20709=VECTOR('',#71209,10.);
#20710=VECTOR('',#71210,10.);
#20711=VECTOR('',#71211,10.);
#20712=VECTOR('',#71214,10.);
#20713=VECTOR('',#71215,10.);
#20714=VECTOR('',#71216,10.);
#20715=VECTOR('',#71219,10.);
#20716=VECTOR('',#71220,10.);
#20717=VECTOR('',#71221,10.);
#20718=VECTOR('',#71224,10.);
#20719=VECTOR('',#71225,10.);
#20720=VECTOR('',#71226,10.);
#20721=VECTOR('',#71229,10.);
#20722=VECTOR('',#71230,10.);
#20723=VECTOR('',#71231,10.);
#20724=VECTOR('',#71234,10.);
#20725=VECTOR('',#71235,10.);
#20726=VECTOR('',#71236,10.);
#20727=VECTOR('',#71239,10.);
#20728=VECTOR('',#71240,10.);
#20729=VECTOR('',#71241,10.);
#20730=VECTOR('',#71244,10.);
#20731=VECTOR('',#71245,10.);
#20732=VECTOR('',#71246,10.);
#20733=VECTOR('',#71249,10.);
#20734=VECTOR('',#71250,10.);
#20735=VECTOR('',#71251,10.);
#20736=VECTOR('',#71254,10.);
#20737=VECTOR('',#71255,10.);
#20738=VECTOR('',#71256,10.);
#20739=VECTOR('',#71259,10.);
#20740=VECTOR('',#71260,10.);
#20741=VECTOR('',#71261,10.);
#20742=VECTOR('',#71264,10.);
#20743=VECTOR('',#71265,10.);
#20744=VECTOR('',#71266,10.);
#20745=VECTOR('',#71269,10.);
#20746=VECTOR('',#71270,10.);
#20747=VECTOR('',#71271,10.);
#20748=VECTOR('',#71274,10.);
#20749=VECTOR('',#71275,10.);
#20750=VECTOR('',#71276,10.);
#20751=VECTOR('',#71279,10.);
#20752=VECTOR('',#71280,10.);
#20753=VECTOR('',#71281,10.);
#20754=VECTOR('',#71284,10.);
#20755=VECTOR('',#71285,10.);
#20756=VECTOR('',#71286,10.);
#20757=VECTOR('',#71289,10.);
#20758=VECTOR('',#71290,10.);
#20759=VECTOR('',#71291,10.);
#20760=VECTOR('',#71294,10.);
#20761=VECTOR('',#71295,10.);
#20762=VECTOR('',#71296,10.);
#20763=VECTOR('',#71299,10.);
#20764=VECTOR('',#71300,10.);
#20765=VECTOR('',#71301,10.);
#20766=VECTOR('',#71304,10.);
#20767=VECTOR('',#71305,10.);
#20768=VECTOR('',#71306,10.);
#20769=VECTOR('',#71309,10.);
#20770=VECTOR('',#71310,10.);
#20771=VECTOR('',#71311,10.);
#20772=VECTOR('',#71314,10.);
#20773=VECTOR('',#71315,10.);
#20774=VECTOR('',#71316,10.);
#20775=VECTOR('',#71319,10.);
#20776=VECTOR('',#71320,10.);
#20777=VECTOR('',#71321,10.);
#20778=VECTOR('',#71324,10.);
#20779=VECTOR('',#71325,10.);
#20780=VECTOR('',#71326,10.);
#20781=VECTOR('',#71329,10.);
#20782=VECTOR('',#71330,10.);
#20783=VECTOR('',#71331,10.);
#20784=VECTOR('',#71334,10.);
#20785=VECTOR('',#71335,10.);
#20786=VECTOR('',#71336,10.);
#20787=VECTOR('',#71339,10.);
#20788=VECTOR('',#71340,10.);
#20789=VECTOR('',#71341,10.);
#20790=VECTOR('',#71344,10.);
#20791=VECTOR('',#71345,10.);
#20792=VECTOR('',#71346,10.);
#20793=VECTOR('',#71349,10.);
#20794=VECTOR('',#71350,10.);
#20795=VECTOR('',#71351,10.);
#20796=VECTOR('',#71354,10.);
#20797=VECTOR('',#71355,10.);
#20798=VECTOR('',#71356,10.);
#20799=VECTOR('',#71359,10.);
#20800=VECTOR('',#71360,10.);
#20801=VECTOR('',#71361,10.);
#20802=VECTOR('',#71364,10.);
#20803=VECTOR('',#71365,10.);
#20804=VECTOR('',#71366,10.);
#20805=VECTOR('',#71369,10.);
#20806=VECTOR('',#71370,10.);
#20807=VECTOR('',#71371,10.);
#20808=VECTOR('',#71374,10.);
#20809=VECTOR('',#71375,10.);
#20810=VECTOR('',#71376,10.);
#20811=VECTOR('',#71379,10.);
#20812=VECTOR('',#71380,10.);
#20813=VECTOR('',#71381,10.);
#20814=VECTOR('',#71384,10.);
#20815=VECTOR('',#71385,10.);
#20816=VECTOR('',#71386,10.);
#20817=VECTOR('',#71389,10.);
#20818=VECTOR('',#71390,10.);
#20819=VECTOR('',#71391,10.);
#20820=VECTOR('',#71394,10.);
#20821=VECTOR('',#71395,10.);
#20822=VECTOR('',#71396,10.);
#20823=VECTOR('',#71399,10.);
#20824=VECTOR('',#71400,10.);
#20825=VECTOR('',#71401,10.);
#20826=VECTOR('',#71404,10.);
#20827=VECTOR('',#71405,10.);
#20828=VECTOR('',#71406,10.);
#20829=VECTOR('',#71409,10.);
#20830=VECTOR('',#71410,10.);
#20831=VECTOR('',#71411,10.);
#20832=VECTOR('',#71414,10.);
#20833=VECTOR('',#71415,10.);
#20834=VECTOR('',#71416,10.);
#20835=VECTOR('',#71419,10.);
#20836=VECTOR('',#71420,10.);
#20837=VECTOR('',#71421,10.);
#20838=VECTOR('',#71424,10.);
#20839=VECTOR('',#71425,10.);
#20840=VECTOR('',#71426,10.);
#20841=VECTOR('',#71429,10.);
#20842=VECTOR('',#71430,10.);
#20843=VECTOR('',#71431,10.);
#20844=VECTOR('',#71434,10.);
#20845=VECTOR('',#71435,10.);
#20846=VECTOR('',#71436,10.);
#20847=VECTOR('',#71439,10.);
#20848=VECTOR('',#71440,10.);
#20849=VECTOR('',#71441,10.);
#20850=VECTOR('',#71444,10.);
#20851=VECTOR('',#71445,10.);
#20852=VECTOR('',#71446,10.);
#20853=VECTOR('',#71449,10.);
#20854=VECTOR('',#71450,10.);
#20855=VECTOR('',#71451,10.);
#20856=VECTOR('',#71454,10.);
#20857=VECTOR('',#71455,10.);
#20858=VECTOR('',#71456,10.);
#20859=VECTOR('',#71459,10.);
#20860=VECTOR('',#71460,10.);
#20861=VECTOR('',#71461,10.);
#20862=VECTOR('',#71464,10.);
#20863=VECTOR('',#71465,10.);
#20864=VECTOR('',#71466,10.);
#20865=VECTOR('',#71469,10.);
#20866=VECTOR('',#71470,10.);
#20867=VECTOR('',#71471,10.);
#20868=VECTOR('',#71474,10.);
#20869=VECTOR('',#71475,10.);
#20870=VECTOR('',#71476,10.);
#20871=VECTOR('',#71479,10.);
#20872=VECTOR('',#71480,10.);
#20873=VECTOR('',#71481,10.);
#20874=VECTOR('',#71484,10.);
#20875=VECTOR('',#71485,10.);
#20876=VECTOR('',#71486,10.);
#20877=VECTOR('',#71489,10.);
#20878=VECTOR('',#71490,10.);
#20879=VECTOR('',#71491,10.);
#20880=VECTOR('',#71494,10.);
#20881=VECTOR('',#71495,10.);
#20882=VECTOR('',#71496,10.);
#20883=VECTOR('',#71499,10.);
#20884=VECTOR('',#71500,10.);
#20885=VECTOR('',#71501,10.);
#20886=VECTOR('',#71504,10.);
#20887=VECTOR('',#71505,10.);
#20888=VECTOR('',#71506,10.);
#20889=VECTOR('',#71509,10.);
#20890=VECTOR('',#71510,10.);
#20891=VECTOR('',#71511,10.);
#20892=VECTOR('',#71514,10.);
#20893=VECTOR('',#71515,10.);
#20894=VECTOR('',#71516,10.);
#20895=VECTOR('',#71519,10.);
#20896=VECTOR('',#71520,10.);
#20897=VECTOR('',#71521,10.);
#20898=VECTOR('',#71524,10.);
#20899=VECTOR('',#71525,10.);
#20900=VECTOR('',#71526,10.);
#20901=VECTOR('',#71529,10.);
#20902=VECTOR('',#71530,10.);
#20903=VECTOR('',#71531,10.);
#20904=VECTOR('',#71534,10.);
#20905=VECTOR('',#71535,10.);
#20906=VECTOR('',#71536,10.);
#20907=VECTOR('',#71539,10.);
#20908=VECTOR('',#71540,10.);
#20909=VECTOR('',#71541,10.);
#20910=VECTOR('',#71544,10.);
#20911=VECTOR('',#71545,10.);
#20912=VECTOR('',#71546,10.);
#20913=VECTOR('',#71549,10.);
#20914=VECTOR('',#71550,10.);
#20915=VECTOR('',#71551,10.);
#20916=VECTOR('',#71554,10.);
#20917=VECTOR('',#71555,10.);
#20918=VECTOR('',#71556,10.);
#20919=VECTOR('',#71559,10.);
#20920=VECTOR('',#71560,10.);
#20921=VECTOR('',#71561,10.);
#20922=VECTOR('',#71564,10.);
#20923=VECTOR('',#71565,10.);
#20924=VECTOR('',#71566,10.);
#20925=VECTOR('',#71569,10.);
#20926=VECTOR('',#71570,10.);
#20927=VECTOR('',#71571,10.);
#20928=VECTOR('',#71574,10.);
#20929=VECTOR('',#71575,10.);
#20930=VECTOR('',#71576,10.);
#20931=VECTOR('',#71579,10.);
#20932=VECTOR('',#71580,10.);
#20933=VECTOR('',#71581,10.);
#20934=VECTOR('',#71584,10.);
#20935=VECTOR('',#71585,10.);
#20936=VECTOR('',#71586,10.);
#20937=VECTOR('',#71589,10.);
#20938=VECTOR('',#71590,10.);
#20939=VECTOR('',#71591,10.);
#20940=VECTOR('',#71594,10.);
#20941=VECTOR('',#71595,10.);
#20942=VECTOR('',#71596,10.);
#20943=VECTOR('',#71599,10.);
#20944=VECTOR('',#71600,10.);
#20945=VECTOR('',#71601,10.);
#20946=VECTOR('',#71604,10.);
#20947=VECTOR('',#71605,10.);
#20948=VECTOR('',#71606,10.);
#20949=VECTOR('',#71609,10.);
#20950=VECTOR('',#71610,10.);
#20951=VECTOR('',#71611,10.);
#20952=VECTOR('',#71614,10.);
#20953=VECTOR('',#71615,10.);
#20954=VECTOR('',#71616,10.);
#20955=VECTOR('',#71619,10.);
#20956=VECTOR('',#71620,10.);
#20957=VECTOR('',#71621,10.);
#20958=VECTOR('',#71624,10.);
#20959=VECTOR('',#71625,10.);
#20960=VECTOR('',#71626,10.);
#20961=VECTOR('',#71629,10.);
#20962=VECTOR('',#71630,10.);
#20963=VECTOR('',#71631,10.);
#20964=VECTOR('',#71634,10.);
#20965=VECTOR('',#71635,10.);
#20966=VECTOR('',#71636,10.);
#20967=VECTOR('',#71639,10.);
#20968=VECTOR('',#71640,10.);
#20969=VECTOR('',#71641,10.);
#20970=VECTOR('',#71644,10.);
#20971=VECTOR('',#71645,10.);
#20972=VECTOR('',#71646,10.);
#20973=VECTOR('',#71649,10.);
#20974=VECTOR('',#71650,10.);
#20975=VECTOR('',#71651,10.);
#20976=VECTOR('',#71654,10.);
#20977=VECTOR('',#71655,10.);
#20978=VECTOR('',#71656,10.);
#20979=VECTOR('',#71659,10.);
#20980=VECTOR('',#71660,10.);
#20981=VECTOR('',#71661,10.);
#20982=VECTOR('',#71664,10.);
#20983=VECTOR('',#71665,10.);
#20984=VECTOR('',#71666,10.);
#20985=VECTOR('',#71669,10.);
#20986=VECTOR('',#71670,10.);
#20987=VECTOR('',#71671,10.);
#20988=VECTOR('',#71674,10.);
#20989=VECTOR('',#71675,10.);
#20990=VECTOR('',#71676,10.);
#20991=VECTOR('',#71679,10.);
#20992=VECTOR('',#71680,10.);
#20993=VECTOR('',#71681,10.);
#20994=VECTOR('',#71684,10.);
#20995=VECTOR('',#71685,10.);
#20996=VECTOR('',#71686,10.);
#20997=VECTOR('',#71689,10.);
#20998=VECTOR('',#71690,10.);
#20999=VECTOR('',#71691,10.);
#21000=VECTOR('',#71694,10.);
#21001=VECTOR('',#71695,10.);
#21002=VECTOR('',#71696,10.);
#21003=VECTOR('',#71699,10.);
#21004=VECTOR('',#71700,10.);
#21005=VECTOR('',#71701,10.);
#21006=VECTOR('',#71704,10.);
#21007=VECTOR('',#71705,10.);
#21008=VECTOR('',#71706,10.);
#21009=VECTOR('',#71709,10.);
#21010=VECTOR('',#71710,10.);
#21011=VECTOR('',#71711,10.);
#21012=VECTOR('',#71714,10.);
#21013=VECTOR('',#71715,10.);
#21014=VECTOR('',#71716,10.);
#21015=VECTOR('',#71719,10.);
#21016=VECTOR('',#71720,10.);
#21017=VECTOR('',#71721,10.);
#21018=VECTOR('',#71724,10.);
#21019=VECTOR('',#71725,10.);
#21020=VECTOR('',#71726,10.);
#21021=VECTOR('',#71729,10.);
#21022=VECTOR('',#71730,10.);
#21023=VECTOR('',#71731,10.);
#21024=VECTOR('',#71734,10.);
#21025=VECTOR('',#71735,10.);
#21026=VECTOR('',#71736,10.);
#21027=VECTOR('',#71739,10.);
#21028=VECTOR('',#71740,10.);
#21029=VECTOR('',#71741,10.);
#21030=VECTOR('',#71744,10.);
#21031=VECTOR('',#71745,10.);
#21032=VECTOR('',#71746,10.);
#21033=VECTOR('',#71749,10.);
#21034=VECTOR('',#71750,10.);
#21035=VECTOR('',#71751,10.);
#21036=VECTOR('',#71754,10.);
#21037=VECTOR('',#71755,10.);
#21038=VECTOR('',#71756,10.);
#21039=VECTOR('',#71759,10.);
#21040=VECTOR('',#71760,10.);
#21041=VECTOR('',#71761,10.);
#21042=VECTOR('',#71764,10.);
#21043=VECTOR('',#71765,10.);
#21044=VECTOR('',#71766,10.);
#21045=VECTOR('',#71769,10.);
#21046=VECTOR('',#71770,10.);
#21047=VECTOR('',#71771,10.);
#21048=VECTOR('',#71774,10.);
#21049=VECTOR('',#71775,10.);
#21050=VECTOR('',#71776,10.);
#21051=VECTOR('',#71779,10.);
#21052=VECTOR('',#71780,10.);
#21053=VECTOR('',#71781,10.);
#21054=VECTOR('',#71784,10.);
#21055=VECTOR('',#71785,10.);
#21056=VECTOR('',#71786,10.);
#21057=VECTOR('',#71789,10.);
#21058=VECTOR('',#71790,10.);
#21059=VECTOR('',#71791,10.);
#21060=VECTOR('',#71794,10.);
#21061=VECTOR('',#71795,10.);
#21062=VECTOR('',#71796,10.);
#21063=VECTOR('',#71799,10.);
#21064=VECTOR('',#71800,10.);
#21065=VECTOR('',#71801,10.);
#21066=VECTOR('',#71804,10.);
#21067=VECTOR('',#71805,10.);
#21068=VECTOR('',#71806,10.);
#21069=VECTOR('',#71809,10.);
#21070=VECTOR('',#71810,10.);
#21071=VECTOR('',#71811,10.);
#21072=VECTOR('',#71814,10.);
#21073=VECTOR('',#71815,10.);
#21074=VECTOR('',#71816,10.);
#21075=VECTOR('',#71819,10.);
#21076=VECTOR('',#71820,10.);
#21077=VECTOR('',#71821,10.);
#21078=VECTOR('',#71824,10.);
#21079=VECTOR('',#71825,10.);
#21080=VECTOR('',#71826,10.);
#21081=VECTOR('',#71829,10.);
#21082=VECTOR('',#71830,10.);
#21083=VECTOR('',#71831,10.);
#21084=VECTOR('',#71834,10.);
#21085=VECTOR('',#71835,10.);
#21086=VECTOR('',#71836,10.);
#21087=VECTOR('',#71839,10.);
#21088=VECTOR('',#71840,10.);
#21089=VECTOR('',#71841,10.);
#21090=VECTOR('',#71844,10.);
#21091=VECTOR('',#71845,10.);
#21092=VECTOR('',#71846,10.);
#21093=VECTOR('',#71849,10.);
#21094=VECTOR('',#71850,10.);
#21095=VECTOR('',#71851,10.);
#21096=VECTOR('',#71854,10.);
#21097=VECTOR('',#71855,10.);
#21098=VECTOR('',#71856,10.);
#21099=VECTOR('',#71859,10.);
#21100=VECTOR('',#71860,10.);
#21101=VECTOR('',#71861,10.);
#21102=VECTOR('',#71864,10.);
#21103=VECTOR('',#71865,10.);
#21104=VECTOR('',#71866,10.);
#21105=VECTOR('',#71869,10.);
#21106=VECTOR('',#71870,10.);
#21107=VECTOR('',#71871,10.);
#21108=VECTOR('',#71874,10.);
#21109=VECTOR('',#71875,10.);
#21110=VECTOR('',#71876,10.);
#21111=VECTOR('',#71879,10.);
#21112=VECTOR('',#71880,10.);
#21113=VECTOR('',#71881,10.);
#21114=VECTOR('',#71884,10.);
#21115=VECTOR('',#71885,10.);
#21116=VECTOR('',#71886,10.);
#21117=VECTOR('',#71889,10.);
#21118=VECTOR('',#71890,10.);
#21119=VECTOR('',#71891,10.);
#21120=VECTOR('',#71894,10.);
#21121=VECTOR('',#71895,10.);
#21122=VECTOR('',#71896,10.);
#21123=VECTOR('',#71899,10.);
#21124=VECTOR('',#71900,10.);
#21125=VECTOR('',#71901,10.);
#21126=VECTOR('',#71904,10.);
#21127=VECTOR('',#71905,10.);
#21128=VECTOR('',#71906,10.);
#21129=VECTOR('',#71909,10.);
#21130=VECTOR('',#71910,10.);
#21131=VECTOR('',#71911,10.);
#21132=VECTOR('',#71914,10.);
#21133=VECTOR('',#71915,10.);
#21134=VECTOR('',#71916,10.);
#21135=VECTOR('',#71919,10.);
#21136=VECTOR('',#71920,10.);
#21137=VECTOR('',#71921,10.);
#21138=VECTOR('',#71924,10.);
#21139=VECTOR('',#71925,10.);
#21140=VECTOR('',#71926,10.);
#21141=VECTOR('',#71929,10.);
#21142=VECTOR('',#71930,10.);
#21143=VECTOR('',#71931,10.);
#21144=VECTOR('',#71934,10.);
#21145=VECTOR('',#71935,10.);
#21146=VECTOR('',#71936,10.);
#21147=VECTOR('',#71939,10.);
#21148=VECTOR('',#71940,10.);
#21149=VECTOR('',#71941,10.);
#21150=VECTOR('',#71944,10.);
#21151=VECTOR('',#71945,10.);
#21152=VECTOR('',#71946,10.);
#21153=VECTOR('',#71949,10.);
#21154=VECTOR('',#71950,10.);
#21155=VECTOR('',#71951,10.);
#21156=VECTOR('',#71954,10.);
#21157=VECTOR('',#71955,10.);
#21158=VECTOR('',#71956,10.);
#21159=VECTOR('',#71959,10.);
#21160=VECTOR('',#71960,10.);
#21161=VECTOR('',#71961,10.);
#21162=VECTOR('',#71964,10.);
#21163=VECTOR('',#71965,10.);
#21164=VECTOR('',#71966,10.);
#21165=VECTOR('',#71969,10.);
#21166=VECTOR('',#71970,10.);
#21167=VECTOR('',#71971,10.);
#21168=VECTOR('',#71974,10.);
#21169=VECTOR('',#71975,10.);
#21170=VECTOR('',#71976,10.);
#21171=VECTOR('',#71979,10.);
#21172=VECTOR('',#71980,10.);
#21173=VECTOR('',#71981,10.);
#21174=VECTOR('',#71984,10.);
#21175=VECTOR('',#71985,10.);
#21176=VECTOR('',#71986,10.);
#21177=VECTOR('',#71989,10.);
#21178=VECTOR('',#71990,10.);
#21179=VECTOR('',#71991,10.);
#21180=VECTOR('',#71994,10.);
#21181=VECTOR('',#71995,10.);
#21182=VECTOR('',#71996,10.);
#21183=VECTOR('',#71999,10.);
#21184=VECTOR('',#72000,10.);
#21185=VECTOR('',#72001,10.);
#21186=VECTOR('',#72004,10.);
#21187=VECTOR('',#72005,10.);
#21188=VECTOR('',#72006,10.);
#21189=VECTOR('',#72009,10.);
#21190=VECTOR('',#72010,10.);
#21191=VECTOR('',#72011,10.);
#21192=VECTOR('',#72014,10.);
#21193=VECTOR('',#72015,10.);
#21194=VECTOR('',#72016,10.);
#21195=VECTOR('',#72019,10.);
#21196=VECTOR('',#72020,10.);
#21197=VECTOR('',#72021,10.);
#21198=VECTOR('',#72024,10.);
#21199=VECTOR('',#72025,10.);
#21200=VECTOR('',#72026,10.);
#21201=VECTOR('',#72029,10.);
#21202=VECTOR('',#72030,10.);
#21203=VECTOR('',#72031,10.);
#21204=VECTOR('',#72034,10.);
#21205=VECTOR('',#72035,10.);
#21206=VECTOR('',#72036,10.);
#21207=VECTOR('',#72039,10.);
#21208=VECTOR('',#72040,10.);
#21209=VECTOR('',#72041,10.);
#21210=VECTOR('',#72044,10.);
#21211=VECTOR('',#72045,10.);
#21212=VECTOR('',#72046,10.);
#21213=VECTOR('',#72049,10.);
#21214=VECTOR('',#72050,10.);
#21215=VECTOR('',#72051,10.);
#21216=VECTOR('',#72054,10.);
#21217=VECTOR('',#72055,10.);
#21218=VECTOR('',#72056,10.);
#21219=VECTOR('',#72059,10.);
#21220=VECTOR('',#72060,10.);
#21221=VECTOR('',#72061,10.);
#21222=VECTOR('',#72064,10.);
#21223=VECTOR('',#72065,10.);
#21224=VECTOR('',#72066,10.);
#21225=VECTOR('',#72069,10.);
#21226=VECTOR('',#72070,10.);
#21227=VECTOR('',#72071,10.);
#21228=VECTOR('',#72074,10.);
#21229=VECTOR('',#72075,10.);
#21230=VECTOR('',#72076,10.);
#21231=VECTOR('',#72079,10.);
#21232=VECTOR('',#72080,10.);
#21233=VECTOR('',#72081,10.);
#21234=VECTOR('',#72084,10.);
#21235=VECTOR('',#72085,10.);
#21236=VECTOR('',#72086,10.);
#21237=VECTOR('',#72089,10.);
#21238=VECTOR('',#72090,10.);
#21239=VECTOR('',#72091,10.);
#21240=VECTOR('',#72094,10.);
#21241=VECTOR('',#72095,10.);
#21242=VECTOR('',#72096,10.);
#21243=VECTOR('',#72099,10.);
#21244=VECTOR('',#72100,10.);
#21245=VECTOR('',#72101,10.);
#21246=VECTOR('',#72104,10.);
#21247=VECTOR('',#72105,10.);
#21248=VECTOR('',#72106,10.);
#21249=VECTOR('',#72109,10.);
#21250=VECTOR('',#72110,10.);
#21251=VECTOR('',#72111,10.);
#21252=VECTOR('',#72114,10.);
#21253=VECTOR('',#72115,10.);
#21254=VECTOR('',#72116,10.);
#21255=VECTOR('',#72119,10.);
#21256=VECTOR('',#72120,10.);
#21257=VECTOR('',#72121,10.);
#21258=VECTOR('',#72124,10.);
#21259=VECTOR('',#72125,10.);
#21260=VECTOR('',#72126,10.);
#21261=VECTOR('',#72129,10.);
#21262=VECTOR('',#72130,10.);
#21263=VECTOR('',#72131,10.);
#21264=VECTOR('',#72134,10.);
#21265=VECTOR('',#72135,10.);
#21266=VECTOR('',#72136,10.);
#21267=VECTOR('',#72139,10.);
#21268=VECTOR('',#72140,10.);
#21269=VECTOR('',#72141,10.);
#21270=VECTOR('',#72144,10.);
#21271=VECTOR('',#72145,10.);
#21272=VECTOR('',#72146,10.);
#21273=VECTOR('',#72149,10.);
#21274=VECTOR('',#72150,10.);
#21275=VECTOR('',#72151,10.);
#21276=VECTOR('',#72154,10.);
#21277=VECTOR('',#72155,10.);
#21278=VECTOR('',#72156,10.);
#21279=VECTOR('',#72159,10.);
#21280=VECTOR('',#72160,10.);
#21281=VECTOR('',#72161,10.);
#21282=VECTOR('',#72164,10.);
#21283=VECTOR('',#72165,10.);
#21284=VECTOR('',#72166,10.);
#21285=VECTOR('',#72169,10.);
#21286=VECTOR('',#72170,10.);
#21287=VECTOR('',#72171,10.);
#21288=VECTOR('',#72174,10.);
#21289=VECTOR('',#72175,10.);
#21290=VECTOR('',#72176,10.);
#21291=VECTOR('',#72179,10.);
#21292=VECTOR('',#72180,10.);
#21293=VECTOR('',#72181,10.);
#21294=VECTOR('',#72184,10.);
#21295=VECTOR('',#72185,10.);
#21296=VECTOR('',#72186,10.);
#21297=VECTOR('',#72189,10.);
#21298=VECTOR('',#72190,10.);
#21299=VECTOR('',#72191,10.);
#21300=VECTOR('',#72194,10.);
#21301=VECTOR('',#72195,10.);
#21302=VECTOR('',#72196,10.);
#21303=VECTOR('',#72199,10.);
#21304=VECTOR('',#72200,10.);
#21305=VECTOR('',#72201,10.);
#21306=VECTOR('',#72204,10.);
#21307=VECTOR('',#72205,10.);
#21308=VECTOR('',#72206,10.);
#21309=VECTOR('',#72209,10.);
#21310=VECTOR('',#72210,10.);
#21311=VECTOR('',#72211,10.);
#21312=VECTOR('',#72214,10.);
#21313=VECTOR('',#72215,10.);
#21314=VECTOR('',#72216,10.);
#21315=VECTOR('',#72219,10.);
#21316=VECTOR('',#72220,10.);
#21317=VECTOR('',#72221,10.);
#21318=VECTOR('',#72224,10.);
#21319=VECTOR('',#72225,10.);
#21320=VECTOR('',#72226,10.);
#21321=VECTOR('',#72229,10.);
#21322=VECTOR('',#72230,10.);
#21323=VECTOR('',#72231,10.);
#21324=VECTOR('',#72234,10.);
#21325=VECTOR('',#72235,10.);
#21326=VECTOR('',#72236,10.);
#21327=VECTOR('',#72239,10.);
#21328=VECTOR('',#72240,10.);
#21329=VECTOR('',#72241,10.);
#21330=VECTOR('',#72244,10.);
#21331=VECTOR('',#72245,10.);
#21332=VECTOR('',#72246,10.);
#21333=VECTOR('',#72249,10.);
#21334=VECTOR('',#72250,10.);
#21335=VECTOR('',#72251,10.);
#21336=VECTOR('',#72254,10.);
#21337=VECTOR('',#72255,10.);
#21338=VECTOR('',#72256,10.);
#21339=VECTOR('',#72259,10.);
#21340=VECTOR('',#72260,10.);
#21341=VECTOR('',#72261,10.);
#21342=VECTOR('',#72264,10.);
#21343=VECTOR('',#72265,10.);
#21344=VECTOR('',#72266,10.);
#21345=VECTOR('',#72269,10.);
#21346=VECTOR('',#72270,10.);
#21347=VECTOR('',#72271,10.);
#21348=VECTOR('',#72274,10.);
#21349=VECTOR('',#72275,10.);
#21350=VECTOR('',#72276,10.);
#21351=VECTOR('',#72279,10.);
#21352=VECTOR('',#72280,10.);
#21353=VECTOR('',#72281,10.);
#21354=VECTOR('',#72284,10.);
#21355=VECTOR('',#72285,10.);
#21356=VECTOR('',#72286,10.);
#21357=VECTOR('',#72289,10.);
#21358=VECTOR('',#72290,10.);
#21359=VECTOR('',#72291,10.);
#21360=VECTOR('',#72294,10.);
#21361=VECTOR('',#72295,10.);
#21362=VECTOR('',#72296,10.);
#21363=VECTOR('',#72299,10.);
#21364=VECTOR('',#72300,10.);
#21365=VECTOR('',#72301,10.);
#21366=VECTOR('',#72304,10.);
#21367=VECTOR('',#72305,10.);
#21368=VECTOR('',#72306,10.);
#21369=VECTOR('',#72309,10.);
#21370=VECTOR('',#72310,10.);
#21371=VECTOR('',#72311,10.);
#21372=VECTOR('',#72314,10.);
#21373=VECTOR('',#72315,10.);
#21374=VECTOR('',#72316,10.);
#21375=VECTOR('',#72319,10.);
#21376=VECTOR('',#72320,10.);
#21377=VECTOR('',#72321,10.);
#21378=VECTOR('',#72324,10.);
#21379=VECTOR('',#72325,10.);
#21380=VECTOR('',#72326,10.);
#21381=VECTOR('',#72329,10.);
#21382=VECTOR('',#72330,10.);
#21383=VECTOR('',#72331,10.);
#21384=VECTOR('',#72334,10.);
#21385=VECTOR('',#72335,10.);
#21386=VECTOR('',#72336,10.);
#21387=VECTOR('',#72339,10.);
#21388=VECTOR('',#72340,10.);
#21389=VECTOR('',#72341,10.);
#21390=VECTOR('',#72344,10.);
#21391=VECTOR('',#72345,10.);
#21392=VECTOR('',#72346,10.);
#21393=VECTOR('',#72349,10.);
#21394=VECTOR('',#72350,10.);
#21395=VECTOR('',#72351,10.);
#21396=VECTOR('',#72354,10.);
#21397=VECTOR('',#72355,10.);
#21398=VECTOR('',#72356,10.);
#21399=VECTOR('',#72359,10.);
#21400=VECTOR('',#72360,10.);
#21401=VECTOR('',#72361,10.);
#21402=VECTOR('',#72364,10.);
#21403=VECTOR('',#72365,10.);
#21404=VECTOR('',#72366,10.);
#21405=VECTOR('',#72369,10.);
#21406=VECTOR('',#72370,10.);
#21407=VECTOR('',#72371,10.);
#21408=VECTOR('',#72374,10.);
#21409=VECTOR('',#72375,10.);
#21410=VECTOR('',#72376,10.);
#21411=VECTOR('',#72379,10.);
#21412=VECTOR('',#72380,10.);
#21413=VECTOR('',#72381,10.);
#21414=VECTOR('',#72384,10.);
#21415=VECTOR('',#72385,10.);
#21416=VECTOR('',#72386,10.);
#21417=VECTOR('',#72389,10.);
#21418=VECTOR('',#72390,10.);
#21419=VECTOR('',#72391,10.);
#21420=VECTOR('',#72394,10.);
#21421=VECTOR('',#72395,10.);
#21422=VECTOR('',#72396,10.);
#21423=VECTOR('',#72399,10.);
#21424=VECTOR('',#72400,10.);
#21425=VECTOR('',#72401,10.);
#21426=VECTOR('',#72404,10.);
#21427=VECTOR('',#72405,10.);
#21428=VECTOR('',#72406,10.);
#21429=VECTOR('',#72409,10.);
#21430=VECTOR('',#72410,10.);
#21431=VECTOR('',#72411,10.);
#21432=VECTOR('',#72414,10.);
#21433=VECTOR('',#72415,10.);
#21434=VECTOR('',#72416,10.);
#21435=VECTOR('',#72419,10.);
#21436=VECTOR('',#72420,10.);
#21437=VECTOR('',#72421,10.);
#21438=VECTOR('',#72424,10.);
#21439=VECTOR('',#72425,10.);
#21440=VECTOR('',#72426,10.);
#21441=VECTOR('',#72429,10.);
#21442=VECTOR('',#72430,10.);
#21443=VECTOR('',#72431,10.);
#21444=VECTOR('',#72434,10.);
#21445=VECTOR('',#72435,10.);
#21446=VECTOR('',#72436,10.);
#21447=VECTOR('',#72439,10.);
#21448=VECTOR('',#72440,10.);
#21449=VECTOR('',#72441,10.);
#21450=VECTOR('',#72444,10.);
#21451=VECTOR('',#72445,10.);
#21452=VECTOR('',#72446,10.);
#21453=VECTOR('',#72449,10.);
#21454=VECTOR('',#72450,10.);
#21455=VECTOR('',#72451,10.);
#21456=VECTOR('',#72454,10.);
#21457=VECTOR('',#72455,10.);
#21458=VECTOR('',#72456,10.);
#21459=VECTOR('',#72459,10.);
#21460=VECTOR('',#72460,10.);
#21461=VECTOR('',#72461,10.);
#21462=VECTOR('',#72464,10.);
#21463=VECTOR('',#72465,10.);
#21464=VECTOR('',#72466,10.);
#21465=VECTOR('',#72469,10.);
#21466=VECTOR('',#72470,10.);
#21467=VECTOR('',#72471,10.);
#21468=VECTOR('',#72474,10.);
#21469=VECTOR('',#72475,10.);
#21470=VECTOR('',#72476,10.);
#21471=VECTOR('',#72479,10.);
#21472=VECTOR('',#72480,10.);
#21473=VECTOR('',#72481,10.);
#21474=VECTOR('',#72484,10.);
#21475=VECTOR('',#72485,10.);
#21476=VECTOR('',#72486,10.);
#21477=VECTOR('',#72489,10.);
#21478=VECTOR('',#72490,10.);
#21479=VECTOR('',#72491,10.);
#21480=VECTOR('',#72494,10.);
#21481=VECTOR('',#72495,10.);
#21482=VECTOR('',#72496,10.);
#21483=VECTOR('',#72499,10.);
#21484=VECTOR('',#72500,10.);
#21485=VECTOR('',#72501,10.);
#21486=VECTOR('',#72504,10.);
#21487=VECTOR('',#72505,10.);
#21488=VECTOR('',#72506,10.);
#21489=VECTOR('',#72509,10.);
#21490=VECTOR('',#72510,10.);
#21491=VECTOR('',#72511,10.);
#21492=VECTOR('',#72514,10.);
#21493=VECTOR('',#72515,10.);
#21494=VECTOR('',#72516,10.);
#21495=VECTOR('',#72519,10.);
#21496=VECTOR('',#72520,10.);
#21497=VECTOR('',#72521,10.);
#21498=VECTOR('',#72524,10.);
#21499=VECTOR('',#72525,10.);
#21500=VECTOR('',#72526,10.);
#21501=VECTOR('',#72529,10.);
#21502=VECTOR('',#72530,10.);
#21503=VECTOR('',#72531,10.);
#21504=VECTOR('',#72534,10.);
#21505=VECTOR('',#72535,10.);
#21506=VECTOR('',#72536,10.);
#21507=VECTOR('',#72539,10.);
#21508=VECTOR('',#72540,10.);
#21509=VECTOR('',#72541,10.);
#21510=VECTOR('',#72544,10.);
#21511=VECTOR('',#72545,10.);
#21512=VECTOR('',#72546,10.);
#21513=VECTOR('',#72549,10.);
#21514=VECTOR('',#72550,10.);
#21515=VECTOR('',#72551,10.);
#21516=VECTOR('',#72554,10.);
#21517=VECTOR('',#72555,10.);
#21518=VECTOR('',#72556,10.);
#21519=VECTOR('',#72559,10.);
#21520=VECTOR('',#72560,10.);
#21521=VECTOR('',#72561,10.);
#21522=VECTOR('',#72564,10.);
#21523=VECTOR('',#72565,10.);
#21524=VECTOR('',#72566,10.);
#21525=VECTOR('',#72569,10.);
#21526=VECTOR('',#72570,10.);
#21527=VECTOR('',#72571,10.);
#21528=VECTOR('',#72574,10.);
#21529=VECTOR('',#72575,10.);
#21530=VECTOR('',#72576,10.);
#21531=VECTOR('',#72579,10.);
#21532=VECTOR('',#72580,10.);
#21533=VECTOR('',#72581,10.);
#21534=VECTOR('',#72584,10.);
#21535=VECTOR('',#72585,10.);
#21536=VECTOR('',#72586,10.);
#21537=VECTOR('',#72589,10.);
#21538=VECTOR('',#72590,10.);
#21539=VECTOR('',#72591,10.);
#21540=VECTOR('',#72594,10.);
#21541=VECTOR('',#72595,10.);
#21542=VECTOR('',#72596,10.);
#21543=VECTOR('',#72599,10.);
#21544=VECTOR('',#72600,10.);
#21545=VECTOR('',#72601,10.);
#21546=VECTOR('',#72604,10.);
#21547=VECTOR('',#72605,10.);
#21548=VECTOR('',#72606,10.);
#21549=VECTOR('',#72609,10.);
#21550=VECTOR('',#72610,10.);
#21551=VECTOR('',#72611,10.);
#21552=VECTOR('',#72614,10.);
#21553=VECTOR('',#72615,10.);
#21554=VECTOR('',#72616,10.);
#21555=VECTOR('',#72619,10.);
#21556=VECTOR('',#72620,10.);
#21557=VECTOR('',#72621,10.);
#21558=VECTOR('',#72624,10.);
#21559=VECTOR('',#72625,10.);
#21560=VECTOR('',#72626,10.);
#21561=VECTOR('',#72629,10.);
#21562=VECTOR('',#72630,10.);
#21563=VECTOR('',#72631,10.);
#21564=VECTOR('',#72634,10.);
#21565=VECTOR('',#72635,10.);
#21566=VECTOR('',#72636,10.);
#21567=VECTOR('',#72639,10.);
#21568=VECTOR('',#72640,10.);
#21569=VECTOR('',#72641,10.);
#21570=VECTOR('',#72644,10.);
#21571=VECTOR('',#72645,10.);
#21572=VECTOR('',#72646,10.);
#21573=VECTOR('',#72649,10.);
#21574=VECTOR('',#72650,10.);
#21575=VECTOR('',#72651,10.);
#21576=VECTOR('',#72654,10.);
#21577=VECTOR('',#72655,10.);
#21578=VECTOR('',#72656,10.);
#21579=VECTOR('',#72659,10.);
#21580=VECTOR('',#72660,10.);
#21581=VECTOR('',#72661,10.);
#21582=VECTOR('',#72664,10.);
#21583=VECTOR('',#72665,10.);
#21584=VECTOR('',#72666,10.);
#21585=VECTOR('',#72669,10.);
#21586=VECTOR('',#72670,10.);
#21587=VECTOR('',#72671,10.);
#21588=VECTOR('',#72674,10.);
#21589=VECTOR('',#72675,10.);
#21590=VECTOR('',#72676,10.);
#21591=VECTOR('',#72679,10.);
#21592=VECTOR('',#72680,10.);
#21593=VECTOR('',#72681,10.);
#21594=VECTOR('',#72684,10.);
#21595=VECTOR('',#72685,10.);
#21596=VECTOR('',#72686,10.);
#21597=VECTOR('',#72689,10.);
#21598=VECTOR('',#72690,10.);
#21599=VECTOR('',#72691,10.);
#21600=VECTOR('',#72694,10.);
#21601=VECTOR('',#72695,10.);
#21602=VECTOR('',#72696,10.);
#21603=VECTOR('',#72699,10.);
#21604=VECTOR('',#72700,10.);
#21605=VECTOR('',#72701,10.);
#21606=VECTOR('',#72704,10.);
#21607=VECTOR('',#72705,10.);
#21608=VECTOR('',#72706,10.);
#21609=VECTOR('',#72709,10.);
#21610=VECTOR('',#72710,10.);
#21611=VECTOR('',#72711,10.);
#21612=VECTOR('',#72714,10.);
#21613=VECTOR('',#72715,10.);
#21614=VECTOR('',#72716,10.);
#21615=VECTOR('',#72719,10.);
#21616=VECTOR('',#72720,10.);
#21617=VECTOR('',#72721,10.);
#21618=VECTOR('',#72724,10.);
#21619=VECTOR('',#72725,10.);
#21620=VECTOR('',#72726,10.);
#21621=VECTOR('',#72729,10.);
#21622=VECTOR('',#72730,10.);
#21623=VECTOR('',#72731,10.);
#21624=VECTOR('',#72734,10.);
#21625=VECTOR('',#72735,10.);
#21626=VECTOR('',#72736,10.);
#21627=VECTOR('',#72739,10.);
#21628=VECTOR('',#72740,10.);
#21629=VECTOR('',#72741,10.);
#21630=VECTOR('',#72744,10.);
#21631=VECTOR('',#72745,10.);
#21632=VECTOR('',#72746,10.);
#21633=VECTOR('',#72749,10.);
#21634=VECTOR('',#72750,10.);
#21635=VECTOR('',#72751,10.);
#21636=VECTOR('',#72754,10.);
#21637=VECTOR('',#72755,10.);
#21638=VECTOR('',#72756,10.);
#21639=VECTOR('',#72759,10.);
#21640=VECTOR('',#72760,10.);
#21641=VECTOR('',#72761,10.);
#21642=VECTOR('',#72764,10.);
#21643=VECTOR('',#72765,10.);
#21644=VECTOR('',#72766,10.);
#21645=VECTOR('',#72769,10.);
#21646=VECTOR('',#72770,10.);
#21647=VECTOR('',#72771,10.);
#21648=VECTOR('',#72774,10.);
#21649=VECTOR('',#72775,10.);
#21650=VECTOR('',#72776,10.);
#21651=VECTOR('',#72779,10.);
#21652=VECTOR('',#72780,10.);
#21653=VECTOR('',#72781,10.);
#21654=VECTOR('',#72784,10.);
#21655=VECTOR('',#72785,10.);
#21656=VECTOR('',#72786,10.);
#21657=VECTOR('',#72789,10.);
#21658=VECTOR('',#72790,10.);
#21659=VECTOR('',#72791,10.);
#21660=VECTOR('',#72794,10.);
#21661=VECTOR('',#72795,10.);
#21662=VECTOR('',#72796,10.);
#21663=VECTOR('',#72799,10.);
#21664=VECTOR('',#72800,10.);
#21665=VECTOR('',#72801,10.);
#21666=VECTOR('',#72804,10.);
#21667=VECTOR('',#72805,10.);
#21668=VECTOR('',#72806,10.);
#21669=VECTOR('',#72809,10.);
#21670=VECTOR('',#72810,10.);
#21671=VECTOR('',#72811,10.);
#21672=VECTOR('',#72814,10.);
#21673=VECTOR('',#72815,10.);
#21674=VECTOR('',#72816,10.);
#21675=VECTOR('',#72819,10.);
#21676=VECTOR('',#72820,10.);
#21677=VECTOR('',#72821,10.);
#21678=VECTOR('',#72824,10.);
#21679=VECTOR('',#72825,10.);
#21680=VECTOR('',#72826,10.);
#21681=VECTOR('',#72829,10.);
#21682=VECTOR('',#72830,10.);
#21683=VECTOR('',#72831,10.);
#21684=VECTOR('',#72834,10.);
#21685=VECTOR('',#72835,10.);
#21686=VECTOR('',#72836,10.);
#21687=VECTOR('',#72839,10.);
#21688=VECTOR('',#72840,10.);
#21689=VECTOR('',#72841,10.);
#21690=VECTOR('',#72844,10.);
#21691=VECTOR('',#72845,10.);
#21692=VECTOR('',#72846,10.);
#21693=VECTOR('',#72849,10.);
#21694=VECTOR('',#72850,10.);
#21695=VECTOR('',#72851,10.);
#21696=VECTOR('',#72854,10.);
#21697=VECTOR('',#72855,10.);
#21698=VECTOR('',#72856,10.);
#21699=VECTOR('',#72859,10.);
#21700=VECTOR('',#72860,10.);
#21701=VECTOR('',#72861,10.);
#21702=VECTOR('',#72864,10.);
#21703=VECTOR('',#72865,10.);
#21704=VECTOR('',#72866,10.);
#21705=VECTOR('',#72869,10.);
#21706=VECTOR('',#72870,10.);
#21707=VECTOR('',#72871,10.);
#21708=VECTOR('',#72874,10.);
#21709=VECTOR('',#72875,10.);
#21710=VECTOR('',#72876,10.);
#21711=VECTOR('',#72879,10.);
#21712=VECTOR('',#72880,10.);
#21713=VECTOR('',#72881,10.);
#21714=VECTOR('',#72884,10.);
#21715=VECTOR('',#72885,10.);
#21716=VECTOR('',#72886,10.);
#21717=VECTOR('',#72889,10.);
#21718=VECTOR('',#72890,10.);
#21719=VECTOR('',#72891,10.);
#21720=VECTOR('',#72894,10.);
#21721=VECTOR('',#72895,10.);
#21722=VECTOR('',#72896,10.);
#21723=VECTOR('',#72899,10.);
#21724=VECTOR('',#72900,10.);
#21725=VECTOR('',#72901,10.);
#21726=VECTOR('',#72904,10.);
#21727=VECTOR('',#72905,10.);
#21728=VECTOR('',#72906,10.);
#21729=VECTOR('',#72909,10.);
#21730=VECTOR('',#72910,10.);
#21731=VECTOR('',#72911,10.);
#21732=VECTOR('',#72914,10.);
#21733=VECTOR('',#72915,10.);
#21734=VECTOR('',#72916,10.);
#21735=VECTOR('',#72919,10.);
#21736=VECTOR('',#72920,10.);
#21737=VECTOR('',#72921,10.);
#21738=VECTOR('',#72924,10.);
#21739=VECTOR('',#72925,10.);
#21740=VECTOR('',#72926,10.);
#21741=VECTOR('',#72929,10.);
#21742=VECTOR('',#72930,10.);
#21743=VECTOR('',#72931,10.);
#21744=VECTOR('',#72934,10.);
#21745=VECTOR('',#72935,10.);
#21746=VECTOR('',#72936,10.);
#21747=VECTOR('',#72939,10.);
#21748=VECTOR('',#72940,10.);
#21749=VECTOR('',#72941,10.);
#21750=VECTOR('',#72944,10.);
#21751=VECTOR('',#72945,10.);
#21752=VECTOR('',#72946,10.);
#21753=VECTOR('',#72949,10.);
#21754=VECTOR('',#72950,10.);
#21755=VECTOR('',#72951,10.);
#21756=VECTOR('',#72954,10.);
#21757=VECTOR('',#72955,10.);
#21758=VECTOR('',#72956,10.);
#21759=VECTOR('',#72959,10.);
#21760=VECTOR('',#72960,10.);
#21761=VECTOR('',#72961,10.);
#21762=VECTOR('',#72964,10.);
#21763=VECTOR('',#72965,10.);
#21764=VECTOR('',#72966,10.);
#21765=VECTOR('',#72969,10.);
#21766=VECTOR('',#72970,10.);
#21767=VECTOR('',#72971,10.);
#21768=VECTOR('',#72974,10.);
#21769=VECTOR('',#72975,10.);
#21770=VECTOR('',#72976,10.);
#21771=VECTOR('',#72979,10.);
#21772=VECTOR('',#72980,10.);
#21773=VECTOR('',#72981,10.);
#21774=VECTOR('',#72984,10.);
#21775=VECTOR('',#72985,10.);
#21776=VECTOR('',#72986,10.);
#21777=VECTOR('',#72989,10.);
#21778=VECTOR('',#72990,10.);
#21779=VECTOR('',#72991,10.);
#21780=VECTOR('',#72994,10.);
#21781=VECTOR('',#72995,10.);
#21782=VECTOR('',#72996,10.);
#21783=VECTOR('',#72999,10.);
#21784=VECTOR('',#73000,10.);
#21785=VECTOR('',#73001,10.);
#21786=VECTOR('',#73004,10.);
#21787=VECTOR('',#73005,10.);
#21788=VECTOR('',#73006,10.);
#21789=VECTOR('',#73009,10.);
#21790=VECTOR('',#73010,10.);
#21791=VECTOR('',#73011,10.);
#21792=VECTOR('',#73014,10.);
#21793=VECTOR('',#73015,10.);
#21794=VECTOR('',#73016,10.);
#21795=VECTOR('',#73019,10.);
#21796=VECTOR('',#73020,10.);
#21797=VECTOR('',#73021,10.);
#21798=VECTOR('',#73024,10.);
#21799=VECTOR('',#73025,10.);
#21800=VECTOR('',#73026,10.);
#21801=VECTOR('',#73029,10.);
#21802=VECTOR('',#73030,10.);
#21803=VECTOR('',#73031,10.);
#21804=VECTOR('',#73034,10.);
#21805=VECTOR('',#73035,10.);
#21806=VECTOR('',#73036,10.);
#21807=VECTOR('',#73039,10.);
#21808=VECTOR('',#73040,10.);
#21809=VECTOR('',#73041,10.);
#21810=VECTOR('',#73044,10.);
#21811=VECTOR('',#73045,10.);
#21812=VECTOR('',#73046,10.);
#21813=VECTOR('',#73049,10.);
#21814=VECTOR('',#73050,10.);
#21815=VECTOR('',#73051,10.);
#21816=VECTOR('',#73054,10.);
#21817=VECTOR('',#73055,10.);
#21818=VECTOR('',#73056,10.);
#21819=VECTOR('',#73059,10.);
#21820=VECTOR('',#73060,10.);
#21821=VECTOR('',#73061,10.);
#21822=VECTOR('',#73064,10.);
#21823=VECTOR('',#73065,10.);
#21824=VECTOR('',#73066,10.);
#21825=VECTOR('',#73069,10.);
#21826=VECTOR('',#73070,10.);
#21827=VECTOR('',#73071,10.);
#21828=VECTOR('',#73074,10.);
#21829=VECTOR('',#73075,10.);
#21830=VECTOR('',#73076,10.);
#21831=VECTOR('',#73079,10.);
#21832=VECTOR('',#73080,10.);
#21833=VECTOR('',#73081,10.);
#21834=VECTOR('',#73084,10.);
#21835=VECTOR('',#73085,10.);
#21836=VECTOR('',#73086,10.);
#21837=VECTOR('',#73089,10.);
#21838=VECTOR('',#73090,10.);
#21839=VECTOR('',#73091,10.);
#21840=VECTOR('',#73094,10.);
#21841=VECTOR('',#73095,10.);
#21842=VECTOR('',#73096,10.);
#21843=VECTOR('',#73099,10.);
#21844=VECTOR('',#73100,10.);
#21845=VECTOR('',#73101,10.);
#21846=VECTOR('',#73104,10.);
#21847=VECTOR('',#73105,10.);
#21848=VECTOR('',#73106,10.);
#21849=VECTOR('',#73109,10.);
#21850=VECTOR('',#73110,10.);
#21851=VECTOR('',#73111,10.);
#21852=VECTOR('',#73114,10.);
#21853=VECTOR('',#73115,10.);
#21854=VECTOR('',#73116,10.);
#21855=VECTOR('',#73119,10.);
#21856=VECTOR('',#73120,10.);
#21857=VECTOR('',#73121,10.);
#21858=VECTOR('',#73124,10.);
#21859=VECTOR('',#73125,10.);
#21860=VECTOR('',#73126,10.);
#21861=VECTOR('',#73129,10.);
#21862=VECTOR('',#73130,10.);
#21863=VECTOR('',#73131,10.);
#21864=VECTOR('',#73134,10.);
#21865=VECTOR('',#73135,10.);
#21866=VECTOR('',#73136,10.);
#21867=VECTOR('',#73139,10.);
#21868=VECTOR('',#73140,10.);
#21869=VECTOR('',#73141,10.);
#21870=VECTOR('',#73144,10.);
#21871=VECTOR('',#73145,10.);
#21872=VECTOR('',#73146,10.);
#21873=VECTOR('',#73149,10.);
#21874=VECTOR('',#73150,10.);
#21875=VECTOR('',#73151,10.);
#21876=VECTOR('',#73154,10.);
#21877=VECTOR('',#73155,10.);
#21878=VECTOR('',#73156,10.);
#21879=VECTOR('',#73159,10.);
#21880=VECTOR('',#73160,10.);
#21881=VECTOR('',#73161,10.);
#21882=VECTOR('',#73164,10.);
#21883=VECTOR('',#73165,10.);
#21884=VECTOR('',#73166,10.);
#21885=VECTOR('',#73169,10.);
#21886=VECTOR('',#73170,10.);
#21887=VECTOR('',#73171,10.);
#21888=VECTOR('',#73174,10.);
#21889=VECTOR('',#73175,10.);
#21890=VECTOR('',#73176,10.);
#21891=VECTOR('',#73179,10.);
#21892=VECTOR('',#73180,10.);
#21893=VECTOR('',#73181,10.);
#21894=VECTOR('',#73184,10.);
#21895=VECTOR('',#73185,10.);
#21896=VECTOR('',#73186,10.);
#21897=VECTOR('',#73189,10.);
#21898=VECTOR('',#73190,10.);
#21899=VECTOR('',#73191,10.);
#21900=VECTOR('',#73194,10.);
#21901=VECTOR('',#73195,10.);
#21902=VECTOR('',#73196,10.);
#21903=VECTOR('',#73199,10.);
#21904=VECTOR('',#73200,10.);
#21905=VECTOR('',#73201,10.);
#21906=VECTOR('',#73204,10.);
#21907=VECTOR('',#73205,10.);
#21908=VECTOR('',#73206,10.);
#21909=VECTOR('',#73209,10.);
#21910=VECTOR('',#73210,10.);
#21911=VECTOR('',#73211,10.);
#21912=VECTOR('',#73214,10.);
#21913=VECTOR('',#73215,10.);
#21914=VECTOR('',#73216,10.);
#21915=VECTOR('',#73219,10.);
#21916=VECTOR('',#73220,10.);
#21917=VECTOR('',#73221,10.);
#21918=VECTOR('',#73224,10.);
#21919=VECTOR('',#73225,10.);
#21920=VECTOR('',#73226,10.);
#21921=VECTOR('',#73229,10.);
#21922=VECTOR('',#73230,10.);
#21923=VECTOR('',#73231,10.);
#21924=VECTOR('',#73234,10.);
#21925=VECTOR('',#73235,10.);
#21926=VECTOR('',#73236,10.);
#21927=VECTOR('',#73239,10.);
#21928=VECTOR('',#73240,10.);
#21929=VECTOR('',#73241,10.);
#21930=VECTOR('',#73244,10.);
#21931=VECTOR('',#73245,10.);
#21932=VECTOR('',#73246,10.);
#21933=VECTOR('',#73249,10.);
#21934=VECTOR('',#73250,10.);
#21935=VECTOR('',#73251,10.);
#21936=VECTOR('',#73254,10.);
#21937=VECTOR('',#73255,10.);
#21938=VECTOR('',#73256,10.);
#21939=VECTOR('',#73259,10.);
#21940=VECTOR('',#73260,10.);
#21941=VECTOR('',#73261,10.);
#21942=VECTOR('',#73264,10.);
#21943=VECTOR('',#73265,10.);
#21944=VECTOR('',#73266,10.);
#21945=VECTOR('',#73269,10.);
#21946=VECTOR('',#73270,10.);
#21947=VECTOR('',#73271,10.);
#21948=VECTOR('',#73274,10.);
#21949=VECTOR('',#73275,10.);
#21950=VECTOR('',#73276,10.);
#21951=VECTOR('',#73279,10.);
#21952=VECTOR('',#73280,10.);
#21953=VECTOR('',#73281,10.);
#21954=VECTOR('',#73284,10.);
#21955=VECTOR('',#73285,10.);
#21956=VECTOR('',#73286,10.);
#21957=VECTOR('',#73289,10.);
#21958=VECTOR('',#73290,10.);
#21959=VECTOR('',#73291,10.);
#21960=VECTOR('',#73294,10.);
#21961=VECTOR('',#73295,10.);
#21962=VECTOR('',#73296,10.);
#21963=VECTOR('',#73299,10.);
#21964=VECTOR('',#73300,10.);
#21965=VECTOR('',#73301,10.);
#21966=VECTOR('',#73304,10.);
#21967=VECTOR('',#73305,10.);
#21968=VECTOR('',#73306,10.);
#21969=VECTOR('',#73309,10.);
#21970=VECTOR('',#73310,10.);
#21971=VECTOR('',#73311,10.);
#21972=VECTOR('',#73314,10.);
#21973=VECTOR('',#73315,10.);
#21974=VECTOR('',#73316,10.);
#21975=VECTOR('',#73319,10.);
#21976=VECTOR('',#73320,10.);
#21977=VECTOR('',#73321,10.);
#21978=VECTOR('',#73324,10.);
#21979=VECTOR('',#73325,10.);
#21980=VECTOR('',#73326,10.);
#21981=VECTOR('',#73329,10.);
#21982=VECTOR('',#73330,10.);
#21983=VECTOR('',#73331,10.);
#21984=VECTOR('',#73334,10.);
#21985=VECTOR('',#73335,10.);
#21986=VECTOR('',#73336,10.);
#21987=VECTOR('',#73339,10.);
#21988=VECTOR('',#73340,10.);
#21989=VECTOR('',#73341,10.);
#21990=VECTOR('',#73344,10.);
#21991=VECTOR('',#73345,10.);
#21992=VECTOR('',#73346,10.);
#21993=VECTOR('',#73349,10.);
#21994=VECTOR('',#73350,10.);
#21995=VECTOR('',#73351,10.);
#21996=VECTOR('',#73354,10.);
#21997=VECTOR('',#73355,10.);
#21998=VECTOR('',#73356,10.);
#21999=VECTOR('',#73359,10.);
#22000=VECTOR('',#73360,10.);
#22001=VECTOR('',#73361,10.);
#22002=VECTOR('',#73364,10.);
#22003=VECTOR('',#73365,10.);
#22004=VECTOR('',#73366,10.);
#22005=VECTOR('',#73369,10.);
#22006=VECTOR('',#73370,10.);
#22007=VECTOR('',#73371,10.);
#22008=VECTOR('',#73374,10.);
#22009=VECTOR('',#73375,10.);
#22010=VECTOR('',#73376,10.);
#22011=VECTOR('',#73379,10.);
#22012=VECTOR('',#73380,10.);
#22013=VECTOR('',#73381,10.);
#22014=VECTOR('',#73384,10.);
#22015=VECTOR('',#73385,10.);
#22016=VECTOR('',#73386,10.);
#22017=VECTOR('',#73389,10.);
#22018=VECTOR('',#73390,10.);
#22019=VECTOR('',#73391,10.);
#22020=VECTOR('',#73394,10.);
#22021=VECTOR('',#73395,10.);
#22022=VECTOR('',#73396,10.);
#22023=VECTOR('',#73399,10.);
#22024=VECTOR('',#73400,10.);
#22025=VECTOR('',#73401,10.);
#22026=VECTOR('',#73404,10.);
#22027=VECTOR('',#73405,10.);
#22028=VECTOR('',#73406,10.);
#22029=VECTOR('',#73409,10.);
#22030=VECTOR('',#73410,10.);
#22031=VECTOR('',#73411,10.);
#22032=VECTOR('',#73414,10.);
#22033=VECTOR('',#73415,10.);
#22034=VECTOR('',#73416,10.);
#22035=VECTOR('',#73419,10.);
#22036=VECTOR('',#73420,10.);
#22037=VECTOR('',#73421,10.);
#22038=VECTOR('',#73424,10.);
#22039=VECTOR('',#73425,10.);
#22040=VECTOR('',#73426,10.);
#22041=VECTOR('',#73429,10.);
#22042=VECTOR('',#73430,10.);
#22043=VECTOR('',#73431,10.);
#22044=VECTOR('',#73434,10.);
#22045=VECTOR('',#73435,10.);
#22046=VECTOR('',#73436,10.);
#22047=VECTOR('',#73439,10.);
#22048=VECTOR('',#73440,10.);
#22049=VECTOR('',#73441,10.);
#22050=VECTOR('',#73444,10.);
#22051=VECTOR('',#73445,10.);
#22052=VECTOR('',#73446,10.);
#22053=VECTOR('',#73449,10.);
#22054=VECTOR('',#73450,10.);
#22055=VECTOR('',#73451,10.);
#22056=VECTOR('',#73454,10.);
#22057=VECTOR('',#73455,10.);
#22058=VECTOR('',#73456,10.);
#22059=VECTOR('',#73459,10.);
#22060=VECTOR('',#73460,10.);
#22061=VECTOR('',#73461,10.);
#22062=VECTOR('',#73464,10.);
#22063=VECTOR('',#73465,10.);
#22064=VECTOR('',#73466,10.);
#22065=VECTOR('',#73469,10.);
#22066=VECTOR('',#73470,10.);
#22067=VECTOR('',#73471,10.);
#22068=VECTOR('',#73474,10.);
#22069=VECTOR('',#73475,10.);
#22070=VECTOR('',#73476,10.);
#22071=VECTOR('',#73479,10.);
#22072=VECTOR('',#73480,10.);
#22073=VECTOR('',#73481,10.);
#22074=VECTOR('',#73484,10.);
#22075=VECTOR('',#73485,10.);
#22076=VECTOR('',#73486,10.);
#22077=VECTOR('',#73489,10.);
#22078=VECTOR('',#73490,10.);
#22079=VECTOR('',#73491,10.);
#22080=VECTOR('',#73494,10.);
#22081=VECTOR('',#73495,10.);
#22082=VECTOR('',#73496,10.);
#22083=VECTOR('',#73499,10.);
#22084=VECTOR('',#73500,10.);
#22085=VECTOR('',#73501,10.);
#22086=VECTOR('',#73504,10.);
#22087=VECTOR('',#73505,10.);
#22088=VECTOR('',#73506,10.);
#22089=VECTOR('',#73509,10.);
#22090=VECTOR('',#73510,10.);
#22091=VECTOR('',#73511,10.);
#22092=VECTOR('',#73514,10.);
#22093=VECTOR('',#73515,10.);
#22094=VECTOR('',#73516,10.);
#22095=VECTOR('',#73519,10.);
#22096=VECTOR('',#73520,10.);
#22097=VECTOR('',#73521,10.);
#22098=VECTOR('',#73524,10.);
#22099=VECTOR('',#73525,10.);
#22100=VECTOR('',#73526,10.);
#22101=VECTOR('',#73529,10.);
#22102=VECTOR('',#73530,10.);
#22103=VECTOR('',#73531,10.);
#22104=VECTOR('',#73534,10.);
#22105=VECTOR('',#73535,10.);
#22106=VECTOR('',#73536,10.);
#22107=VECTOR('',#73539,10.);
#22108=VECTOR('',#73540,10.);
#22109=VECTOR('',#73541,10.);
#22110=VECTOR('',#73544,10.);
#22111=VECTOR('',#73545,10.);
#22112=VECTOR('',#73546,10.);
#22113=VECTOR('',#73549,10.);
#22114=VECTOR('',#73550,10.);
#22115=VECTOR('',#73551,10.);
#22116=VECTOR('',#73554,10.);
#22117=VECTOR('',#73555,10.);
#22118=VECTOR('',#73556,10.);
#22119=VECTOR('',#73559,10.);
#22120=VECTOR('',#73560,10.);
#22121=VECTOR('',#73561,10.);
#22122=VECTOR('',#73564,10.);
#22123=VECTOR('',#73565,10.);
#22124=VECTOR('',#73566,10.);
#22125=VECTOR('',#73569,10.);
#22126=VECTOR('',#73570,10.);
#22127=VECTOR('',#73571,10.);
#22128=VECTOR('',#73574,10.);
#22129=VECTOR('',#73575,10.);
#22130=VECTOR('',#73576,10.);
#22131=VECTOR('',#73579,10.);
#22132=VECTOR('',#73580,10.);
#22133=VECTOR('',#73581,10.);
#22134=VECTOR('',#73584,10.);
#22135=VECTOR('',#73585,10.);
#22136=VECTOR('',#73586,10.);
#22137=VECTOR('',#73589,10.);
#22138=VECTOR('',#73590,10.);
#22139=VECTOR('',#73591,10.);
#22140=VECTOR('',#73594,10.);
#22141=VECTOR('',#73595,10.);
#22142=VECTOR('',#73596,10.);
#22143=VECTOR('',#73599,10.);
#22144=VECTOR('',#73600,10.);
#22145=VECTOR('',#73601,10.);
#22146=VECTOR('',#73604,10.);
#22147=VECTOR('',#73605,10.);
#22148=VECTOR('',#73606,10.);
#22149=VECTOR('',#73609,10.);
#22150=VECTOR('',#73610,10.);
#22151=VECTOR('',#73611,10.);
#22152=VECTOR('',#73614,10.);
#22153=VECTOR('',#73615,10.);
#22154=VECTOR('',#73616,10.);
#22155=VECTOR('',#73619,10.);
#22156=VECTOR('',#73620,10.);
#22157=VECTOR('',#73621,10.);
#22158=VECTOR('',#73624,10.);
#22159=VECTOR('',#73625,10.);
#22160=VECTOR('',#73626,10.);
#22161=VECTOR('',#73629,10.);
#22162=VECTOR('',#73630,10.);
#22163=VECTOR('',#73631,10.);
#22164=VECTOR('',#73634,10.);
#22165=VECTOR('',#73635,10.);
#22166=VECTOR('',#73636,10.);
#22167=VECTOR('',#73639,10.);
#22168=VECTOR('',#73640,10.);
#22169=VECTOR('',#73641,10.);
#22170=VECTOR('',#73644,10.);
#22171=VECTOR('',#73645,10.);
#22172=VECTOR('',#73646,10.);
#22173=VECTOR('',#73649,10.);
#22174=VECTOR('',#73650,10.);
#22175=VECTOR('',#73651,10.);
#22176=VECTOR('',#73654,10.);
#22177=VECTOR('',#73655,10.);
#22178=VECTOR('',#73656,10.);
#22179=VECTOR('',#73659,10.);
#22180=VECTOR('',#73660,10.);
#22181=VECTOR('',#73661,10.);
#22182=VECTOR('',#73664,10.);
#22183=VECTOR('',#73665,10.);
#22184=VECTOR('',#73666,10.);
#22185=VECTOR('',#73669,10.);
#22186=VECTOR('',#73670,10.);
#22187=VECTOR('',#73671,10.);
#22188=VECTOR('',#73674,10.);
#22189=VECTOR('',#73675,10.);
#22190=VECTOR('',#73676,10.);
#22191=VECTOR('',#73679,10.);
#22192=VECTOR('',#73680,10.);
#22193=VECTOR('',#73683,10.);
#22194=VECTOR('',#73684,10.);
#22195=VECTOR('',#73695,10.);
#22196=VECTOR('',#73698,10.);
#22197=VECTOR('',#73703,10.);
#22198=VECTOR('',#73710,10.);
#22199=VECTOR('',#73715,10.);
#22200=VECTOR('',#73716,10.);
#22201=VECTOR('',#73717,10.);
#22202=VECTOR('',#73718,10.);
#22203=VECTOR('',#73719,10.);
#22204=VECTOR('',#73726,10.);
#22205=VECTOR('',#73729,10.);
#22206=VECTOR('',#73730,10.);
#22207=VECTOR('',#73731,10.);
#22208=VECTOR('',#73734,10.);
#22209=VECTOR('',#73735,10.);
#22210=VECTOR('',#73736,10.);
#22211=VECTOR('',#73737,10.);
#22212=VECTOR('',#73738,10.);
#22213=VECTOR('',#73739,10.);
#22214=VECTOR('',#73746,10.);
#22215=VECTOR('',#73749,10.);
#22216=VECTOR('',#73750,10.);
#22217=VECTOR('',#73753,10.);
#22218=VECTOR('',#73760,10.);
#22219=VECTOR('',#73763,10.);
#22220=VECTOR('',#73764,10.);
#22221=VECTOR('',#73765,10.);
#22222=VECTOR('',#73766,10.);
#22223=VECTOR('',#73769,10.);
#22224=VECTOR('',#73770,10.);
#22225=VECTOR('',#73773,10.);
#22226=VECTOR('',#73774,10.);
#22227=VECTOR('',#73775,10.);
#22228=VECTOR('',#73778,10.);
#22229=VECTOR('',#73779,10.);
#22230=VECTOR('',#73786,2.15);
#22231=VECTOR('',#73791,10.);
#22232=VECTOR('',#73798,10.);
#22233=VECTOR('',#73799,10.);
#22234=VECTOR('',#73800,10.);
#22235=VECTOR('',#73801,10.);
#22236=VECTOR('',#73804,10.);
#22237=VECTOR('',#73805,10.);
#22238=VECTOR('',#73806,10.);
#22239=VECTOR('',#73809,10.);
#22240=VECTOR('',#73810,10.);
#22241=VECTOR('',#73813,10.);
#22242=VECTOR('',#73814,10.);
#22243=VECTOR('',#73817,10.);
#22244=VECTOR('',#73818,10.);
#22245=VECTOR('',#73819,10.);
#22246=VECTOR('',#73820,10.);
#22247=VECTOR('',#73823,10.);
#22248=VECTOR('',#73824,10.);
#22249=VECTOR('',#73825,10.);
#22250=VECTOR('',#73828,10.);
#22251=VECTOR('',#73829,10.);
#22252=VECTOR('',#73832,10.);
#22253=VECTOR('',#73833,10.);
#22254=VECTOR('',#73836,10.);
#22255=VECTOR('',#73837,10.);
#22256=VECTOR('',#73838,10.);
#22257=VECTOR('',#73839,10.);
#22258=VECTOR('',#73842,10.);
#22259=VECTOR('',#73843,10.);
#22260=VECTOR('',#73844,10.);
#22261=VECTOR('',#73847,10.);
#22262=VECTOR('',#73848,10.);
#22263=VECTOR('',#73851,10.);
#22264=VECTOR('',#73852,10.);
#22265=VECTOR('',#73855,10.);
#22266=VECTOR('',#73856,10.);
#22267=VECTOR('',#73857,10.);
#22268=VECTOR('',#73858,10.);
#22269=VECTOR('',#73861,10.);
#22270=VECTOR('',#73862,10.);
#22271=VECTOR('',#73863,10.);
#22272=VECTOR('',#73866,10.);
#22273=VECTOR('',#73867,10.);
#22274=VECTOR('',#73870,10.);
#22275=VECTOR('',#73871,10.);
#22276=VECTOR('',#73874,10.);
#22277=VECTOR('',#73875,10.);
#22278=VECTOR('',#73876,10.);
#22279=VECTOR('',#73877,10.);
#22280=VECTOR('',#73880,10.);
#22281=VECTOR('',#73881,10.);
#22282=VECTOR('',#73882,10.);
#22283=VECTOR('',#73885,10.);
#22284=VECTOR('',#73886,10.);
#22285=VECTOR('',#73889,10.);
#22286=VECTOR('',#73890,10.);
#22287=VECTOR('',#73893,10.);
#22288=VECTOR('',#73894,10.);
#22289=VECTOR('',#73895,10.);
#22290=VECTOR('',#73896,10.);
#22291=VECTOR('',#73899,10.);
#22292=VECTOR('',#73900,10.);
#22293=VECTOR('',#73901,10.);
#22294=VECTOR('',#73904,10.);
#22295=VECTOR('',#73905,10.);
#22296=VECTOR('',#73908,10.);
#22297=VECTOR('',#73909,10.);
#22298=VECTOR('',#73912,10.);
#22299=VECTOR('',#73913,10.);
#22300=VECTOR('',#73914,10.);
#22301=VECTOR('',#73915,10.);
#22302=VECTOR('',#73918,10.);
#22303=VECTOR('',#73919,10.);
#22304=VECTOR('',#73920,10.);
#22305=VECTOR('',#73923,10.);
#22306=VECTOR('',#73924,10.);
#22307=VECTOR('',#73927,10.);
#22308=VECTOR('',#73928,10.);
#22309=VECTOR('',#73931,10.);
#22310=VECTOR('',#73932,10.);
#22311=VECTOR('',#73933,10.);
#22312=VECTOR('',#73934,10.);
#22313=VECTOR('',#73937,10.);
#22314=VECTOR('',#73938,10.);
#22315=VECTOR('',#73939,10.);
#22316=VECTOR('',#73942,10.);
#22317=VECTOR('',#73943,10.);
#22318=VECTOR('',#73946,10.);
#22319=VECTOR('',#73947,10.);
#22320=VECTOR('',#73950,10.);
#22321=VECTOR('',#73951,10.);
#22322=VECTOR('',#73952,10.);
#22323=VECTOR('',#73955,10.);
#22324=VECTOR('',#73956,10.);
#22325=VECTOR('',#73957,10.);
#22326=VECTOR('',#73962,10.);
#22327=VECTOR('',#73965,10.);
#22328=VECTOR('',#73966,10.);
#22329=VECTOR('',#73967,10.);
#22330=VECTOR('',#73968,10.);
#22331=VECTOR('',#73971,10.);
#22332=VECTOR('',#73972,10.);
#22333=VECTOR('',#73973,10.);
#22334=VECTOR('',#73976,10.);
#22335=VECTOR('',#73977,10.);
#22336=VECTOR('',#73980,10.);
#22337=VECTOR('',#73981,10.);
#22338=VECTOR('',#73984,10.);
#22339=VECTOR('',#73985,10.);
#22340=VECTOR('',#73986,10.);
#22341=VECTOR('',#73987,10.);
#22342=VECTOR('',#73990,10.);
#22343=VECTOR('',#73991,10.);
#22344=VECTOR('',#73992,10.);
#22345=VECTOR('',#73995,10.);
#22346=VECTOR('',#73996,10.);
#22347=VECTOR('',#73999,10.);
#22348=VECTOR('',#74000,10.);
#22349=VECTOR('',#74003,10.);
#22350=VECTOR('',#74004,10.);
#22351=VECTOR('',#74005,10.);
#22352=VECTOR('',#74006,10.);
#22353=VECTOR('',#74009,10.);
#22354=VECTOR('',#74010,10.);
#22355=VECTOR('',#74011,10.);
#22356=VECTOR('',#74014,10.);
#22357=VECTOR('',#74015,10.);
#22358=VECTOR('',#74018,10.);
#22359=VECTOR('',#74019,10.);
#22360=VECTOR('',#74022,10.);
#22361=VECTOR('',#74023,10.);
#22362=VECTOR('',#74024,10.);
#22363=VECTOR('',#74025,10.);
#22364=VECTOR('',#74028,10.);
#22365=VECTOR('',#74029,10.);
#22366=VECTOR('',#74030,10.);
#22367=VECTOR('',#74033,10.);
#22368=VECTOR('',#74034,10.);
#22369=VECTOR('',#74037,10.);
#22370=VECTOR('',#74038,10.);
#22371=VECTOR('',#74041,10.);
#22372=VECTOR('',#74042,10.);
#22373=VECTOR('',#74043,10.);
#22374=VECTOR('',#74044,10.);
#22375=VECTOR('',#74047,10.);
#22376=VECTOR('',#74048,10.);
#22377=VECTOR('',#74049,10.);
#22378=VECTOR('',#74052,10.);
#22379=VECTOR('',#74053,10.);
#22380=VECTOR('',#74056,10.);
#22381=VECTOR('',#74057,10.);
#22382=VECTOR('',#74060,10.);
#22383=VECTOR('',#74061,10.);
#22384=VECTOR('',#74062,10.);
#22385=VECTOR('',#74063,10.);
#22386=VECTOR('',#74066,10.);
#22387=VECTOR('',#74067,10.);
#22388=VECTOR('',#74068,10.);
#22389=VECTOR('',#74071,10.);
#22390=VECTOR('',#74072,10.);
#22391=VECTOR('',#74075,10.);
#22392=VECTOR('',#74076,10.);
#22393=VECTOR('',#74079,10.);
#22394=VECTOR('',#74080,10.);
#22395=VECTOR('',#74081,10.);
#22396=VECTOR('',#74082,10.);
#22397=VECTOR('',#74085,10.);
#22398=VECTOR('',#74086,10.);
#22399=VECTOR('',#74087,10.);
#22400=VECTOR('',#74090,10.);
#22401=VECTOR('',#74091,10.);
#22402=VECTOR('',#74094,10.);
#22403=VECTOR('',#74095,10.);
#22404=VECTOR('',#74098,10.);
#22405=VECTOR('',#74099,10.);
#22406=VECTOR('',#74100,10.);
#22407=VECTOR('',#74103,10.);
#22408=VECTOR('',#74104,10.);
#22409=VECTOR('',#74105,10.);
#22410=VECTOR('',#74110,10.);
#22411=VECTOR('',#74113,10.);
#22412=VECTOR('',#74120,10.);
#22413=VECTOR('',#74123,10.);
#22414=VECTOR('',#74124,10.);
#22415=VECTOR('',#74125,10.);
#22416=VECTOR('',#74126,10.);
#22417=VECTOR('',#74127,10.);
#22418=VECTOR('',#74128,10.);
#22419=VECTOR('',#74129,10.);
#22420=VECTOR('',#74130,10.);
#22421=VECTOR('',#74131,10.);
#22422=VECTOR('',#74132,10.);
#22423=VECTOR('',#74133,10.);
#22424=VECTOR('',#74134,10.);
#22425=VECTOR('',#74135,10.);
#22426=VECTOR('',#74136,10.);
#22427=VECTOR('',#74137,10.);
#22428=VECTOR('',#74138,10.);
#22429=VECTOR('',#74139,10.);
#22430=VECTOR('',#74140,10.);
#22431=VECTOR('',#74141,10.);
#22432=VECTOR('',#74142,10.);
#22433=VECTOR('',#74143,10.);
#22434=VECTOR('',#74148,1.09999999999999);
#22435=VECTOR('',#74153,1.54999999999999);
#22436=VECTOR('',#74162,10.);
#22437=VECTOR('',#74167,10.);
#22438=VECTOR('',#74170,10.);
#22439=VECTOR('',#74175,1.09999999999999);
#22440=VECTOR('',#74180,1.54999999999999);
#22441=VECTOR('',#74187,10.);
#22442=VECTOR('',#74190,10.);
#22443=VECTOR('',#74195,10.);
#22444=VECTOR('',#74196,10.);
#22445=VECTOR('',#74199,10.);
#22446=VECTOR('',#74200,10.);
#22447=VECTOR('',#74205,10.);
#22448=VECTOR('',#74208,10.);
#22449=VECTOR('',#74211,10.);
#22450=VECTOR('',#74218,1.99999999999999);
#22451=VECTOR('',#74223,1.99999999999999);
#22452=VECTOR('',#74226,1.99999999999999);
#22453=VECTOR('',#74229,1.99999999999999);
#22454=VECTOR('',#74232,1.99999999999999);
#22455=VECTOR('',#74235,1.99999999999999);
#22456=VECTOR('',#74238,1.99999999999999);
#22457=VECTOR('',#74241,1.99999999999999);
#22458=VECTOR('',#74244,1.99999999999999);
#22459=VECTOR('',#74247,1.99999999999999);
#22460=VECTOR('',#74250,1.99999999999999);
#22461=VECTOR('',#74253,1.5555);
#22462=VECTOR('',#74258,1.5555);
#22463=VECTOR('',#74261,1.5555);
#22464=VECTOR('',#74264,1.5555);
#22465=VECTOR('',#74267,1.5555);
#22466=VECTOR('',#74270,1.5555);
#22467=VECTOR('',#74273,1.5555);
#22468=VECTOR('',#74276,1.5555);
#22469=VECTOR('',#74279,1.5555);
#22470=VECTOR('',#74282,1.5555);
#22471=VECTOR('',#74315,10.);
#22472=VECTOR('',#74316,10.);
#22473=VECTOR('',#74317,10.);
#22474=VECTOR('',#74318,10.);
#22475=VECTOR('',#74321,10.);
#22476=VECTOR('',#74322,10.);
#22477=VECTOR('',#74323,10.);
#22478=VECTOR('',#74324,10.);
#22479=VECTOR('',#74351,3.5);
#22480=VECTOR('',#74356,1.75000000000001);
#22481=VECTOR('',#74363,1.5);
#22482=VECTOR('',#74368,1.5);
#22483=VECTOR('',#74371,1.5);
#22484=VECTOR('',#74374,1.5);
#22485=VECTOR('',#74377,1.5);
#22486=VECTOR('',#74380,1.17775);
#22487=VECTOR('',#74385,1.17775);
#22488=VECTOR('',#74388,1.17775);
#22489=VECTOR('',#74391,1.17775);
#22490=VECTOR('',#74412,0.916025403784442);
#22491=VECTOR('',#74427,10.);
#22492=VECTOR('',#74428,10.);
#22493=VECTOR('',#74433,10.);
#22494=VECTOR('',#74434,10.);
#22495=VECTOR('',#74439,10.);
#22496=VECTOR('',#74442,10.);
#22497=VECTOR('',#74445,10.);
#22498=VECTOR('',#74446,10.);
#22499=VECTOR('',#74451,10.);
#22500=VECTOR('',#74454,10.);
#22501=VECTOR('',#74457,10.);
#22502=VECTOR('',#74460,10.);
#22503=VECTOR('',#74463,10.);
#22504=VECTOR('',#74464,10.);
#22505=VECTOR('',#74465,10.);
#22506=VECTOR('',#74466,10.);
#22507=VECTOR('',#74469,10.);
#22508=VECTOR('',#74470,10.);
#22509=VECTOR('',#74471,10.);
#22510=VECTOR('',#74474,10.);
#22511=VECTOR('',#74475,10.);
#22512=VECTOR('',#74476,10.);
#22513=VECTOR('',#74483,10.);
#22514=VECTOR('',#74488,10.);
#22515=VECTOR('',#74491,10.);
#22516=VECTOR('',#74494,10.);
#22517=VECTOR('',#74511,10.);
#22518=VECTOR('',#74516,10.);
#22519=VECTOR('',#74521,0.866025403784434);
#22520=VECTOR('',#74524,10.);
#22521=VECTOR('',#74527,10.);
#22522=VECTOR('',#74536,1.35000000000002);
#22523=VECTOR('',#74545,1.25);
#22524=VECTOR('',#74552,0.999999999999996);
#22525=VECTOR('',#74557,0.999999999999996);
#22526=VECTOR('',#74560,0.999999999999996);
#22527=VECTOR('',#74563,0.999999999999996);
#22528=VECTOR('',#74568,0.739000000000001);
#22529=VECTOR('',#74573,0.739000000000001);
#22530=VECTOR('',#74576,0.739000000000001);
#22531=VECTOR('',#74595,0.569615242270665);
#22532=VECTOR('',#74610,10.);
#22533=VECTOR('',#74611,10.);
#22534=VECTOR('',#74616,10.);
#22535=VECTOR('',#74617,10.);
#22536=VECTOR('',#74622,10.);
#22537=VECTOR('',#74625,10.);
#22538=VECTOR('',#74628,10.);
#22539=VECTOR('',#74629,10.);
#22540=VECTOR('',#74634,10.);
#22541=VECTOR('',#74637,10.);
#22542=VECTOR('',#74640,10.);
#22543=VECTOR('',#74643,10.);
#22544=VECTOR('',#74646,10.);
#22545=VECTOR('',#74647,10.);
#22546=VECTOR('',#74648,10.);
#22547=VECTOR('',#74649,10.);
#22548=VECTOR('',#74652,10.);
#22549=VECTOR('',#74653,10.);
#22550=VECTOR('',#74654,10.);
#22551=VECTOR('',#74657,10.);
#22552=VECTOR('',#74658,10.);
#22553=VECTOR('',#74659,10.);
#22554=VECTOR('',#74666,10.);
#22555=VECTOR('',#74671,10.);
#22556=VECTOR('',#74674,10.);
#22557=VECTOR('',#74677,10.);
#22558=VECTOR('',#74694,10.);
#22559=VECTOR('',#74699,10.);
#22560=VECTOR('',#74704,0.519615242270657);
#22561=VECTOR('',#74707,10.);
#22562=VECTOR('',#74710,10.);
#22563=VECTOR('',#74719,0.88000000000001);
#22564=VECTOR('',#74728,0.749999999999993);
#22565=VECTOR('',#74735,1.49999999999999);
#22566=VECTOR('',#74740,1.49999999999999);
#22567=VECTOR('',#74743,1.49999999999999);
#22568=VECTOR('',#74746,1.49999999999999);
#22569=VECTOR('',#74749,1.49999999999999);
#22570=VECTOR('',#74752,1.49999999999999);
#22571=VECTOR('',#74755,1.49999999999999);
#22572=VECTOR('',#74758,1.49999999999999);
#22573=VECTOR('',#74761,1.49999999999999);
#22574=VECTOR('',#74764,1.49999999999999);
#22575=VECTOR('',#74767,1.49999999999999);
#22576=VECTOR('',#74770,1.17775);
#22577=VECTOR('',#74775,1.17775);
#22578=VECTOR('',#74778,1.17775);
#22579=VECTOR('',#74781,1.17775);
#22580=VECTOR('',#74784,1.17775);
#22581=VECTOR('',#74787,1.17775);
#22582=VECTOR('',#74790,1.17775);
#22583=VECTOR('',#74793,1.17775);
#22584=VECTOR('',#74796,1.17775);
#22585=VECTOR('',#74799,1.17775);
#22586=VECTOR('',#74820,0.916025403784424);
#22587=VECTOR('',#74835,10.);
#22588=VECTOR('',#74836,10.);
#22589=VECTOR('',#74841,10.);
#22590=VECTOR('',#74842,10.);
#22591=VECTOR('',#74847,10.);
#22592=VECTOR('',#74850,10.);
#22593=VECTOR('',#74853,10.);
#22594=VECTOR('',#74854,10.);
#22595=VECTOR('',#74859,10.);
#22596=VECTOR('',#74862,10.);
#22597=VECTOR('',#74865,10.);
#22598=VECTOR('',#74868,10.);
#22599=VECTOR('',#74871,10.);
#22600=VECTOR('',#74872,10.);
#22601=VECTOR('',#74873,10.);
#22602=VECTOR('',#74874,10.);
#22603=VECTOR('',#74877,10.);
#22604=VECTOR('',#74878,10.);
#22605=VECTOR('',#74879,10.);
#22606=VECTOR('',#74882,10.);
#22607=VECTOR('',#74883,10.);
#22608=VECTOR('',#74884,10.);
#22609=VECTOR('',#74891,10.);
#22610=VECTOR('',#74896,10.);
#22611=VECTOR('',#74899,10.);
#22612=VECTOR('',#74902,10.);
#22613=VECTOR('',#74919,10.);
#22614=VECTOR('',#74924,10.);
#22615=VECTOR('',#74929,0.866025403784434);
#22616=VECTOR('',#74932,10.);
#22617=VECTOR('',#74935,10.);
#22618=VECTOR('',#74944,1.34999999999998);
#22619=VECTOR('',#74953,1.25);
#22620=VECTOR('',#74960,0.999999999999996);
#22621=VECTOR('',#74965,0.999999999999996);
#22622=VECTOR('',#74968,0.999999999999996);
#22623=VECTOR('',#74971,0.999999999999996);
#22624=VECTOR('',#74974,0.999999999999996);
#22625=VECTOR('',#74977,0.999999999999996);
#22626=VECTOR('',#74980,0.739000000000001);
#22627=VECTOR('',#74985,0.739000000000001);
#22628=VECTOR('',#74990,0.739000000000001);
#22629=VECTOR('',#74993,0.739000000000001);
#22630=VECTOR('',#74996,0.739000000000001);
#22631=VECTOR('',#74999,0.739000000000001);
#22632=VECTOR('',#75020,0.569615242270665);
#22633=VECTOR('',#75035,10.);
#22634=VECTOR('',#75036,10.);
#22635=VECTOR('',#75041,10.);
#22636=VECTOR('',#75042,10.);
#22637=VECTOR('',#75047,10.);
#22638=VECTOR('',#75050,10.);
#22639=VECTOR('',#75053,10.);
#22640=VECTOR('',#75054,10.);
#22641=VECTOR('',#75059,10.);
#22642=VECTOR('',#75062,10.);
#22643=VECTOR('',#75065,10.);
#22644=VECTOR('',#75068,10.);
#22645=VECTOR('',#75071,10.);
#22646=VECTOR('',#75072,10.);
#22647=VECTOR('',#75073,10.);
#22648=VECTOR('',#75074,10.);
#22649=VECTOR('',#75077,10.);
#22650=VECTOR('',#75078,10.);
#22651=VECTOR('',#75079,10.);
#22652=VECTOR('',#75082,10.);
#22653=VECTOR('',#75083,10.);
#22654=VECTOR('',#75084,10.);
#22655=VECTOR('',#75091,10.);
#22656=VECTOR('',#75096,10.);
#22657=VECTOR('',#75099,10.);
#22658=VECTOR('',#75102,10.);
#22659=VECTOR('',#75119,10.);
#22660=VECTOR('',#75124,10.);
#22661=VECTOR('',#75129,0.519615242270657);
#22662=VECTOR('',#75132,10.);
#22663=VECTOR('',#75135,10.);
#22664=VECTOR('',#75144,0.88000000000001);
#22665=VECTOR('',#75153,0.749999999999993);
#22666=VECTOR('',#75160,0.999999999999996);
#22667=VECTOR('',#75165,0.999999999999996);
#22668=VECTOR('',#75168,0.999999999999996);
#22669=VECTOR('',#75171,0.999999999999996);
#22670=VECTOR('',#75174,0.999999999999996);
#22671=VECTOR('',#75177,0.999999999999996);
#22672=VECTOR('',#75180,0.999999999999996);
#22673=VECTOR('',#75183,0.999999999999996);
#22674=VECTOR('',#75188,0.739000000000001);
#22675=VECTOR('',#75193,0.739000000000001);
#22676=VECTOR('',#75196,0.739000000000001);
#22677=VECTOR('',#75199,0.739000000000001);
#22678=VECTOR('',#75202,0.739000000000001);
#22679=VECTOR('',#75205,0.739000000000001);
#22680=VECTOR('',#75208,0.739000000000001);
#22681=VECTOR('',#75225,10.);
#22682=VECTOR('',#75226,10.);
#22683=VECTOR('',#75227,10.);
#22684=VECTOR('',#75228,10.);
#22685=VECTOR('',#75231,10.);
#22686=VECTOR('',#75232,10.);
#22687=VECTOR('',#75233,10.);
#22688=VECTOR('',#75236,10.);
#22689=VECTOR('',#75237,10.);
#22690=VECTOR('',#75238,10.);
#22691=VECTOR('',#75241,10.);
#22692=VECTOR('',#75242,10.);
#22693=VECTOR('',#75243,10.);
#22694=VECTOR('',#75246,10.);
#22695=VECTOR('',#75247,10.);
#22696=VECTOR('',#75248,10.);
#22697=VECTOR('',#75251,10.);
#22698=VECTOR('',#75252,10.);
#22699=VECTOR('',#75261,0.899999999999999);
#22700=VECTOR('',#75270,1.45);
#22701=VECTOR('',#75277,1.25);
#22702=VECTOR('',#75282,1.25);
#22703=VECTOR('',#75285,1.25);
#22704=VECTOR('',#75288,1.25);
#22705=VECTOR('',#75291,1.25);
#22706=VECTOR('',#75294,1.25);
#22707=VECTOR('',#75297,1.25);
#22708=VECTOR('',#75300,1.25);
#22709=VECTOR('',#75303,1.25);
#22710=VECTOR('',#75306,1.25);
#22711=VECTOR('',#75309,1.25);
#22712=VECTOR('',#75312,1.25);
#22713=VECTOR('',#75315,1.25);
#22714=VECTOR('',#75318,0.958249999999999);
#22715=VECTOR('',#75323,0.958249999999999);
#22716=VECTOR('',#75326,0.958249999999999);
#22717=VECTOR('',#75329,0.958249999999999);
#22718=VECTOR('',#75332,0.958249999999999);
#22719=VECTOR('',#75335,0.958249999999999);
#22720=VECTOR('',#75338,0.958249999999999);
#22721=VECTOR('',#75341,0.958249999999999);
#22722=VECTOR('',#75344,0.958249999999999);
#22723=VECTOR('',#75347,0.958249999999999);
#22724=VECTOR('',#75350,0.958249999999999);
#22725=VECTOR('',#75353,0.958249999999999);
#22726=VECTOR('',#75386,1.04);
#22727=VECTOR('',#75393,10.);
#22728=VECTOR('',#75394,10.);
#22729=VECTOR('',#75395,10.);
#22730=VECTOR('',#75400,10.);
#22731=VECTOR('',#75403,10.);
#22732=VECTOR('',#75408,10.);
#22733=VECTOR('',#75411,10.);
#22734=VECTOR('',#75414,10.);
#22735=VECTOR('',#75417,10.);
#22736=VECTOR('',#75420,10.);
#22737=VECTOR('',#75423,10.);
#22738=VECTOR('',#75426,10.);
#22739=VECTOR('',#75429,10.);
#22740=VECTOR('',#75432,10.);
#22741=VECTOR('',#75435,10.);
#22742=VECTOR('',#75438,10.);
#22743=VECTOR('',#75441,10.);
#22744=VECTOR('',#75444,10.);
#22745=VECTOR('',#75447,10.);
#22746=VECTOR('',#75450,10.);
#22747=VECTOR('',#75453,10.);
#22748=VECTOR('',#75456,10.);
#22749=VECTOR('',#75459,10.);
#22750=VECTOR('',#75462,10.);
#22751=VECTOR('',#75465,10.);
#22752=VECTOR('',#75468,10.);
#22753=VECTOR('',#75471,10.);
#22754=VECTOR('',#75474,10.);
#22755=VECTOR('',#75477,10.);
#22756=VECTOR('',#75480,10.);
#22757=VECTOR('',#75483,10.);
#22758=VECTOR('',#75486,10.);
#22759=VECTOR('',#75489,10.);
#22760=VECTOR('',#75492,10.);
#22761=VECTOR('',#75495,10.);
#22762=VECTOR('',#75498,10.);
#22763=VECTOR('',#75501,10.);
#22764=VECTOR('',#75504,10.);
#22765=VECTOR('',#75507,10.);
#22766=VECTOR('',#75510,10.);
#22767=VECTOR('',#75513,10.);
#22768=VECTOR('',#75516,10.);
#22769=VECTOR('',#75519,2.25);
#22770=VECTOR('',#75526,10.);
#22771=VECTOR('',#75529,10.);
#22772=VECTOR('',#75532,10.);
#22773=VECTOR('',#75535,10.);
#22774=VECTOR('',#75538,10.);
#22775=VECTOR('',#75541,10.);
#22776=VECTOR('',#75544,10.);
#22777=VECTOR('',#75547,10.);
#22778=VECTOR('',#75550,10.);
#22779=VECTOR('',#75553,10.);
#22780=VECTOR('',#75556,10.);
#22781=VECTOR('',#75559,10.);
#22782=VECTOR('',#75562,10.);
#22783=VECTOR('',#75565,10.);
#22784=VECTOR('',#75568,10.);
#22785=VECTOR('',#75571,10.);
#22786=VECTOR('',#75574,10.);
#22787=VECTOR('',#75577,10.);
#22788=VECTOR('',#75580,10.);
#22789=VECTOR('',#75583,10.);
#22790=VECTOR('',#75586,10.);
#22791=VECTOR('',#75589,10.);
#22792=VECTOR('',#75592,10.);
#22793=VECTOR('',#75595,10.);
#22794=VECTOR('',#75598,10.);
#22795=VECTOR('',#75601,10.);
#22796=VECTOR('',#75604,10.);
#22797=VECTOR('',#75607,10.);
#22798=VECTOR('',#75610,10.);
#22799=VECTOR('',#75613,10.);
#22800=VECTOR('',#75616,10.);
#22801=VECTOR('',#75619,10.);
#22802=VECTOR('',#75622,10.);
#22803=VECTOR('',#75627,10.);
#22804=VECTOR('',#75628,10.);
#22805=VECTOR('',#75631,10.);
#22806=VECTOR('',#75636,10.);
#22807=VECTOR('',#75637,10.);
#22808=VECTOR('',#75640,10.);
#22809=VECTOR('',#75645,10.);
#22810=VECTOR('',#75646,10.);
#22811=VECTOR('',#75649,10.);
#22812=VECTOR('',#75654,10.);
#22813=VECTOR('',#75655,10.);
#22814=VECTOR('',#75658,10.);
#22815=VECTOR('',#75663,10.);
#22816=VECTOR('',#75664,10.);
#22817=VECTOR('',#75667,10.);
#22818=VECTOR('',#75672,10.);
#22819=VECTOR('',#75673,10.);
#22820=VECTOR('',#75676,10.);
#22821=VECTOR('',#75681,10.);
#22822=VECTOR('',#75682,10.);
#22823=VECTOR('',#75685,10.);
#22824=VECTOR('',#75690,10.);
#22825=VECTOR('',#75691,10.);
#22826=VECTOR('',#75694,10.);
#22827=VECTOR('',#75699,10.);
#22828=VECTOR('',#75700,10.);
#22829=VECTOR('',#75703,10.);
#22830=VECTOR('',#75708,10.);
#22831=VECTOR('',#75709,10.);
#22832=VECTOR('',#75712,10.);
#22833=VECTOR('',#75717,10.);
#22834=VECTOR('',#75718,10.);
#22835=VECTOR('',#75721,10.);
#22836=VECTOR('',#75726,10.);
#22837=VECTOR('',#75727,10.);
#22838=VECTOR('',#75730,10.);
#22839=VECTOR('',#75735,10.);
#22840=VECTOR('',#75736,10.);
#22841=VECTOR('',#75739,10.);
#22842=VECTOR('',#75744,10.);
#22843=VECTOR('',#75745,10.);
#22844=VECTOR('',#75748,10.);
#22845=VECTOR('',#75753,10.);
#22846=VECTOR('',#75754,10.);
#22847=VECTOR('',#75757,10.);
#22848=VECTOR('',#75762,10.);
#22849=VECTOR('',#75763,10.);
#22850=VECTOR('',#75766,10.);
#22851=VECTOR('',#75771,10.);
#22852=VECTOR('',#75772,10.);
#22853=VECTOR('',#75775,10.);
#22854=VECTOR('',#75780,10.);
#22855=VECTOR('',#75781,10.);
#22856=VECTOR('',#75784,10.);
#22857=VECTOR('',#75789,10.);
#22858=VECTOR('',#75790,10.);
#22859=VECTOR('',#75793,10.);
#22860=VECTOR('',#75798,10.);
#22861=VECTOR('',#75799,10.);
#22862=VECTOR('',#75802,10.);
#22863=VECTOR('',#75807,10.);
#22864=VECTOR('',#75808,10.);
#22865=VECTOR('',#75811,10.);
#22866=VECTOR('',#75816,10.);
#22867=VECTOR('',#75817,10.);
#22868=VECTOR('',#75820,10.);
#22869=VECTOR('',#75825,10.);
#22870=VECTOR('',#75826,10.);
#22871=VECTOR('',#75829,10.);
#22872=VECTOR('',#75834,10.);
#22873=VECTOR('',#75835,10.);
#22874=VECTOR('',#75838,10.);
#22875=VECTOR('',#75843,10.);
#22876=VECTOR('',#75844,10.);
#22877=VECTOR('',#75847,10.);
#22878=VECTOR('',#75852,10.);
#22879=VECTOR('',#75853,10.);
#22880=VECTOR('',#75856,10.);
#22881=VECTOR('',#75861,10.);
#22882=VECTOR('',#75862,10.);
#22883=VECTOR('',#75865,10.);
#22884=VECTOR('',#75870,10.);
#22885=VECTOR('',#75871,10.);
#22886=VECTOR('',#75874,10.);
#22887=VECTOR('',#75879,10.);
#22888=VECTOR('',#75880,10.);
#22889=VECTOR('',#75883,10.);
#22890=VECTOR('',#75888,10.);
#22891=VECTOR('',#75889,10.);
#22892=VECTOR('',#75892,10.);
#22893=VECTOR('',#75897,10.);
#22894=VECTOR('',#75898,10.);
#22895=VECTOR('',#75901,10.);
#22896=VECTOR('',#75906,10.);
#22897=VECTOR('',#75907,10.);
#22898=VECTOR('',#75910,10.);
#22899=VECTOR('',#75915,10.);
#22900=VECTOR('',#75916,10.);
#22901=VECTOR('',#75919,10.);
#22902=VECTOR('',#75924,10.);
#22903=VECTOR('',#75925,10.);
#22904=VECTOR('',#75928,10.);
#22905=VECTOR('',#75933,10.);
#22906=VECTOR('',#75934,10.);
#22907=VECTOR('',#75937,10.);
#22908=VECTOR('',#75948,2.1);
#22909=VECTOR('',#75955,1.20470053837925);
#22910=VECTOR('',#75970,10.);
#22911=VECTOR('',#75971,10.);
#22912=VECTOR('',#75976,10.);
#22913=VECTOR('',#75977,10.);
#22914=VECTOR('',#75982,10.);
#22915=VECTOR('',#75985,10.);
#22916=VECTOR('',#75988,10.);
#22917=VECTOR('',#75989,10.);
#22918=VECTOR('',#75994,10.);
#22919=VECTOR('',#75997,10.);
#22920=VECTOR('',#76000,10.);
#22921=VECTOR('',#76003,10.);
#22922=VECTOR('',#76006,10.);
#22923=VECTOR('',#76007,10.);
#22924=VECTOR('',#76008,10.);
#22925=VECTOR('',#76009,10.);
#22926=VECTOR('',#76012,10.);
#22927=VECTOR('',#76013,10.);
#22928=VECTOR('',#76014,10.);
#22929=VECTOR('',#76017,10.);
#22930=VECTOR('',#76018,10.);
#22931=VECTOR('',#76019,10.);
#22932=VECTOR('',#76026,10.);
#22933=VECTOR('',#76031,10.);
#22934=VECTOR('',#76034,10.);
#22935=VECTOR('',#76037,10.);
#22936=VECTOR('',#76054,10.);
#22937=VECTOR('',#76059,10.);
#22938=VECTOR('',#76064,1.15470053837925);
#22939=VECTOR('',#76067,10.);
#22940=VECTOR('',#76070,10.);
#22941=VECTOR('',#76083,0.85);
#22942=VECTOR('',#76088,1.);
#22943=VECTOR('',#76093,0.85);
#22944=B_SPLINE_CURVE_WITH_KNOTS('',2,(#76154,#76155,#76156),
 .UNSPECIFIED.,.F.,.F.,(3,3),(0.,1.),.UNSPECIFIED.);
#22945=B_SPLINE_CURVE_WITH_KNOTS('',2,(#76160,#76161,#76162),
 .UNSPECIFIED.,.F.,.F.,(3,3),(0.,1.),.UNSPECIFIED.);
#22946=B_SPLINE_CURVE_WITH_KNOTS('',2,(#76171,#76172,#76173),
 .UNSPECIFIED.,.F.,.F.,(3,3),(0.,1.),.UNSPECIFIED.);
#22947=B_SPLINE_CURVE_WITH_KNOTS('',2,(#76176,#76177,#76178),
 .UNSPECIFIED.,.F.,.F.,(3,3),(0.,1.),.UNSPECIFIED.);
#22948=B_SPLINE_CURVE_WITH_KNOTS('',2,(#76186,#76187,#76188),
 .UNSPECIFIED.,.F.,.F.,(3,3),(0.,1.),.UNSPECIFIED.);
#22949=B_SPLINE_CURVE_WITH_KNOTS('',2,(#76191,#76192,#76193),
 .UNSPECIFIED.,.F.,.F.,(3,3),(0.,1.),.UNSPECIFIED.);
#22950=B_SPLINE_CURVE_WITH_KNOTS('',2,(#76201,#76202,#76203),
 .UNSPECIFIED.,.F.,.F.,(3,3),(0.,1.),.UNSPECIFIED.);
#22951=B_SPLINE_CURVE_WITH_KNOTS('',2,(#76206,#76207,#76208),
 .UNSPECIFIED.,.F.,.F.,(3,3),(0.,1.),.UNSPECIFIED.);
#22952=B_SPLINE_CURVE_WITH_KNOTS('',2,(#76216,#76217,#76218),
 .UNSPECIFIED.,.F.,.F.,(3,3),(0.,1.),.UNSPECIFIED.);
#22953=B_SPLINE_CURVE_WITH_KNOTS('',2,(#76221,#76222,#76223),
 .UNSPECIFIED.,.F.,.F.,(3,3),(0.,1.),.UNSPECIFIED.);
#22954=B_SPLINE_CURVE_WITH_KNOTS('',2,(#76231,#76232,#76233),
 .UNSPECIFIED.,.F.,.F.,(3,3),(0.,1.),.UNSPECIFIED.);
#22955=B_SPLINE_CURVE_WITH_KNOTS('',2,(#76236,#76237,#76238),
 .UNSPECIFIED.,.F.,.F.,(3,3),(0.,1.),.UNSPECIFIED.);
#22956=B_SPLINE_CURVE_WITH_KNOTS('',2,(#76246,#76247,#76248),
 .UNSPECIFIED.,.F.,.F.,(3,3),(0.,1.),.UNSPECIFIED.);
#22957=B_SPLINE_CURVE_WITH_KNOTS('',2,(#76251,#76252,#76253),
 .UNSPECIFIED.,.F.,.F.,(3,3),(0.,1.),.UNSPECIFIED.);
#22958=B_SPLINE_CURVE_WITH_KNOTS('',2,(#76260,#76261,#76262),
 .UNSPECIFIED.,.F.,.F.,(3,3),(0.,1.),.UNSPECIFIED.);
#22959=B_SPLINE_CURVE_WITH_KNOTS('',2,(#76263,#76264,#76265),
 .UNSPECIFIED.,.F.,.F.,(3,3),(0.,1.),.UNSPECIFIED.);
#22960=B_SPLINE_CURVE_WITH_KNOTS('',2,(#76274,#76275,#76276),
 .UNSPECIFIED.,.F.,.F.,(3,3),(0.,1.),.UNSPECIFIED.);
#22961=B_SPLINE_CURVE_WITH_KNOTS('',2,(#76280,#76281,#76282),
 .UNSPECIFIED.,.F.,.F.,(3,3),(0.,1.),.UNSPECIFIED.);
#22962=B_SPLINE_CURVE_WITH_KNOTS('',2,(#76291,#76292,#76293),
 .UNSPECIFIED.,.F.,.F.,(3,3),(0.,1.),.UNSPECIFIED.);
#22963=B_SPLINE_CURVE_WITH_KNOTS('',2,(#76296,#76297,#76298),
 .UNSPECIFIED.,.F.,.F.,(3,3),(0.,1.),.UNSPECIFIED.);
#22964=B_SPLINE_CURVE_WITH_KNOTS('',2,(#76306,#76307,#76308),
 .UNSPECIFIED.,.F.,.F.,(3,3),(0.,1.),.UNSPECIFIED.);
#22965=B_SPLINE_CURVE_WITH_KNOTS('',2,(#76311,#76312,#76313),
 .UNSPECIFIED.,.F.,.F.,(3,3),(0.,1.),.UNSPECIFIED.);
#22966=B_SPLINE_CURVE_WITH_KNOTS('',2,(#76321,#76322,#76323),
 .UNSPECIFIED.,.F.,.F.,(3,3),(0.,1.),.UNSPECIFIED.);
#22967=B_SPLINE_CURVE_WITH_KNOTS('',2,(#76326,#76327,#76328),
 .UNSPECIFIED.,.F.,.F.,(3,3),(0.,1.),.UNSPECIFIED.);
#22968=B_SPLINE_CURVE_WITH_KNOTS('',2,(#76336,#76337,#76338),
 .UNSPECIFIED.,.F.,.F.,(3,3),(0.,1.),.UNSPECIFIED.);
#22969=B_SPLINE_CURVE_WITH_KNOTS('',2,(#76341,#76342,#76343),
 .UNSPECIFIED.,.F.,.F.,(3,3),(0.,1.),.UNSPECIFIED.);
#22970=B_SPLINE_CURVE_WITH_KNOTS('',2,(#76351,#76352,#76353),
 .UNSPECIFIED.,.F.,.F.,(3,3),(0.,1.),.UNSPECIFIED.);
#22971=B_SPLINE_CURVE_WITH_KNOTS('',2,(#76356,#76357,#76358),
 .UNSPECIFIED.,.F.,.F.,(3,3),(0.,1.),.UNSPECIFIED.);
#22972=B_SPLINE_CURVE_WITH_KNOTS('',2,(#76366,#76367,#76368),
 .UNSPECIFIED.,.F.,.F.,(3,3),(0.,1.),.UNSPECIFIED.);
#22973=B_SPLINE_CURVE_WITH_KNOTS('',2,(#76371,#76372,#76373),
 .UNSPECIFIED.,.F.,.F.,(3,3),(0.,1.),.UNSPECIFIED.);
#22974=B_SPLINE_CURVE_WITH_KNOTS('',2,(#76381,#76382,#76383),
 .UNSPECIFIED.,.F.,.F.,(3,3),(0.,1.),.UNSPECIFIED.);
#22975=B_SPLINE_CURVE_WITH_KNOTS('',2,(#76386,#76387,#76388),
 .UNSPECIFIED.,.F.,.F.,(3,3),(0.,1.),.UNSPECIFIED.);
#22976=B_SPLINE_CURVE_WITH_KNOTS('',2,(#76396,#76397,#76398),
 .UNSPECIFIED.,.F.,.F.,(3,3),(0.,1.),.UNSPECIFIED.);
#22977=B_SPLINE_CURVE_WITH_KNOTS('',2,(#76401,#76402,#76403),
 .UNSPECIFIED.,.F.,.F.,(3,3),(0.,1.),.UNSPECIFIED.);
#22978=B_SPLINE_CURVE_WITH_KNOTS('',2,(#76411,#76412,#76413),
 .UNSPECIFIED.,.F.,.F.,(3,3),(0.,1.),.UNSPECIFIED.);
#22979=B_SPLINE_CURVE_WITH_KNOTS('',2,(#76416,#76417,#76418),
 .UNSPECIFIED.,.F.,.F.,(3,3),(0.,1.),.UNSPECIFIED.);
#22980=B_SPLINE_CURVE_WITH_KNOTS('',2,(#76426,#76427,#76428),
 .UNSPECIFIED.,.F.,.F.,(3,3),(0.,1.),.UNSPECIFIED.);
#22981=B_SPLINE_CURVE_WITH_KNOTS('',2,(#76431,#76432,#76433),
 .UNSPECIFIED.,.F.,.F.,(3,3),(0.,1.),.UNSPECIFIED.);
#22982=B_SPLINE_CURVE_WITH_KNOTS('',2,(#76440,#76441,#76442),
 .UNSPECIFIED.,.F.,.F.,(3,3),(0.,1.),.UNSPECIFIED.);
#22983=B_SPLINE_CURVE_WITH_KNOTS('',2,(#76443,#76444,#76445),
 .UNSPECIFIED.,.F.,.F.,(3,3),(0.,1.),.UNSPECIFIED.);
#22984=B_SPLINE_CURVE_WITH_KNOTS('',2,(#76455,#76456,#76457),
 .UNSPECIFIED.,.F.,.F.,(3,3),(0.,1.),.UNSPECIFIED.);
#22985=B_SPLINE_CURVE_WITH_KNOTS('',2,(#76461,#76462,#76463),
 .UNSPECIFIED.,.F.,.F.,(3,3),(0.,1.),.UNSPECIFIED.);
#22986=B_SPLINE_CURVE_WITH_KNOTS('',2,(#76472,#76473,#76474),
 .UNSPECIFIED.,.F.,.F.,(3,3),(0.,1.),.UNSPECIFIED.);
#22987=B_SPLINE_CURVE_WITH_KNOTS('',2,(#76477,#76478,#76479),
 .UNSPECIFIED.,.F.,.F.,(3,3),(0.,1.),.UNSPECIFIED.);
#22988=B_SPLINE_CURVE_WITH_KNOTS('',2,(#76487,#76488,#76489),
 .UNSPECIFIED.,.F.,.F.,(3,3),(0.,1.),.UNSPECIFIED.);
#22989=B_SPLINE_CURVE_WITH_KNOTS('',2,(#76492,#76493,#76494),
 .UNSPECIFIED.,.F.,.F.,(3,3),(0.,1.),.UNSPECIFIED.);
#22990=B_SPLINE_CURVE_WITH_KNOTS('',2,(#76502,#76503,#76504),
 .UNSPECIFIED.,.F.,.F.,(3,3),(0.,1.),.UNSPECIFIED.);
#22991=B_SPLINE_CURVE_WITH_KNOTS('',2,(#76507,#76508,#76509),
 .UNSPECIFIED.,.F.,.F.,(3,3),(0.,1.),.UNSPECIFIED.);
#22992=B_SPLINE_CURVE_WITH_KNOTS('',2,(#76517,#76518,#76519),
 .UNSPECIFIED.,.F.,.F.,(3,3),(0.,1.),.UNSPECIFIED.);
#22993=B_SPLINE_CURVE_WITH_KNOTS('',2,(#76522,#76523,#76524),
 .UNSPECIFIED.,.F.,.F.,(3,3),(0.,1.),.UNSPECIFIED.);
#22994=B_SPLINE_CURVE_WITH_KNOTS('',2,(#76532,#76533,#76534),
 .UNSPECIFIED.,.F.,.F.,(3,3),(0.,1.),.UNSPECIFIED.);
#22995=B_SPLINE_CURVE_WITH_KNOTS('',2,(#76537,#76538,#76539),
 .UNSPECIFIED.,.F.,.F.,(3,3),(0.,1.),.UNSPECIFIED.);
#22996=B_SPLINE_CURVE_WITH_KNOTS('',2,(#76547,#76548,#76549),
 .UNSPECIFIED.,.F.,.F.,(3,3),(0.,1.),.UNSPECIFIED.);
#22997=B_SPLINE_CURVE_WITH_KNOTS('',2,(#76552,#76553,#76554),
 .UNSPECIFIED.,.F.,.F.,(3,3),(0.,1.),.UNSPECIFIED.);
#22998=B_SPLINE_CURVE_WITH_KNOTS('',2,(#76561,#76562,#76563),
 .UNSPECIFIED.,.F.,.F.,(3,3),(0.,1.),.UNSPECIFIED.);
#22999=B_SPLINE_CURVE_WITH_KNOTS('',2,(#76564,#76565,#76566),
 .UNSPECIFIED.,.F.,.F.,(3,3),(0.,1.),.UNSPECIFIED.);
#23000=B_SPLINE_CURVE_WITH_KNOTS('',2,(#76575,#76576,#76577),
 .UNSPECIFIED.,.F.,.F.,(3,3),(0.,1.),.UNSPECIFIED.);
#23001=B_SPLINE_CURVE_WITH_KNOTS('',2,(#76581,#76582,#76583),
 .UNSPECIFIED.,.F.,.F.,(3,3),(0.,1.),.UNSPECIFIED.);
#23002=B_SPLINE_CURVE_WITH_KNOTS('',2,(#76592,#76593,#76594),
 .UNSPECIFIED.,.F.,.F.,(3,3),(0.,1.),.UNSPECIFIED.);
#23003=B_SPLINE_CURVE_WITH_KNOTS('',2,(#76597,#76598,#76599),
 .UNSPECIFIED.,.F.,.F.,(3,3),(0.,1.),.UNSPECIFIED.);
#23004=B_SPLINE_CURVE_WITH_KNOTS('',2,(#76607,#76608,#76609),
 .UNSPECIFIED.,.F.,.F.,(3,3),(0.,1.),.UNSPECIFIED.);
#23005=B_SPLINE_CURVE_WITH_KNOTS('',2,(#76612,#76613,#76614),
 .UNSPECIFIED.,.F.,.F.,(3,3),(0.,1.),.UNSPECIFIED.);
#23006=B_SPLINE_CURVE_WITH_KNOTS('',2,(#76622,#76623,#76624),
 .UNSPECIFIED.,.F.,.F.,(3,3),(0.,1.),.UNSPECIFIED.);
#23007=B_SPLINE_CURVE_WITH_KNOTS('',2,(#76627,#76628,#76629),
 .UNSPECIFIED.,.F.,.F.,(3,3),(0.,1.),.UNSPECIFIED.);
#23008=B_SPLINE_CURVE_WITH_KNOTS('',2,(#76637,#76638,#76639),
 .UNSPECIFIED.,.F.,.F.,(3,3),(0.,1.),.UNSPECIFIED.);
#23009=B_SPLINE_CURVE_WITH_KNOTS('',2,(#76642,#76643,#76644),
 .UNSPECIFIED.,.F.,.F.,(3,3),(0.,1.),.UNSPECIFIED.);
#23010=B_SPLINE_CURVE_WITH_KNOTS('',2,(#76652,#76653,#76654),
 .UNSPECIFIED.,.F.,.F.,(3,3),(0.,1.),.UNSPECIFIED.);
#23011=B_SPLINE_CURVE_WITH_KNOTS('',2,(#76657,#76658,#76659),
 .UNSPECIFIED.,.F.,.F.,(3,3),(0.,1.),.UNSPECIFIED.);
#23012=B_SPLINE_CURVE_WITH_KNOTS('',2,(#76667,#76668,#76669),
 .UNSPECIFIED.,.F.,.F.,(3,3),(0.,1.),.UNSPECIFIED.);
#23013=B_SPLINE_CURVE_WITH_KNOTS('',2,(#76672,#76673,#76674),
 .UNSPECIFIED.,.F.,.F.,(3,3),(0.,1.),.UNSPECIFIED.);
#23014=B_SPLINE_CURVE_WITH_KNOTS('',2,(#76682,#76683,#76684),
 .UNSPECIFIED.,.F.,.F.,(3,3),(0.,1.),.UNSPECIFIED.);
#23015=B_SPLINE_CURVE_WITH_KNOTS('',2,(#76687,#76688,#76689),
 .UNSPECIFIED.,.F.,.F.,(3,3),(0.,1.),.UNSPECIFIED.);
#23016=B_SPLINE_CURVE_WITH_KNOTS('',2,(#76697,#76698,#76699),
 .UNSPECIFIED.,.F.,.F.,(3,3),(0.,1.),.UNSPECIFIED.);
#23017=B_SPLINE_CURVE_WITH_KNOTS('',2,(#76702,#76703,#76704),
 .UNSPECIFIED.,.F.,.F.,(3,3),(0.,1.),.UNSPECIFIED.);
#23018=B_SPLINE_CURVE_WITH_KNOTS('',2,(#76712,#76713,#76714),
 .UNSPECIFIED.,.F.,.F.,(3,3),(0.,1.),.UNSPECIFIED.);
#23019=B_SPLINE_CURVE_WITH_KNOTS('',2,(#76717,#76718,#76719),
 .UNSPECIFIED.,.F.,.F.,(3,3),(0.,1.),.UNSPECIFIED.);
#23020=B_SPLINE_CURVE_WITH_KNOTS('',2,(#76727,#76728,#76729),
 .UNSPECIFIED.,.F.,.F.,(3,3),(0.,1.),.UNSPECIFIED.);
#23021=B_SPLINE_CURVE_WITH_KNOTS('',2,(#76732,#76733,#76734),
 .UNSPECIFIED.,.F.,.F.,(3,3),(0.,1.),.UNSPECIFIED.);
#23022=B_SPLINE_CURVE_WITH_KNOTS('',2,(#76742,#76743,#76744),
 .UNSPECIFIED.,.F.,.F.,(3,3),(0.,1.),.UNSPECIFIED.);
#23023=B_SPLINE_CURVE_WITH_KNOTS('',2,(#76747,#76748,#76749),
 .UNSPECIFIED.,.F.,.F.,(3,3),(0.,1.),.UNSPECIFIED.);
#23024=B_SPLINE_CURVE_WITH_KNOTS('',2,(#76757,#76758,#76759),
 .UNSPECIFIED.,.F.,.F.,(3,3),(0.,1.),.UNSPECIFIED.);
#23025=B_SPLINE_CURVE_WITH_KNOTS('',2,(#76762,#76763,#76764),
 .UNSPECIFIED.,.F.,.F.,(3,3),(0.,1.),.UNSPECIFIED.);
#23026=B_SPLINE_CURVE_WITH_KNOTS('',2,(#76772,#76773,#76774),
 .UNSPECIFIED.,.F.,.F.,(3,3),(0.,1.),.UNSPECIFIED.);
#23027=B_SPLINE_CURVE_WITH_KNOTS('',2,(#76777,#76778,#76779),
 .UNSPECIFIED.,.F.,.F.,(3,3),(0.,1.),.UNSPECIFIED.);
#23028=B_SPLINE_CURVE_WITH_KNOTS('',2,(#76787,#76788,#76789),
 .UNSPECIFIED.,.F.,.F.,(3,3),(0.,1.),.UNSPECIFIED.);
#23029=B_SPLINE_CURVE_WITH_KNOTS('',2,(#76792,#76793,#76794),
 .UNSPECIFIED.,.F.,.F.,(3,3),(0.,1.),.UNSPECIFIED.);
#23030=B_SPLINE_CURVE_WITH_KNOTS('',2,(#76802,#76803,#76804),
 .UNSPECIFIED.,.F.,.F.,(3,3),(0.,1.),.UNSPECIFIED.);
#23031=B_SPLINE_CURVE_WITH_KNOTS('',2,(#76807,#76808,#76809),
 .UNSPECIFIED.,.F.,.F.,(3,3),(0.,1.),.UNSPECIFIED.);
#23032=B_SPLINE_CURVE_WITH_KNOTS('',2,(#76817,#76818,#76819),
 .UNSPECIFIED.,.F.,.F.,(3,3),(0.,1.),.UNSPECIFIED.);
#23033=B_SPLINE_CURVE_WITH_KNOTS('',2,(#76822,#76823,#76824),
 .UNSPECIFIED.,.F.,.F.,(3,3),(0.,1.),.UNSPECIFIED.);
#23034=B_SPLINE_CURVE_WITH_KNOTS('',2,(#76832,#76833,#76834),
 .UNSPECIFIED.,.F.,.F.,(3,3),(0.,1.),.UNSPECIFIED.);
#23035=B_SPLINE_CURVE_WITH_KNOTS('',2,(#76837,#76838,#76839),
 .UNSPECIFIED.,.F.,.F.,(3,3),(0.,1.),.UNSPECIFIED.);
#23036=B_SPLINE_CURVE_WITH_KNOTS('',2,(#76847,#76848,#76849),
 .UNSPECIFIED.,.F.,.F.,(3,3),(0.,1.),.UNSPECIFIED.);
#23037=B_SPLINE_CURVE_WITH_KNOTS('',2,(#76852,#76853,#76854),
 .UNSPECIFIED.,.F.,.F.,(3,3),(0.,1.),.UNSPECIFIED.);
#23038=B_SPLINE_CURVE_WITH_KNOTS('',2,(#76862,#76863,#76864),
 .UNSPECIFIED.,.F.,.F.,(3,3),(0.,1.),.UNSPECIFIED.);
#23039=B_SPLINE_CURVE_WITH_KNOTS('',2,(#76867,#76868,#76869),
 .UNSPECIFIED.,.F.,.F.,(3,3),(0.,1.),.UNSPECIFIED.);
#23040=B_SPLINE_CURVE_WITH_KNOTS('',2,(#76882,#76883,#76884),
 .UNSPECIFIED.,.F.,.F.,(3,3),(0.,1.),.UNSPECIFIED.);
#23041=B_SPLINE_CURVE_WITH_KNOTS('',2,(#76885,#76886,#76887),
 .UNSPECIFIED.,.F.,.F.,(3,3),(0.,1.),.UNSPECIFIED.);
#23042=B_SPLINE_CURVE_WITH_KNOTS('',2,(#76899,#76900,#76901),
 .UNSPECIFIED.,.F.,.F.,(3,3),(0.,1.),.UNSPECIFIED.);
#23043=B_SPLINE_CURVE_WITH_KNOTS('',2,(#76905,#76906,#76907),
 .UNSPECIFIED.,.F.,.F.,(3,3),(0.,1.),.UNSPECIFIED.);
#23044=B_SPLINE_CURVE_WITH_KNOTS('',2,(#76916,#76917,#76918),
 .UNSPECIFIED.,.F.,.F.,(3,3),(0.,1.),.UNSPECIFIED.);
#23045=B_SPLINE_CURVE_WITH_KNOTS('',2,(#76921,#76922,#76923),
 .UNSPECIFIED.,.F.,.F.,(3,3),(0.,1.),.UNSPECIFIED.);
#23046=B_SPLINE_CURVE_WITH_KNOTS('',2,(#76931,#76932,#76933),
 .UNSPECIFIED.,.F.,.F.,(3,3),(0.,1.),.UNSPECIFIED.);
#23047=B_SPLINE_CURVE_WITH_KNOTS('',2,(#76936,#76937,#76938),
 .UNSPECIFIED.,.F.,.F.,(3,3),(0.,1.),.UNSPECIFIED.);
#23048=B_SPLINE_CURVE_WITH_KNOTS('',2,(#76946,#76947,#76948),
 .UNSPECIFIED.,.F.,.F.,(3,3),(0.,1.),.UNSPECIFIED.);
#23049=B_SPLINE_CURVE_WITH_KNOTS('',2,(#76951,#76952,#76953),
 .UNSPECIFIED.,.F.,.F.,(3,3),(0.,1.),.UNSPECIFIED.);
#23050=B_SPLINE_CURVE_WITH_KNOTS('',2,(#76961,#76962,#76963),
 .UNSPECIFIED.,.F.,.F.,(3,3),(0.,1.),.UNSPECIFIED.);
#23051=B_SPLINE_CURVE_WITH_KNOTS('',2,(#76966,#76967,#76968),
 .UNSPECIFIED.,.F.,.F.,(3,3),(0.,1.),.UNSPECIFIED.);
#23052=B_SPLINE_CURVE_WITH_KNOTS('',2,(#76976,#76977,#76978),
 .UNSPECIFIED.,.F.,.F.,(3,3),(0.,1.),.UNSPECIFIED.);
#23053=B_SPLINE_CURVE_WITH_KNOTS('',2,(#76981,#76982,#76983),
 .UNSPECIFIED.,.F.,.F.,(3,3),(0.,1.),.UNSPECIFIED.);
#23054=B_SPLINE_CURVE_WITH_KNOTS('',2,(#76991,#76992,#76993),
 .UNSPECIFIED.,.F.,.F.,(3,3),(0.,1.),.UNSPECIFIED.);
#23055=B_SPLINE_CURVE_WITH_KNOTS('',2,(#76996,#76997,#76998),
 .UNSPECIFIED.,.F.,.F.,(3,3),(0.,1.),.UNSPECIFIED.);
#23056=B_SPLINE_CURVE_WITH_KNOTS('',2,(#77005,#77006,#77007),
 .UNSPECIFIED.,.F.,.F.,(3,3),(0.,1.),.UNSPECIFIED.);
#23057=B_SPLINE_CURVE_WITH_KNOTS('',2,(#77008,#77009,#77010),
 .UNSPECIFIED.,.F.,.F.,(3,3),(0.,1.),.UNSPECIFIED.);
#23058=B_SPLINE_CURVE_WITH_KNOTS('',2,(#77019,#77020,#77021),
 .UNSPECIFIED.,.F.,.F.,(3,3),(0.,1.),.UNSPECIFIED.);
#23059=B_SPLINE_CURVE_WITH_KNOTS('',2,(#77025,#77026,#77027),
 .UNSPECIFIED.,.F.,.F.,(3,3),(0.,1.),.UNSPECIFIED.);
#23060=B_SPLINE_CURVE_WITH_KNOTS('',2,(#77036,#77037,#77038),
 .UNSPECIFIED.,.F.,.F.,(3,3),(0.,1.),.UNSPECIFIED.);
#23061=B_SPLINE_CURVE_WITH_KNOTS('',2,(#77041,#77042,#77043),
 .UNSPECIFIED.,.F.,.F.,(3,3),(0.,1.),.UNSPECIFIED.);
#23062=B_SPLINE_CURVE_WITH_KNOTS('',2,(#77051,#77052,#77053),
 .UNSPECIFIED.,.F.,.F.,(3,3),(0.,1.),.UNSPECIFIED.);
#23063=B_SPLINE_CURVE_WITH_KNOTS('',2,(#77056,#77057,#77058),
 .UNSPECIFIED.,.F.,.F.,(3,3),(0.,1.),.UNSPECIFIED.);
#23064=B_SPLINE_CURVE_WITH_KNOTS('',2,(#77066,#77067,#77068),
 .UNSPECIFIED.,.F.,.F.,(3,3),(0.,1.),.UNSPECIFIED.);
#23065=B_SPLINE_CURVE_WITH_KNOTS('',2,(#77071,#77072,#77073),
 .UNSPECIFIED.,.F.,.F.,(3,3),(0.,1.),.UNSPECIFIED.);
#23066=B_SPLINE_CURVE_WITH_KNOTS('',2,(#77081,#77082,#77083),
 .UNSPECIFIED.,.F.,.F.,(3,3),(0.,1.),.UNSPECIFIED.);
#23067=B_SPLINE_CURVE_WITH_KNOTS('',2,(#77086,#77087,#77088),
 .UNSPECIFIED.,.F.,.F.,(3,3),(0.,1.),.UNSPECIFIED.);
#23068=B_SPLINE_CURVE_WITH_KNOTS('',2,(#77096,#77097,#77098),
 .UNSPECIFIED.,.F.,.F.,(3,3),(0.,1.),.UNSPECIFIED.);
#23069=B_SPLINE_CURVE_WITH_KNOTS('',2,(#77101,#77102,#77103),
 .UNSPECIFIED.,.F.,.F.,(3,3),(0.,1.),.UNSPECIFIED.);
#23070=B_SPLINE_CURVE_WITH_KNOTS('',2,(#77111,#77112,#77113),
 .UNSPECIFIED.,.F.,.F.,(3,3),(0.,1.),.UNSPECIFIED.);
#23071=B_SPLINE_CURVE_WITH_KNOTS('',2,(#77116,#77117,#77118),
 .UNSPECIFIED.,.F.,.F.,(3,3),(0.,1.),.UNSPECIFIED.);
#23072=B_SPLINE_CURVE_WITH_KNOTS('',2,(#77126,#77127,#77128),
 .UNSPECIFIED.,.F.,.F.,(3,3),(0.,1.),.UNSPECIFIED.);
#23073=B_SPLINE_CURVE_WITH_KNOTS('',2,(#77131,#77132,#77133),
 .UNSPECIFIED.,.F.,.F.,(3,3),(0.,1.),.UNSPECIFIED.);
#23074=B_SPLINE_CURVE_WITH_KNOTS('',2,(#77141,#77142,#77143),
 .UNSPECIFIED.,.F.,.F.,(3,3),(0.,1.),.UNSPECIFIED.);
#23075=B_SPLINE_CURVE_WITH_KNOTS('',2,(#77146,#77147,#77148),
 .UNSPECIFIED.,.F.,.F.,(3,3),(0.,1.),.UNSPECIFIED.);
#23076=B_SPLINE_CURVE_WITH_KNOTS('',2,(#77156,#77157,#77158),
 .UNSPECIFIED.,.F.,.F.,(3,3),(0.,1.),.UNSPECIFIED.);
#23077=B_SPLINE_CURVE_WITH_KNOTS('',2,(#77161,#77162,#77163),
 .UNSPECIFIED.,.F.,.F.,(3,3),(0.,1.),.UNSPECIFIED.);
#23078=B_SPLINE_CURVE_WITH_KNOTS('',2,(#77171,#77172,#77173),
 .UNSPECIFIED.,.F.,.F.,(3,3),(0.,1.),.UNSPECIFIED.);
#23079=B_SPLINE_CURVE_WITH_KNOTS('',2,(#77176,#77177,#77178),
 .UNSPECIFIED.,.F.,.F.,(3,3),(0.,1.),.UNSPECIFIED.);
#23080=B_SPLINE_CURVE_WITH_KNOTS('',2,(#77185,#77186,#77187),
 .UNSPECIFIED.,.F.,.F.,(3,3),(0.,1.),.UNSPECIFIED.);
#23081=B_SPLINE_CURVE_WITH_KNOTS('',2,(#77188,#77189,#77190),
 .UNSPECIFIED.,.F.,.F.,(3,3),(0.,1.),.UNSPECIFIED.);
#23082=B_SPLINE_CURVE_WITH_KNOTS('',2,(#77200,#77201,#77202),
 .UNSPECIFIED.,.F.,.F.,(3,3),(0.,1.),.UNSPECIFIED.);
#23083=B_SPLINE_CURVE_WITH_KNOTS('',2,(#77206,#77207,#77208),
 .UNSPECIFIED.,.F.,.F.,(3,3),(0.,1.),.UNSPECIFIED.);
#23084=B_SPLINE_CURVE_WITH_KNOTS('',2,(#77217,#77218,#77219),
 .UNSPECIFIED.,.F.,.F.,(3,3),(0.,1.),.UNSPECIFIED.);
#23085=B_SPLINE_CURVE_WITH_KNOTS('',2,(#77222,#77223,#77224),
 .UNSPECIFIED.,.F.,.F.,(3,3),(0.,1.),.UNSPECIFIED.);
#23086=B_SPLINE_CURVE_WITH_KNOTS('',2,(#77232,#77233,#77234),
 .UNSPECIFIED.,.F.,.F.,(3,3),(0.,1.),.UNSPECIFIED.);
#23087=B_SPLINE_CURVE_WITH_KNOTS('',2,(#77237,#77238,#77239),
 .UNSPECIFIED.,.F.,.F.,(3,3),(0.,1.),.UNSPECIFIED.);
#23088=B_SPLINE_CURVE_WITH_KNOTS('',2,(#77247,#77248,#77249),
 .UNSPECIFIED.,.F.,.F.,(3,3),(0.,1.),.UNSPECIFIED.);
#23089=B_SPLINE_CURVE_WITH_KNOTS('',2,(#77252,#77253,#77254),
 .UNSPECIFIED.,.F.,.F.,(3,3),(0.,1.),.UNSPECIFIED.);
#23090=B_SPLINE_CURVE_WITH_KNOTS('',2,(#77262,#77263,#77264),
 .UNSPECIFIED.,.F.,.F.,(3,3),(0.,1.),.UNSPECIFIED.);
#23091=B_SPLINE_CURVE_WITH_KNOTS('',2,(#77267,#77268,#77269),
 .UNSPECIFIED.,.F.,.F.,(3,3),(0.,1.),.UNSPECIFIED.);
#23092=B_SPLINE_CURVE_WITH_KNOTS('',2,(#77277,#77278,#77279),
 .UNSPECIFIED.,.F.,.F.,(3,3),(0.,1.),.UNSPECIFIED.);
#23093=B_SPLINE_CURVE_WITH_KNOTS('',2,(#77282,#77283,#77284),
 .UNSPECIFIED.,.F.,.F.,(3,3),(0.,1.),.UNSPECIFIED.);
#23094=B_SPLINE_CURVE_WITH_KNOTS('',2,(#77292,#77293,#77294),
 .UNSPECIFIED.,.F.,.F.,(3,3),(0.,1.),.UNSPECIFIED.);
#23095=B_SPLINE_CURVE_WITH_KNOTS('',2,(#77297,#77298,#77299),
 .UNSPECIFIED.,.F.,.F.,(3,3),(0.,1.),.UNSPECIFIED.);
#23096=B_SPLINE_CURVE_WITH_KNOTS('',2,(#77306,#77307,#77308),
 .UNSPECIFIED.,.F.,.F.,(3,3),(0.,1.),.UNSPECIFIED.);
#23097=B_SPLINE_CURVE_WITH_KNOTS('',2,(#77309,#77310,#77311),
 .UNSPECIFIED.,.F.,.F.,(3,3),(0.,1.),.UNSPECIFIED.);
#23098=B_SPLINE_CURVE_WITH_KNOTS('',2,(#77320,#77321,#77322),
 .UNSPECIFIED.,.F.,.F.,(3,3),(0.,1.),.UNSPECIFIED.);
#23099=B_SPLINE_CURVE_WITH_KNOTS('',2,(#77326,#77327,#77328),
 .UNSPECIFIED.,.F.,.F.,(3,3),(0.,1.),.UNSPECIFIED.);
#23100=B_SPLINE_CURVE_WITH_KNOTS('',2,(#77337,#77338,#77339),
 .UNSPECIFIED.,.F.,.F.,(3,3),(0.,1.),.UNSPECIFIED.);
#23101=B_SPLINE_CURVE_WITH_KNOTS('',2,(#77342,#77343,#77344),
 .UNSPECIFIED.,.F.,.F.,(3,3),(0.,1.),.UNSPECIFIED.);
#23102=B_SPLINE_CURVE_WITH_KNOTS('',2,(#77352,#77353,#77354),
 .UNSPECIFIED.,.F.,.F.,(3,3),(0.,1.),.UNSPECIFIED.);
#23103=B_SPLINE_CURVE_WITH_KNOTS('',2,(#77357,#77358,#77359),
 .UNSPECIFIED.,.F.,.F.,(3,3),(0.,1.),.UNSPECIFIED.);
#23104=B_SPLINE_CURVE_WITH_KNOTS('',2,(#77367,#77368,#77369),
 .UNSPECIFIED.,.F.,.F.,(3,3),(0.,1.),.UNSPECIFIED.);
#23105=B_SPLINE_CURVE_WITH_KNOTS('',2,(#77372,#77373,#77374),
 .UNSPECIFIED.,.F.,.F.,(3,3),(0.,1.),.UNSPECIFIED.);
#23106=B_SPLINE_CURVE_WITH_KNOTS('',2,(#77382,#77383,#77384),
 .UNSPECIFIED.,.F.,.F.,(3,3),(0.,1.),.UNSPECIFIED.);
#23107=B_SPLINE_CURVE_WITH_KNOTS('',2,(#77387,#77388,#77389),
 .UNSPECIFIED.,.F.,.F.,(3,3),(0.,1.),.UNSPECIFIED.);
#23108=B_SPLINE_CURVE_WITH_KNOTS('',2,(#77397,#77398,#77399),
 .UNSPECIFIED.,.F.,.F.,(3,3),(0.,1.),.UNSPECIFIED.);
#23109=B_SPLINE_CURVE_WITH_KNOTS('',2,(#77402,#77403,#77404),
 .UNSPECIFIED.,.F.,.F.,(3,3),(0.,1.),.UNSPECIFIED.);
#23110=B_SPLINE_CURVE_WITH_KNOTS('',2,(#77412,#77413,#77414),
 .UNSPECIFIED.,.F.,.F.,(3,3),(0.,1.),.UNSPECIFIED.);
#23111=B_SPLINE_CURVE_WITH_KNOTS('',2,(#77417,#77418,#77419),
 .UNSPECIFIED.,.F.,.F.,(3,3),(0.,1.),.UNSPECIFIED.);
#23112=B_SPLINE_CURVE_WITH_KNOTS('',2,(#77427,#77428,#77429),
 .UNSPECIFIED.,.F.,.F.,(3,3),(0.,1.),.UNSPECIFIED.);
#23113=B_SPLINE_CURVE_WITH_KNOTS('',2,(#77432,#77433,#77434),
 .UNSPECIFIED.,.F.,.F.,(3,3),(0.,1.),.UNSPECIFIED.);
#23114=B_SPLINE_CURVE_WITH_KNOTS('',2,(#77441,#77442,#77443),
 .UNSPECIFIED.,.F.,.F.,(3,3),(0.,1.),.UNSPECIFIED.);
#23115=B_SPLINE_CURVE_WITH_KNOTS('',2,(#77444,#77445,#77446),
 .UNSPECIFIED.,.F.,.F.,(3,3),(0.,1.),.UNSPECIFIED.);
#23116=B_SPLINE_CURVE_WITH_KNOTS('',2,(#77455,#77456,#77457),
 .UNSPECIFIED.,.F.,.F.,(3,3),(0.,1.),.UNSPECIFIED.);
#23117=B_SPLINE_CURVE_WITH_KNOTS('',2,(#77461,#77462,#77463),
 .UNSPECIFIED.,.F.,.F.,(3,3),(0.,1.),.UNSPECIFIED.);
#23118=B_SPLINE_CURVE_WITH_KNOTS('',2,(#77472,#77473,#77474),
 .UNSPECIFIED.,.F.,.F.,(3,3),(0.,1.),.UNSPECIFIED.);
#23119=B_SPLINE_CURVE_WITH_KNOTS('',2,(#77477,#77478,#77479),
 .UNSPECIFIED.,.F.,.F.,(3,3),(0.,1.),.UNSPECIFIED.);
#23120=B_SPLINE_CURVE_WITH_KNOTS('',2,(#77487,#77488,#77489),
 .UNSPECIFIED.,.F.,.F.,(3,3),(0.,1.),.UNSPECIFIED.);
#23121=B_SPLINE_CURVE_WITH_KNOTS('',2,(#77492,#77493,#77494),
 .UNSPECIFIED.,.F.,.F.,(3,3),(0.,1.),.UNSPECIFIED.);
#23122=B_SPLINE_CURVE_WITH_KNOTS('',2,(#77502,#77503,#77504),
 .UNSPECIFIED.,.F.,.F.,(3,3),(0.,1.),.UNSPECIFIED.);
#23123=B_SPLINE_CURVE_WITH_KNOTS('',2,(#77507,#77508,#77509),
 .UNSPECIFIED.,.F.,.F.,(3,3),(0.,1.),.UNSPECIFIED.);
#23124=B_SPLINE_CURVE_WITH_KNOTS('',2,(#77517,#77518,#77519),
 .UNSPECIFIED.,.F.,.F.,(3,3),(0.,1.),.UNSPECIFIED.);
#23125=B_SPLINE_CURVE_WITH_KNOTS('',2,(#77522,#77523,#77524),
 .UNSPECIFIED.,.F.,.F.,(3,3),(0.,1.),.UNSPECIFIED.);
#23126=B_SPLINE_CURVE_WITH_KNOTS('',2,(#77532,#77533,#77534),
 .UNSPECIFIED.,.F.,.F.,(3,3),(0.,1.),.UNSPECIFIED.);
#23127=B_SPLINE_CURVE_WITH_KNOTS('',2,(#77537,#77538,#77539),
 .UNSPECIFIED.,.F.,.F.,(3,3),(0.,1.),.UNSPECIFIED.);
#23128=B_SPLINE_CURVE_WITH_KNOTS('',2,(#77547,#77548,#77549),
 .UNSPECIFIED.,.F.,.F.,(3,3),(0.,1.),.UNSPECIFIED.);
#23129=B_SPLINE_CURVE_WITH_KNOTS('',2,(#77552,#77553,#77554),
 .UNSPECIFIED.,.F.,.F.,(3,3),(0.,1.),.UNSPECIFIED.);
#23130=B_SPLINE_CURVE_WITH_KNOTS('',2,(#77562,#77563,#77564),
 .UNSPECIFIED.,.F.,.F.,(3,3),(0.,1.),.UNSPECIFIED.);
#23131=B_SPLINE_CURVE_WITH_KNOTS('',2,(#77567,#77568,#77569),
 .UNSPECIFIED.,.F.,.F.,(3,3),(0.,1.),.UNSPECIFIED.);
#23132=B_SPLINE_CURVE_WITH_KNOTS('',2,(#77577,#77578,#77579),
 .UNSPECIFIED.,.F.,.F.,(3,3),(0.,1.),.UNSPECIFIED.);
#23133=B_SPLINE_CURVE_WITH_KNOTS('',2,(#77582,#77583,#77584),
 .UNSPECIFIED.,.F.,.F.,(3,3),(0.,1.),.UNSPECIFIED.);
#23134=B_SPLINE_CURVE_WITH_KNOTS('',2,(#77592,#77593,#77594),
 .UNSPECIFIED.,.F.,.F.,(3,3),(0.,1.),.UNSPECIFIED.);
#23135=B_SPLINE_CURVE_WITH_KNOTS('',2,(#77597,#77598,#77599),
 .UNSPECIFIED.,.F.,.F.,(3,3),(0.,1.),.UNSPECIFIED.);
#23136=B_SPLINE_CURVE_WITH_KNOTS('',2,(#77607,#77608,#77609),
 .UNSPECIFIED.,.F.,.F.,(3,3),(0.,1.),.UNSPECIFIED.);
#23137=B_SPLINE_CURVE_WITH_KNOTS('',2,(#77612,#77613,#77614),
 .UNSPECIFIED.,.F.,.F.,(3,3),(0.,1.),.UNSPECIFIED.);
#23138=B_SPLINE_CURVE_WITH_KNOTS('',2,(#77622,#77623,#77624),
 .UNSPECIFIED.,.F.,.F.,(3,3),(0.,1.),.UNSPECIFIED.);
#23139=B_SPLINE_CURVE_WITH_KNOTS('',2,(#77627,#77628,#77629),
 .UNSPECIFIED.,.F.,.F.,(3,3),(0.,1.),.UNSPECIFIED.);
#23140=B_SPLINE_CURVE_WITH_KNOTS('',2,(#77637,#77638,#77639),
 .UNSPECIFIED.,.F.,.F.,(3,3),(0.,1.),.UNSPECIFIED.);
#23141=B_SPLINE_CURVE_WITH_KNOTS('',2,(#77642,#77643,#77644),
 .UNSPECIFIED.,.F.,.F.,(3,3),(0.,1.),.UNSPECIFIED.);
#23142=B_SPLINE_CURVE_WITH_KNOTS('',2,(#77652,#77653,#77654),
 .UNSPECIFIED.,.F.,.F.,(3,3),(0.,1.),.UNSPECIFIED.);
#23143=B_SPLINE_CURVE_WITH_KNOTS('',2,(#77657,#77658,#77659),
 .UNSPECIFIED.,.F.,.F.,(3,3),(0.,1.),.UNSPECIFIED.);
#23144=B_SPLINE_CURVE_WITH_KNOTS('',2,(#77667,#77668,#77669),
 .UNSPECIFIED.,.F.,.F.,(3,3),(0.,1.),.UNSPECIFIED.);
#23145=B_SPLINE_CURVE_WITH_KNOTS('',2,(#77672,#77673,#77674),
 .UNSPECIFIED.,.F.,.F.,(3,3),(0.,1.),.UNSPECIFIED.);
#23146=B_SPLINE_CURVE_WITH_KNOTS('',2,(#77681,#77682,#77683),
 .UNSPECIFIED.,.F.,.F.,(3,3),(0.,1.),.UNSPECIFIED.);
#23147=B_SPLINE_CURVE_WITH_KNOTS('',2,(#77684,#77685,#77686),
 .UNSPECIFIED.,.F.,.F.,(3,3),(0.,1.),.UNSPECIFIED.);
#23148=B_SPLINE_CURVE_WITH_KNOTS('',2,(#77699,#77700,#77701),
 .UNSPECIFIED.,.F.,.F.,(3,3),(0.,1.),.UNSPECIFIED.);
#23149=B_SPLINE_CURVE_WITH_KNOTS('',2,(#77705,#77706,#77707),
 .UNSPECIFIED.,.F.,.F.,(3,3),(0.,1.),.UNSPECIFIED.);
#23150=B_SPLINE_CURVE_WITH_KNOTS('',2,(#77716,#77717,#77718),
 .UNSPECIFIED.,.F.,.F.,(3,3),(0.,1.),.UNSPECIFIED.);
#23151=B_SPLINE_CURVE_WITH_KNOTS('',2,(#77721,#77722,#77723),
 .UNSPECIFIED.,.F.,.F.,(3,3),(0.,1.),.UNSPECIFIED.);
#23152=B_SPLINE_CURVE_WITH_KNOTS('',2,(#77731,#77732,#77733),
 .UNSPECIFIED.,.F.,.F.,(3,3),(0.,1.),.UNSPECIFIED.);
#23153=B_SPLINE_CURVE_WITH_KNOTS('',2,(#77736,#77737,#77738),
 .UNSPECIFIED.,.F.,.F.,(3,3),(0.,1.),.UNSPECIFIED.);
#23154=B_SPLINE_CURVE_WITH_KNOTS('',2,(#77746,#77747,#77748),
 .UNSPECIFIED.,.F.,.F.,(3,3),(0.,1.),.UNSPECIFIED.);
#23155=B_SPLINE_CURVE_WITH_KNOTS('',2,(#77751,#77752,#77753),
 .UNSPECIFIED.,.F.,.F.,(3,3),(0.,1.),.UNSPECIFIED.);
#23156=B_SPLINE_CURVE_WITH_KNOTS('',2,(#77761,#77762,#77763),
 .UNSPECIFIED.,.F.,.F.,(3,3),(0.,1.),.UNSPECIFIED.);
#23157=B_SPLINE_CURVE_WITH_KNOTS('',2,(#77766,#77767,#77768),
 .UNSPECIFIED.,.F.,.F.,(3,3),(0.,1.),.UNSPECIFIED.);
#23158=B_SPLINE_CURVE_WITH_KNOTS('',2,(#77776,#77777,#77778),
 .UNSPECIFIED.,.F.,.F.,(3,3),(0.,1.),.UNSPECIFIED.);
#23159=B_SPLINE_CURVE_WITH_KNOTS('',2,(#77781,#77782,#77783),
 .UNSPECIFIED.,.F.,.F.,(3,3),(0.,1.),.UNSPECIFIED.);
#23160=B_SPLINE_CURVE_WITH_KNOTS('',2,(#77791,#77792,#77793),
 .UNSPECIFIED.,.F.,.F.,(3,3),(0.,1.),.UNSPECIFIED.);
#23161=B_SPLINE_CURVE_WITH_KNOTS('',2,(#77796,#77797,#77798),
 .UNSPECIFIED.,.F.,.F.,(3,3),(0.,1.),.UNSPECIFIED.);
#23162=B_SPLINE_CURVE_WITH_KNOTS('',2,(#77805,#77806,#77807),
 .UNSPECIFIED.,.F.,.F.,(3,3),(0.,1.),.UNSPECIFIED.);
#23163=B_SPLINE_CURVE_WITH_KNOTS('',2,(#77808,#77809,#77810),
 .UNSPECIFIED.,.F.,.F.,(3,3),(0.,1.),.UNSPECIFIED.);
#23164=B_SPLINE_CURVE_WITH_KNOTS('',2,(#77819,#77820,#77821),
 .UNSPECIFIED.,.F.,.F.,(3,3),(0.,1.),.UNSPECIFIED.);
#23165=B_SPLINE_CURVE_WITH_KNOTS('',2,(#77825,#77826,#77827),
 .UNSPECIFIED.,.F.,.F.,(3,3),(0.,1.),.UNSPECIFIED.);
#23166=B_SPLINE_CURVE_WITH_KNOTS('',2,(#77836,#77837,#77838),
 .UNSPECIFIED.,.F.,.F.,(3,3),(0.,1.),.UNSPECIFIED.);
#23167=B_SPLINE_CURVE_WITH_KNOTS('',2,(#77841,#77842,#77843),
 .UNSPECIFIED.,.F.,.F.,(3,3),(0.,1.),.UNSPECIFIED.);
#23168=B_SPLINE_CURVE_WITH_KNOTS('',2,(#77851,#77852,#77853),
 .UNSPECIFIED.,.F.,.F.,(3,3),(0.,1.),.UNSPECIFIED.);
#23169=B_SPLINE_CURVE_WITH_KNOTS('',2,(#77856,#77857,#77858),
 .UNSPECIFIED.,.F.,.F.,(3,3),(0.,1.),.UNSPECIFIED.);
#23170=B_SPLINE_CURVE_WITH_KNOTS('',2,(#77866,#77867,#77868),
 .UNSPECIFIED.,.F.,.F.,(3,3),(0.,1.),.UNSPECIFIED.);
#23171=B_SPLINE_CURVE_WITH_KNOTS('',2,(#77871,#77872,#77873),
 .UNSPECIFIED.,.F.,.F.,(3,3),(0.,1.),.UNSPECIFIED.);
#23172=B_SPLINE_CURVE_WITH_KNOTS('',2,(#77881,#77882,#77883),
 .UNSPECIFIED.,.F.,.F.,(3,3),(0.,1.),.UNSPECIFIED.);
#23173=B_SPLINE_CURVE_WITH_KNOTS('',2,(#77886,#77887,#77888),
 .UNSPECIFIED.,.F.,.F.,(3,3),(0.,1.),.UNSPECIFIED.);
#23174=B_SPLINE_CURVE_WITH_KNOTS('',2,(#77896,#77897,#77898),
 .UNSPECIFIED.,.F.,.F.,(3,3),(0.,1.),.UNSPECIFIED.);
#23175=B_SPLINE_CURVE_WITH_KNOTS('',2,(#77901,#77902,#77903),
 .UNSPECIFIED.,.F.,.F.,(3,3),(0.,1.),.UNSPECIFIED.);
#23176=B_SPLINE_CURVE_WITH_KNOTS('',2,(#77911,#77912,#77913),
 .UNSPECIFIED.,.F.,.F.,(3,3),(0.,1.),.UNSPECIFIED.);
#23177=B_SPLINE_CURVE_WITH_KNOTS('',2,(#77916,#77917,#77918),
 .UNSPECIFIED.,.F.,.F.,(3,3),(0.,1.),.UNSPECIFIED.);
#23178=B_SPLINE_CURVE_WITH_KNOTS('',2,(#77926,#77927,#77928),
 .UNSPECIFIED.,.F.,.F.,(3,3),(0.,1.),.UNSPECIFIED.);
#23179=B_SPLINE_CURVE_WITH_KNOTS('',2,(#77931,#77932,#77933),
 .UNSPECIFIED.,.F.,.F.,(3,3),(0.,1.),.UNSPECIFIED.);
#23180=B_SPLINE_CURVE_WITH_KNOTS('',2,(#77941,#77942,#77943),
 .UNSPECIFIED.,.F.,.F.,(3,3),(0.,1.),.UNSPECIFIED.);
#23181=B_SPLINE_CURVE_WITH_KNOTS('',2,(#77946,#77947,#77948),
 .UNSPECIFIED.,.F.,.F.,(3,3),(0.,1.),.UNSPECIFIED.);
#23182=B_SPLINE_CURVE_WITH_KNOTS('',2,(#77956,#77957,#77958),
 .UNSPECIFIED.,.F.,.F.,(3,3),(0.,1.),.UNSPECIFIED.);
#23183=B_SPLINE_CURVE_WITH_KNOTS('',2,(#77961,#77962,#77963),
 .UNSPECIFIED.,.F.,.F.,(3,3),(0.,1.),.UNSPECIFIED.);
#23184=B_SPLINE_CURVE_WITH_KNOTS('',2,(#77971,#77972,#77973),
 .UNSPECIFIED.,.F.,.F.,(3,3),(0.,1.),.UNSPECIFIED.);
#23185=B_SPLINE_CURVE_WITH_KNOTS('',2,(#77976,#77977,#77978),
 .UNSPECIFIED.,.F.,.F.,(3,3),(0.,1.),.UNSPECIFIED.);
#23186=B_SPLINE_CURVE_WITH_KNOTS('',2,(#77985,#77986,#77987),
 .UNSPECIFIED.,.F.,.F.,(3,3),(0.,1.),.UNSPECIFIED.);
#23187=B_SPLINE_CURVE_WITH_KNOTS('',2,(#77988,#77989,#77990),
 .UNSPECIFIED.,.F.,.F.,(3,3),(0.,1.),.UNSPECIFIED.);
#23188=B_SPLINE_CURVE_WITH_KNOTS('',2,(#78000,#78001,#78002),
 .UNSPECIFIED.,.F.,.F.,(3,3),(0.,1.),.UNSPECIFIED.);
#23189=B_SPLINE_CURVE_WITH_KNOTS('',2,(#78006,#78007,#78008),
 .UNSPECIFIED.,.F.,.F.,(3,3),(0.,1.),.UNSPECIFIED.);
#23190=B_SPLINE_CURVE_WITH_KNOTS('',2,(#78017,#78018,#78019),
 .UNSPECIFIED.,.F.,.F.,(3,3),(0.,1.),.UNSPECIFIED.);
#23191=B_SPLINE_CURVE_WITH_KNOTS('',2,(#78022,#78023,#78024),
 .UNSPECIFIED.,.F.,.F.,(3,3),(0.,1.),.UNSPECIFIED.);
#23192=B_SPLINE_CURVE_WITH_KNOTS('',2,(#78032,#78033,#78034),
 .UNSPECIFIED.,.F.,.F.,(3,3),(0.,1.),.UNSPECIFIED.);
#23193=B_SPLINE_CURVE_WITH_KNOTS('',2,(#78037,#78038,#78039),
 .UNSPECIFIED.,.F.,.F.,(3,3),(0.,1.),.UNSPECIFIED.);
#23194=B_SPLINE_CURVE_WITH_KNOTS('',2,(#78053,#78054,#78055),
 .UNSPECIFIED.,.F.,.F.,(3,3),(0.,1.),.UNSPECIFIED.);
#23195=B_SPLINE_CURVE_WITH_KNOTS('',2,(#78058,#78059,#78060),
 .UNSPECIFIED.,.F.,.F.,(3,3),(0.,1.),.UNSPECIFIED.);
#23196=B_SPLINE_CURVE_WITH_KNOTS('',2,(#78068,#78069,#78070),
 .UNSPECIFIED.,.F.,.F.,(3,3),(0.,1.),.UNSPECIFIED.);
#23197=B_SPLINE_CURVE_WITH_KNOTS('',2,(#78073,#78074,#78075),
 .UNSPECIFIED.,.F.,.F.,(3,3),(0.,1.),.UNSPECIFIED.);
#23198=B_SPLINE_CURVE_WITH_KNOTS('',2,(#78083,#78084,#78085),
 .UNSPECIFIED.,.F.,.F.,(3,3),(0.,1.),.UNSPECIFIED.);
#23199=B_SPLINE_CURVE_WITH_KNOTS('',2,(#78088,#78089,#78090),
 .UNSPECIFIED.,.F.,.F.,(3,3),(0.,1.),.UNSPECIFIED.);
#23200=B_SPLINE_CURVE_WITH_KNOTS('',2,(#78122,#78123,#78124),
 .UNSPECIFIED.,.F.,.F.,(3,3),(0.,1.),.UNSPECIFIED.);
#23201=B_SPLINE_CURVE_WITH_KNOTS('',2,(#78128,#78129,#78130),
 .UNSPECIFIED.,.F.,.F.,(3,3),(0.,1.),.UNSPECIFIED.);
#23202=B_SPLINE_CURVE_WITH_KNOTS('',2,(#78139,#78140,#78141),
 .UNSPECIFIED.,.F.,.F.,(3,3),(0.,1.),.UNSPECIFIED.);
#23203=B_SPLINE_CURVE_WITH_KNOTS('',2,(#78144,#78145,#78146),
 .UNSPECIFIED.,.F.,.F.,(3,3),(0.,1.),.UNSPECIFIED.);
#23204=B_SPLINE_CURVE_WITH_KNOTS('',2,(#78154,#78155,#78156),
 .UNSPECIFIED.,.F.,.F.,(3,3),(0.,1.),.UNSPECIFIED.);
#23205=B_SPLINE_CURVE_WITH_KNOTS('',2,(#78159,#78160,#78161),
 .UNSPECIFIED.,.F.,.F.,(3,3),(0.,1.),.UNSPECIFIED.);
#23206=B_SPLINE_CURVE_WITH_KNOTS('',2,(#78169,#78170,#78171),
 .UNSPECIFIED.,.F.,.F.,(3,3),(0.,1.),.UNSPECIFIED.);
#23207=B_SPLINE_CURVE_WITH_KNOTS('',2,(#78174,#78175,#78176),
 .UNSPECIFIED.,.F.,.F.,(3,3),(0.,1.),.UNSPECIFIED.);
#23208=B_SPLINE_CURVE_WITH_KNOTS('',2,(#78184,#78185,#78186),
 .UNSPECIFIED.,.F.,.F.,(3,3),(0.,1.),.UNSPECIFIED.);
#23209=B_SPLINE_CURVE_WITH_KNOTS('',2,(#78189,#78190,#78191),
 .UNSPECIFIED.,.F.,.F.,(3,3),(0.,1.),.UNSPECIFIED.);
#23210=B_SPLINE_CURVE_WITH_KNOTS('',2,(#78199,#78200,#78201),
 .UNSPECIFIED.,.F.,.F.,(3,3),(0.,1.),.UNSPECIFIED.);
#23211=B_SPLINE_CURVE_WITH_KNOTS('',2,(#78204,#78205,#78206),
 .UNSPECIFIED.,.F.,.F.,(3,3),(0.,1.),.UNSPECIFIED.);
#23212=B_SPLINE_CURVE_WITH_KNOTS('',2,(#78214,#78215,#78216),
 .UNSPECIFIED.,.F.,.F.,(3,3),(0.,1.),.UNSPECIFIED.);
#23213=B_SPLINE_CURVE_WITH_KNOTS('',2,(#78219,#78220,#78221),
 .UNSPECIFIED.,.F.,.F.,(3,3),(0.,1.),.UNSPECIFIED.);
#23214=B_SPLINE_CURVE_WITH_KNOTS('',2,(#78228,#78229,#78230),
 .UNSPECIFIED.,.F.,.F.,(3,3),(0.,1.),.UNSPECIFIED.);
#23215=B_SPLINE_CURVE_WITH_KNOTS('',2,(#78231,#78232,#78233),
 .UNSPECIFIED.,.F.,.F.,(3,3),(0.,1.),.UNSPECIFIED.);
#23216=B_SPLINE_CURVE_WITH_KNOTS('',2,(#78242,#78243,#78244),
 .UNSPECIFIED.,.F.,.F.,(3,3),(0.,1.),.UNSPECIFIED.);
#23217=B_SPLINE_CURVE_WITH_KNOTS('',2,(#78248,#78249,#78250),
 .UNSPECIFIED.,.F.,.F.,(3,3),(0.,1.),.UNSPECIFIED.);
#23218=B_SPLINE_CURVE_WITH_KNOTS('',2,(#78259,#78260,#78261),
 .UNSPECIFIED.,.F.,.F.,(3,3),(0.,1.),.UNSPECIFIED.);
#23219=B_SPLINE_CURVE_WITH_KNOTS('',2,(#78264,#78265,#78266),
 .UNSPECIFIED.,.F.,.F.,(3,3),(0.,1.),.UNSPECIFIED.);
#23220=B_SPLINE_CURVE_WITH_KNOTS('',2,(#78274,#78275,#78276),
 .UNSPECIFIED.,.F.,.F.,(3,3),(0.,1.),.UNSPECIFIED.);
#23221=B_SPLINE_CURVE_WITH_KNOTS('',2,(#78279,#78280,#78281),
 .UNSPECIFIED.,.F.,.F.,(3,3),(0.,1.),.UNSPECIFIED.);
#23222=B_SPLINE_CURVE_WITH_KNOTS('',2,(#78289,#78290,#78291),
 .UNSPECIFIED.,.F.,.F.,(3,3),(0.,1.),.UNSPECIFIED.);
#23223=B_SPLINE_CURVE_WITH_KNOTS('',2,(#78294,#78295,#78296),
 .UNSPECIFIED.,.F.,.F.,(3,3),(0.,1.),.UNSPECIFIED.);
#23224=B_SPLINE_CURVE_WITH_KNOTS('',2,(#78304,#78305,#78306),
 .UNSPECIFIED.,.F.,.F.,(3,3),(0.,1.),.UNSPECIFIED.);
#23225=B_SPLINE_CURVE_WITH_KNOTS('',2,(#78309,#78310,#78311),
 .UNSPECIFIED.,.F.,.F.,(3,3),(0.,1.),.UNSPECIFIED.);
#23226=B_SPLINE_CURVE_WITH_KNOTS('',2,(#78319,#78320,#78321),
 .UNSPECIFIED.,.F.,.F.,(3,3),(0.,1.),.UNSPECIFIED.);
#23227=B_SPLINE_CURVE_WITH_KNOTS('',2,(#78324,#78325,#78326),
 .UNSPECIFIED.,.F.,.F.,(3,3),(0.,1.),.UNSPECIFIED.);
#23228=B_SPLINE_CURVE_WITH_KNOTS('',2,(#78334,#78335,#78336),
 .UNSPECIFIED.,.F.,.F.,(3,3),(0.,1.),.UNSPECIFIED.);
#23229=B_SPLINE_CURVE_WITH_KNOTS('',2,(#78339,#78340,#78341),
 .UNSPECIFIED.,.F.,.F.,(3,3),(0.,1.),.UNSPECIFIED.);
#23230=B_SPLINE_CURVE_WITH_KNOTS('',2,(#78349,#78350,#78351),
 .UNSPECIFIED.,.F.,.F.,(3,3),(0.,1.),.UNSPECIFIED.);
#23231=B_SPLINE_CURVE_WITH_KNOTS('',2,(#78354,#78355,#78356),
 .UNSPECIFIED.,.F.,.F.,(3,3),(0.,1.),.UNSPECIFIED.);
#23232=B_SPLINE_CURVE_WITH_KNOTS('',2,(#78364,#78365,#78366),
 .UNSPECIFIED.,.F.,.F.,(3,3),(0.,1.),.UNSPECIFIED.);
#23233=B_SPLINE_CURVE_WITH_KNOTS('',2,(#78369,#78370,#78371),
 .UNSPECIFIED.,.F.,.F.,(3,3),(0.,1.),.UNSPECIFIED.);
#23234=B_SPLINE_CURVE_WITH_KNOTS('',2,(#78379,#78380,#78381),
 .UNSPECIFIED.,.F.,.F.,(3,3),(0.,1.),.UNSPECIFIED.);
#23235=B_SPLINE_CURVE_WITH_KNOTS('',2,(#78384,#78385,#78386),
 .UNSPECIFIED.,.F.,.F.,(3,3),(0.,1.),.UNSPECIFIED.);
#23236=B_SPLINE_CURVE_WITH_KNOTS('',2,(#78394,#78395,#78396),
 .UNSPECIFIED.,.F.,.F.,(3,3),(0.,1.),.UNSPECIFIED.);
#23237=B_SPLINE_CURVE_WITH_KNOTS('',2,(#78399,#78400,#78401),
 .UNSPECIFIED.,.F.,.F.,(3,3),(0.,1.),.UNSPECIFIED.);
#23238=B_SPLINE_CURVE_WITH_KNOTS('',2,(#78408,#78409,#78410),
 .UNSPECIFIED.,.F.,.F.,(3,3),(0.,1.),.UNSPECIFIED.);
#23239=B_SPLINE_CURVE_WITH_KNOTS('',2,(#78411,#78412,#78413),
 .UNSPECIFIED.,.F.,.F.,(3,3),(0.,1.),.UNSPECIFIED.);
#23240=B_SPLINE_CURVE_WITH_KNOTS('',2,(#78423,#78424,#78425),
 .UNSPECIFIED.,.F.,.F.,(3,3),(0.,1.),.UNSPECIFIED.);
#23241=B_SPLINE_CURVE_WITH_KNOTS('',2,(#78429,#78430,#78431),
 .UNSPECIFIED.,.F.,.F.,(3,3),(0.,1.),.UNSPECIFIED.);
#23242=B_SPLINE_CURVE_WITH_KNOTS('',2,(#78440,#78441,#78442),
 .UNSPECIFIED.,.F.,.F.,(3,3),(0.,1.),.UNSPECIFIED.);
#23243=B_SPLINE_CURVE_WITH_KNOTS('',2,(#78445,#78446,#78447),
 .UNSPECIFIED.,.F.,.F.,(3,3),(0.,1.),.UNSPECIFIED.);
#23244=B_SPLINE_CURVE_WITH_KNOTS('',2,(#78455,#78456,#78457),
 .UNSPECIFIED.,.F.,.F.,(3,3),(0.,1.),.UNSPECIFIED.);
#23245=B_SPLINE_CURVE_WITH_KNOTS('',2,(#78460,#78461,#78462),
 .UNSPECIFIED.,.F.,.F.,(3,3),(0.,1.),.UNSPECIFIED.);
#23246=B_SPLINE_CURVE_WITH_KNOTS('',2,(#78470,#78471,#78472),
 .UNSPECIFIED.,.F.,.F.,(3,3),(0.,1.),.UNSPECIFIED.);
#23247=B_SPLINE_CURVE_WITH_KNOTS('',2,(#78475,#78476,#78477),
 .UNSPECIFIED.,.F.,.F.,(3,3),(0.,1.),.UNSPECIFIED.);
#23248=B_SPLINE_CURVE_WITH_KNOTS('',2,(#78485,#78486,#78487),
 .UNSPECIFIED.,.F.,.F.,(3,3),(0.,1.),.UNSPECIFIED.);
#23249=B_SPLINE_CURVE_WITH_KNOTS('',2,(#78490,#78491,#78492),
 .UNSPECIFIED.,.F.,.F.,(3,3),(0.,1.),.UNSPECIFIED.);
#23250=B_SPLINE_CURVE_WITH_KNOTS('',2,(#78500,#78501,#78502),
 .UNSPECIFIED.,.F.,.F.,(3,3),(0.,1.),.UNSPECIFIED.);
#23251=B_SPLINE_CURVE_WITH_KNOTS('',2,(#78505,#78506,#78507),
 .UNSPECIFIED.,.F.,.F.,(3,3),(0.,1.),.UNSPECIFIED.);
#23252=B_SPLINE_CURVE_WITH_KNOTS('',2,(#78515,#78516,#78517),
 .UNSPECIFIED.,.F.,.F.,(3,3),(0.,1.),.UNSPECIFIED.);
#23253=B_SPLINE_CURVE_WITH_KNOTS('',2,(#78520,#78521,#78522),
 .UNSPECIFIED.,.F.,.F.,(3,3),(0.,1.),.UNSPECIFIED.);
#23254=B_SPLINE_CURVE_WITH_KNOTS('',2,(#78530,#78531,#78532),
 .UNSPECIFIED.,.F.,.F.,(3,3),(0.,1.),.UNSPECIFIED.);
#23255=B_SPLINE_CURVE_WITH_KNOTS('',2,(#78535,#78536,#78537),
 .UNSPECIFIED.,.F.,.F.,(3,3),(0.,1.),.UNSPECIFIED.);
#23256=B_SPLINE_CURVE_WITH_KNOTS('',2,(#78544,#78545,#78546),
 .UNSPECIFIED.,.F.,.F.,(3,3),(0.,1.),.UNSPECIFIED.);
#23257=B_SPLINE_CURVE_WITH_KNOTS('',2,(#78547,#78548,#78549),
 .UNSPECIFIED.,.F.,.F.,(3,3),(0.,1.),.UNSPECIFIED.);
#23258=B_SPLINE_CURVE_WITH_KNOTS('',2,(#78558,#78559,#78560),
 .UNSPECIFIED.,.F.,.F.,(3,3),(0.,1.),.UNSPECIFIED.);
#23259=B_SPLINE_CURVE_WITH_KNOTS('',2,(#78564,#78565,#78566),
 .UNSPECIFIED.,.F.,.F.,(3,3),(0.,1.),.UNSPECIFIED.);
#23260=B_SPLINE_CURVE_WITH_KNOTS('',2,(#78575,#78576,#78577),
 .UNSPECIFIED.,.F.,.F.,(3,3),(0.,1.),.UNSPECIFIED.);
#23261=B_SPLINE_CURVE_WITH_KNOTS('',2,(#78580,#78581,#78582),
 .UNSPECIFIED.,.F.,.F.,(3,3),(0.,1.),.UNSPECIFIED.);
#23262=B_SPLINE_CURVE_WITH_KNOTS('',2,(#78590,#78591,#78592),
 .UNSPECIFIED.,.F.,.F.,(3,3),(0.,1.),.UNSPECIFIED.);
#23263=B_SPLINE_CURVE_WITH_KNOTS('',2,(#78595,#78596,#78597),
 .UNSPECIFIED.,.F.,.F.,(3,3),(0.,1.),.UNSPECIFIED.);
#23264=B_SPLINE_CURVE_WITH_KNOTS('',2,(#78605,#78606,#78607),
 .UNSPECIFIED.,.F.,.F.,(3,3),(0.,1.),.UNSPECIFIED.);
#23265=B_SPLINE_CURVE_WITH_KNOTS('',2,(#78610,#78611,#78612),
 .UNSPECIFIED.,.F.,.F.,(3,3),(0.,1.),.UNSPECIFIED.);
#23266=B_SPLINE_CURVE_WITH_KNOTS('',2,(#78620,#78621,#78622),
 .UNSPECIFIED.,.F.,.F.,(3,3),(0.,1.),.UNSPECIFIED.);
#23267=B_SPLINE_CURVE_WITH_KNOTS('',2,(#78625,#78626,#78627),
 .UNSPECIFIED.,.F.,.F.,(3,3),(0.,1.),.UNSPECIFIED.);
#23268=B_SPLINE_CURVE_WITH_KNOTS('',2,(#78635,#78636,#78637),
 .UNSPECIFIED.,.F.,.F.,(3,3),(0.,1.),.UNSPECIFIED.);
#23269=B_SPLINE_CURVE_WITH_KNOTS('',2,(#78640,#78641,#78642),
 .UNSPECIFIED.,.F.,.F.,(3,3),(0.,1.),.UNSPECIFIED.);
#23270=B_SPLINE_CURVE_WITH_KNOTS('',2,(#78650,#78651,#78652),
 .UNSPECIFIED.,.F.,.F.,(3,3),(0.,1.),.UNSPECIFIED.);
#23271=B_SPLINE_CURVE_WITH_KNOTS('',2,(#78655,#78656,#78657),
 .UNSPECIFIED.,.F.,.F.,(3,3),(0.,1.),.UNSPECIFIED.);
#23272=B_SPLINE_CURVE_WITH_KNOTS('',2,(#78665,#78666,#78667),
 .UNSPECIFIED.,.F.,.F.,(3,3),(0.,1.),.UNSPECIFIED.);
#23273=B_SPLINE_CURVE_WITH_KNOTS('',2,(#78670,#78671,#78672),
 .UNSPECIFIED.,.F.,.F.,(3,3),(0.,1.),.UNSPECIFIED.);
#23274=B_SPLINE_CURVE_WITH_KNOTS('',2,(#78680,#78681,#78682),
 .UNSPECIFIED.,.F.,.F.,(3,3),(0.,1.),.UNSPECIFIED.);
#23275=B_SPLINE_CURVE_WITH_KNOTS('',2,(#78685,#78686,#78687),
 .UNSPECIFIED.,.F.,.F.,(3,3),(0.,1.),.UNSPECIFIED.);
#23276=B_SPLINE_CURVE_WITH_KNOTS('',2,(#78695,#78696,#78697),
 .UNSPECIFIED.,.F.,.F.,(3,3),(0.,1.),.UNSPECIFIED.);
#23277=B_SPLINE_CURVE_WITH_KNOTS('',2,(#78700,#78701,#78702),
 .UNSPECIFIED.,.F.,.F.,(3,3),(0.,1.),.UNSPECIFIED.);
#23278=B_SPLINE_CURVE_WITH_KNOTS('',2,(#78710,#78711,#78712),
 .UNSPECIFIED.,.F.,.F.,(3,3),(0.,1.),.UNSPECIFIED.);
#23279=B_SPLINE_CURVE_WITH_KNOTS('',2,(#78715,#78716,#78717),
 .UNSPECIFIED.,.F.,.F.,(3,3),(0.,1.),.UNSPECIFIED.);
#23280=B_SPLINE_CURVE_WITH_KNOTS('',2,(#78725,#78726,#78727),
 .UNSPECIFIED.,.F.,.F.,(3,3),(0.,1.),.UNSPECIFIED.);
#23281=B_SPLINE_CURVE_WITH_KNOTS('',2,(#78730,#78731,#78732),
 .UNSPECIFIED.,.F.,.F.,(3,3),(0.,1.),.UNSPECIFIED.);
#23282=B_SPLINE_CURVE_WITH_KNOTS('',2,(#78740,#78741,#78742),
 .UNSPECIFIED.,.F.,.F.,(3,3),(0.,1.),.UNSPECIFIED.);
#23283=B_SPLINE_CURVE_WITH_KNOTS('',2,(#78745,#78746,#78747),
 .UNSPECIFIED.,.F.,.F.,(3,3),(0.,1.),.UNSPECIFIED.);
#23284=B_SPLINE_CURVE_WITH_KNOTS('',2,(#78755,#78756,#78757),
 .UNSPECIFIED.,.F.,.F.,(3,3),(0.,1.),.UNSPECIFIED.);
#23285=B_SPLINE_CURVE_WITH_KNOTS('',2,(#78760,#78761,#78762),
 .UNSPECIFIED.,.F.,.F.,(3,3),(0.,1.),.UNSPECIFIED.);
#23286=B_SPLINE_CURVE_WITH_KNOTS('',2,(#78770,#78771,#78772),
 .UNSPECIFIED.,.F.,.F.,(3,3),(0.,1.),.UNSPECIFIED.);
#23287=B_SPLINE_CURVE_WITH_KNOTS('',2,(#78775,#78776,#78777),
 .UNSPECIFIED.,.F.,.F.,(3,3),(0.,1.),.UNSPECIFIED.);
#23288=B_SPLINE_CURVE_WITH_KNOTS('',2,(#78785,#78786,#78787),
 .UNSPECIFIED.,.F.,.F.,(3,3),(0.,1.),.UNSPECIFIED.);
#23289=B_SPLINE_CURVE_WITH_KNOTS('',2,(#78790,#78791,#78792),
 .UNSPECIFIED.,.F.,.F.,(3,3),(0.,1.),.UNSPECIFIED.);
#23290=B_SPLINE_CURVE_WITH_KNOTS('',2,(#78800,#78801,#78802),
 .UNSPECIFIED.,.F.,.F.,(3,3),(0.,1.),.UNSPECIFIED.);
#23291=B_SPLINE_CURVE_WITH_KNOTS('',2,(#78805,#78806,#78807),
 .UNSPECIFIED.,.F.,.F.,(3,3),(0.,1.),.UNSPECIFIED.);
#23292=B_SPLINE_CURVE_WITH_KNOTS('',2,(#78820,#78821,#78822),
 .UNSPECIFIED.,.F.,.F.,(3,3),(0.,1.),.UNSPECIFIED.);
#23293=B_SPLINE_CURVE_WITH_KNOTS('',2,(#78823,#78824,#78825),
 .UNSPECIFIED.,.F.,.F.,(3,3),(0.,1.),.UNSPECIFIED.);
#23294=B_SPLINE_CURVE_WITH_KNOTS('',2,(#78837,#78838,#78839),
 .UNSPECIFIED.,.F.,.F.,(3,3),(0.,1.),.UNSPECIFIED.);
#23295=B_SPLINE_CURVE_WITH_KNOTS('',2,(#78843,#78844,#78845),
 .UNSPECIFIED.,.F.,.F.,(3,3),(0.,1.),.UNSPECIFIED.);
#23296=B_SPLINE_CURVE_WITH_KNOTS('',2,(#78854,#78855,#78856),
 .UNSPECIFIED.,.F.,.F.,(3,3),(0.,1.),.UNSPECIFIED.);
#23297=B_SPLINE_CURVE_WITH_KNOTS('',2,(#78859,#78860,#78861),
 .UNSPECIFIED.,.F.,.F.,(3,3),(0.,1.),.UNSPECIFIED.);
#23298=B_SPLINE_CURVE_WITH_KNOTS('',2,(#78869,#78870,#78871),
 .UNSPECIFIED.,.F.,.F.,(3,3),(0.,1.),.UNSPECIFIED.);
#23299=B_SPLINE_CURVE_WITH_KNOTS('',2,(#78874,#78875,#78876),
 .UNSPECIFIED.,.F.,.F.,(3,3),(0.,1.),.UNSPECIFIED.);
#23300=B_SPLINE_CURVE_WITH_KNOTS('',2,(#78884,#78885,#78886),
 .UNSPECIFIED.,.F.,.F.,(3,3),(0.,1.),.UNSPECIFIED.);
#23301=B_SPLINE_CURVE_WITH_KNOTS('',2,(#78889,#78890,#78891),
 .UNSPECIFIED.,.F.,.F.,(3,3),(0.,1.),.UNSPECIFIED.);
#23302=B_SPLINE_CURVE_WITH_KNOTS('',2,(#78899,#78900,#78901),
 .UNSPECIFIED.,.F.,.F.,(3,3),(0.,1.),.UNSPECIFIED.);
#23303=B_SPLINE_CURVE_WITH_KNOTS('',2,(#78904,#78905,#78906),
 .UNSPECIFIED.,.F.,.F.,(3,3),(0.,1.),.UNSPECIFIED.);
#23304=B_SPLINE_CURVE_WITH_KNOTS('',2,(#78914,#78915,#78916),
 .UNSPECIFIED.,.F.,.F.,(3,3),(0.,1.),.UNSPECIFIED.);
#23305=B_SPLINE_CURVE_WITH_KNOTS('',2,(#78919,#78920,#78921),
 .UNSPECIFIED.,.F.,.F.,(3,3),(0.,1.),.UNSPECIFIED.);
#23306=B_SPLINE_CURVE_WITH_KNOTS('',2,(#78929,#78930,#78931),
 .UNSPECIFIED.,.F.,.F.,(3,3),(0.,1.),.UNSPECIFIED.);
#23307=B_SPLINE_CURVE_WITH_KNOTS('',2,(#78934,#78935,#78936),
 .UNSPECIFIED.,.F.,.F.,(3,3),(0.,1.),.UNSPECIFIED.);
#23308=B_SPLINE_CURVE_WITH_KNOTS('',2,(#78943,#78944,#78945),
 .UNSPECIFIED.,.F.,.F.,(3,3),(0.,1.),.UNSPECIFIED.);
#23309=B_SPLINE_CURVE_WITH_KNOTS('',2,(#78946,#78947,#78948),
 .UNSPECIFIED.,.F.,.F.,(3,3),(0.,1.),.UNSPECIFIED.);
#23310=B_SPLINE_CURVE_WITH_KNOTS('',2,(#78957,#78958,#78959),
 .UNSPECIFIED.,.F.,.F.,(3,3),(0.,1.),.UNSPECIFIED.);
#23311=B_SPLINE_CURVE_WITH_KNOTS('',2,(#78963,#78964,#78965),
 .UNSPECIFIED.,.F.,.F.,(3,3),(0.,1.),.UNSPECIFIED.);
#23312=B_SPLINE_CURVE_WITH_KNOTS('',2,(#78974,#78975,#78976),
 .UNSPECIFIED.,.F.,.F.,(3,3),(0.,1.),.UNSPECIFIED.);
#23313=B_SPLINE_CURVE_WITH_KNOTS('',2,(#78979,#78980,#78981),
 .UNSPECIFIED.,.F.,.F.,(3,3),(0.,1.),.UNSPECIFIED.);
#23314=B_SPLINE_CURVE_WITH_KNOTS('',2,(#78989,#78990,#78991),
 .UNSPECIFIED.,.F.,.F.,(3,3),(0.,1.),.UNSPECIFIED.);
#23315=B_SPLINE_CURVE_WITH_KNOTS('',2,(#78994,#78995,#78996),
 .UNSPECIFIED.,.F.,.F.,(3,3),(0.,1.),.UNSPECIFIED.);
#23316=B_SPLINE_CURVE_WITH_KNOTS('',2,(#79004,#79005,#79006),
 .UNSPECIFIED.,.F.,.F.,(3,3),(0.,1.),.UNSPECIFIED.);
#23317=B_SPLINE_CURVE_WITH_KNOTS('',2,(#79009,#79010,#79011),
 .UNSPECIFIED.,.F.,.F.,(3,3),(0.,1.),.UNSPECIFIED.);
#23318=B_SPLINE_CURVE_WITH_KNOTS('',2,(#79019,#79020,#79021),
 .UNSPECIFIED.,.F.,.F.,(3,3),(0.,1.),.UNSPECIFIED.);
#23319=B_SPLINE_CURVE_WITH_KNOTS('',2,(#79024,#79025,#79026),
 .UNSPECIFIED.,.F.,.F.,(3,3),(0.,1.),.UNSPECIFIED.);
#23320=B_SPLINE_CURVE_WITH_KNOTS('',2,(#79034,#79035,#79036),
 .UNSPECIFIED.,.F.,.F.,(3,3),(0.,1.),.UNSPECIFIED.);
#23321=B_SPLINE_CURVE_WITH_KNOTS('',2,(#79039,#79040,#79041),
 .UNSPECIFIED.,.F.,.F.,(3,3),(0.,1.),.UNSPECIFIED.);
#23322=B_SPLINE_CURVE_WITH_KNOTS('',2,(#79049,#79050,#79051),
 .UNSPECIFIED.,.F.,.F.,(3,3),(0.,1.),.UNSPECIFIED.);
#23323=B_SPLINE_CURVE_WITH_KNOTS('',2,(#79054,#79055,#79056),
 .UNSPECIFIED.,.F.,.F.,(3,3),(0.,1.),.UNSPECIFIED.);
#23324=B_SPLINE_CURVE_WITH_KNOTS('',2,(#79064,#79065,#79066),
 .UNSPECIFIED.,.F.,.F.,(3,3),(0.,1.),.UNSPECIFIED.);
#23325=B_SPLINE_CURVE_WITH_KNOTS('',2,(#79069,#79070,#79071),
 .UNSPECIFIED.,.F.,.F.,(3,3),(0.,1.),.UNSPECIFIED.);
#23326=B_SPLINE_CURVE_WITH_KNOTS('',2,(#79079,#79080,#79081),
 .UNSPECIFIED.,.F.,.F.,(3,3),(0.,1.),.UNSPECIFIED.);
#23327=B_SPLINE_CURVE_WITH_KNOTS('',2,(#79084,#79085,#79086),
 .UNSPECIFIED.,.F.,.F.,(3,3),(0.,1.),.UNSPECIFIED.);
#23328=B_SPLINE_CURVE_WITH_KNOTS('',2,(#79094,#79095,#79096),
 .UNSPECIFIED.,.F.,.F.,(3,3),(0.,1.),.UNSPECIFIED.);
#23329=B_SPLINE_CURVE_WITH_KNOTS('',2,(#79099,#79100,#79101),
 .UNSPECIFIED.,.F.,.F.,(3,3),(0.,1.),.UNSPECIFIED.);
#23330=B_SPLINE_CURVE_WITH_KNOTS('',2,(#79109,#79110,#79111),
 .UNSPECIFIED.,.F.,.F.,(3,3),(0.,1.),.UNSPECIFIED.);
#23331=B_SPLINE_CURVE_WITH_KNOTS('',2,(#79114,#79115,#79116),
 .UNSPECIFIED.,.F.,.F.,(3,3),(0.,1.),.UNSPECIFIED.);
#23332=B_SPLINE_CURVE_WITH_KNOTS('',2,(#79123,#79124,#79125),
 .UNSPECIFIED.,.F.,.F.,(3,3),(0.,1.),.UNSPECIFIED.);
#23333=B_SPLINE_CURVE_WITH_KNOTS('',2,(#79126,#79127,#79128),
 .UNSPECIFIED.,.F.,.F.,(3,3),(0.,1.),.UNSPECIFIED.);
#23334=B_SPLINE_CURVE_WITH_KNOTS('',2,(#79138,#79139,#79140),
 .UNSPECIFIED.,.F.,.F.,(3,3),(0.,1.),.UNSPECIFIED.);
#23335=B_SPLINE_CURVE_WITH_KNOTS('',2,(#79144,#79145,#79146),
 .UNSPECIFIED.,.F.,.F.,(3,3),(0.,1.),.UNSPECIFIED.);
#23336=B_SPLINE_CURVE_WITH_KNOTS('',2,(#79155,#79156,#79157),
 .UNSPECIFIED.,.F.,.F.,(3,3),(0.,1.),.UNSPECIFIED.);
#23337=B_SPLINE_CURVE_WITH_KNOTS('',2,(#79160,#79161,#79162),
 .UNSPECIFIED.,.F.,.F.,(3,3),(0.,1.),.UNSPECIFIED.);
#23338=B_SPLINE_CURVE_WITH_KNOTS('',2,(#79170,#79171,#79172),
 .UNSPECIFIED.,.F.,.F.,(3,3),(0.,1.),.UNSPECIFIED.);
#23339=B_SPLINE_CURVE_WITH_KNOTS('',2,(#79175,#79176,#79177),
 .UNSPECIFIED.,.F.,.F.,(3,3),(0.,1.),.UNSPECIFIED.);
#23340=B_SPLINE_CURVE_WITH_KNOTS('',2,(#79185,#79186,#79187),
 .UNSPECIFIED.,.F.,.F.,(3,3),(0.,1.),.UNSPECIFIED.);
#23341=B_SPLINE_CURVE_WITH_KNOTS('',2,(#79190,#79191,#79192),
 .UNSPECIFIED.,.F.,.F.,(3,3),(0.,1.),.UNSPECIFIED.);
#23342=B_SPLINE_CURVE_WITH_KNOTS('',2,(#79200,#79201,#79202),
 .UNSPECIFIED.,.F.,.F.,(3,3),(0.,1.),.UNSPECIFIED.);
#23343=B_SPLINE_CURVE_WITH_KNOTS('',2,(#79205,#79206,#79207),
 .UNSPECIFIED.,.F.,.F.,(3,3),(0.,1.),.UNSPECIFIED.);
#23344=B_SPLINE_CURVE_WITH_KNOTS('',2,(#79215,#79216,#79217),
 .UNSPECIFIED.,.F.,.F.,(3,3),(0.,1.),.UNSPECIFIED.);
#23345=B_SPLINE_CURVE_WITH_KNOTS('',2,(#79220,#79221,#79222),
 .UNSPECIFIED.,.F.,.F.,(3,3),(0.,1.),.UNSPECIFIED.);
#23346=B_SPLINE_CURVE_WITH_KNOTS('',2,(#79266,#79267,#79268),
 .UNSPECIFIED.,.F.,.F.,(3,3),(0.,1.),.UNSPECIFIED.);
#23347=B_SPLINE_CURVE_WITH_KNOTS('',2,(#79271,#79272,#79273),
 .UNSPECIFIED.,.F.,.F.,(3,3),(0.,1.),.UNSPECIFIED.);
#23348=B_SPLINE_CURVE_WITH_KNOTS('',2,(#79281,#79282,#79283),
 .UNSPECIFIED.,.F.,.F.,(3,3),(0.,1.),.UNSPECIFIED.);
#23349=B_SPLINE_CURVE_WITH_KNOTS('',2,(#79286,#79287,#79288),
 .UNSPECIFIED.,.F.,.F.,(3,3),(0.,1.),.UNSPECIFIED.);
#23350=B_SPLINE_CURVE_WITH_KNOTS('',2,(#79296,#79297,#79298),
 .UNSPECIFIED.,.F.,.F.,(3,3),(0.,1.),.UNSPECIFIED.);
#23351=B_SPLINE_CURVE_WITH_KNOTS('',2,(#79301,#79302,#79303),
 .UNSPECIFIED.,.F.,.F.,(3,3),(0.,1.),.UNSPECIFIED.);
#23352=B_SPLINE_CURVE_WITH_KNOTS('',2,(#79311,#79312,#79313),
 .UNSPECIFIED.,.F.,.F.,(3,3),(0.,1.),.UNSPECIFIED.);
#23353=B_SPLINE_CURVE_WITH_KNOTS('',2,(#79316,#79317,#79318),
 .UNSPECIFIED.,.F.,.F.,(3,3),(0.,1.),.UNSPECIFIED.);
#23354=B_SPLINE_CURVE_WITH_KNOTS('',2,(#79326,#79327,#79328),
 .UNSPECIFIED.,.F.,.F.,(3,3),(0.,1.),.UNSPECIFIED.);
#23355=B_SPLINE_CURVE_WITH_KNOTS('',2,(#79331,#79332,#79333),
 .UNSPECIFIED.,.F.,.F.,(3,3),(0.,1.),.UNSPECIFIED.);
#23356=B_SPLINE_CURVE_WITH_KNOTS('',2,(#79341,#79342,#79343),
 .UNSPECIFIED.,.F.,.F.,(3,3),(0.,1.),.UNSPECIFIED.);
#23357=B_SPLINE_CURVE_WITH_KNOTS('',2,(#79346,#79347,#79348),
 .UNSPECIFIED.,.F.,.F.,(3,3),(0.,1.),.UNSPECIFIED.);
#23358=B_SPLINE_CURVE_WITH_KNOTS('',2,(#79356,#79357,#79358),
 .UNSPECIFIED.,.F.,.F.,(3,3),(0.,1.),.UNSPECIFIED.);
#23359=B_SPLINE_CURVE_WITH_KNOTS('',2,(#79361,#79362,#79363),
 .UNSPECIFIED.,.F.,.F.,(3,3),(0.,1.),.UNSPECIFIED.);
#23360=B_SPLINE_CURVE_WITH_KNOTS('',2,(#79371,#79372,#79373),
 .UNSPECIFIED.,.F.,.F.,(3,3),(0.,1.),.UNSPECIFIED.);
#23361=B_SPLINE_CURVE_WITH_KNOTS('',2,(#79376,#79377,#79378),
 .UNSPECIFIED.,.F.,.F.,(3,3),(0.,1.),.UNSPECIFIED.);
#23362=B_SPLINE_CURVE_WITH_KNOTS('',2,(#79391,#79392,#79393),
 .UNSPECIFIED.,.F.,.F.,(3,3),(0.,1.),.UNSPECIFIED.);
#23363=B_SPLINE_CURVE_WITH_KNOTS('',2,(#79394,#79395,#79396),
 .UNSPECIFIED.,.F.,.F.,(3,3),(0.,1.),.UNSPECIFIED.);
#23364=B_SPLINE_CURVE_WITH_KNOTS('',2,(#79407,#79408,#79409),
 .UNSPECIFIED.,.F.,.F.,(3,3),(0.,1.),.UNSPECIFIED.);
#23365=B_SPLINE_CURVE_WITH_KNOTS('',2,(#79413,#79414,#79415),
 .UNSPECIFIED.,.F.,.F.,(3,3),(0.,1.),.UNSPECIFIED.);
#23366=B_SPLINE_CURVE_WITH_KNOTS('',2,(#79424,#79425,#79426),
 .UNSPECIFIED.,.F.,.F.,(3,3),(0.,1.),.UNSPECIFIED.);
#23367=B_SPLINE_CURVE_WITH_KNOTS('',2,(#79429,#79430,#79431),
 .UNSPECIFIED.,.F.,.F.,(3,3),(0.,1.),.UNSPECIFIED.);
#23368=B_SPLINE_CURVE_WITH_KNOTS('',2,(#79439,#79440,#79441),
 .UNSPECIFIED.,.F.,.F.,(3,3),(0.,1.),.UNSPECIFIED.);
#23369=B_SPLINE_CURVE_WITH_KNOTS('',2,(#79444,#79445,#79446),
 .UNSPECIFIED.,.F.,.F.,(3,3),(0.,1.),.UNSPECIFIED.);
#23370=B_SPLINE_CURVE_WITH_KNOTS('',2,(#79454,#79455,#79456),
 .UNSPECIFIED.,.F.,.F.,(3,3),(0.,1.),.UNSPECIFIED.);
#23371=B_SPLINE_CURVE_WITH_KNOTS('',2,(#79459,#79460,#79461),
 .UNSPECIFIED.,.F.,.F.,(3,3),(0.,1.),.UNSPECIFIED.);
#23372=B_SPLINE_CURVE_WITH_KNOTS('',2,(#79469,#79470,#79471),
 .UNSPECIFIED.,.F.,.F.,(3,3),(0.,1.),.UNSPECIFIED.);
#23373=B_SPLINE_CURVE_WITH_KNOTS('',2,(#79474,#79475,#79476),
 .UNSPECIFIED.,.F.,.F.,(3,3),(0.,1.),.UNSPECIFIED.);
#23374=B_SPLINE_CURVE_WITH_KNOTS('',2,(#79484,#79485,#79486),
 .UNSPECIFIED.,.F.,.F.,(3,3),(0.,1.),.UNSPECIFIED.);
#23375=B_SPLINE_CURVE_WITH_KNOTS('',2,(#79489,#79490,#79491),
 .UNSPECIFIED.,.F.,.F.,(3,3),(0.,1.),.UNSPECIFIED.);
#23376=B_SPLINE_CURVE_WITH_KNOTS('',2,(#79499,#79500,#79501),
 .UNSPECIFIED.,.F.,.F.,(3,3),(0.,1.),.UNSPECIFIED.);
#23377=B_SPLINE_CURVE_WITH_KNOTS('',2,(#79504,#79505,#79506),
 .UNSPECIFIED.,.F.,.F.,(3,3),(0.,1.),.UNSPECIFIED.);
#23378=B_SPLINE_CURVE_WITH_KNOTS('',2,(#79513,#79514,#79515),
 .UNSPECIFIED.,.F.,.F.,(3,3),(0.,1.),.UNSPECIFIED.);
#23379=B_SPLINE_CURVE_WITH_KNOTS('',2,(#79516,#79517,#79518),
 .UNSPECIFIED.,.F.,.F.,(3,3),(0.,1.),.UNSPECIFIED.);
#23380=B_SPLINE_CURVE_WITH_KNOTS('',2,(#79527,#79528,#79529),
 .UNSPECIFIED.,.F.,.F.,(3,3),(0.,1.),.UNSPECIFIED.);
#23381=B_SPLINE_CURVE_WITH_KNOTS('',2,(#79533,#79534,#79535),
 .UNSPECIFIED.,.F.,.F.,(3,3),(0.,1.),.UNSPECIFIED.);
#23382=B_SPLINE_CURVE_WITH_KNOTS('',2,(#79544,#79545,#79546),
 .UNSPECIFIED.,.F.,.F.,(3,3),(0.,1.),.UNSPECIFIED.);
#23383=B_SPLINE_CURVE_WITH_KNOTS('',2,(#79549,#79550,#79551),
 .UNSPECIFIED.,.F.,.F.,(3,3),(0.,1.),.UNSPECIFIED.);
#23384=B_SPLINE_CURVE_WITH_KNOTS('',2,(#79559,#79560,#79561),
 .UNSPECIFIED.,.F.,.F.,(3,3),(0.,1.),.UNSPECIFIED.);
#23385=B_SPLINE_CURVE_WITH_KNOTS('',2,(#79564,#79565,#79566),
 .UNSPECIFIED.,.F.,.F.,(3,3),(0.,1.),.UNSPECIFIED.);
#23386=B_SPLINE_CURVE_WITH_KNOTS('',2,(#79574,#79575,#79576),
 .UNSPECIFIED.,.F.,.F.,(3,3),(0.,1.),.UNSPECIFIED.);
#23387=B_SPLINE_CURVE_WITH_KNOTS('',2,(#79579,#79580,#79581),
 .UNSPECIFIED.,.F.,.F.,(3,3),(0.,1.),.UNSPECIFIED.);
#23388=B_SPLINE_CURVE_WITH_KNOTS('',2,(#79589,#79590,#79591),
 .UNSPECIFIED.,.F.,.F.,(3,3),(0.,1.),.UNSPECIFIED.);
#23389=B_SPLINE_CURVE_WITH_KNOTS('',2,(#79594,#79595,#79596),
 .UNSPECIFIED.,.F.,.F.,(3,3),(0.,1.),.UNSPECIFIED.);
#23390=B_SPLINE_CURVE_WITH_KNOTS('',2,(#79604,#79605,#79606),
 .UNSPECIFIED.,.F.,.F.,(3,3),(0.,1.),.UNSPECIFIED.);
#23391=B_SPLINE_CURVE_WITH_KNOTS('',2,(#79609,#79610,#79611),
 .UNSPECIFIED.,.F.,.F.,(3,3),(0.,1.),.UNSPECIFIED.);
#23392=B_SPLINE_CURVE_WITH_KNOTS('',2,(#79619,#79620,#79621),
 .UNSPECIFIED.,.F.,.F.,(3,3),(0.,1.),.UNSPECIFIED.);
#23393=B_SPLINE_CURVE_WITH_KNOTS('',2,(#79624,#79625,#79626),
 .UNSPECIFIED.,.F.,.F.,(3,3),(0.,1.),.UNSPECIFIED.);
#23394=B_SPLINE_CURVE_WITH_KNOTS('',2,(#79634,#79635,#79636),
 .UNSPECIFIED.,.F.,.F.,(3,3),(0.,1.),.UNSPECIFIED.);
#23395=B_SPLINE_CURVE_WITH_KNOTS('',2,(#79639,#79640,#79641),
 .UNSPECIFIED.,.F.,.F.,(3,3),(0.,1.),.UNSPECIFIED.);
#23396=B_SPLINE_CURVE_WITH_KNOTS('',2,(#79649,#79650,#79651),
 .UNSPECIFIED.,.F.,.F.,(3,3),(0.,1.),.UNSPECIFIED.);
#23397=B_SPLINE_CURVE_WITH_KNOTS('',2,(#79654,#79655,#79656),
 .UNSPECIFIED.,.F.,.F.,(3,3),(0.,1.),.UNSPECIFIED.);
#23398=B_SPLINE_CURVE_WITH_KNOTS('',2,(#79664,#79665,#79666),
 .UNSPECIFIED.,.F.,.F.,(3,3),(0.,1.),.UNSPECIFIED.);
#23399=B_SPLINE_CURVE_WITH_KNOTS('',2,(#79669,#79670,#79671),
 .UNSPECIFIED.,.F.,.F.,(3,3),(0.,1.),.UNSPECIFIED.);
#23400=B_SPLINE_CURVE_WITH_KNOTS('',2,(#79679,#79680,#79681),
 .UNSPECIFIED.,.F.,.F.,(3,3),(0.,1.),.UNSPECIFIED.);
#23401=B_SPLINE_CURVE_WITH_KNOTS('',2,(#79684,#79685,#79686),
 .UNSPECIFIED.,.F.,.F.,(3,3),(0.,1.),.UNSPECIFIED.);
#23402=B_SPLINE_CURVE_WITH_KNOTS('',2,(#79693,#79694,#79695),
 .UNSPECIFIED.,.F.,.F.,(3,3),(0.,1.),.UNSPECIFIED.);
#23403=B_SPLINE_CURVE_WITH_KNOTS('',2,(#79696,#79697,#79698),
 .UNSPECIFIED.,.F.,.F.,(3,3),(0.,1.),.UNSPECIFIED.);
#23404=B_SPLINE_CURVE_WITH_KNOTS('',2,(#79795,#79796,#79797),
 .UNSPECIFIED.,.F.,.F.,(3,3),(0.,1.),.UNSPECIFIED.);
#23405=B_SPLINE_CURVE_WITH_KNOTS('',2,(#79801,#79802,#79803),
 .UNSPECIFIED.,.F.,.F.,(3,3),(0.,1.),.UNSPECIFIED.);
#23406=B_SPLINE_CURVE_WITH_KNOTS('',2,(#79812,#79813,#79814),
 .UNSPECIFIED.,.F.,.F.,(3,3),(0.,1.),.UNSPECIFIED.);
#23407=B_SPLINE_CURVE_WITH_KNOTS('',2,(#79817,#79818,#79819),
 .UNSPECIFIED.,.F.,.F.,(3,3),(0.,1.),.UNSPECIFIED.);
#23408=B_SPLINE_CURVE_WITH_KNOTS('',2,(#79827,#79828,#79829),
 .UNSPECIFIED.,.F.,.F.,(3,3),(0.,1.),.UNSPECIFIED.);
#23409=B_SPLINE_CURVE_WITH_KNOTS('',2,(#79832,#79833,#79834),
 .UNSPECIFIED.,.F.,.F.,(3,3),(0.,1.),.UNSPECIFIED.);
#23410=B_SPLINE_CURVE_WITH_KNOTS('',2,(#79842,#79843,#79844),
 .UNSPECIFIED.,.F.,.F.,(3,3),(0.,1.),.UNSPECIFIED.);
#23411=B_SPLINE_CURVE_WITH_KNOTS('',2,(#79847,#79848,#79849),
 .UNSPECIFIED.,.F.,.F.,(3,3),(0.,1.),.UNSPECIFIED.);
#23412=B_SPLINE_CURVE_WITH_KNOTS('',2,(#79857,#79858,#79859),
 .UNSPECIFIED.,.F.,.F.,(3,3),(0.,1.),.UNSPECIFIED.);
#23413=B_SPLINE_CURVE_WITH_KNOTS('',2,(#79862,#79863,#79864),
 .UNSPECIFIED.,.F.,.F.,(3,3),(0.,1.),.UNSPECIFIED.);
#23414=B_SPLINE_CURVE_WITH_KNOTS('',2,(#79872,#79873,#79874),
 .UNSPECIFIED.,.F.,.F.,(3,3),(0.,1.),.UNSPECIFIED.);
#23415=B_SPLINE_CURVE_WITH_KNOTS('',2,(#79877,#79878,#79879),
 .UNSPECIFIED.,.F.,.F.,(3,3),(0.,1.),.UNSPECIFIED.);
#23416=B_SPLINE_CURVE_WITH_KNOTS('',2,(#79887,#79888,#79889),
 .UNSPECIFIED.,.F.,.F.,(3,3),(0.,1.),.UNSPECIFIED.);
#23417=B_SPLINE_CURVE_WITH_KNOTS('',2,(#79892,#79893,#79894),
 .UNSPECIFIED.,.F.,.F.,(3,3),(0.,1.),.UNSPECIFIED.);
#23418=B_SPLINE_CURVE_WITH_KNOTS('',2,(#79901,#79902,#79903),
 .UNSPECIFIED.,.F.,.F.,(3,3),(0.,1.),.UNSPECIFIED.);
#23419=B_SPLINE_CURVE_WITH_KNOTS('',2,(#79904,#79905,#79906),
 .UNSPECIFIED.,.F.,.F.,(3,3),(0.,1.),.UNSPECIFIED.);
#23420=B_SPLINE_CURVE_WITH_KNOTS('',2,(#79915,#79916,#79917),
 .UNSPECIFIED.,.F.,.F.,(3,3),(0.,1.),.UNSPECIFIED.);
#23421=B_SPLINE_CURVE_WITH_KNOTS('',2,(#79921,#79922,#79923),
 .UNSPECIFIED.,.F.,.F.,(3,3),(0.,1.),.UNSPECIFIED.);
#23422=B_SPLINE_CURVE_WITH_KNOTS('',2,(#79932,#79933,#79934),
 .UNSPECIFIED.,.F.,.F.,(3,3),(0.,1.),.UNSPECIFIED.);
#23423=B_SPLINE_CURVE_WITH_KNOTS('',2,(#79937,#79938,#79939),
 .UNSPECIFIED.,.F.,.F.,(3,3),(0.,1.),.UNSPECIFIED.);
#23424=B_SPLINE_CURVE_WITH_KNOTS('',2,(#79947,#79948,#79949),
 .UNSPECIFIED.,.F.,.F.,(3,3),(0.,1.),.UNSPECIFIED.);
#23425=B_SPLINE_CURVE_WITH_KNOTS('',2,(#79952,#79953,#79954),
 .UNSPECIFIED.,.F.,.F.,(3,3),(0.,1.),.UNSPECIFIED.);
#23426=B_SPLINE_CURVE_WITH_KNOTS('',2,(#79962,#79963,#79964),
 .UNSPECIFIED.,.F.,.F.,(3,3),(0.,1.),.UNSPECIFIED.);
#23427=B_SPLINE_CURVE_WITH_KNOTS('',2,(#79967,#79968,#79969),
 .UNSPECIFIED.,.F.,.F.,(3,3),(0.,1.),.UNSPECIFIED.);
#23428=B_SPLINE_CURVE_WITH_KNOTS('',2,(#79977,#79978,#79979),
 .UNSPECIFIED.,.F.,.F.,(3,3),(0.,1.),.UNSPECIFIED.);
#23429=B_SPLINE_CURVE_WITH_KNOTS('',2,(#79982,#79983,#79984),
 .UNSPECIFIED.,.F.,.F.,(3,3),(0.,1.),.UNSPECIFIED.);
#23430=B_SPLINE_CURVE_WITH_KNOTS('',2,(#79992,#79993,#79994),
 .UNSPECIFIED.,.F.,.F.,(3,3),(0.,1.),.UNSPECIFIED.);
#23431=B_SPLINE_CURVE_WITH_KNOTS('',2,(#79997,#79998,#79999),
 .UNSPECIFIED.,.F.,.F.,(3,3),(0.,1.),.UNSPECIFIED.);
#23432=B_SPLINE_CURVE_WITH_KNOTS('',2,(#80007,#80008,#80009),
 .UNSPECIFIED.,.F.,.F.,(3,3),(0.,1.),.UNSPECIFIED.);
#23433=B_SPLINE_CURVE_WITH_KNOTS('',2,(#80012,#80013,#80014),
 .UNSPECIFIED.,.F.,.F.,(3,3),(0.,1.),.UNSPECIFIED.);
#23434=B_SPLINE_CURVE_WITH_KNOTS('',2,(#80022,#80023,#80024),
 .UNSPECIFIED.,.F.,.F.,(3,3),(0.,1.),.UNSPECIFIED.);
#23435=B_SPLINE_CURVE_WITH_KNOTS('',2,(#80027,#80028,#80029),
 .UNSPECIFIED.,.F.,.F.,(3,3),(0.,1.),.UNSPECIFIED.);
#23436=B_SPLINE_CURVE_WITH_KNOTS('',2,(#80037,#80038,#80039),
 .UNSPECIFIED.,.F.,.F.,(3,3),(0.,1.),.UNSPECIFIED.);
#23437=B_SPLINE_CURVE_WITH_KNOTS('',2,(#80042,#80043,#80044),
 .UNSPECIFIED.,.F.,.F.,(3,3),(0.,1.),.UNSPECIFIED.);
#23438=B_SPLINE_CURVE_WITH_KNOTS('',2,(#80052,#80053,#80054),
 .UNSPECIFIED.,.F.,.F.,(3,3),(0.,1.),.UNSPECIFIED.);
#23439=B_SPLINE_CURVE_WITH_KNOTS('',2,(#80057,#80058,#80059),
 .UNSPECIFIED.,.F.,.F.,(3,3),(0.,1.),.UNSPECIFIED.);
#23440=B_SPLINE_CURVE_WITH_KNOTS('',2,(#80067,#80068,#80069),
 .UNSPECIFIED.,.F.,.F.,(3,3),(0.,1.),.UNSPECIFIED.);
#23441=B_SPLINE_CURVE_WITH_KNOTS('',2,(#80072,#80073,#80074),
 .UNSPECIFIED.,.F.,.F.,(3,3),(0.,1.),.UNSPECIFIED.);
#23442=B_SPLINE_CURVE_WITH_KNOTS('',2,(#80081,#80082,#80083),
 .UNSPECIFIED.,.F.,.F.,(3,3),(0.,1.),.UNSPECIFIED.);
#23443=B_SPLINE_CURVE_WITH_KNOTS('',2,(#80084,#80085,#80086),
 .UNSPECIFIED.,.F.,.F.,(3,3),(0.,1.),.UNSPECIFIED.);
#23444=B_SPLINE_CURVE_WITH_KNOTS('',2,(#80096,#80097,#80098),
 .UNSPECIFIED.,.F.,.F.,(3,3),(0.,1.),.UNSPECIFIED.);
#23445=B_SPLINE_CURVE_WITH_KNOTS('',2,(#80102,#80103,#80104),
 .UNSPECIFIED.,.F.,.F.,(3,3),(0.,1.),.UNSPECIFIED.);
#23446=B_SPLINE_CURVE_WITH_KNOTS('',2,(#80113,#80114,#80115),
 .UNSPECIFIED.,.F.,.F.,(3,3),(0.,1.),.UNSPECIFIED.);
#23447=B_SPLINE_CURVE_WITH_KNOTS('',2,(#80118,#80119,#80120),
 .UNSPECIFIED.,.F.,.F.,(3,3),(0.,1.),.UNSPECIFIED.);
#23448=B_SPLINE_CURVE_WITH_KNOTS('',2,(#80128,#80129,#80130),
 .UNSPECIFIED.,.F.,.F.,(3,3),(0.,1.),.UNSPECIFIED.);
#23449=B_SPLINE_CURVE_WITH_KNOTS('',2,(#80133,#80134,#80135),
 .UNSPECIFIED.,.F.,.F.,(3,3),(0.,1.),.UNSPECIFIED.);
#23450=B_SPLINE_CURVE_WITH_KNOTS('',2,(#80143,#80144,#80145),
 .UNSPECIFIED.,.F.,.F.,(3,3),(0.,1.),.UNSPECIFIED.);
#23451=B_SPLINE_CURVE_WITH_KNOTS('',2,(#80148,#80149,#80150),
 .UNSPECIFIED.,.F.,.F.,(3,3),(0.,1.),.UNSPECIFIED.);
#23452=B_SPLINE_CURVE_WITH_KNOTS('',2,(#80158,#80159,#80160),
 .UNSPECIFIED.,.F.,.F.,(3,3),(0.,1.),.UNSPECIFIED.);
#23453=B_SPLINE_CURVE_WITH_KNOTS('',2,(#80163,#80164,#80165),
 .UNSPECIFIED.,.F.,.F.,(3,3),(0.,1.),.UNSPECIFIED.);
#23454=B_SPLINE_CURVE_WITH_KNOTS('',2,(#80173,#80174,#80175),
 .UNSPECIFIED.,.F.,.F.,(3,3),(0.,1.),.UNSPECIFIED.);
#23455=B_SPLINE_CURVE_WITH_KNOTS('',2,(#80178,#80179,#80180),
 .UNSPECIFIED.,.F.,.F.,(3,3),(0.,1.),.UNSPECIFIED.);
#23456=B_SPLINE_CURVE_WITH_KNOTS('',2,(#80188,#80189,#80190),
 .UNSPECIFIED.,.F.,.F.,(3,3),(0.,1.),.UNSPECIFIED.);
#23457=B_SPLINE_CURVE_WITH_KNOTS('',2,(#80193,#80194,#80195),
 .UNSPECIFIED.,.F.,.F.,(3,3),(0.,1.),.UNSPECIFIED.);
#23458=B_SPLINE_CURVE_WITH_KNOTS('',2,(#80203,#80204,#80205),
 .UNSPECIFIED.,.F.,.F.,(3,3),(0.,1.),.UNSPECIFIED.);
#23459=B_SPLINE_CURVE_WITH_KNOTS('',2,(#80208,#80209,#80210),
 .UNSPECIFIED.,.F.,.F.,(3,3),(0.,1.),.UNSPECIFIED.);
#23460=B_SPLINE_CURVE_WITH_KNOTS('',2,(#80218,#80219,#80220),
 .UNSPECIFIED.,.F.,.F.,(3,3),(0.,1.),.UNSPECIFIED.);
#23461=B_SPLINE_CURVE_WITH_KNOTS('',2,(#80223,#80224,#80225),
 .UNSPECIFIED.,.F.,.F.,(3,3),(0.,1.),.UNSPECIFIED.);
#23462=B_SPLINE_CURVE_WITH_KNOTS('',2,(#80233,#80234,#80235),
 .UNSPECIFIED.,.F.,.F.,(3,3),(0.,1.),.UNSPECIFIED.);
#23463=B_SPLINE_CURVE_WITH_KNOTS('',2,(#80238,#80239,#80240),
 .UNSPECIFIED.,.F.,.F.,(3,3),(0.,1.),.UNSPECIFIED.);
#23464=B_SPLINE_CURVE_WITH_KNOTS('',2,(#80248,#80249,#80250),
 .UNSPECIFIED.,.F.,.F.,(3,3),(0.,1.),.UNSPECIFIED.);
#23465=B_SPLINE_CURVE_WITH_KNOTS('',2,(#80253,#80254,#80255),
 .UNSPECIFIED.,.F.,.F.,(3,3),(0.,1.),.UNSPECIFIED.);
#23466=B_SPLINE_CURVE_WITH_KNOTS('',2,(#80263,#80264,#80265),
 .UNSPECIFIED.,.F.,.F.,(3,3),(0.,1.),.UNSPECIFIED.);
#23467=B_SPLINE_CURVE_WITH_KNOTS('',2,(#80268,#80269,#80270),
 .UNSPECIFIED.,.F.,.F.,(3,3),(0.,1.),.UNSPECIFIED.);
#23468=B_SPLINE_CURVE_WITH_KNOTS('',2,(#80284,#80285,#80286),
 .UNSPECIFIED.,.F.,.F.,(3,3),(0.,1.),.UNSPECIFIED.);
#23469=B_SPLINE_CURVE_WITH_KNOTS('',2,(#80289,#80290,#80291),
 .UNSPECIFIED.,.F.,.F.,(3,3),(0.,1.),.UNSPECIFIED.);
#23470=B_SPLINE_CURVE_WITH_KNOTS('',2,(#80299,#80300,#80301),
 .UNSPECIFIED.,.F.,.F.,(3,3),(0.,1.),.UNSPECIFIED.);
#23471=B_SPLINE_CURVE_WITH_KNOTS('',2,(#80304,#80305,#80306),
 .UNSPECIFIED.,.F.,.F.,(3,3),(0.,1.),.UNSPECIFIED.);
#23472=B_SPLINE_CURVE_WITH_KNOTS('',2,(#80314,#80315,#80316),
 .UNSPECIFIED.,.F.,.F.,(3,3),(0.,1.),.UNSPECIFIED.);
#23473=B_SPLINE_CURVE_WITH_KNOTS('',2,(#80319,#80320,#80321),
 .UNSPECIFIED.,.F.,.F.,(3,3),(0.,1.),.UNSPECIFIED.);
#23474=B_SPLINE_CURVE_WITH_KNOTS('',2,(#80329,#80330,#80331),
 .UNSPECIFIED.,.F.,.F.,(3,3),(0.,1.),.UNSPECIFIED.);
#23475=B_SPLINE_CURVE_WITH_KNOTS('',2,(#80334,#80335,#80336),
 .UNSPECIFIED.,.F.,.F.,(3,3),(0.,1.),.UNSPECIFIED.);
#23476=B_SPLINE_CURVE_WITH_KNOTS('',2,(#80344,#80345,#80346),
 .UNSPECIFIED.,.F.,.F.,(3,3),(0.,1.),.UNSPECIFIED.);
#23477=B_SPLINE_CURVE_WITH_KNOTS('',2,(#80349,#80350,#80351),
 .UNSPECIFIED.,.F.,.F.,(3,3),(0.,1.),.UNSPECIFIED.);
#23478=B_SPLINE_CURVE_WITH_KNOTS('',2,(#80359,#80360,#80361),
 .UNSPECIFIED.,.F.,.F.,(3,3),(0.,1.),.UNSPECIFIED.);
#23479=B_SPLINE_CURVE_WITH_KNOTS('',2,(#80364,#80365,#80366),
 .UNSPECIFIED.,.F.,.F.,(3,3),(0.,1.),.UNSPECIFIED.);
#23480=B_SPLINE_CURVE_WITH_KNOTS('',2,(#80374,#80375,#80376),
 .UNSPECIFIED.,.F.,.F.,(3,3),(0.,1.),.UNSPECIFIED.);
#23481=B_SPLINE_CURVE_WITH_KNOTS('',2,(#80379,#80380,#80381),
 .UNSPECIFIED.,.F.,.F.,(3,3),(0.,1.),.UNSPECIFIED.);
#23482=B_SPLINE_CURVE_WITH_KNOTS('',2,(#80395,#80396,#80397),
 .UNSPECIFIED.,.F.,.F.,(3,3),(0.,1.),.UNSPECIFIED.);
#23483=B_SPLINE_CURVE_WITH_KNOTS('',2,(#80400,#80401,#80402),
 .UNSPECIFIED.,.F.,.F.,(3,3),(0.,1.),.UNSPECIFIED.);
#23484=B_SPLINE_CURVE_WITH_KNOTS('',2,(#80410,#80411,#80412),
 .UNSPECIFIED.,.F.,.F.,(3,3),(0.,1.),.UNSPECIFIED.);
#23485=B_SPLINE_CURVE_WITH_KNOTS('',2,(#80415,#80416,#80417),
 .UNSPECIFIED.,.F.,.F.,(3,3),(0.,1.),.UNSPECIFIED.);
#23486=B_SPLINE_CURVE_WITH_KNOTS('',2,(#80425,#80426,#80427),
 .UNSPECIFIED.,.F.,.F.,(3,3),(0.,1.),.UNSPECIFIED.);
#23487=B_SPLINE_CURVE_WITH_KNOTS('',2,(#80430,#80431,#80432),
 .UNSPECIFIED.,.F.,.F.,(3,3),(0.,1.),.UNSPECIFIED.);
#23488=B_SPLINE_CURVE_WITH_KNOTS('',2,(#80440,#80441,#80442),
 .UNSPECIFIED.,.F.,.F.,(3,3),(0.,1.),.UNSPECIFIED.);
#23489=B_SPLINE_CURVE_WITH_KNOTS('',2,(#80445,#80446,#80447),
 .UNSPECIFIED.,.F.,.F.,(3,3),(0.,1.),.UNSPECIFIED.);
#23490=B_SPLINE_CURVE_WITH_KNOTS('',2,(#80455,#80456,#80457),
 .UNSPECIFIED.,.F.,.F.,(3,3),(0.,1.),.UNSPECIFIED.);
#23491=B_SPLINE_CURVE_WITH_KNOTS('',2,(#80460,#80461,#80462),
 .UNSPECIFIED.,.F.,.F.,(3,3),(0.,1.),.UNSPECIFIED.);
#23492=B_SPLINE_CURVE_WITH_KNOTS('',2,(#80470,#80471,#80472),
 .UNSPECIFIED.,.F.,.F.,(3,3),(0.,1.),.UNSPECIFIED.);
#23493=B_SPLINE_CURVE_WITH_KNOTS('',2,(#80475,#80476,#80477),
 .UNSPECIFIED.,.F.,.F.,(3,3),(0.,1.),.UNSPECIFIED.);
#23494=B_SPLINE_CURVE_WITH_KNOTS('',2,(#80485,#80486,#80487),
 .UNSPECIFIED.,.F.,.F.,(3,3),(0.,1.),.UNSPECIFIED.);
#23495=B_SPLINE_CURVE_WITH_KNOTS('',2,(#80490,#80491,#80492),
 .UNSPECIFIED.,.F.,.F.,(3,3),(0.,1.),.UNSPECIFIED.);
#23496=B_SPLINE_CURVE_WITH_KNOTS('',2,(#80505,#80506,#80507),
 .UNSPECIFIED.,.F.,.F.,(3,3),(0.,1.),.UNSPECIFIED.);
#23497=B_SPLINE_CURVE_WITH_KNOTS('',2,(#80508,#80509,#80510),
 .UNSPECIFIED.,.F.,.F.,(3,3),(0.,1.),.UNSPECIFIED.);
#23498=B_SPLINE_CURVE_WITH_KNOTS('',2,(#80521,#80522,#80523),
 .UNSPECIFIED.,.F.,.F.,(3,3),(0.,1.),.UNSPECIFIED.);
#23499=B_SPLINE_CURVE_WITH_KNOTS('',2,(#80527,#80528,#80529),
 .UNSPECIFIED.,.F.,.F.,(3,3),(0.,1.),.UNSPECIFIED.);
#23500=B_SPLINE_CURVE_WITH_KNOTS('',2,(#80538,#80539,#80540),
 .UNSPECIFIED.,.F.,.F.,(3,3),(0.,1.),.UNSPECIFIED.);
#23501=B_SPLINE_CURVE_WITH_KNOTS('',2,(#80543,#80544,#80545),
 .UNSPECIFIED.,.F.,.F.,(3,3),(0.,1.),.UNSPECIFIED.);
#23502=B_SPLINE_CURVE_WITH_KNOTS('',2,(#80553,#80554,#80555),
 .UNSPECIFIED.,.F.,.F.,(3,3),(0.,1.),.UNSPECIFIED.);
#23503=B_SPLINE_CURVE_WITH_KNOTS('',2,(#80558,#80559,#80560),
 .UNSPECIFIED.,.F.,.F.,(3,3),(0.,1.),.UNSPECIFIED.);
#23504=B_SPLINE_CURVE_WITH_KNOTS('',2,(#80568,#80569,#80570),
 .UNSPECIFIED.,.F.,.F.,(3,3),(0.,1.),.UNSPECIFIED.);
#23505=B_SPLINE_CURVE_WITH_KNOTS('',2,(#80573,#80574,#80575),
 .UNSPECIFIED.,.F.,.F.,(3,3),(0.,1.),.UNSPECIFIED.);
#23506=B_SPLINE_CURVE_WITH_KNOTS('',2,(#80583,#80584,#80585),
 .UNSPECIFIED.,.F.,.F.,(3,3),(0.,1.),.UNSPECIFIED.);
#23507=B_SPLINE_CURVE_WITH_KNOTS('',2,(#80588,#80589,#80590),
 .UNSPECIFIED.,.F.,.F.,(3,3),(0.,1.),.UNSPECIFIED.);
#23508=B_SPLINE_CURVE_WITH_KNOTS('',2,(#80598,#80599,#80600),
 .UNSPECIFIED.,.F.,.F.,(3,3),(0.,1.),.UNSPECIFIED.);
#23509=B_SPLINE_CURVE_WITH_KNOTS('',2,(#80603,#80604,#80605),
 .UNSPECIFIED.,.F.,.F.,(3,3),(0.,1.),.UNSPECIFIED.);
#23510=B_SPLINE_CURVE_WITH_KNOTS('',2,(#80613,#80614,#80615),
 .UNSPECIFIED.,.F.,.F.,(3,3),(0.,1.),.UNSPECIFIED.);
#23511=B_SPLINE_CURVE_WITH_KNOTS('',2,(#80618,#80619,#80620),
 .UNSPECIFIED.,.F.,.F.,(3,3),(0.,1.),.UNSPECIFIED.);
#23512=B_SPLINE_CURVE_WITH_KNOTS('',2,(#80627,#80628,#80629),
 .UNSPECIFIED.,.F.,.F.,(3,3),(0.,1.),.UNSPECIFIED.);
#23513=B_SPLINE_CURVE_WITH_KNOTS('',2,(#80630,#80631,#80632),
 .UNSPECIFIED.,.F.,.F.,(3,3),(0.,1.),.UNSPECIFIED.);
#23514=B_SPLINE_CURVE_WITH_KNOTS('',2,(#80641,#80642,#80643),
 .UNSPECIFIED.,.F.,.F.,(3,3),(0.,1.),.UNSPECIFIED.);
#23515=B_SPLINE_CURVE_WITH_KNOTS('',2,(#80647,#80648,#80649),
 .UNSPECIFIED.,.F.,.F.,(3,3),(0.,1.),.UNSPECIFIED.);
#23516=B_SPLINE_CURVE_WITH_KNOTS('',2,(#80658,#80659,#80660),
 .UNSPECIFIED.,.F.,.F.,(3,3),(0.,1.),.UNSPECIFIED.);
#23517=B_SPLINE_CURVE_WITH_KNOTS('',2,(#80663,#80664,#80665),
 .UNSPECIFIED.,.F.,.F.,(3,3),(0.,1.),.UNSPECIFIED.);
#23518=B_SPLINE_CURVE_WITH_KNOTS('',2,(#80673,#80674,#80675),
 .UNSPECIFIED.,.F.,.F.,(3,3),(0.,1.),.UNSPECIFIED.);
#23519=B_SPLINE_CURVE_WITH_KNOTS('',2,(#80678,#80679,#80680),
 .UNSPECIFIED.,.F.,.F.,(3,3),(0.,1.),.UNSPECIFIED.);
#23520=B_SPLINE_CURVE_WITH_KNOTS('',2,(#80688,#80689,#80690),
 .UNSPECIFIED.,.F.,.F.,(3,3),(0.,1.),.UNSPECIFIED.);
#23521=B_SPLINE_CURVE_WITH_KNOTS('',2,(#80693,#80694,#80695),
 .UNSPECIFIED.,.F.,.F.,(3,3),(0.,1.),.UNSPECIFIED.);
#23522=B_SPLINE_CURVE_WITH_KNOTS('',2,(#80703,#80704,#80705),
 .UNSPECIFIED.,.F.,.F.,(3,3),(0.,1.),.UNSPECIFIED.);
#23523=B_SPLINE_CURVE_WITH_KNOTS('',2,(#80708,#80709,#80710),
 .UNSPECIFIED.,.F.,.F.,(3,3),(0.,1.),.UNSPECIFIED.);
#23524=B_SPLINE_CURVE_WITH_KNOTS('',2,(#80718,#80719,#80720),
 .UNSPECIFIED.,.F.,.F.,(3,3),(0.,1.),.UNSPECIFIED.);
#23525=B_SPLINE_CURVE_WITH_KNOTS('',2,(#80723,#80724,#80725),
 .UNSPECIFIED.,.F.,.F.,(3,3),(0.,1.),.UNSPECIFIED.);
#23526=B_SPLINE_CURVE_WITH_KNOTS('',2,(#80733,#80734,#80735),
 .UNSPECIFIED.,.F.,.F.,(3,3),(0.,1.),.UNSPECIFIED.);
#23527=B_SPLINE_CURVE_WITH_KNOTS('',2,(#80738,#80739,#80740),
 .UNSPECIFIED.,.F.,.F.,(3,3),(0.,1.),.UNSPECIFIED.);
#23528=B_SPLINE_CURVE_WITH_KNOTS('',2,(#80748,#80749,#80750),
 .UNSPECIFIED.,.F.,.F.,(3,3),(0.,1.),.UNSPECIFIED.);
#23529=B_SPLINE_CURVE_WITH_KNOTS('',2,(#80753,#80754,#80755),
 .UNSPECIFIED.,.F.,.F.,(3,3),(0.,1.),.UNSPECIFIED.);
#23530=B_SPLINE_CURVE_WITH_KNOTS('',2,(#80763,#80764,#80765),
 .UNSPECIFIED.,.F.,.F.,(3,3),(0.,1.),.UNSPECIFIED.);
#23531=B_SPLINE_CURVE_WITH_KNOTS('',2,(#80768,#80769,#80770),
 .UNSPECIFIED.,.F.,.F.,(3,3),(0.,1.),.UNSPECIFIED.);
#23532=B_SPLINE_CURVE_WITH_KNOTS('',2,(#80778,#80779,#80780),
 .UNSPECIFIED.,.F.,.F.,(3,3),(0.,1.),.UNSPECIFIED.);
#23533=B_SPLINE_CURVE_WITH_KNOTS('',2,(#80783,#80784,#80785),
 .UNSPECIFIED.,.F.,.F.,(3,3),(0.,1.),.UNSPECIFIED.);
#23534=B_SPLINE_CURVE_WITH_KNOTS('',2,(#80793,#80794,#80795),
 .UNSPECIFIED.,.F.,.F.,(3,3),(0.,1.),.UNSPECIFIED.);
#23535=B_SPLINE_CURVE_WITH_KNOTS('',2,(#80798,#80799,#80800),
 .UNSPECIFIED.,.F.,.F.,(3,3),(0.,1.),.UNSPECIFIED.);
#23536=B_SPLINE_CURVE_WITH_KNOTS('',2,(#80807,#80808,#80809),
 .UNSPECIFIED.,.F.,.F.,(3,3),(0.,1.),.UNSPECIFIED.);
#23537=B_SPLINE_CURVE_WITH_KNOTS('',2,(#80810,#80811,#80812),
 .UNSPECIFIED.,.F.,.F.,(3,3),(0.,1.),.UNSPECIFIED.);
#23538=B_SPLINE_CURVE_WITH_KNOTS('',2,(#80822,#80823,#80824),
 .UNSPECIFIED.,.F.,.F.,(3,3),(0.,1.),.UNSPECIFIED.);
#23539=B_SPLINE_CURVE_WITH_KNOTS('',2,(#80828,#80829,#80830),
 .UNSPECIFIED.,.F.,.F.,(3,3),(0.,1.),.UNSPECIFIED.);
#23540=B_SPLINE_CURVE_WITH_KNOTS('',2,(#80839,#80840,#80841),
 .UNSPECIFIED.,.F.,.F.,(3,3),(0.,1.),.UNSPECIFIED.);
#23541=B_SPLINE_CURVE_WITH_KNOTS('',2,(#80844,#80845,#80846),
 .UNSPECIFIED.,.F.,.F.,(3,3),(0.,1.),.UNSPECIFIED.);
#23542=B_SPLINE_CURVE_WITH_KNOTS('',2,(#80854,#80855,#80856),
 .UNSPECIFIED.,.F.,.F.,(3,3),(0.,1.),.UNSPECIFIED.);
#23543=B_SPLINE_CURVE_WITH_KNOTS('',2,(#80859,#80860,#80861),
 .UNSPECIFIED.,.F.,.F.,(3,3),(0.,1.),.UNSPECIFIED.);
#23544=B_SPLINE_CURVE_WITH_KNOTS('',2,(#80869,#80870,#80871),
 .UNSPECIFIED.,.F.,.F.,(3,3),(0.,1.),.UNSPECIFIED.);
#23545=B_SPLINE_CURVE_WITH_KNOTS('',2,(#80874,#80875,#80876),
 .UNSPECIFIED.,.F.,.F.,(3,3),(0.,1.),.UNSPECIFIED.);
#23546=B_SPLINE_CURVE_WITH_KNOTS('',2,(#80884,#80885,#80886),
 .UNSPECIFIED.,.F.,.F.,(3,3),(0.,1.),.UNSPECIFIED.);
#23547=B_SPLINE_CURVE_WITH_KNOTS('',2,(#80889,#80890,#80891),
 .UNSPECIFIED.,.F.,.F.,(3,3),(0.,1.),.UNSPECIFIED.);
#23548=B_SPLINE_CURVE_WITH_KNOTS('',2,(#80899,#80900,#80901),
 .UNSPECIFIED.,.F.,.F.,(3,3),(0.,1.),.UNSPECIFIED.);
#23549=B_SPLINE_CURVE_WITH_KNOTS('',2,(#80904,#80905,#80906),
 .UNSPECIFIED.,.F.,.F.,(3,3),(0.,1.),.UNSPECIFIED.);
#23550=B_SPLINE_CURVE_WITH_KNOTS('',2,(#80914,#80915,#80916),
 .UNSPECIFIED.,.F.,.F.,(3,3),(0.,1.),.UNSPECIFIED.);
#23551=B_SPLINE_CURVE_WITH_KNOTS('',2,(#80919,#80920,#80921),
 .UNSPECIFIED.,.F.,.F.,(3,3),(0.,1.),.UNSPECIFIED.);
#23552=B_SPLINE_CURVE_WITH_KNOTS('',2,(#80929,#80930,#80931),
 .UNSPECIFIED.,.F.,.F.,(3,3),(0.,1.),.UNSPECIFIED.);
#23553=B_SPLINE_CURVE_WITH_KNOTS('',2,(#80934,#80935,#80936),
 .UNSPECIFIED.,.F.,.F.,(3,3),(0.,1.),.UNSPECIFIED.);
#23554=B_SPLINE_CURVE_WITH_KNOTS('',2,(#80944,#80945,#80946),
 .UNSPECIFIED.,.F.,.F.,(3,3),(0.,1.),.UNSPECIFIED.);
#23555=B_SPLINE_CURVE_WITH_KNOTS('',2,(#80949,#80950,#80951),
 .UNSPECIFIED.,.F.,.F.,(3,3),(0.,1.),.UNSPECIFIED.);
#23556=B_SPLINE_CURVE_WITH_KNOTS('',2,(#80965,#80966,#80967),
 .UNSPECIFIED.,.F.,.F.,(3,3),(0.,1.),.UNSPECIFIED.);
#23557=B_SPLINE_CURVE_WITH_KNOTS('',2,(#80970,#80971,#80972),
 .UNSPECIFIED.,.F.,.F.,(3,3),(0.,1.),.UNSPECIFIED.);
#23558=B_SPLINE_CURVE_WITH_KNOTS('',2,(#80980,#80981,#80982),
 .UNSPECIFIED.,.F.,.F.,(3,3),(0.,1.),.UNSPECIFIED.);
#23559=B_SPLINE_CURVE_WITH_KNOTS('',2,(#80985,#80986,#80987),
 .UNSPECIFIED.,.F.,.F.,(3,3),(0.,1.),.UNSPECIFIED.);
#23560=B_SPLINE_CURVE_WITH_KNOTS('',2,(#80995,#80996,#80997),
 .UNSPECIFIED.,.F.,.F.,(3,3),(0.,1.),.UNSPECIFIED.);
#23561=B_SPLINE_CURVE_WITH_KNOTS('',2,(#81000,#81001,#81002),
 .UNSPECIFIED.,.F.,.F.,(3,3),(0.,1.),.UNSPECIFIED.);
#23562=B_SPLINE_CURVE_WITH_KNOTS('',2,(#81010,#81011,#81012),
 .UNSPECIFIED.,.F.,.F.,(3,3),(0.,1.),.UNSPECIFIED.);
#23563=B_SPLINE_CURVE_WITH_KNOTS('',2,(#81015,#81016,#81017),
 .UNSPECIFIED.,.F.,.F.,(3,3),(0.,1.),.UNSPECIFIED.);
#23564=B_SPLINE_CURVE_WITH_KNOTS('',2,(#81025,#81026,#81027),
 .UNSPECIFIED.,.F.,.F.,(3,3),(0.,1.),.UNSPECIFIED.);
#23565=B_SPLINE_CURVE_WITH_KNOTS('',2,(#81030,#81031,#81032),
 .UNSPECIFIED.,.F.,.F.,(3,3),(0.,1.),.UNSPECIFIED.);
#23566=B_SPLINE_CURVE_WITH_KNOTS('',2,(#81040,#81041,#81042),
 .UNSPECIFIED.,.F.,.F.,(3,3),(0.,1.),.UNSPECIFIED.);
#23567=B_SPLINE_CURVE_WITH_KNOTS('',2,(#81045,#81046,#81047),
 .UNSPECIFIED.,.F.,.F.,(3,3),(0.,1.),.UNSPECIFIED.);
#23568=B_SPLINE_CURVE_WITH_KNOTS('',2,(#81055,#81056,#81057),
 .UNSPECIFIED.,.F.,.F.,(3,3),(0.,1.),.UNSPECIFIED.);
#23569=B_SPLINE_CURVE_WITH_KNOTS('',2,(#81060,#81061,#81062),
 .UNSPECIFIED.,.F.,.F.,(3,3),(0.,1.),.UNSPECIFIED.);
#23570=B_SPLINE_CURVE_WITH_KNOTS('',2,(#81070,#81071,#81072),
 .UNSPECIFIED.,.F.,.F.,(3,3),(0.,1.),.UNSPECIFIED.);
#23571=B_SPLINE_CURVE_WITH_KNOTS('',2,(#81075,#81076,#81077),
 .UNSPECIFIED.,.F.,.F.,(3,3),(0.,1.),.UNSPECIFIED.);
#23572=B_SPLINE_CURVE_WITH_KNOTS('',2,(#81085,#81086,#81087),
 .UNSPECIFIED.,.F.,.F.,(3,3),(0.,1.),.UNSPECIFIED.);
#23573=B_SPLINE_CURVE_WITH_KNOTS('',2,(#81090,#81091,#81092),
 .UNSPECIFIED.,.F.,.F.,(3,3),(0.,1.),.UNSPECIFIED.);
#23574=B_SPLINE_CURVE_WITH_KNOTS('',2,(#81118,#81119,#81120),
 .UNSPECIFIED.,.F.,.F.,(3,3),(0.,1.),.UNSPECIFIED.);
#23575=B_SPLINE_CURVE_WITH_KNOTS('',2,(#81124,#81125,#81126),
 .UNSPECIFIED.,.F.,.F.,(3,3),(0.,1.),.UNSPECIFIED.);
#23576=B_SPLINE_CURVE_WITH_KNOTS('',2,(#81135,#81136,#81137),
 .UNSPECIFIED.,.F.,.F.,(3,3),(0.,1.),.UNSPECIFIED.);
#23577=B_SPLINE_CURVE_WITH_KNOTS('',2,(#81140,#81141,#81142),
 .UNSPECIFIED.,.F.,.F.,(3,3),(0.,1.),.UNSPECIFIED.);
#23578=B_SPLINE_CURVE_WITH_KNOTS('',2,(#81150,#81151,#81152),
 .UNSPECIFIED.,.F.,.F.,(3,3),(0.,1.),.UNSPECIFIED.);
#23579=B_SPLINE_CURVE_WITH_KNOTS('',2,(#81155,#81156,#81157),
 .UNSPECIFIED.,.F.,.F.,(3,3),(0.,1.),.UNSPECIFIED.);
#23580=B_SPLINE_CURVE_WITH_KNOTS('',2,(#81165,#81166,#81167),
 .UNSPECIFIED.,.F.,.F.,(3,3),(0.,1.),.UNSPECIFIED.);
#23581=B_SPLINE_CURVE_WITH_KNOTS('',2,(#81170,#81171,#81172),
 .UNSPECIFIED.,.F.,.F.,(3,3),(0.,1.),.UNSPECIFIED.);
#23582=B_SPLINE_CURVE_WITH_KNOTS('',2,(#81180,#81181,#81182),
 .UNSPECIFIED.,.F.,.F.,(3,3),(0.,1.),.UNSPECIFIED.);
#23583=B_SPLINE_CURVE_WITH_KNOTS('',2,(#81185,#81186,#81187),
 .UNSPECIFIED.,.F.,.F.,(3,3),(0.,1.),.UNSPECIFIED.);
#23584=B_SPLINE_CURVE_WITH_KNOTS('',2,(#81195,#81196,#81197),
 .UNSPECIFIED.,.F.,.F.,(3,3),(0.,1.),.UNSPECIFIED.);
#23585=B_SPLINE_CURVE_WITH_KNOTS('',2,(#81200,#81201,#81202),
 .UNSPECIFIED.,.F.,.F.,(3,3),(0.,1.),.UNSPECIFIED.);
#23586=B_SPLINE_CURVE_WITH_KNOTS('',2,(#81210,#81211,#81212),
 .UNSPECIFIED.,.F.,.F.,(3,3),(0.,1.),.UNSPECIFIED.);
#23587=B_SPLINE_CURVE_WITH_KNOTS('',2,(#81215,#81216,#81217),
 .UNSPECIFIED.,.F.,.F.,(3,3),(0.,1.),.UNSPECIFIED.);
#23588=B_SPLINE_CURVE_WITH_KNOTS('',2,(#81224,#81225,#81226),
 .UNSPECIFIED.,.F.,.F.,(3,3),(0.,1.),.UNSPECIFIED.);
#23589=B_SPLINE_CURVE_WITH_KNOTS('',2,(#81227,#81228,#81229),
 .UNSPECIFIED.,.F.,.F.,(3,3),(0.,1.),.UNSPECIFIED.);
#23590=B_SPLINE_CURVE_WITH_KNOTS('',2,(#81238,#81239,#81240),
 .UNSPECIFIED.,.F.,.F.,(3,3),(0.,1.),.UNSPECIFIED.);
#23591=B_SPLINE_CURVE_WITH_KNOTS('',2,(#81244,#81245,#81246),
 .UNSPECIFIED.,.F.,.F.,(3,3),(0.,1.),.UNSPECIFIED.);
#23592=B_SPLINE_CURVE_WITH_KNOTS('',2,(#81255,#81256,#81257),
 .UNSPECIFIED.,.F.,.F.,(3,3),(0.,1.),.UNSPECIFIED.);
#23593=B_SPLINE_CURVE_WITH_KNOTS('',2,(#81260,#81261,#81262),
 .UNSPECIFIED.,.F.,.F.,(3,3),(0.,1.),.UNSPECIFIED.);
#23594=B_SPLINE_CURVE_WITH_KNOTS('',2,(#81270,#81271,#81272),
 .UNSPECIFIED.,.F.,.F.,(3,3),(0.,1.),.UNSPECIFIED.);
#23595=B_SPLINE_CURVE_WITH_KNOTS('',2,(#81275,#81276,#81277),
 .UNSPECIFIED.,.F.,.F.,(3,3),(0.,1.),.UNSPECIFIED.);
#23596=B_SPLINE_CURVE_WITH_KNOTS('',2,(#81285,#81286,#81287),
 .UNSPECIFIED.,.F.,.F.,(3,3),(0.,1.),.UNSPECIFIED.);
#23597=B_SPLINE_CURVE_WITH_KNOTS('',2,(#81290,#81291,#81292),
 .UNSPECIFIED.,.F.,.F.,(3,3),(0.,1.),.UNSPECIFIED.);
#23598=B_SPLINE_CURVE_WITH_KNOTS('',2,(#81300,#81301,#81302),
 .UNSPECIFIED.,.F.,.F.,(3,3),(0.,1.),.UNSPECIFIED.);
#23599=B_SPLINE_CURVE_WITH_KNOTS('',2,(#81305,#81306,#81307),
 .UNSPECIFIED.,.F.,.F.,(3,3),(0.,1.),.UNSPECIFIED.);
#23600=B_SPLINE_CURVE_WITH_KNOTS('',2,(#81315,#81316,#81317),
 .UNSPECIFIED.,.F.,.F.,(3,3),(0.,1.),.UNSPECIFIED.);
#23601=B_SPLINE_CURVE_WITH_KNOTS('',2,(#81320,#81321,#81322),
 .UNSPECIFIED.,.F.,.F.,(3,3),(0.,1.),.UNSPECIFIED.);
#23602=B_SPLINE_CURVE_WITH_KNOTS('',2,(#81330,#81331,#81332),
 .UNSPECIFIED.,.F.,.F.,(3,3),(0.,1.),.UNSPECIFIED.);
#23603=B_SPLINE_CURVE_WITH_KNOTS('',2,(#81335,#81336,#81337),
 .UNSPECIFIED.,.F.,.F.,(3,3),(0.,1.),.UNSPECIFIED.);
#23604=B_SPLINE_CURVE_WITH_KNOTS('',2,(#81345,#81346,#81347),
 .UNSPECIFIED.,.F.,.F.,(3,3),(0.,1.),.UNSPECIFIED.);
#23605=B_SPLINE_CURVE_WITH_KNOTS('',2,(#81350,#81351,#81352),
 .UNSPECIFIED.,.F.,.F.,(3,3),(0.,1.),.UNSPECIFIED.);
#23606=B_SPLINE_CURVE_WITH_KNOTS('',2,(#81360,#81361,#81362),
 .UNSPECIFIED.,.F.,.F.,(3,3),(0.,1.),.UNSPECIFIED.);
#23607=B_SPLINE_CURVE_WITH_KNOTS('',2,(#81365,#81366,#81367),
 .UNSPECIFIED.,.F.,.F.,(3,3),(0.,1.),.UNSPECIFIED.);
#23608=B_SPLINE_CURVE_WITH_KNOTS('',2,(#81375,#81376,#81377),
 .UNSPECIFIED.,.F.,.F.,(3,3),(0.,1.),.UNSPECIFIED.);
#23609=B_SPLINE_CURVE_WITH_KNOTS('',2,(#81380,#81381,#81382),
 .UNSPECIFIED.,.F.,.F.,(3,3),(0.,1.),.UNSPECIFIED.);
#23610=B_SPLINE_CURVE_WITH_KNOTS('',2,(#81390,#81391,#81392),
 .UNSPECIFIED.,.F.,.F.,(3,3),(0.,1.),.UNSPECIFIED.);
#23611=B_SPLINE_CURVE_WITH_KNOTS('',2,(#81395,#81396,#81397),
 .UNSPECIFIED.,.F.,.F.,(3,3),(0.,1.),.UNSPECIFIED.);
#23612=B_SPLINE_CURVE_WITH_KNOTS('',2,(#81404,#81405,#81406),
 .UNSPECIFIED.,.F.,.F.,(3,3),(0.,1.),.UNSPECIFIED.);
#23613=B_SPLINE_CURVE_WITH_KNOTS('',2,(#81407,#81408,#81409),
 .UNSPECIFIED.,.F.,.F.,(3,3),(0.,1.),.UNSPECIFIED.);
#23614=B_SPLINE_CURVE_WITH_KNOTS('',2,(#81427,#81428,#81429),
 .UNSPECIFIED.,.F.,.F.,(3,3),(0.,1.),.UNSPECIFIED.);
#23615=B_SPLINE_CURVE_WITH_KNOTS('',2,(#81432,#81433,#81434),
 .UNSPECIFIED.,.F.,.F.,(3,3),(0.,1.),.UNSPECIFIED.);
#23616=B_SPLINE_CURVE_WITH_KNOTS('',2,(#81442,#81443,#81444),
 .UNSPECIFIED.,.F.,.F.,(3,3),(0.,1.),.UNSPECIFIED.);
#23617=B_SPLINE_CURVE_WITH_KNOTS('',2,(#81447,#81448,#81449),
 .UNSPECIFIED.,.F.,.F.,(3,3),(0.,1.),.UNSPECIFIED.);
#23618=B_SPLINE_CURVE_WITH_KNOTS('',2,(#81463,#81464,#81465),
 .UNSPECIFIED.,.F.,.F.,(3,3),(0.,1.),.UNSPECIFIED.);
#23619=B_SPLINE_CURVE_WITH_KNOTS('',2,(#81468,#81469,#81470),
 .UNSPECIFIED.,.F.,.F.,(3,3),(0.,1.),.UNSPECIFIED.);
#23620=B_SPLINE_CURVE_WITH_KNOTS('',2,(#81478,#81479,#81480),
 .UNSPECIFIED.,.F.,.F.,(3,3),(0.,1.),.UNSPECIFIED.);
#23621=B_SPLINE_CURVE_WITH_KNOTS('',2,(#81483,#81484,#81485),
 .UNSPECIFIED.,.F.,.F.,(3,3),(0.,1.),.UNSPECIFIED.);
#23622=B_SPLINE_CURVE_WITH_KNOTS('',2,(#81511,#81512,#81513),
 .UNSPECIFIED.,.F.,.F.,(3,3),(0.,1.),.UNSPECIFIED.);
#23623=B_SPLINE_CURVE_WITH_KNOTS('',2,(#81517,#81518,#81519),
 .UNSPECIFIED.,.F.,.F.,(3,3),(0.,1.),.UNSPECIFIED.);
#23624=B_SPLINE_CURVE_WITH_KNOTS('',2,(#81528,#81529,#81530),
 .UNSPECIFIED.,.F.,.F.,(3,3),(0.,1.),.UNSPECIFIED.);
#23625=B_SPLINE_CURVE_WITH_KNOTS('',2,(#81533,#81534,#81535),
 .UNSPECIFIED.,.F.,.F.,(3,3),(0.,1.),.UNSPECIFIED.);
#23626=B_SPLINE_CURVE_WITH_KNOTS('',2,(#81543,#81544,#81545),
 .UNSPECIFIED.,.F.,.F.,(3,3),(0.,1.),.UNSPECIFIED.);
#23627=B_SPLINE_CURVE_WITH_KNOTS('',2,(#81548,#81549,#81550),
 .UNSPECIFIED.,.F.,.F.,(3,3),(0.,1.),.UNSPECIFIED.);
#23628=B_SPLINE_CURVE_WITH_KNOTS('',2,(#81558,#81559,#81560),
 .UNSPECIFIED.,.F.,.F.,(3,3),(0.,1.),.UNSPECIFIED.);
#23629=B_SPLINE_CURVE_WITH_KNOTS('',2,(#81563,#81564,#81565),
 .UNSPECIFIED.,.F.,.F.,(3,3),(0.,1.),.UNSPECIFIED.);
#23630=B_SPLINE_CURVE_WITH_KNOTS('',2,(#81573,#81574,#81575),
 .UNSPECIFIED.,.F.,.F.,(3,3),(0.,1.),.UNSPECIFIED.);
#23631=B_SPLINE_CURVE_WITH_KNOTS('',2,(#81578,#81579,#81580),
 .UNSPECIFIED.,.F.,.F.,(3,3),(0.,1.),.UNSPECIFIED.);
#23632=B_SPLINE_CURVE_WITH_KNOTS('',2,(#81588,#81589,#81590),
 .UNSPECIFIED.,.F.,.F.,(3,3),(0.,1.),.UNSPECIFIED.);
#23633=B_SPLINE_CURVE_WITH_KNOTS('',2,(#81593,#81594,#81595),
 .UNSPECIFIED.,.F.,.F.,(3,3),(0.,1.),.UNSPECIFIED.);
#23634=B_SPLINE_CURVE_WITH_KNOTS('',2,(#81603,#81604,#81605),
 .UNSPECIFIED.,.F.,.F.,(3,3),(0.,1.),.UNSPECIFIED.);
#23635=B_SPLINE_CURVE_WITH_KNOTS('',2,(#81608,#81609,#81610),
 .UNSPECIFIED.,.F.,.F.,(3,3),(0.,1.),.UNSPECIFIED.);
#23636=B_SPLINE_CURVE_WITH_KNOTS('',2,(#81617,#81618,#81619),
 .UNSPECIFIED.,.F.,.F.,(3,3),(0.,1.),.UNSPECIFIED.);
#23637=B_SPLINE_CURVE_WITH_KNOTS('',2,(#81620,#81621,#81622),
 .UNSPECIFIED.,.F.,.F.,(3,3),(0.,1.),.UNSPECIFIED.);
#23638=B_SPLINE_CURVE_WITH_KNOTS('',2,(#81631,#81632,#81633),
 .UNSPECIFIED.,.F.,.F.,(3,3),(0.,1.),.UNSPECIFIED.);
#23639=B_SPLINE_CURVE_WITH_KNOTS('',2,(#81637,#81638,#81639),
 .UNSPECIFIED.,.F.,.F.,(3,3),(0.,1.),.UNSPECIFIED.);
#23640=B_SPLINE_CURVE_WITH_KNOTS('',2,(#81648,#81649,#81650),
 .UNSPECIFIED.,.F.,.F.,(3,3),(0.,1.),.UNSPECIFIED.);
#23641=B_SPLINE_CURVE_WITH_KNOTS('',2,(#81653,#81654,#81655),
 .UNSPECIFIED.,.F.,.F.,(3,3),(0.,1.),.UNSPECIFIED.);
#23642=B_SPLINE_CURVE_WITH_KNOTS('',2,(#81663,#81664,#81665),
 .UNSPECIFIED.,.F.,.F.,(3,3),(0.,1.),.UNSPECIFIED.);
#23643=B_SPLINE_CURVE_WITH_KNOTS('',2,(#81668,#81669,#81670),
 .UNSPECIFIED.,.F.,.F.,(3,3),(0.,1.),.UNSPECIFIED.);
#23644=B_SPLINE_CURVE_WITH_KNOTS('',2,(#81678,#81679,#81680),
 .UNSPECIFIED.,.F.,.F.,(3,3),(0.,1.),.UNSPECIFIED.);
#23645=B_SPLINE_CURVE_WITH_KNOTS('',2,(#81683,#81684,#81685),
 .UNSPECIFIED.,.F.,.F.,(3,3),(0.,1.),.UNSPECIFIED.);
#23646=B_SPLINE_CURVE_WITH_KNOTS('',2,(#81693,#81694,#81695),
 .UNSPECIFIED.,.F.,.F.,(3,3),(0.,1.),.UNSPECIFIED.);
#23647=B_SPLINE_CURVE_WITH_KNOTS('',2,(#81698,#81699,#81700),
 .UNSPECIFIED.,.F.,.F.,(3,3),(0.,1.),.UNSPECIFIED.);
#23648=B_SPLINE_CURVE_WITH_KNOTS('',2,(#81708,#81709,#81710),
 .UNSPECIFIED.,.F.,.F.,(3,3),(0.,1.),.UNSPECIFIED.);
#23649=B_SPLINE_CURVE_WITH_KNOTS('',2,(#81713,#81714,#81715),
 .UNSPECIFIED.,.F.,.F.,(3,3),(0.,1.),.UNSPECIFIED.);
#23650=B_SPLINE_CURVE_WITH_KNOTS('',2,(#81723,#81724,#81725),
 .UNSPECIFIED.,.F.,.F.,(3,3),(0.,1.),.UNSPECIFIED.);
#23651=B_SPLINE_CURVE_WITH_KNOTS('',2,(#81728,#81729,#81730),
 .UNSPECIFIED.,.F.,.F.,(3,3),(0.,1.),.UNSPECIFIED.);
#23652=B_SPLINE_CURVE_WITH_KNOTS('',2,(#81738,#81739,#81740),
 .UNSPECIFIED.,.F.,.F.,(3,3),(0.,1.),.UNSPECIFIED.);
#23653=B_SPLINE_CURVE_WITH_KNOTS('',2,(#81743,#81744,#81745),
 .UNSPECIFIED.,.F.,.F.,(3,3),(0.,1.),.UNSPECIFIED.);
#23654=B_SPLINE_CURVE_WITH_KNOTS('',2,(#81753,#81754,#81755),
 .UNSPECIFIED.,.F.,.F.,(3,3),(0.,1.),.UNSPECIFIED.);
#23655=B_SPLINE_CURVE_WITH_KNOTS('',2,(#81758,#81759,#81760),
 .UNSPECIFIED.,.F.,.F.,(3,3),(0.,1.),.UNSPECIFIED.);
#23656=B_SPLINE_CURVE_WITH_KNOTS('',2,(#81768,#81769,#81770),
 .UNSPECIFIED.,.F.,.F.,(3,3),(0.,1.),.UNSPECIFIED.);
#23657=B_SPLINE_CURVE_WITH_KNOTS('',2,(#81773,#81774,#81775),
 .UNSPECIFIED.,.F.,.F.,(3,3),(0.,1.),.UNSPECIFIED.);
#23658=B_SPLINE_CURVE_WITH_KNOTS('',2,(#81783,#81784,#81785),
 .UNSPECIFIED.,.F.,.F.,(3,3),(0.,1.),.UNSPECIFIED.);
#23659=B_SPLINE_CURVE_WITH_KNOTS('',2,(#81788,#81789,#81790),
 .UNSPECIFIED.,.F.,.F.,(3,3),(0.,1.),.UNSPECIFIED.);
#23660=B_SPLINE_CURVE_WITH_KNOTS('',2,(#81797,#81798,#81799),
 .UNSPECIFIED.,.F.,.F.,(3,3),(0.,1.),.UNSPECIFIED.);
#23661=B_SPLINE_CURVE_WITH_KNOTS('',2,(#81800,#81801,#81802),
 .UNSPECIFIED.,.F.,.F.,(3,3),(0.,1.),.UNSPECIFIED.);
#23662=B_SPLINE_CURVE_WITH_KNOTS('',2,(#81813,#81814,#81815),
 .UNSPECIFIED.,.F.,.F.,(3,3),(0.,1.),.UNSPECIFIED.);
#23663=B_SPLINE_CURVE_WITH_KNOTS('',2,(#81819,#81820,#81821),
 .UNSPECIFIED.,.F.,.F.,(3,3),(0.,1.),.UNSPECIFIED.);
#23664=B_SPLINE_CURVE_WITH_KNOTS('',2,(#81830,#81831,#81832),
 .UNSPECIFIED.,.F.,.F.,(3,3),(0.,1.),.UNSPECIFIED.);
#23665=B_SPLINE_CURVE_WITH_KNOTS('',2,(#81835,#81836,#81837),
 .UNSPECIFIED.,.F.,.F.,(3,3),(0.,1.),.UNSPECIFIED.);
#23666=B_SPLINE_CURVE_WITH_KNOTS('',2,(#81845,#81846,#81847),
 .UNSPECIFIED.,.F.,.F.,(3,3),(0.,1.),.UNSPECIFIED.);
#23667=B_SPLINE_CURVE_WITH_KNOTS('',2,(#81850,#81851,#81852),
 .UNSPECIFIED.,.F.,.F.,(3,3),(0.,1.),.UNSPECIFIED.);
#23668=B_SPLINE_CURVE_WITH_KNOTS('',2,(#81860,#81861,#81862),
 .UNSPECIFIED.,.F.,.F.,(3,3),(0.,1.),.UNSPECIFIED.);
#23669=B_SPLINE_CURVE_WITH_KNOTS('',2,(#81865,#81866,#81867),
 .UNSPECIFIED.,.F.,.F.,(3,3),(0.,1.),.UNSPECIFIED.);
#23670=B_SPLINE_CURVE_WITH_KNOTS('',2,(#81875,#81876,#81877),
 .UNSPECIFIED.,.F.,.F.,(3,3),(0.,1.),.UNSPECIFIED.);
#23671=B_SPLINE_CURVE_WITH_KNOTS('',2,(#81880,#81881,#81882),
 .UNSPECIFIED.,.F.,.F.,(3,3),(0.,1.),.UNSPECIFIED.);
#23672=B_SPLINE_CURVE_WITH_KNOTS('',2,(#81890,#81891,#81892),
 .UNSPECIFIED.,.F.,.F.,(3,3),(0.,1.),.UNSPECIFIED.);
#23673=B_SPLINE_CURVE_WITH_KNOTS('',2,(#81895,#81896,#81897),
 .UNSPECIFIED.,.F.,.F.,(3,3),(0.,1.),.UNSPECIFIED.);
#23674=B_SPLINE_CURVE_WITH_KNOTS('',2,(#81905,#81906,#81907),
 .UNSPECIFIED.,.F.,.F.,(3,3),(0.,1.),.UNSPECIFIED.);
#23675=B_SPLINE_CURVE_WITH_KNOTS('',2,(#81910,#81911,#81912),
 .UNSPECIFIED.,.F.,.F.,(3,3),(0.,1.),.UNSPECIFIED.);
#23676=B_SPLINE_CURVE_WITH_KNOTS('',2,(#81919,#81920,#81921),
 .UNSPECIFIED.,.F.,.F.,(3,3),(0.,1.),.UNSPECIFIED.);
#23677=B_SPLINE_CURVE_WITH_KNOTS('',2,(#81922,#81923,#81924),
 .UNSPECIFIED.,.F.,.F.,(3,3),(0.,1.),.UNSPECIFIED.);
#23678=B_SPLINE_CURVE_WITH_KNOTS('',2,(#81933,#81934,#81935),
 .UNSPECIFIED.,.F.,.F.,(3,3),(0.,1.),.UNSPECIFIED.);
#23679=B_SPLINE_CURVE_WITH_KNOTS('',2,(#81939,#81940,#81941),
 .UNSPECIFIED.,.F.,.F.,(3,3),(0.,1.),.UNSPECIFIED.);
#23680=B_SPLINE_CURVE_WITH_KNOTS('',2,(#81950,#81951,#81952),
 .UNSPECIFIED.,.F.,.F.,(3,3),(0.,1.),.UNSPECIFIED.);
#23681=B_SPLINE_CURVE_WITH_KNOTS('',2,(#81955,#81956,#81957),
 .UNSPECIFIED.,.F.,.F.,(3,3),(0.,1.),.UNSPECIFIED.);
#23682=B_SPLINE_CURVE_WITH_KNOTS('',2,(#81965,#81966,#81967),
 .UNSPECIFIED.,.F.,.F.,(3,3),(0.,1.),.UNSPECIFIED.);
#23683=B_SPLINE_CURVE_WITH_KNOTS('',2,(#81970,#81971,#81972),
 .UNSPECIFIED.,.F.,.F.,(3,3),(0.,1.),.UNSPECIFIED.);
#23684=B_SPLINE_CURVE_WITH_KNOTS('',2,(#81980,#81981,#81982),
 .UNSPECIFIED.,.F.,.F.,(3,3),(0.,1.),.UNSPECIFIED.);
#23685=B_SPLINE_CURVE_WITH_KNOTS('',2,(#81985,#81986,#81987),
 .UNSPECIFIED.,.F.,.F.,(3,3),(0.,1.),.UNSPECIFIED.);
#23686=B_SPLINE_CURVE_WITH_KNOTS('',2,(#81995,#81996,#81997),
 .UNSPECIFIED.,.F.,.F.,(3,3),(0.,1.),.UNSPECIFIED.);
#23687=B_SPLINE_CURVE_WITH_KNOTS('',2,(#82000,#82001,#82002),
 .UNSPECIFIED.,.F.,.F.,(3,3),(0.,1.),.UNSPECIFIED.);
#23688=B_SPLINE_CURVE_WITH_KNOTS('',2,(#82010,#82011,#82012),
 .UNSPECIFIED.,.F.,.F.,(3,3),(0.,1.),.UNSPECIFIED.);
#23689=B_SPLINE_CURVE_WITH_KNOTS('',2,(#82015,#82016,#82017),
 .UNSPECIFIED.,.F.,.F.,(3,3),(0.,1.),.UNSPECIFIED.);
#23690=B_SPLINE_CURVE_WITH_KNOTS('',2,(#82025,#82026,#82027),
 .UNSPECIFIED.,.F.,.F.,(3,3),(0.,1.),.UNSPECIFIED.);
#23691=B_SPLINE_CURVE_WITH_KNOTS('',2,(#82030,#82031,#82032),
 .UNSPECIFIED.,.F.,.F.,(3,3),(0.,1.),.UNSPECIFIED.);
#23692=B_SPLINE_CURVE_WITH_KNOTS('',2,(#82040,#82041,#82042),
 .UNSPECIFIED.,.F.,.F.,(3,3),(0.,1.),.UNSPECIFIED.);
#23693=B_SPLINE_CURVE_WITH_KNOTS('',2,(#82045,#82046,#82047),
 .UNSPECIFIED.,.F.,.F.,(3,3),(0.,1.),.UNSPECIFIED.);
#23694=B_SPLINE_CURVE_WITH_KNOTS('',2,(#82055,#82056,#82057),
 .UNSPECIFIED.,.F.,.F.,(3,3),(0.,1.),.UNSPECIFIED.);
#23695=B_SPLINE_CURVE_WITH_KNOTS('',2,(#82060,#82061,#82062),
 .UNSPECIFIED.,.F.,.F.,(3,3),(0.,1.),.UNSPECIFIED.);
#23696=B_SPLINE_CURVE_WITH_KNOTS('',2,(#82070,#82071,#82072),
 .UNSPECIFIED.,.F.,.F.,(3,3),(0.,1.),.UNSPECIFIED.);
#23697=B_SPLINE_CURVE_WITH_KNOTS('',2,(#82075,#82076,#82077),
 .UNSPECIFIED.,.F.,.F.,(3,3),(0.,1.),.UNSPECIFIED.);
#23698=B_SPLINE_CURVE_WITH_KNOTS('',2,(#82085,#82086,#82087),
 .UNSPECIFIED.,.F.,.F.,(3,3),(0.,1.),.UNSPECIFIED.);
#23699=B_SPLINE_CURVE_WITH_KNOTS('',2,(#82090,#82091,#82092),
 .UNSPECIFIED.,.F.,.F.,(3,3),(0.,1.),.UNSPECIFIED.);
#23700=B_SPLINE_CURVE_WITH_KNOTS('',2,(#82099,#82100,#82101),
 .UNSPECIFIED.,.F.,.F.,(3,3),(0.,1.),.UNSPECIFIED.);
#23701=B_SPLINE_CURVE_WITH_KNOTS('',2,(#82102,#82103,#82104),
 .UNSPECIFIED.,.F.,.F.,(3,3),(0.,1.),.UNSPECIFIED.);
#23702=B_SPLINE_CURVE_WITH_KNOTS('',2,(#82122,#82123,#82124),
 .UNSPECIFIED.,.F.,.F.,(3,3),(0.,1.),.UNSPECIFIED.);
#23703=B_SPLINE_CURVE_WITH_KNOTS('',2,(#82127,#82128,#82129),
 .UNSPECIFIED.,.F.,.F.,(3,3),(0.,1.),.UNSPECIFIED.);
#23704=B_SPLINE_CURVE_WITH_KNOTS('',2,(#82137,#82138,#82139),
 .UNSPECIFIED.,.F.,.F.,(3,3),(0.,1.),.UNSPECIFIED.);
#23705=B_SPLINE_CURVE_WITH_KNOTS('',2,(#82142,#82143,#82144),
 .UNSPECIFIED.,.F.,.F.,(3,3),(0.,1.),.UNSPECIFIED.);
#23706=B_SPLINE_CURVE_WITH_KNOTS('',2,(#82158,#82159,#82160),
 .UNSPECIFIED.,.F.,.F.,(3,3),(0.,1.),.UNSPECIFIED.);
#23707=B_SPLINE_CURVE_WITH_KNOTS('',2,(#82163,#82164,#82165),
 .UNSPECIFIED.,.F.,.F.,(3,3),(0.,1.),.UNSPECIFIED.);
#23708=B_SPLINE_CURVE_WITH_KNOTS('',2,(#82173,#82174,#82175),
 .UNSPECIFIED.,.F.,.F.,(3,3),(0.,1.),.UNSPECIFIED.);
#23709=B_SPLINE_CURVE_WITH_KNOTS('',2,(#82178,#82179,#82180),
 .UNSPECIFIED.,.F.,.F.,(3,3),(0.,1.),.UNSPECIFIED.);
#23710=B_SPLINE_CURVE_WITH_KNOTS('',2,(#82206,#82207,#82208),
 .UNSPECIFIED.,.F.,.F.,(3,3),(0.,1.),.UNSPECIFIED.);
#23711=B_SPLINE_CURVE_WITH_KNOTS('',2,(#82212,#82213,#82214),
 .UNSPECIFIED.,.F.,.F.,(3,3),(0.,1.),.UNSPECIFIED.);
#23712=B_SPLINE_CURVE_WITH_KNOTS('',2,(#82223,#82224,#82225),
 .UNSPECIFIED.,.F.,.F.,(3,3),(0.,1.),.UNSPECIFIED.);
#23713=B_SPLINE_CURVE_WITH_KNOTS('',2,(#82228,#82229,#82230),
 .UNSPECIFIED.,.F.,.F.,(3,3),(0.,1.),.UNSPECIFIED.);
#23714=B_SPLINE_CURVE_WITH_KNOTS('',2,(#82238,#82239,#82240),
 .UNSPECIFIED.,.F.,.F.,(3,3),(0.,1.),.UNSPECIFIED.);
#23715=B_SPLINE_CURVE_WITH_KNOTS('',2,(#82243,#82244,#82245),
 .UNSPECIFIED.,.F.,.F.,(3,3),(0.,1.),.UNSPECIFIED.);
#23716=B_SPLINE_CURVE_WITH_KNOTS('',2,(#82253,#82254,#82255),
 .UNSPECIFIED.,.F.,.F.,(3,3),(0.,1.),.UNSPECIFIED.);
#23717=B_SPLINE_CURVE_WITH_KNOTS('',2,(#82258,#82259,#82260),
 .UNSPECIFIED.,.F.,.F.,(3,3),(0.,1.),.UNSPECIFIED.);
#23718=B_SPLINE_CURVE_WITH_KNOTS('',2,(#82268,#82269,#82270),
 .UNSPECIFIED.,.F.,.F.,(3,3),(0.,1.),.UNSPECIFIED.);
#23719=B_SPLINE_CURVE_WITH_KNOTS('',2,(#82273,#82274,#82275),
 .UNSPECIFIED.,.F.,.F.,(3,3),(0.,1.),.UNSPECIFIED.);
#23720=B_SPLINE_CURVE_WITH_KNOTS('',2,(#82283,#82284,#82285),
 .UNSPECIFIED.,.F.,.F.,(3,3),(0.,1.),.UNSPECIFIED.);
#23721=B_SPLINE_CURVE_WITH_KNOTS('',2,(#82288,#82289,#82290),
 .UNSPECIFIED.,.F.,.F.,(3,3),(0.,1.),.UNSPECIFIED.);
#23722=B_SPLINE_CURVE_WITH_KNOTS('',2,(#82298,#82299,#82300),
 .UNSPECIFIED.,.F.,.F.,(3,3),(0.,1.),.UNSPECIFIED.);
#23723=B_SPLINE_CURVE_WITH_KNOTS('',2,(#82303,#82304,#82305),
 .UNSPECIFIED.,.F.,.F.,(3,3),(0.,1.),.UNSPECIFIED.);
#23724=B_SPLINE_CURVE_WITH_KNOTS('',2,(#82312,#82313,#82314),
 .UNSPECIFIED.,.F.,.F.,(3,3),(0.,1.),.UNSPECIFIED.);
#23725=B_SPLINE_CURVE_WITH_KNOTS('',2,(#82315,#82316,#82317),
 .UNSPECIFIED.,.F.,.F.,(3,3),(0.,1.),.UNSPECIFIED.);
#23726=B_SPLINE_CURVE_WITH_KNOTS('',2,(#82326,#82327,#82328),
 .UNSPECIFIED.,.F.,.F.,(3,3),(0.,1.),.UNSPECIFIED.);
#23727=B_SPLINE_CURVE_WITH_KNOTS('',2,(#82332,#82333,#82334),
 .UNSPECIFIED.,.F.,.F.,(3,3),(0.,1.),.UNSPECIFIED.);
#23728=B_SPLINE_CURVE_WITH_KNOTS('',2,(#82343,#82344,#82345),
 .UNSPECIFIED.,.F.,.F.,(3,3),(0.,1.),.UNSPECIFIED.);
#23729=B_SPLINE_CURVE_WITH_KNOTS('',2,(#82348,#82349,#82350),
 .UNSPECIFIED.,.F.,.F.,(3,3),(0.,1.),.UNSPECIFIED.);
#23730=B_SPLINE_CURVE_WITH_KNOTS('',2,(#82358,#82359,#82360),
 .UNSPECIFIED.,.F.,.F.,(3,3),(0.,1.),.UNSPECIFIED.);
#23731=B_SPLINE_CURVE_WITH_KNOTS('',2,(#82363,#82364,#82365),
 .UNSPECIFIED.,.F.,.F.,(3,3),(0.,1.),.UNSPECIFIED.);
#23732=B_SPLINE_CURVE_WITH_KNOTS('',2,(#82373,#82374,#82375),
 .UNSPECIFIED.,.F.,.F.,(3,3),(0.,1.),.UNSPECIFIED.);
#23733=B_SPLINE_CURVE_WITH_KNOTS('',2,(#82378,#82379,#82380),
 .UNSPECIFIED.,.F.,.F.,(3,3),(0.,1.),.UNSPECIFIED.);
#23734=B_SPLINE_CURVE_WITH_KNOTS('',2,(#82388,#82389,#82390),
 .UNSPECIFIED.,.F.,.F.,(3,3),(0.,1.),.UNSPECIFIED.);
#23735=B_SPLINE_CURVE_WITH_KNOTS('',2,(#82393,#82394,#82395),
 .UNSPECIFIED.,.F.,.F.,(3,3),(0.,1.),.UNSPECIFIED.);
#23736=B_SPLINE_CURVE_WITH_KNOTS('',2,(#82403,#82404,#82405),
 .UNSPECIFIED.,.F.,.F.,(3,3),(0.,1.),.UNSPECIFIED.);
#23737=B_SPLINE_CURVE_WITH_KNOTS('',2,(#82408,#82409,#82410),
 .UNSPECIFIED.,.F.,.F.,(3,3),(0.,1.),.UNSPECIFIED.);
#23738=B_SPLINE_CURVE_WITH_KNOTS('',2,(#82418,#82419,#82420),
 .UNSPECIFIED.,.F.,.F.,(3,3),(0.,1.),.UNSPECIFIED.);
#23739=B_SPLINE_CURVE_WITH_KNOTS('',2,(#82423,#82424,#82425),
 .UNSPECIFIED.,.F.,.F.,(3,3),(0.,1.),.UNSPECIFIED.);
#23740=B_SPLINE_CURVE_WITH_KNOTS('',2,(#82433,#82434,#82435),
 .UNSPECIFIED.,.F.,.F.,(3,3),(0.,1.),.UNSPECIFIED.);
#23741=B_SPLINE_CURVE_WITH_KNOTS('',2,(#82438,#82439,#82440),
 .UNSPECIFIED.,.F.,.F.,(3,3),(0.,1.),.UNSPECIFIED.);
#23742=B_SPLINE_CURVE_WITH_KNOTS('',2,(#82448,#82449,#82450),
 .UNSPECIFIED.,.F.,.F.,(3,3),(0.,1.),.UNSPECIFIED.);
#23743=B_SPLINE_CURVE_WITH_KNOTS('',2,(#82453,#82454,#82455),
 .UNSPECIFIED.,.F.,.F.,(3,3),(0.,1.),.UNSPECIFIED.);
#23744=B_SPLINE_CURVE_WITH_KNOTS('',2,(#82463,#82464,#82465),
 .UNSPECIFIED.,.F.,.F.,(3,3),(0.,1.),.UNSPECIFIED.);
#23745=B_SPLINE_CURVE_WITH_KNOTS('',2,(#82468,#82469,#82470),
 .UNSPECIFIED.,.F.,.F.,(3,3),(0.,1.),.UNSPECIFIED.);
#23746=B_SPLINE_CURVE_WITH_KNOTS('',2,(#82478,#82479,#82480),
 .UNSPECIFIED.,.F.,.F.,(3,3),(0.,1.),.UNSPECIFIED.);
#23747=B_SPLINE_CURVE_WITH_KNOTS('',2,(#82483,#82484,#82485),
 .UNSPECIFIED.,.F.,.F.,(3,3),(0.,1.),.UNSPECIFIED.);
#23748=B_SPLINE_CURVE_WITH_KNOTS('',2,(#82492,#82493,#82494),
 .UNSPECIFIED.,.F.,.F.,(3,3),(0.,1.),.UNSPECIFIED.);
#23749=B_SPLINE_CURVE_WITH_KNOTS('',2,(#82495,#82496,#82497),
 .UNSPECIFIED.,.F.,.F.,(3,3),(0.,1.),.UNSPECIFIED.);
#23750=B_SPLINE_CURVE_WITH_KNOTS('',2,(#82507,#82508,#82509),
 .UNSPECIFIED.,.F.,.F.,(3,3),(0.,1.),.UNSPECIFIED.);
#23751=B_SPLINE_CURVE_WITH_KNOTS('',2,(#82513,#82514,#82515),
 .UNSPECIFIED.,.F.,.F.,(3,3),(0.,1.),.UNSPECIFIED.);
#23752=B_SPLINE_CURVE_WITH_KNOTS('',2,(#82524,#82525,#82526),
 .UNSPECIFIED.,.F.,.F.,(3,3),(0.,1.),.UNSPECIFIED.);
#23753=B_SPLINE_CURVE_WITH_KNOTS('',2,(#82529,#82530,#82531),
 .UNSPECIFIED.,.F.,.F.,(3,3),(0.,1.),.UNSPECIFIED.);
#23754=B_SPLINE_CURVE_WITH_KNOTS('',2,(#82539,#82540,#82541),
 .UNSPECIFIED.,.F.,.F.,(3,3),(0.,1.),.UNSPECIFIED.);
#23755=B_SPLINE_CURVE_WITH_KNOTS('',2,(#82544,#82545,#82546),
 .UNSPECIFIED.,.F.,.F.,(3,3),(0.,1.),.UNSPECIFIED.);
#23756=B_SPLINE_CURVE_WITH_KNOTS('',2,(#82554,#82555,#82556),
 .UNSPECIFIED.,.F.,.F.,(3,3),(0.,1.),.UNSPECIFIED.);
#23757=B_SPLINE_CURVE_WITH_KNOTS('',2,(#82559,#82560,#82561),
 .UNSPECIFIED.,.F.,.F.,(3,3),(0.,1.),.UNSPECIFIED.);
#23758=B_SPLINE_CURVE_WITH_KNOTS('',2,(#82569,#82570,#82571),
 .UNSPECIFIED.,.F.,.F.,(3,3),(0.,1.),.UNSPECIFIED.);
#23759=B_SPLINE_CURVE_WITH_KNOTS('',2,(#82574,#82575,#82576),
 .UNSPECIFIED.,.F.,.F.,(3,3),(0.,1.),.UNSPECIFIED.);
#23760=B_SPLINE_CURVE_WITH_KNOTS('',2,(#82584,#82585,#82586),
 .UNSPECIFIED.,.F.,.F.,(3,3),(0.,1.),.UNSPECIFIED.);
#23761=B_SPLINE_CURVE_WITH_KNOTS('',2,(#82589,#82590,#82591),
 .UNSPECIFIED.,.F.,.F.,(3,3),(0.,1.),.UNSPECIFIED.);
#23762=B_SPLINE_CURVE_WITH_KNOTS('',2,(#82599,#82600,#82601),
 .UNSPECIFIED.,.F.,.F.,(3,3),(0.,1.),.UNSPECIFIED.);
#23763=B_SPLINE_CURVE_WITH_KNOTS('',2,(#82604,#82605,#82606),
 .UNSPECIFIED.,.F.,.F.,(3,3),(0.,1.),.UNSPECIFIED.);
#23764=B_SPLINE_CURVE_WITH_KNOTS('',2,(#82614,#82615,#82616),
 .UNSPECIFIED.,.F.,.F.,(3,3),(0.,1.),.UNSPECIFIED.);
#23765=B_SPLINE_CURVE_WITH_KNOTS('',2,(#82619,#82620,#82621),
 .UNSPECIFIED.,.F.,.F.,(3,3),(0.,1.),.UNSPECIFIED.);
#23766=B_SPLINE_CURVE_WITH_KNOTS('',2,(#82629,#82630,#82631),
 .UNSPECIFIED.,.F.,.F.,(3,3),(0.,1.),.UNSPECIFIED.);
#23767=B_SPLINE_CURVE_WITH_KNOTS('',2,(#82634,#82635,#82636),
 .UNSPECIFIED.,.F.,.F.,(3,3),(0.,1.),.UNSPECIFIED.);
#23768=B_SPLINE_CURVE_WITH_KNOTS('',2,(#82650,#82651,#82652),
 .UNSPECIFIED.,.F.,.F.,(3,3),(0.,1.),.UNSPECIFIED.);
#23769=B_SPLINE_CURVE_WITH_KNOTS('',2,(#82655,#82656,#82657),
 .UNSPECIFIED.,.F.,.F.,(3,3),(0.,1.),.UNSPECIFIED.);
#23770=B_SPLINE_CURVE_WITH_KNOTS('',2,(#82665,#82666,#82667),
 .UNSPECIFIED.,.F.,.F.,(3,3),(0.,1.),.UNSPECIFIED.);
#23771=B_SPLINE_CURVE_WITH_KNOTS('',2,(#82670,#82671,#82672),
 .UNSPECIFIED.,.F.,.F.,(3,3),(0.,1.),.UNSPECIFIED.);
#23772=B_SPLINE_CURVE_WITH_KNOTS('',2,(#82680,#82681,#82682),
 .UNSPECIFIED.,.F.,.F.,(3,3),(0.,1.),.UNSPECIFIED.);
#23773=B_SPLINE_CURVE_WITH_KNOTS('',2,(#82685,#82686,#82687),
 .UNSPECIFIED.,.F.,.F.,(3,3),(0.,1.),.UNSPECIFIED.);
#23774=B_SPLINE_CURVE_WITH_KNOTS('',2,(#82695,#82696,#82697),
 .UNSPECIFIED.,.F.,.F.,(3,3),(0.,1.),.UNSPECIFIED.);
#23775=B_SPLINE_CURVE_WITH_KNOTS('',2,(#82700,#82701,#82702),
 .UNSPECIFIED.,.F.,.F.,(3,3),(0.,1.),.UNSPECIFIED.);
#23776=B_SPLINE_CURVE_WITH_KNOTS('',2,(#82710,#82711,#82712),
 .UNSPECIFIED.,.F.,.F.,(3,3),(0.,1.),.UNSPECIFIED.);
#23777=B_SPLINE_CURVE_WITH_KNOTS('',2,(#82715,#82716,#82717),
 .UNSPECIFIED.,.F.,.F.,(3,3),(0.,1.),.UNSPECIFIED.);
#23778=B_SPLINE_CURVE_WITH_KNOTS('',2,(#82725,#82726,#82727),
 .UNSPECIFIED.,.F.,.F.,(3,3),(0.,1.),.UNSPECIFIED.);
#23779=B_SPLINE_CURVE_WITH_KNOTS('',2,(#82730,#82731,#82732),
 .UNSPECIFIED.,.F.,.F.,(3,3),(0.,1.),.UNSPECIFIED.);
#23780=B_SPLINE_CURVE_WITH_KNOTS('',2,(#82740,#82741,#82742),
 .UNSPECIFIED.,.F.,.F.,(3,3),(0.,1.),.UNSPECIFIED.);
#23781=B_SPLINE_CURVE_WITH_KNOTS('',2,(#82745,#82746,#82747),
 .UNSPECIFIED.,.F.,.F.,(3,3),(0.,1.),.UNSPECIFIED.);
#23782=B_SPLINE_CURVE_WITH_KNOTS('',2,(#82755,#82756,#82757),
 .UNSPECIFIED.,.F.,.F.,(3,3),(0.,1.),.UNSPECIFIED.);
#23783=B_SPLINE_CURVE_WITH_KNOTS('',2,(#82760,#82761,#82762),
 .UNSPECIFIED.,.F.,.F.,(3,3),(0.,1.),.UNSPECIFIED.);
#23784=B_SPLINE_CURVE_WITH_KNOTS('',2,(#82770,#82771,#82772),
 .UNSPECIFIED.,.F.,.F.,(3,3),(0.,1.),.UNSPECIFIED.);
#23785=B_SPLINE_CURVE_WITH_KNOTS('',2,(#82775,#82776,#82777),
 .UNSPECIFIED.,.F.,.F.,(3,3),(0.,1.),.UNSPECIFIED.);
#23786=B_SPLINE_CURVE_WITH_KNOTS('',2,(#82803,#82804,#82805),
 .UNSPECIFIED.,.F.,.F.,(3,3),(0.,1.),.UNSPECIFIED.);
#23787=B_SPLINE_CURVE_WITH_KNOTS('',2,(#82809,#82810,#82811),
 .UNSPECIFIED.,.F.,.F.,(3,3),(0.,1.),.UNSPECIFIED.);
#23788=B_SPLINE_CURVE_WITH_KNOTS('',2,(#82820,#82821,#82822),
 .UNSPECIFIED.,.F.,.F.,(3,3),(0.,1.),.UNSPECIFIED.);
#23789=B_SPLINE_CURVE_WITH_KNOTS('',2,(#82825,#82826,#82827),
 .UNSPECIFIED.,.F.,.F.,(3,3),(0.,1.),.UNSPECIFIED.);
#23790=B_SPLINE_CURVE_WITH_KNOTS('',2,(#82835,#82836,#82837),
 .UNSPECIFIED.,.F.,.F.,(3,3),(0.,1.),.UNSPECIFIED.);
#23791=B_SPLINE_CURVE_WITH_KNOTS('',2,(#82840,#82841,#82842),
 .UNSPECIFIED.,.F.,.F.,(3,3),(0.,1.),.UNSPECIFIED.);
#23792=B_SPLINE_CURVE_WITH_KNOTS('',2,(#82850,#82851,#82852),
 .UNSPECIFIED.,.F.,.F.,(3,3),(0.,1.),.UNSPECIFIED.);
#23793=B_SPLINE_CURVE_WITH_KNOTS('',2,(#82855,#82856,#82857),
 .UNSPECIFIED.,.F.,.F.,(3,3),(0.,1.),.UNSPECIFIED.);
#23794=B_SPLINE_CURVE_WITH_KNOTS('',2,(#82865,#82866,#82867),
 .UNSPECIFIED.,.F.,.F.,(3,3),(0.,1.),.UNSPECIFIED.);
#23795=B_SPLINE_CURVE_WITH_KNOTS('',2,(#82870,#82871,#82872),
 .UNSPECIFIED.,.F.,.F.,(3,3),(0.,1.),.UNSPECIFIED.);
#23796=B_SPLINE_CURVE_WITH_KNOTS('',2,(#82880,#82881,#82882),
 .UNSPECIFIED.,.F.,.F.,(3,3),(0.,1.),.UNSPECIFIED.);
#23797=B_SPLINE_CURVE_WITH_KNOTS('',2,(#82885,#82886,#82887),
 .UNSPECIFIED.,.F.,.F.,(3,3),(0.,1.),.UNSPECIFIED.);
#23798=B_SPLINE_CURVE_WITH_KNOTS('',2,(#82895,#82896,#82897),
 .UNSPECIFIED.,.F.,.F.,(3,3),(0.,1.),.UNSPECIFIED.);
#23799=B_SPLINE_CURVE_WITH_KNOTS('',2,(#82900,#82901,#82902),
 .UNSPECIFIED.,.F.,.F.,(3,3),(0.,1.),.UNSPECIFIED.);
#23800=B_SPLINE_CURVE_WITH_KNOTS('',2,(#82909,#82910,#82911),
 .UNSPECIFIED.,.F.,.F.,(3,3),(0.,1.),.UNSPECIFIED.);
#23801=B_SPLINE_CURVE_WITH_KNOTS('',2,(#82912,#82913,#82914),
 .UNSPECIFIED.,.F.,.F.,(3,3),(0.,1.),.UNSPECIFIED.);
#23802=B_SPLINE_CURVE_WITH_KNOTS('',2,(#82923,#82924,#82925),
 .UNSPECIFIED.,.F.,.F.,(3,3),(0.,1.),.UNSPECIFIED.);
#23803=B_SPLINE_CURVE_WITH_KNOTS('',2,(#82929,#82930,#82931),
 .UNSPECIFIED.,.F.,.F.,(3,3),(0.,1.),.UNSPECIFIED.);
#23804=B_SPLINE_CURVE_WITH_KNOTS('',2,(#82940,#82941,#82942),
 .UNSPECIFIED.,.F.,.F.,(3,3),(0.,1.),.UNSPECIFIED.);
#23805=B_SPLINE_CURVE_WITH_KNOTS('',2,(#82945,#82946,#82947),
 .UNSPECIFIED.,.F.,.F.,(3,3),(0.,1.),.UNSPECIFIED.);
#23806=B_SPLINE_CURVE_WITH_KNOTS('',2,(#82955,#82956,#82957),
 .UNSPECIFIED.,.F.,.F.,(3,3),(0.,1.),.UNSPECIFIED.);
#23807=B_SPLINE_CURVE_WITH_KNOTS('',2,(#82960,#82961,#82962),
 .UNSPECIFIED.,.F.,.F.,(3,3),(0.,1.),.UNSPECIFIED.);
#23808=B_SPLINE_CURVE_WITH_KNOTS('',2,(#82970,#82971,#82972),
 .UNSPECIFIED.,.F.,.F.,(3,3),(0.,1.),.UNSPECIFIED.);
#23809=B_SPLINE_CURVE_WITH_KNOTS('',2,(#82975,#82976,#82977),
 .UNSPECIFIED.,.F.,.F.,(3,3),(0.,1.),.UNSPECIFIED.);
#23810=B_SPLINE_CURVE_WITH_KNOTS('',2,(#82985,#82986,#82987),
 .UNSPECIFIED.,.F.,.F.,(3,3),(0.,1.),.UNSPECIFIED.);
#23811=B_SPLINE_CURVE_WITH_KNOTS('',2,(#82990,#82991,#82992),
 .UNSPECIFIED.,.F.,.F.,(3,3),(0.,1.),.UNSPECIFIED.);
#23812=B_SPLINE_CURVE_WITH_KNOTS('',2,(#83000,#83001,#83002),
 .UNSPECIFIED.,.F.,.F.,(3,3),(0.,1.),.UNSPECIFIED.);
#23813=B_SPLINE_CURVE_WITH_KNOTS('',2,(#83005,#83006,#83007),
 .UNSPECIFIED.,.F.,.F.,(3,3),(0.,1.),.UNSPECIFIED.);
#23814=B_SPLINE_CURVE_WITH_KNOTS('',2,(#83015,#83016,#83017),
 .UNSPECIFIED.,.F.,.F.,(3,3),(0.,1.),.UNSPECIFIED.);
#23815=B_SPLINE_CURVE_WITH_KNOTS('',2,(#83020,#83021,#83022),
 .UNSPECIFIED.,.F.,.F.,(3,3),(0.,1.),.UNSPECIFIED.);
#23816=B_SPLINE_CURVE_WITH_KNOTS('',2,(#83030,#83031,#83032),
 .UNSPECIFIED.,.F.,.F.,(3,3),(0.,1.),.UNSPECIFIED.);
#23817=B_SPLINE_CURVE_WITH_KNOTS('',2,(#83035,#83036,#83037),
 .UNSPECIFIED.,.F.,.F.,(3,3),(0.,1.),.UNSPECIFIED.);
#23818=B_SPLINE_CURVE_WITH_KNOTS('',2,(#83045,#83046,#83047),
 .UNSPECIFIED.,.F.,.F.,(3,3),(0.,1.),.UNSPECIFIED.);
#23819=B_SPLINE_CURVE_WITH_KNOTS('',2,(#83050,#83051,#83052),
 .UNSPECIFIED.,.F.,.F.,(3,3),(0.,1.),.UNSPECIFIED.);
#23820=B_SPLINE_CURVE_WITH_KNOTS('',2,(#83060,#83061,#83062),
 .UNSPECIFIED.,.F.,.F.,(3,3),(0.,1.),.UNSPECIFIED.);
#23821=B_SPLINE_CURVE_WITH_KNOTS('',2,(#83065,#83066,#83067),
 .UNSPECIFIED.,.F.,.F.,(3,3),(0.,1.),.UNSPECIFIED.);
#23822=B_SPLINE_CURVE_WITH_KNOTS('',2,(#83075,#83076,#83077),
 .UNSPECIFIED.,.F.,.F.,(3,3),(0.,1.),.UNSPECIFIED.);
#23823=B_SPLINE_CURVE_WITH_KNOTS('',2,(#83080,#83081,#83082),
 .UNSPECIFIED.,.F.,.F.,(3,3),(0.,1.),.UNSPECIFIED.);
#23824=B_SPLINE_CURVE_WITH_KNOTS('',2,(#83089,#83090,#83091),
 .UNSPECIFIED.,.F.,.F.,(3,3),(0.,1.),.UNSPECIFIED.);
#23825=B_SPLINE_CURVE_WITH_KNOTS('',2,(#83092,#83093,#83094),
 .UNSPECIFIED.,.F.,.F.,(3,3),(0.,1.),.UNSPECIFIED.);
#23826=B_SPLINE_CURVE_WITH_KNOTS('',2,(#83104,#83105,#83106),
 .UNSPECIFIED.,.F.,.F.,(3,3),(0.,1.),.UNSPECIFIED.);
#23827=B_SPLINE_CURVE_WITH_KNOTS('',2,(#83110,#83111,#83112),
 .UNSPECIFIED.,.F.,.F.,(3,3),(0.,1.),.UNSPECIFIED.);
#23828=B_SPLINE_CURVE_WITH_KNOTS('',2,(#83121,#83122,#83123),
 .UNSPECIFIED.,.F.,.F.,(3,3),(0.,1.),.UNSPECIFIED.);
#23829=B_SPLINE_CURVE_WITH_KNOTS('',2,(#83126,#83127,#83128),
 .UNSPECIFIED.,.F.,.F.,(3,3),(0.,1.),.UNSPECIFIED.);
#23830=B_SPLINE_CURVE_WITH_KNOTS('',2,(#83136,#83137,#83138),
 .UNSPECIFIED.,.F.,.F.,(3,3),(0.,1.),.UNSPECIFIED.);
#23831=B_SPLINE_CURVE_WITH_KNOTS('',2,(#83141,#83142,#83143),
 .UNSPECIFIED.,.F.,.F.,(3,3),(0.,1.),.UNSPECIFIED.);
#23832=B_SPLINE_CURVE_WITH_KNOTS('',2,(#83151,#83152,#83153),
 .UNSPECIFIED.,.F.,.F.,(3,3),(0.,1.),.UNSPECIFIED.);
#23833=B_SPLINE_CURVE_WITH_KNOTS('',2,(#83156,#83157,#83158),
 .UNSPECIFIED.,.F.,.F.,(3,3),(0.,1.),.UNSPECIFIED.);
#23834=B_SPLINE_CURVE_WITH_KNOTS('',2,(#83166,#83167,#83168),
 .UNSPECIFIED.,.F.,.F.,(3,3),(0.,1.),.UNSPECIFIED.);
#23835=B_SPLINE_CURVE_WITH_KNOTS('',2,(#83171,#83172,#83173),
 .UNSPECIFIED.,.F.,.F.,(3,3),(0.,1.),.UNSPECIFIED.);
#23836=B_SPLINE_CURVE_WITH_KNOTS('',2,(#83181,#83182,#83183),
 .UNSPECIFIED.,.F.,.F.,(3,3),(0.,1.),.UNSPECIFIED.);
#23837=B_SPLINE_CURVE_WITH_KNOTS('',2,(#83186,#83187,#83188),
 .UNSPECIFIED.,.F.,.F.,(3,3),(0.,1.),.UNSPECIFIED.);
#23838=B_SPLINE_CURVE_WITH_KNOTS('',2,(#83196,#83197,#83198),
 .UNSPECIFIED.,.F.,.F.,(3,3),(0.,1.),.UNSPECIFIED.);
#23839=B_SPLINE_CURVE_WITH_KNOTS('',2,(#83201,#83202,#83203),
 .UNSPECIFIED.,.F.,.F.,(3,3),(0.,1.),.UNSPECIFIED.);
#23840=B_SPLINE_CURVE_WITH_KNOTS('',2,(#83211,#83212,#83213),
 .UNSPECIFIED.,.F.,.F.,(3,3),(0.,1.),.UNSPECIFIED.);
#23841=B_SPLINE_CURVE_WITH_KNOTS('',2,(#83216,#83217,#83218),
 .UNSPECIFIED.,.F.,.F.,(3,3),(0.,1.),.UNSPECIFIED.);
#23842=B_SPLINE_CURVE_WITH_KNOTS('',2,(#83226,#83227,#83228),
 .UNSPECIFIED.,.F.,.F.,(3,3),(0.,1.),.UNSPECIFIED.);
#23843=B_SPLINE_CURVE_WITH_KNOTS('',2,(#83231,#83232,#83233),
 .UNSPECIFIED.,.F.,.F.,(3,3),(0.,1.),.UNSPECIFIED.);
#23844=B_SPLINE_CURVE_WITH_KNOTS('',2,(#83241,#83242,#83243),
 .UNSPECIFIED.,.F.,.F.,(3,3),(0.,1.),.UNSPECIFIED.);
#23845=B_SPLINE_CURVE_WITH_KNOTS('',2,(#83246,#83247,#83248),
 .UNSPECIFIED.,.F.,.F.,(3,3),(0.,1.),.UNSPECIFIED.);
#23846=B_SPLINE_CURVE_WITH_KNOTS('',2,(#83256,#83257,#83258),
 .UNSPECIFIED.,.F.,.F.,(3,3),(0.,1.),.UNSPECIFIED.);
#23847=B_SPLINE_CURVE_WITH_KNOTS('',2,(#83261,#83262,#83263),
 .UNSPECIFIED.,.F.,.F.,(3,3),(0.,1.),.UNSPECIFIED.);
#23848=B_SPLINE_CURVE_WITH_KNOTS('',2,(#83271,#83272,#83273),
 .UNSPECIFIED.,.F.,.F.,(3,3),(0.,1.),.UNSPECIFIED.);
#23849=B_SPLINE_CURVE_WITH_KNOTS('',2,(#83276,#83277,#83278),
 .UNSPECIFIED.,.F.,.F.,(3,3),(0.,1.),.UNSPECIFIED.);
#23850=B_SPLINE_CURVE_WITH_KNOTS('',2,(#83292,#83293,#83294),
 .UNSPECIFIED.,.F.,.F.,(3,3),(0.,1.),.UNSPECIFIED.);
#23851=B_SPLINE_CURVE_WITH_KNOTS('',2,(#83297,#83298,#83299),
 .UNSPECIFIED.,.F.,.F.,(3,3),(0.,1.),.UNSPECIFIED.);
#23852=B_SPLINE_CURVE_WITH_KNOTS('',2,(#83307,#83308,#83309),
 .UNSPECIFIED.,.F.,.F.,(3,3),(0.,1.),.UNSPECIFIED.);
#23853=B_SPLINE_CURVE_WITH_KNOTS('',2,(#83312,#83313,#83314),
 .UNSPECIFIED.,.F.,.F.,(3,3),(0.,1.),.UNSPECIFIED.);
#23854=B_SPLINE_CURVE_WITH_KNOTS('',2,(#83322,#83323,#83324),
 .UNSPECIFIED.,.F.,.F.,(3,3),(0.,1.),.UNSPECIFIED.);
#23855=B_SPLINE_CURVE_WITH_KNOTS('',2,(#83327,#83328,#83329),
 .UNSPECIFIED.,.F.,.F.,(3,3),(0.,1.),.UNSPECIFIED.);
#23856=B_SPLINE_CURVE_WITH_KNOTS('',2,(#83337,#83338,#83339),
 .UNSPECIFIED.,.F.,.F.,(3,3),(0.,1.),.UNSPECIFIED.);
#23857=B_SPLINE_CURVE_WITH_KNOTS('',2,(#83342,#83343,#83344),
 .UNSPECIFIED.,.F.,.F.,(3,3),(0.,1.),.UNSPECIFIED.);
#23858=B_SPLINE_CURVE_WITH_KNOTS('',2,(#83352,#83353,#83354),
 .UNSPECIFIED.,.F.,.F.,(3,3),(0.,1.),.UNSPECIFIED.);
#23859=B_SPLINE_CURVE_WITH_KNOTS('',2,(#83357,#83358,#83359),
 .UNSPECIFIED.,.F.,.F.,(3,3),(0.,1.),.UNSPECIFIED.);
#23860=B_SPLINE_CURVE_WITH_KNOTS('',2,(#83367,#83368,#83369),
 .UNSPECIFIED.,.F.,.F.,(3,3),(0.,1.),.UNSPECIFIED.);
#23861=B_SPLINE_CURVE_WITH_KNOTS('',2,(#83372,#83373,#83374),
 .UNSPECIFIED.,.F.,.F.,(3,3),(0.,1.),.UNSPECIFIED.);
#23862=B_SPLINE_CURVE_WITH_KNOTS('',2,(#83382,#83383,#83384),
 .UNSPECIFIED.,.F.,.F.,(3,3),(0.,1.),.UNSPECIFIED.);
#23863=B_SPLINE_CURVE_WITH_KNOTS('',2,(#83387,#83388,#83389),
 .UNSPECIFIED.,.F.,.F.,(3,3),(0.,1.),.UNSPECIFIED.);
#23864=B_SPLINE_CURVE_WITH_KNOTS('',2,(#83403,#83404,#83405),
 .UNSPECIFIED.,.F.,.F.,(3,3),(0.,1.),.UNSPECIFIED.);
#23865=B_SPLINE_CURVE_WITH_KNOTS('',2,(#83408,#83409,#83410),
 .UNSPECIFIED.,.F.,.F.,(3,3),(0.,1.),.UNSPECIFIED.);
#23866=B_SPLINE_CURVE_WITH_KNOTS('',2,(#83418,#83419,#83420),
 .UNSPECIFIED.,.F.,.F.,(3,3),(0.,1.),.UNSPECIFIED.);
#23867=B_SPLINE_CURVE_WITH_KNOTS('',2,(#83423,#83424,#83425),
 .UNSPECIFIED.,.F.,.F.,(3,3),(0.,1.),.UNSPECIFIED.);
#23868=B_SPLINE_CURVE_WITH_KNOTS('',2,(#83433,#83434,#83435),
 .UNSPECIFIED.,.F.,.F.,(3,3),(0.,1.),.UNSPECIFIED.);
#23869=B_SPLINE_CURVE_WITH_KNOTS('',2,(#83438,#83439,#83440),
 .UNSPECIFIED.,.F.,.F.,(3,3),(0.,1.),.UNSPECIFIED.);
#23870=B_SPLINE_CURVE_WITH_KNOTS('',2,(#83448,#83449,#83450),
 .UNSPECIFIED.,.F.,.F.,(3,3),(0.,1.),.UNSPECIFIED.);
#23871=B_SPLINE_CURVE_WITH_KNOTS('',2,(#83453,#83454,#83455),
 .UNSPECIFIED.,.F.,.F.,(3,3),(0.,1.),.UNSPECIFIED.);
#23872=B_SPLINE_CURVE_WITH_KNOTS('',2,(#83463,#83464,#83465),
 .UNSPECIFIED.,.F.,.F.,(3,3),(0.,1.),.UNSPECIFIED.);
#23873=B_SPLINE_CURVE_WITH_KNOTS('',2,(#83468,#83469,#83470),
 .UNSPECIFIED.,.F.,.F.,(3,3),(0.,1.),.UNSPECIFIED.);
#23874=B_SPLINE_CURVE_WITH_KNOTS('',2,(#83478,#83479,#83480),
 .UNSPECIFIED.,.F.,.F.,(3,3),(0.,1.),.UNSPECIFIED.);
#23875=B_SPLINE_CURVE_WITH_KNOTS('',2,(#83483,#83484,#83485),
 .UNSPECIFIED.,.F.,.F.,(3,3),(0.,1.),.UNSPECIFIED.);
#23876=B_SPLINE_CURVE_WITH_KNOTS('',2,(#83493,#83494,#83495),
 .UNSPECIFIED.,.F.,.F.,(3,3),(0.,1.),.UNSPECIFIED.);
#23877=B_SPLINE_CURVE_WITH_KNOTS('',2,(#83498,#83499,#83500),
 .UNSPECIFIED.,.F.,.F.,(3,3),(0.,1.),.UNSPECIFIED.);
#23878=B_SPLINE_CURVE_WITH_KNOTS('',2,(#83513,#83514,#83515),
 .UNSPECIFIED.,.F.,.F.,(3,3),(0.,1.),.UNSPECIFIED.);
#23879=B_SPLINE_CURVE_WITH_KNOTS('',2,(#83516,#83517,#83518),
 .UNSPECIFIED.,.F.,.F.,(3,3),(0.,1.),.UNSPECIFIED.);
#23880=B_SPLINE_CURVE_WITH_KNOTS('',2,(#83529,#83530,#83531),
 .UNSPECIFIED.,.F.,.F.,(3,3),(0.,1.),.UNSPECIFIED.);
#23881=B_SPLINE_CURVE_WITH_KNOTS('',2,(#83535,#83536,#83537),
 .UNSPECIFIED.,.F.,.F.,(3,3),(0.,1.),.UNSPECIFIED.);
#23882=B_SPLINE_CURVE_WITH_KNOTS('',2,(#83546,#83547,#83548),
 .UNSPECIFIED.,.F.,.F.,(3,3),(0.,1.),.UNSPECIFIED.);
#23883=B_SPLINE_CURVE_WITH_KNOTS('',2,(#83551,#83552,#83553),
 .UNSPECIFIED.,.F.,.F.,(3,3),(0.,1.),.UNSPECIFIED.);
#23884=B_SPLINE_CURVE_WITH_KNOTS('',2,(#83561,#83562,#83563),
 .UNSPECIFIED.,.F.,.F.,(3,3),(0.,1.),.UNSPECIFIED.);
#23885=B_SPLINE_CURVE_WITH_KNOTS('',2,(#83566,#83567,#83568),
 .UNSPECIFIED.,.F.,.F.,(3,3),(0.,1.),.UNSPECIFIED.);
#23886=B_SPLINE_CURVE_WITH_KNOTS('',2,(#83576,#83577,#83578),
 .UNSPECIFIED.,.F.,.F.,(3,3),(0.,1.),.UNSPECIFIED.);
#23887=B_SPLINE_CURVE_WITH_KNOTS('',2,(#83581,#83582,#83583),
 .UNSPECIFIED.,.F.,.F.,(3,3),(0.,1.),.UNSPECIFIED.);
#23888=B_SPLINE_CURVE_WITH_KNOTS('',2,(#83591,#83592,#83593),
 .UNSPECIFIED.,.F.,.F.,(3,3),(0.,1.),.UNSPECIFIED.);
#23889=B_SPLINE_CURVE_WITH_KNOTS('',2,(#83596,#83597,#83598),
 .UNSPECIFIED.,.F.,.F.,(3,3),(0.,1.),.UNSPECIFIED.);
#23890=B_SPLINE_CURVE_WITH_KNOTS('',2,(#83606,#83607,#83608),
 .UNSPECIFIED.,.F.,.F.,(3,3),(0.,1.),.UNSPECIFIED.);
#23891=B_SPLINE_CURVE_WITH_KNOTS('',2,(#83611,#83612,#83613),
 .UNSPECIFIED.,.F.,.F.,(3,3),(0.,1.),.UNSPECIFIED.);
#23892=B_SPLINE_CURVE_WITH_KNOTS('',2,(#83621,#83622,#83623),
 .UNSPECIFIED.,.F.,.F.,(3,3),(0.,1.),.UNSPECIFIED.);
#23893=B_SPLINE_CURVE_WITH_KNOTS('',2,(#83626,#83627,#83628),
 .UNSPECIFIED.,.F.,.F.,(3,3),(0.,1.),.UNSPECIFIED.);
#23894=B_SPLINE_CURVE_WITH_KNOTS('',2,(#83635,#83636,#83637),
 .UNSPECIFIED.,.F.,.F.,(3,3),(0.,1.),.UNSPECIFIED.);
#23895=B_SPLINE_CURVE_WITH_KNOTS('',2,(#83638,#83639,#83640),
 .UNSPECIFIED.,.F.,.F.,(3,3),(0.,1.),.UNSPECIFIED.);
#23896=B_SPLINE_CURVE_WITH_KNOTS('',2,(#83649,#83650,#83651),
 .UNSPECIFIED.,.F.,.F.,(3,3),(0.,1.),.UNSPECIFIED.);
#23897=B_SPLINE_CURVE_WITH_KNOTS('',2,(#83655,#83656,#83657),
 .UNSPECIFIED.,.F.,.F.,(3,3),(0.,1.),.UNSPECIFIED.);
#23898=B_SPLINE_CURVE_WITH_KNOTS('',2,(#83666,#83667,#83668),
 .UNSPECIFIED.,.F.,.F.,(3,3),(0.,1.),.UNSPECIFIED.);
#23899=B_SPLINE_CURVE_WITH_KNOTS('',2,(#83671,#83672,#83673),
 .UNSPECIFIED.,.F.,.F.,(3,3),(0.,1.),.UNSPECIFIED.);
#23900=B_SPLINE_CURVE_WITH_KNOTS('',2,(#83681,#83682,#83683),
 .UNSPECIFIED.,.F.,.F.,(3,3),(0.,1.),.UNSPECIFIED.);
#23901=B_SPLINE_CURVE_WITH_KNOTS('',2,(#83686,#83687,#83688),
 .UNSPECIFIED.,.F.,.F.,(3,3),(0.,1.),.UNSPECIFIED.);
#23902=B_SPLINE_CURVE_WITH_KNOTS('',2,(#83696,#83697,#83698),
 .UNSPECIFIED.,.F.,.F.,(3,3),(0.,1.),.UNSPECIFIED.);
#23903=B_SPLINE_CURVE_WITH_KNOTS('',2,(#83701,#83702,#83703),
 .UNSPECIFIED.,.F.,.F.,(3,3),(0.,1.),.UNSPECIFIED.);
#23904=B_SPLINE_CURVE_WITH_KNOTS('',2,(#83711,#83712,#83713),
 .UNSPECIFIED.,.F.,.F.,(3,3),(0.,1.),.UNSPECIFIED.);
#23905=B_SPLINE_CURVE_WITH_KNOTS('',2,(#83716,#83717,#83718),
 .UNSPECIFIED.,.F.,.F.,(3,3),(0.,1.),.UNSPECIFIED.);
#23906=B_SPLINE_CURVE_WITH_KNOTS('',2,(#83726,#83727,#83728),
 .UNSPECIFIED.,.F.,.F.,(3,3),(0.,1.),.UNSPECIFIED.);
#23907=B_SPLINE_CURVE_WITH_KNOTS('',2,(#83731,#83732,#83733),
 .UNSPECIFIED.,.F.,.F.,(3,3),(0.,1.),.UNSPECIFIED.);
#23908=B_SPLINE_CURVE_WITH_KNOTS('',2,(#83741,#83742,#83743),
 .UNSPECIFIED.,.F.,.F.,(3,3),(0.,1.),.UNSPECIFIED.);
#23909=B_SPLINE_CURVE_WITH_KNOTS('',2,(#83746,#83747,#83748),
 .UNSPECIFIED.,.F.,.F.,(3,3),(0.,1.),.UNSPECIFIED.);
#23910=B_SPLINE_CURVE_WITH_KNOTS('',2,(#83756,#83757,#83758),
 .UNSPECIFIED.,.F.,.F.,(3,3),(0.,1.),.UNSPECIFIED.);
#23911=B_SPLINE_CURVE_WITH_KNOTS('',2,(#83761,#83762,#83763),
 .UNSPECIFIED.,.F.,.F.,(3,3),(0.,1.),.UNSPECIFIED.);
#23912=B_SPLINE_CURVE_WITH_KNOTS('',2,(#83771,#83772,#83773),
 .UNSPECIFIED.,.F.,.F.,(3,3),(0.,1.),.UNSPECIFIED.);
#23913=B_SPLINE_CURVE_WITH_KNOTS('',2,(#83776,#83777,#83778),
 .UNSPECIFIED.,.F.,.F.,(3,3),(0.,1.),.UNSPECIFIED.);
#23914=B_SPLINE_CURVE_WITH_KNOTS('',2,(#83786,#83787,#83788),
 .UNSPECIFIED.,.F.,.F.,(3,3),(0.,1.),.UNSPECIFIED.);
#23915=B_SPLINE_CURVE_WITH_KNOTS('',2,(#83791,#83792,#83793),
 .UNSPECIFIED.,.F.,.F.,(3,3),(0.,1.),.UNSPECIFIED.);
#23916=B_SPLINE_CURVE_WITH_KNOTS('',2,(#83801,#83802,#83803),
 .UNSPECIFIED.,.F.,.F.,(3,3),(0.,1.),.UNSPECIFIED.);
#23917=B_SPLINE_CURVE_WITH_KNOTS('',2,(#83806,#83807,#83808),
 .UNSPECIFIED.,.F.,.F.,(3,3),(0.,1.),.UNSPECIFIED.);
#23918=B_SPLINE_CURVE_WITH_KNOTS('',2,(#83815,#83816,#83817),
 .UNSPECIFIED.,.F.,.F.,(3,3),(0.,1.),.UNSPECIFIED.);
#23919=B_SPLINE_CURVE_WITH_KNOTS('',2,(#83818,#83819,#83820),
 .UNSPECIFIED.,.F.,.F.,(3,3),(0.,1.),.UNSPECIFIED.);
#23920=B_SPLINE_CURVE_WITH_KNOTS('',2,(#83917,#83918,#83919),
 .UNSPECIFIED.,.F.,.F.,(3,3),(0.,1.),.UNSPECIFIED.);
#23921=B_SPLINE_CURVE_WITH_KNOTS('',2,(#83923,#83924,#83925),
 .UNSPECIFIED.,.F.,.F.,(3,3),(0.,1.),.UNSPECIFIED.);
#23922=B_SPLINE_CURVE_WITH_KNOTS('',2,(#83934,#83935,#83936),
 .UNSPECIFIED.,.F.,.F.,(3,3),(0.,1.),.UNSPECIFIED.);
#23923=B_SPLINE_CURVE_WITH_KNOTS('',2,(#83939,#83940,#83941),
 .UNSPECIFIED.,.F.,.F.,(3,3),(0.,1.),.UNSPECIFIED.);
#23924=B_SPLINE_CURVE_WITH_KNOTS('',2,(#83949,#83950,#83951),
 .UNSPECIFIED.,.F.,.F.,(3,3),(0.,1.),.UNSPECIFIED.);
#23925=B_SPLINE_CURVE_WITH_KNOTS('',2,(#83954,#83955,#83956),
 .UNSPECIFIED.,.F.,.F.,(3,3),(0.,1.),.UNSPECIFIED.);
#23926=B_SPLINE_CURVE_WITH_KNOTS('',2,(#83964,#83965,#83966),
 .UNSPECIFIED.,.F.,.F.,(3,3),(0.,1.),.UNSPECIFIED.);
#23927=B_SPLINE_CURVE_WITH_KNOTS('',2,(#83969,#83970,#83971),
 .UNSPECIFIED.,.F.,.F.,(3,3),(0.,1.),.UNSPECIFIED.);
#23928=B_SPLINE_CURVE_WITH_KNOTS('',2,(#83979,#83980,#83981),
 .UNSPECIFIED.,.F.,.F.,(3,3),(0.,1.),.UNSPECIFIED.);
#23929=B_SPLINE_CURVE_WITH_KNOTS('',2,(#83984,#83985,#83986),
 .UNSPECIFIED.,.F.,.F.,(3,3),(0.,1.),.UNSPECIFIED.);
#23930=B_SPLINE_CURVE_WITH_KNOTS('',2,(#83994,#83995,#83996),
 .UNSPECIFIED.,.F.,.F.,(3,3),(0.,1.),.UNSPECIFIED.);
#23931=B_SPLINE_CURVE_WITH_KNOTS('',2,(#83999,#84000,#84001),
 .UNSPECIFIED.,.F.,.F.,(3,3),(0.,1.),.UNSPECIFIED.);
#23932=B_SPLINE_CURVE_WITH_KNOTS('',2,(#84009,#84010,#84011),
 .UNSPECIFIED.,.F.,.F.,(3,3),(0.,1.),.UNSPECIFIED.);
#23933=B_SPLINE_CURVE_WITH_KNOTS('',2,(#84014,#84015,#84016),
 .UNSPECIFIED.,.F.,.F.,(3,3),(0.,1.),.UNSPECIFIED.);
#23934=B_SPLINE_CURVE_WITH_KNOTS('',2,(#84023,#84024,#84025),
 .UNSPECIFIED.,.F.,.F.,(3,3),(0.,1.),.UNSPECIFIED.);
#23935=B_SPLINE_CURVE_WITH_KNOTS('',2,(#84026,#84027,#84028),
 .UNSPECIFIED.,.F.,.F.,(3,3),(0.,1.),.UNSPECIFIED.);
#23936=B_SPLINE_CURVE_WITH_KNOTS('',2,(#84037,#84038,#84039),
 .UNSPECIFIED.,.F.,.F.,(3,3),(0.,1.),.UNSPECIFIED.);
#23937=B_SPLINE_CURVE_WITH_KNOTS('',2,(#84043,#84044,#84045),
 .UNSPECIFIED.,.F.,.F.,(3,3),(0.,1.),.UNSPECIFIED.);
#23938=B_SPLINE_CURVE_WITH_KNOTS('',2,(#84054,#84055,#84056),
 .UNSPECIFIED.,.F.,.F.,(3,3),(0.,1.),.UNSPECIFIED.);
#23939=B_SPLINE_CURVE_WITH_KNOTS('',2,(#84059,#84060,#84061),
 .UNSPECIFIED.,.F.,.F.,(3,3),(0.,1.),.UNSPECIFIED.);
#23940=B_SPLINE_CURVE_WITH_KNOTS('',2,(#84069,#84070,#84071),
 .UNSPECIFIED.,.F.,.F.,(3,3),(0.,1.),.UNSPECIFIED.);
#23941=B_SPLINE_CURVE_WITH_KNOTS('',2,(#84074,#84075,#84076),
 .UNSPECIFIED.,.F.,.F.,(3,3),(0.,1.),.UNSPECIFIED.);
#23942=B_SPLINE_CURVE_WITH_KNOTS('',2,(#84084,#84085,#84086),
 .UNSPECIFIED.,.F.,.F.,(3,3),(0.,1.),.UNSPECIFIED.);
#23943=B_SPLINE_CURVE_WITH_KNOTS('',2,(#84089,#84090,#84091),
 .UNSPECIFIED.,.F.,.F.,(3,3),(0.,1.),.UNSPECIFIED.);
#23944=B_SPLINE_CURVE_WITH_KNOTS('',2,(#84099,#84100,#84101),
 .UNSPECIFIED.,.F.,.F.,(3,3),(0.,1.),.UNSPECIFIED.);
#23945=B_SPLINE_CURVE_WITH_KNOTS('',2,(#84104,#84105,#84106),
 .UNSPECIFIED.,.F.,.F.,(3,3),(0.,1.),.UNSPECIFIED.);
#23946=B_SPLINE_CURVE_WITH_KNOTS('',2,(#84114,#84115,#84116),
 .UNSPECIFIED.,.F.,.F.,(3,3),(0.,1.),.UNSPECIFIED.);
#23947=B_SPLINE_CURVE_WITH_KNOTS('',2,(#84119,#84120,#84121),
 .UNSPECIFIED.,.F.,.F.,(3,3),(0.,1.),.UNSPECIFIED.);
#23948=B_SPLINE_CURVE_WITH_KNOTS('',2,(#84129,#84130,#84131),
 .UNSPECIFIED.,.F.,.F.,(3,3),(0.,1.),.UNSPECIFIED.);
#23949=B_SPLINE_CURVE_WITH_KNOTS('',2,(#84134,#84135,#84136),
 .UNSPECIFIED.,.F.,.F.,(3,3),(0.,1.),.UNSPECIFIED.);
#23950=B_SPLINE_CURVE_WITH_KNOTS('',2,(#84144,#84145,#84146),
 .UNSPECIFIED.,.F.,.F.,(3,3),(0.,1.),.UNSPECIFIED.);
#23951=B_SPLINE_CURVE_WITH_KNOTS('',2,(#84149,#84150,#84151),
 .UNSPECIFIED.,.F.,.F.,(3,3),(0.,1.),.UNSPECIFIED.);
#23952=B_SPLINE_CURVE_WITH_KNOTS('',2,(#84159,#84160,#84161),
 .UNSPECIFIED.,.F.,.F.,(3,3),(0.,1.),.UNSPECIFIED.);
#23953=B_SPLINE_CURVE_WITH_KNOTS('',2,(#84164,#84165,#84166),
 .UNSPECIFIED.,.F.,.F.,(3,3),(0.,1.),.UNSPECIFIED.);
#23954=B_SPLINE_CURVE_WITH_KNOTS('',2,(#84174,#84175,#84176),
 .UNSPECIFIED.,.F.,.F.,(3,3),(0.,1.),.UNSPECIFIED.);
#23955=B_SPLINE_CURVE_WITH_KNOTS('',2,(#84179,#84180,#84181),
 .UNSPECIFIED.,.F.,.F.,(3,3),(0.,1.),.UNSPECIFIED.);
#23956=B_SPLINE_CURVE_WITH_KNOTS('',2,(#84189,#84190,#84191),
 .UNSPECIFIED.,.F.,.F.,(3,3),(0.,1.),.UNSPECIFIED.);
#23957=B_SPLINE_CURVE_WITH_KNOTS('',2,(#84194,#84195,#84196),
 .UNSPECIFIED.,.F.,.F.,(3,3),(0.,1.),.UNSPECIFIED.);
#23958=B_SPLINE_CURVE_WITH_KNOTS('',2,(#84203,#84204,#84205),
 .UNSPECIFIED.,.F.,.F.,(3,3),(0.,1.),.UNSPECIFIED.);
#23959=B_SPLINE_CURVE_WITH_KNOTS('',2,(#84206,#84207,#84208),
 .UNSPECIFIED.,.F.,.F.,(3,3),(0.,1.),.UNSPECIFIED.);
#23960=B_SPLINE_CURVE_WITH_KNOTS('',2,(#84218,#84219,#84220),
 .UNSPECIFIED.,.F.,.F.,(3,3),(0.,1.),.UNSPECIFIED.);
#23961=B_SPLINE_CURVE_WITH_KNOTS('',2,(#84224,#84225,#84226),
 .UNSPECIFIED.,.F.,.F.,(3,3),(0.,1.),.UNSPECIFIED.);
#23962=B_SPLINE_CURVE_WITH_KNOTS('',2,(#84235,#84236,#84237),
 .UNSPECIFIED.,.F.,.F.,(3,3),(0.,1.),.UNSPECIFIED.);
#23963=B_SPLINE_CURVE_WITH_KNOTS('',2,(#84240,#84241,#84242),
 .UNSPECIFIED.,.F.,.F.,(3,3),(0.,1.),.UNSPECIFIED.);
#23964=B_SPLINE_CURVE_WITH_KNOTS('',2,(#84250,#84251,#84252),
 .UNSPECIFIED.,.F.,.F.,(3,3),(0.,1.),.UNSPECIFIED.);
#23965=B_SPLINE_CURVE_WITH_KNOTS('',2,(#84255,#84256,#84257),
 .UNSPECIFIED.,.F.,.F.,(3,3),(0.,1.),.UNSPECIFIED.);
#23966=B_SPLINE_CURVE_WITH_KNOTS('',2,(#84265,#84266,#84267),
 .UNSPECIFIED.,.F.,.F.,(3,3),(0.,1.),.UNSPECIFIED.);
#23967=B_SPLINE_CURVE_WITH_KNOTS('',2,(#84270,#84271,#84272),
 .UNSPECIFIED.,.F.,.F.,(3,3),(0.,1.),.UNSPECIFIED.);
#23968=B_SPLINE_CURVE_WITH_KNOTS('',2,(#84280,#84281,#84282),
 .UNSPECIFIED.,.F.,.F.,(3,3),(0.,1.),.UNSPECIFIED.);
#23969=B_SPLINE_CURVE_WITH_KNOTS('',2,(#84285,#84286,#84287),
 .UNSPECIFIED.,.F.,.F.,(3,3),(0.,1.),.UNSPECIFIED.);
#23970=B_SPLINE_CURVE_WITH_KNOTS('',2,(#84295,#84296,#84297),
 .UNSPECIFIED.,.F.,.F.,(3,3),(0.,1.),.UNSPECIFIED.);
#23971=B_SPLINE_CURVE_WITH_KNOTS('',2,(#84300,#84301,#84302),
 .UNSPECIFIED.,.F.,.F.,(3,3),(0.,1.),.UNSPECIFIED.);
#23972=B_SPLINE_CURVE_WITH_KNOTS('',2,(#84346,#84347,#84348),
 .UNSPECIFIED.,.F.,.F.,(3,3),(0.,1.),.UNSPECIFIED.);
#23973=B_SPLINE_CURVE_WITH_KNOTS('',2,(#84351,#84352,#84353),
 .UNSPECIFIED.,.F.,.F.,(3,3),(0.,1.),.UNSPECIFIED.);
#23974=B_SPLINE_CURVE_WITH_KNOTS('',2,(#84361,#84362,#84363),
 .UNSPECIFIED.,.F.,.F.,(3,3),(0.,1.),.UNSPECIFIED.);
#23975=B_SPLINE_CURVE_WITH_KNOTS('',2,(#84366,#84367,#84368),
 .UNSPECIFIED.,.F.,.F.,(3,3),(0.,1.),.UNSPECIFIED.);
#23976=B_SPLINE_CURVE_WITH_KNOTS('',2,(#84376,#84377,#84378),
 .UNSPECIFIED.,.F.,.F.,(3,3),(0.,1.),.UNSPECIFIED.);
#23977=B_SPLINE_CURVE_WITH_KNOTS('',2,(#84381,#84382,#84383),
 .UNSPECIFIED.,.F.,.F.,(3,3),(0.,1.),.UNSPECIFIED.);
#23978=B_SPLINE_CURVE_WITH_KNOTS('',2,(#84391,#84392,#84393),
 .UNSPECIFIED.,.F.,.F.,(3,3),(0.,1.),.UNSPECIFIED.);
#23979=B_SPLINE_CURVE_WITH_KNOTS('',2,(#84396,#84397,#84398),
 .UNSPECIFIED.,.F.,.F.,(3,3),(0.,1.),.UNSPECIFIED.);
#23980=B_SPLINE_CURVE_WITH_KNOTS('',2,(#84406,#84407,#84408),
 .UNSPECIFIED.,.F.,.F.,(3,3),(0.,1.),.UNSPECIFIED.);
#23981=B_SPLINE_CURVE_WITH_KNOTS('',2,(#84411,#84412,#84413),
 .UNSPECIFIED.,.F.,.F.,(3,3),(0.,1.),.UNSPECIFIED.);
#23982=B_SPLINE_CURVE_WITH_KNOTS('',2,(#84421,#84422,#84423),
 .UNSPECIFIED.,.F.,.F.,(3,3),(0.,1.),.UNSPECIFIED.);
#23983=B_SPLINE_CURVE_WITH_KNOTS('',2,(#84426,#84427,#84428),
 .UNSPECIFIED.,.F.,.F.,(3,3),(0.,1.),.UNSPECIFIED.);
#23984=B_SPLINE_CURVE_WITH_KNOTS('',2,(#84436,#84437,#84438),
 .UNSPECIFIED.,.F.,.F.,(3,3),(0.,1.),.UNSPECIFIED.);
#23985=B_SPLINE_CURVE_WITH_KNOTS('',2,(#84441,#84442,#84443),
 .UNSPECIFIED.,.F.,.F.,(3,3),(0.,1.),.UNSPECIFIED.);
#23986=B_SPLINE_CURVE_WITH_KNOTS('',2,(#84451,#84452,#84453),
 .UNSPECIFIED.,.F.,.F.,(3,3),(0.,1.),.UNSPECIFIED.);
#23987=B_SPLINE_CURVE_WITH_KNOTS('',2,(#84456,#84457,#84458),
 .UNSPECIFIED.,.F.,.F.,(3,3),(0.,1.),.UNSPECIFIED.);
#23988=B_SPLINE_CURVE_WITH_KNOTS('',2,(#84471,#84472,#84473),
 .UNSPECIFIED.,.F.,.F.,(3,3),(0.,1.),.UNSPECIFIED.);
#23989=B_SPLINE_CURVE_WITH_KNOTS('',2,(#84474,#84475,#84476),
 .UNSPECIFIED.,.F.,.F.,(3,3),(0.,1.),.UNSPECIFIED.);
#23990=B_SPLINE_CURVE_WITH_KNOTS('',2,(#84487,#84488,#84489),
 .UNSPECIFIED.,.F.,.F.,(3,3),(0.,1.),.UNSPECIFIED.);
#23991=B_SPLINE_CURVE_WITH_KNOTS('',2,(#84493,#84494,#84495),
 .UNSPECIFIED.,.F.,.F.,(3,3),(0.,1.),.UNSPECIFIED.);
#23992=B_SPLINE_CURVE_WITH_KNOTS('',2,(#84504,#84505,#84506),
 .UNSPECIFIED.,.F.,.F.,(3,3),(0.,1.),.UNSPECIFIED.);
#23993=B_SPLINE_CURVE_WITH_KNOTS('',2,(#84509,#84510,#84511),
 .UNSPECIFIED.,.F.,.F.,(3,3),(0.,1.),.UNSPECIFIED.);
#23994=B_SPLINE_CURVE_WITH_KNOTS('',2,(#84519,#84520,#84521),
 .UNSPECIFIED.,.F.,.F.,(3,3),(0.,1.),.UNSPECIFIED.);
#23995=B_SPLINE_CURVE_WITH_KNOTS('',2,(#84524,#84525,#84526),
 .UNSPECIFIED.,.F.,.F.,(3,3),(0.,1.),.UNSPECIFIED.);
#23996=B_SPLINE_CURVE_WITH_KNOTS('',2,(#84534,#84535,#84536),
 .UNSPECIFIED.,.F.,.F.,(3,3),(0.,1.),.UNSPECIFIED.);
#23997=B_SPLINE_CURVE_WITH_KNOTS('',2,(#84539,#84540,#84541),
 .UNSPECIFIED.,.F.,.F.,(3,3),(0.,1.),.UNSPECIFIED.);
#23998=B_SPLINE_CURVE_WITH_KNOTS('',2,(#84549,#84550,#84551),
 .UNSPECIFIED.,.F.,.F.,(3,3),(0.,1.),.UNSPECIFIED.);
#23999=B_SPLINE_CURVE_WITH_KNOTS('',2,(#84554,#84555,#84556),
 .UNSPECIFIED.,.F.,.F.,(3,3),(0.,1.),.UNSPECIFIED.);
#24000=B_SPLINE_CURVE_WITH_KNOTS('',2,(#84564,#84565,#84566),
 .UNSPECIFIED.,.F.,.F.,(3,3),(0.,1.),.UNSPECIFIED.);
#24001=B_SPLINE_CURVE_WITH_KNOTS('',2,(#84569,#84570,#84571),
 .UNSPECIFIED.,.F.,.F.,(3,3),(0.,1.),.UNSPECIFIED.);
#24002=B_SPLINE_CURVE_WITH_KNOTS('',2,(#84579,#84580,#84581),
 .UNSPECIFIED.,.F.,.F.,(3,3),(0.,1.),.UNSPECIFIED.);
#24003=B_SPLINE_CURVE_WITH_KNOTS('',2,(#84584,#84585,#84586),
 .UNSPECIFIED.,.F.,.F.,(3,3),(0.,1.),.UNSPECIFIED.);
#24004=B_SPLINE_CURVE_WITH_KNOTS('',2,(#84593,#84594,#84595),
 .UNSPECIFIED.,.F.,.F.,(3,3),(0.,1.),.UNSPECIFIED.);
#24005=B_SPLINE_CURVE_WITH_KNOTS('',2,(#84596,#84597,#84598),
 .UNSPECIFIED.,.F.,.F.,(3,3),(0.,1.),.UNSPECIFIED.);
#24006=B_SPLINE_CURVE_WITH_KNOTS('',2,(#84607,#84608,#84609),
 .UNSPECIFIED.,.F.,.F.,(3,3),(0.,1.),.UNSPECIFIED.);
#24007=B_SPLINE_CURVE_WITH_KNOTS('',2,(#84613,#84614,#84615),
 .UNSPECIFIED.,.F.,.F.,(3,3),(0.,1.),.UNSPECIFIED.);
#24008=B_SPLINE_CURVE_WITH_KNOTS('',2,(#84624,#84625,#84626),
 .UNSPECIFIED.,.F.,.F.,(3,3),(0.,1.),.UNSPECIFIED.);
#24009=B_SPLINE_CURVE_WITH_KNOTS('',2,(#84629,#84630,#84631),
 .UNSPECIFIED.,.F.,.F.,(3,3),(0.,1.),.UNSPECIFIED.);
#24010=B_SPLINE_CURVE_WITH_KNOTS('',2,(#84639,#84640,#84641),
 .UNSPECIFIED.,.F.,.F.,(3,3),(0.,1.),.UNSPECIFIED.);
#24011=B_SPLINE_CURVE_WITH_KNOTS('',2,(#84644,#84645,#84646),
 .UNSPECIFIED.,.F.,.F.,(3,3),(0.,1.),.UNSPECIFIED.);
#24012=B_SPLINE_CURVE_WITH_KNOTS('',2,(#84654,#84655,#84656),
 .UNSPECIFIED.,.F.,.F.,(3,3),(0.,1.),.UNSPECIFIED.);
#24013=B_SPLINE_CURVE_WITH_KNOTS('',2,(#84659,#84660,#84661),
 .UNSPECIFIED.,.F.,.F.,(3,3),(0.,1.),.UNSPECIFIED.);
#24014=B_SPLINE_CURVE_WITH_KNOTS('',2,(#84669,#84670,#84671),
 .UNSPECIFIED.,.F.,.F.,(3,3),(0.,1.),.UNSPECIFIED.);
#24015=B_SPLINE_CURVE_WITH_KNOTS('',2,(#84674,#84675,#84676),
 .UNSPECIFIED.,.F.,.F.,(3,3),(0.,1.),.UNSPECIFIED.);
#24016=B_SPLINE_CURVE_WITH_KNOTS('',2,(#84684,#84685,#84686),
 .UNSPECIFIED.,.F.,.F.,(3,3),(0.,1.),.UNSPECIFIED.);
#24017=B_SPLINE_CURVE_WITH_KNOTS('',2,(#84689,#84690,#84691),
 .UNSPECIFIED.,.F.,.F.,(3,3),(0.,1.),.UNSPECIFIED.);
#24018=B_SPLINE_CURVE_WITH_KNOTS('',2,(#84699,#84700,#84701),
 .UNSPECIFIED.,.F.,.F.,(3,3),(0.,1.),.UNSPECIFIED.);
#24019=B_SPLINE_CURVE_WITH_KNOTS('',2,(#84704,#84705,#84706),
 .UNSPECIFIED.,.F.,.F.,(3,3),(0.,1.),.UNSPECIFIED.);
#24020=B_SPLINE_CURVE_WITH_KNOTS('',2,(#84714,#84715,#84716),
 .UNSPECIFIED.,.F.,.F.,(3,3),(0.,1.),.UNSPECIFIED.);
#24021=B_SPLINE_CURVE_WITH_KNOTS('',2,(#84719,#84720,#84721),
 .UNSPECIFIED.,.F.,.F.,(3,3),(0.,1.),.UNSPECIFIED.);
#24022=B_SPLINE_CURVE_WITH_KNOTS('',2,(#84729,#84730,#84731),
 .UNSPECIFIED.,.F.,.F.,(3,3),(0.,1.),.UNSPECIFIED.);
#24023=B_SPLINE_CURVE_WITH_KNOTS('',2,(#84734,#84735,#84736),
 .UNSPECIFIED.,.F.,.F.,(3,3),(0.,1.),.UNSPECIFIED.);
#24024=B_SPLINE_CURVE_WITH_KNOTS('',2,(#84744,#84745,#84746),
 .UNSPECIFIED.,.F.,.F.,(3,3),(0.,1.),.UNSPECIFIED.);
#24025=B_SPLINE_CURVE_WITH_KNOTS('',2,(#84749,#84750,#84751),
 .UNSPECIFIED.,.F.,.F.,(3,3),(0.,1.),.UNSPECIFIED.);
#24026=B_SPLINE_CURVE_WITH_KNOTS('',2,(#84759,#84760,#84761),
 .UNSPECIFIED.,.F.,.F.,(3,3),(0.,1.),.UNSPECIFIED.);
#24027=B_SPLINE_CURVE_WITH_KNOTS('',2,(#84764,#84765,#84766),
 .UNSPECIFIED.,.F.,.F.,(3,3),(0.,1.),.UNSPECIFIED.);
#24028=B_SPLINE_CURVE_WITH_KNOTS('',2,(#84773,#84774,#84775),
 .UNSPECIFIED.,.F.,.F.,(3,3),(0.,1.),.UNSPECIFIED.);
#24029=B_SPLINE_CURVE_WITH_KNOTS('',2,(#84776,#84777,#84778),
 .UNSPECIFIED.,.F.,.F.,(3,3),(0.,1.),.UNSPECIFIED.);
#24030=B_SPLINE_CURVE_WITH_KNOTS('',2,(#84788,#84789,#84790),
 .UNSPECIFIED.,.F.,.F.,(3,3),(0.,1.),.UNSPECIFIED.);
#24031=B_SPLINE_CURVE_WITH_KNOTS('',2,(#84794,#84795,#84796),
 .UNSPECIFIED.,.F.,.F.,(3,3),(0.,1.),.UNSPECIFIED.);
#24032=B_SPLINE_CURVE_WITH_KNOTS('',2,(#84805,#84806,#84807),
 .UNSPECIFIED.,.F.,.F.,(3,3),(0.,1.),.UNSPECIFIED.);
#24033=B_SPLINE_CURVE_WITH_KNOTS('',2,(#84810,#84811,#84812),
 .UNSPECIFIED.,.F.,.F.,(3,3),(0.,1.),.UNSPECIFIED.);
#24034=B_SPLINE_CURVE_WITH_KNOTS('',2,(#84820,#84821,#84822),
 .UNSPECIFIED.,.F.,.F.,(3,3),(0.,1.),.UNSPECIFIED.);
#24035=B_SPLINE_CURVE_WITH_KNOTS('',2,(#84825,#84826,#84827),
 .UNSPECIFIED.,.F.,.F.,(3,3),(0.,1.),.UNSPECIFIED.);
#24036=B_SPLINE_CURVE_WITH_KNOTS('',2,(#84835,#84836,#84837),
 .UNSPECIFIED.,.F.,.F.,(3,3),(0.,1.),.UNSPECIFIED.);
#24037=B_SPLINE_CURVE_WITH_KNOTS('',2,(#84840,#84841,#84842),
 .UNSPECIFIED.,.F.,.F.,(3,3),(0.,1.),.UNSPECIFIED.);
#24038=B_SPLINE_CURVE_WITH_KNOTS('',2,(#84850,#84851,#84852),
 .UNSPECIFIED.,.F.,.F.,(3,3),(0.,1.),.UNSPECIFIED.);
#24039=B_SPLINE_CURVE_WITH_KNOTS('',2,(#84855,#84856,#84857),
 .UNSPECIFIED.,.F.,.F.,(3,3),(0.,1.),.UNSPECIFIED.);
#24040=B_SPLINE_CURVE_WITH_KNOTS('',2,(#84865,#84866,#84867),
 .UNSPECIFIED.,.F.,.F.,(3,3),(0.,1.),.UNSPECIFIED.);
#24041=B_SPLINE_CURVE_WITH_KNOTS('',2,(#84870,#84871,#84872),
 .UNSPECIFIED.,.F.,.F.,(3,3),(0.,1.),.UNSPECIFIED.);
#24042=B_SPLINE_CURVE_WITH_KNOTS('',2,(#84880,#84881,#84882),
 .UNSPECIFIED.,.F.,.F.,(3,3),(0.,1.),.UNSPECIFIED.);
#24043=B_SPLINE_CURVE_WITH_KNOTS('',2,(#84885,#84886,#84887),
 .UNSPECIFIED.,.F.,.F.,(3,3),(0.,1.),.UNSPECIFIED.);
#24044=B_SPLINE_CURVE_WITH_KNOTS('',2,(#84895,#84896,#84897),
 .UNSPECIFIED.,.F.,.F.,(3,3),(0.,1.),.UNSPECIFIED.);
#24045=B_SPLINE_CURVE_WITH_KNOTS('',2,(#84900,#84901,#84902),
 .UNSPECIFIED.,.F.,.F.,(3,3),(0.,1.),.UNSPECIFIED.);
#24046=B_SPLINE_CURVE_WITH_KNOTS('',2,(#84909,#84910,#84911),
 .UNSPECIFIED.,.F.,.F.,(3,3),(0.,1.),.UNSPECIFIED.);
#24047=B_SPLINE_CURVE_WITH_KNOTS('',2,(#84912,#84913,#84914),
 .UNSPECIFIED.,.F.,.F.,(3,3),(0.,1.),.UNSPECIFIED.);
#24048=B_SPLINE_CURVE_WITH_KNOTS('',2,(#84923,#84924,#84925),
 .UNSPECIFIED.,.F.,.F.,(3,3),(0.,1.),.UNSPECIFIED.);
#24049=B_SPLINE_CURVE_WITH_KNOTS('',2,(#84929,#84930,#84931),
 .UNSPECIFIED.,.F.,.F.,(3,3),(0.,1.),.UNSPECIFIED.);
#24050=B_SPLINE_CURVE_WITH_KNOTS('',2,(#84940,#84941,#84942),
 .UNSPECIFIED.,.F.,.F.,(3,3),(0.,1.),.UNSPECIFIED.);
#24051=B_SPLINE_CURVE_WITH_KNOTS('',2,(#84945,#84946,#84947),
 .UNSPECIFIED.,.F.,.F.,(3,3),(0.,1.),.UNSPECIFIED.);
#24052=B_SPLINE_CURVE_WITH_KNOTS('',2,(#84955,#84956,#84957),
 .UNSPECIFIED.,.F.,.F.,(3,3),(0.,1.),.UNSPECIFIED.);
#24053=B_SPLINE_CURVE_WITH_KNOTS('',2,(#84960,#84961,#84962),
 .UNSPECIFIED.,.F.,.F.,(3,3),(0.,1.),.UNSPECIFIED.);
#24054=B_SPLINE_CURVE_WITH_KNOTS('',2,(#84970,#84971,#84972),
 .UNSPECIFIED.,.F.,.F.,(3,3),(0.,1.),.UNSPECIFIED.);
#24055=B_SPLINE_CURVE_WITH_KNOTS('',2,(#84975,#84976,#84977),
 .UNSPECIFIED.,.F.,.F.,(3,3),(0.,1.),.UNSPECIFIED.);
#24056=B_SPLINE_CURVE_WITH_KNOTS('',2,(#84985,#84986,#84987),
 .UNSPECIFIED.,.F.,.F.,(3,3),(0.,1.),.UNSPECIFIED.);
#24057=B_SPLINE_CURVE_WITH_KNOTS('',2,(#84990,#84991,#84992),
 .UNSPECIFIED.,.F.,.F.,(3,3),(0.,1.),.UNSPECIFIED.);
#24058=B_SPLINE_CURVE_WITH_KNOTS('',2,(#85000,#85001,#85002),
 .UNSPECIFIED.,.F.,.F.,(3,3),(0.,1.),.UNSPECIFIED.);
#24059=B_SPLINE_CURVE_WITH_KNOTS('',2,(#85005,#85006,#85007),
 .UNSPECIFIED.,.F.,.F.,(3,3),(0.,1.),.UNSPECIFIED.);
#24060=B_SPLINE_CURVE_WITH_KNOTS('',2,(#85015,#85016,#85017),
 .UNSPECIFIED.,.F.,.F.,(3,3),(0.,1.),.UNSPECIFIED.);
#24061=B_SPLINE_CURVE_WITH_KNOTS('',2,(#85020,#85021,#85022),
 .UNSPECIFIED.,.F.,.F.,(3,3),(0.,1.),.UNSPECIFIED.);
#24062=B_SPLINE_CURVE_WITH_KNOTS('',2,(#85030,#85031,#85032),
 .UNSPECIFIED.,.F.,.F.,(3,3),(0.,1.),.UNSPECIFIED.);
#24063=B_SPLINE_CURVE_WITH_KNOTS('',2,(#85035,#85036,#85037),
 .UNSPECIFIED.,.F.,.F.,(3,3),(0.,1.),.UNSPECIFIED.);
#24064=B_SPLINE_CURVE_WITH_KNOTS('',2,(#85045,#85046,#85047),
 .UNSPECIFIED.,.F.,.F.,(3,3),(0.,1.),.UNSPECIFIED.);
#24065=B_SPLINE_CURVE_WITH_KNOTS('',2,(#85050,#85051,#85052),
 .UNSPECIFIED.,.F.,.F.,(3,3),(0.,1.),.UNSPECIFIED.);
#24066=B_SPLINE_CURVE_WITH_KNOTS('',2,(#85060,#85061,#85062),
 .UNSPECIFIED.,.F.,.F.,(3,3),(0.,1.),.UNSPECIFIED.);
#24067=B_SPLINE_CURVE_WITH_KNOTS('',2,(#85065,#85066,#85067),
 .UNSPECIFIED.,.F.,.F.,(3,3),(0.,1.),.UNSPECIFIED.);
#24068=B_SPLINE_CURVE_WITH_KNOTS('',2,(#85075,#85076,#85077),
 .UNSPECIFIED.,.F.,.F.,(3,3),(0.,1.),.UNSPECIFIED.);
#24069=B_SPLINE_CURVE_WITH_KNOTS('',2,(#85080,#85081,#85082),
 .UNSPECIFIED.,.F.,.F.,(3,3),(0.,1.),.UNSPECIFIED.);
#24070=B_SPLINE_CURVE_WITH_KNOTS('',2,(#85090,#85091,#85092),
 .UNSPECIFIED.,.F.,.F.,(3,3),(0.,1.),.UNSPECIFIED.);
#24071=B_SPLINE_CURVE_WITH_KNOTS('',2,(#85095,#85096,#85097),
 .UNSPECIFIED.,.F.,.F.,(3,3),(0.,1.),.UNSPECIFIED.);
#24072=B_SPLINE_CURVE_WITH_KNOTS('',2,(#85105,#85106,#85107),
 .UNSPECIFIED.,.F.,.F.,(3,3),(0.,1.),.UNSPECIFIED.);
#24073=B_SPLINE_CURVE_WITH_KNOTS('',2,(#85110,#85111,#85112),
 .UNSPECIFIED.,.F.,.F.,(3,3),(0.,1.),.UNSPECIFIED.);
#24074=B_SPLINE_CURVE_WITH_KNOTS('',2,(#85120,#85121,#85122),
 .UNSPECIFIED.,.F.,.F.,(3,3),(0.,1.),.UNSPECIFIED.);
#24075=B_SPLINE_CURVE_WITH_KNOTS('',2,(#85125,#85126,#85127),
 .UNSPECIFIED.,.F.,.F.,(3,3),(0.,1.),.UNSPECIFIED.);
#24076=B_SPLINE_CURVE_WITH_KNOTS('',2,(#85135,#85136,#85137),
 .UNSPECIFIED.,.F.,.F.,(3,3),(0.,1.),.UNSPECIFIED.);
#24077=B_SPLINE_CURVE_WITH_KNOTS('',2,(#85140,#85141,#85142),
 .UNSPECIFIED.,.F.,.F.,(3,3),(0.,1.),.UNSPECIFIED.);
#24078=B_SPLINE_CURVE_WITH_KNOTS('',2,(#85150,#85151,#85152),
 .UNSPECIFIED.,.F.,.F.,(3,3),(0.,1.),.UNSPECIFIED.);
#24079=B_SPLINE_CURVE_WITH_KNOTS('',2,(#85155,#85156,#85157),
 .UNSPECIFIED.,.F.,.F.,(3,3),(0.,1.),.UNSPECIFIED.);
#24080=B_SPLINE_CURVE_WITH_KNOTS('',2,(#85165,#85166,#85167),
 .UNSPECIFIED.,.F.,.F.,(3,3),(0.,1.),.UNSPECIFIED.);
#24081=B_SPLINE_CURVE_WITH_KNOTS('',2,(#85170,#85171,#85172),
 .UNSPECIFIED.,.F.,.F.,(3,3),(0.,1.),.UNSPECIFIED.);
#24082=B_SPLINE_CURVE_WITH_KNOTS('',2,(#85185,#85186,#85187),
 .UNSPECIFIED.,.F.,.F.,(3,3),(0.,1.),.UNSPECIFIED.);
#24083=B_SPLINE_CURVE_WITH_KNOTS('',2,(#85188,#85189,#85190),
 .UNSPECIFIED.,.F.,.F.,(3,3),(0.,1.),.UNSPECIFIED.);
#24084=B_SPLINE_CURVE_WITH_KNOTS('',2,(#85202,#85203,#85204),
 .UNSPECIFIED.,.F.,.F.,(3,3),(0.,1.),.UNSPECIFIED.);
#24085=B_SPLINE_CURVE_WITH_KNOTS('',2,(#85208,#85209,#85210),
 .UNSPECIFIED.,.F.,.F.,(3,3),(0.,1.),.UNSPECIFIED.);
#24086=B_SPLINE_CURVE_WITH_KNOTS('',2,(#85219,#85220,#85221),
 .UNSPECIFIED.,.F.,.F.,(3,3),(0.,1.),.UNSPECIFIED.);
#24087=B_SPLINE_CURVE_WITH_KNOTS('',2,(#85224,#85225,#85226),
 .UNSPECIFIED.,.F.,.F.,(3,3),(0.,1.),.UNSPECIFIED.);
#24088=B_SPLINE_CURVE_WITH_KNOTS('',2,(#85234,#85235,#85236),
 .UNSPECIFIED.,.F.,.F.,(3,3),(0.,1.),.UNSPECIFIED.);
#24089=B_SPLINE_CURVE_WITH_KNOTS('',2,(#85239,#85240,#85241),
 .UNSPECIFIED.,.F.,.F.,(3,3),(0.,1.),.UNSPECIFIED.);
#24090=B_SPLINE_CURVE_WITH_KNOTS('',2,(#85249,#85250,#85251),
 .UNSPECIFIED.,.F.,.F.,(3,3),(0.,1.),.UNSPECIFIED.);
#24091=B_SPLINE_CURVE_WITH_KNOTS('',2,(#85254,#85255,#85256),
 .UNSPECIFIED.,.F.,.F.,(3,3),(0.,1.),.UNSPECIFIED.);
#24092=B_SPLINE_CURVE_WITH_KNOTS('',2,(#85264,#85265,#85266),
 .UNSPECIFIED.,.F.,.F.,(3,3),(0.,1.),.UNSPECIFIED.);
#24093=B_SPLINE_CURVE_WITH_KNOTS('',2,(#85269,#85270,#85271),
 .UNSPECIFIED.,.F.,.F.,(3,3),(0.,1.),.UNSPECIFIED.);
#24094=B_SPLINE_CURVE_WITH_KNOTS('',2,(#85279,#85280,#85281),
 .UNSPECIFIED.,.F.,.F.,(3,3),(0.,1.),.UNSPECIFIED.);
#24095=B_SPLINE_CURVE_WITH_KNOTS('',2,(#85284,#85285,#85286),
 .UNSPECIFIED.,.F.,.F.,(3,3),(0.,1.),.UNSPECIFIED.);
#24096=B_SPLINE_CURVE_WITH_KNOTS('',2,(#85294,#85295,#85296),
 .UNSPECIFIED.,.F.,.F.,(3,3),(0.,1.),.UNSPECIFIED.);
#24097=B_SPLINE_CURVE_WITH_KNOTS('',2,(#85299,#85300,#85301),
 .UNSPECIFIED.,.F.,.F.,(3,3),(0.,1.),.UNSPECIFIED.);
#24098=B_SPLINE_CURVE_WITH_KNOTS('',2,(#85308,#85309,#85310),
 .UNSPECIFIED.,.F.,.F.,(3,3),(0.,1.),.UNSPECIFIED.);
#24099=B_SPLINE_CURVE_WITH_KNOTS('',2,(#85311,#85312,#85313),
 .UNSPECIFIED.,.F.,.F.,(3,3),(0.,1.),.UNSPECIFIED.);
#24100=B_SPLINE_CURVE_WITH_KNOTS('',2,(#85322,#85323,#85324),
 .UNSPECIFIED.,.F.,.F.,(3,3),(0.,1.),.UNSPECIFIED.);
#24101=B_SPLINE_CURVE_WITH_KNOTS('',2,(#85328,#85329,#85330),
 .UNSPECIFIED.,.F.,.F.,(3,3),(0.,1.),.UNSPECIFIED.);
#24102=B_SPLINE_CURVE_WITH_KNOTS('',2,(#85339,#85340,#85341),
 .UNSPECIFIED.,.F.,.F.,(3,3),(0.,1.),.UNSPECIFIED.);
#24103=B_SPLINE_CURVE_WITH_KNOTS('',2,(#85344,#85345,#85346),
 .UNSPECIFIED.,.F.,.F.,(3,3),(0.,1.),.UNSPECIFIED.);
#24104=B_SPLINE_CURVE_WITH_KNOTS('',2,(#85354,#85355,#85356),
 .UNSPECIFIED.,.F.,.F.,(3,3),(0.,1.),.UNSPECIFIED.);
#24105=B_SPLINE_CURVE_WITH_KNOTS('',2,(#85359,#85360,#85361),
 .UNSPECIFIED.,.F.,.F.,(3,3),(0.,1.),.UNSPECIFIED.);
#24106=B_SPLINE_CURVE_WITH_KNOTS('',2,(#85369,#85370,#85371),
 .UNSPECIFIED.,.F.,.F.,(3,3),(0.,1.),.UNSPECIFIED.);
#24107=B_SPLINE_CURVE_WITH_KNOTS('',2,(#85374,#85375,#85376),
 .UNSPECIFIED.,.F.,.F.,(3,3),(0.,1.),.UNSPECIFIED.);
#24108=B_SPLINE_CURVE_WITH_KNOTS('',2,(#85384,#85385,#85386),
 .UNSPECIFIED.,.F.,.F.,(3,3),(0.,1.),.UNSPECIFIED.);
#24109=B_SPLINE_CURVE_WITH_KNOTS('',2,(#85389,#85390,#85391),
 .UNSPECIFIED.,.F.,.F.,(3,3),(0.,1.),.UNSPECIFIED.);
#24110=B_SPLINE_CURVE_WITH_KNOTS('',2,(#85399,#85400,#85401),
 .UNSPECIFIED.,.F.,.F.,(3,3),(0.,1.),.UNSPECIFIED.);
#24111=B_SPLINE_CURVE_WITH_KNOTS('',2,(#85404,#85405,#85406),
 .UNSPECIFIED.,.F.,.F.,(3,3),(0.,1.),.UNSPECIFIED.);
#24112=B_SPLINE_CURVE_WITH_KNOTS('',2,(#85414,#85415,#85416),
 .UNSPECIFIED.,.F.,.F.,(3,3),(0.,1.),.UNSPECIFIED.);
#24113=B_SPLINE_CURVE_WITH_KNOTS('',2,(#85419,#85420,#85421),
 .UNSPECIFIED.,.F.,.F.,(3,3),(0.,1.),.UNSPECIFIED.);
#24114=B_SPLINE_CURVE_WITH_KNOTS('',2,(#85429,#85430,#85431),
 .UNSPECIFIED.,.F.,.F.,(3,3),(0.,1.),.UNSPECIFIED.);
#24115=B_SPLINE_CURVE_WITH_KNOTS('',2,(#85434,#85435,#85436),
 .UNSPECIFIED.,.F.,.F.,(3,3),(0.,1.),.UNSPECIFIED.);
#24116=B_SPLINE_CURVE_WITH_KNOTS('',2,(#85444,#85445,#85446),
 .UNSPECIFIED.,.F.,.F.,(3,3),(0.,1.),.UNSPECIFIED.);
#24117=B_SPLINE_CURVE_WITH_KNOTS('',2,(#85449,#85450,#85451),
 .UNSPECIFIED.,.F.,.F.,(3,3),(0.,1.),.UNSPECIFIED.);
#24118=B_SPLINE_CURVE_WITH_KNOTS('',2,(#85459,#85460,#85461),
 .UNSPECIFIED.,.F.,.F.,(3,3),(0.,1.),.UNSPECIFIED.);
#24119=B_SPLINE_CURVE_WITH_KNOTS('',2,(#85464,#85465,#85466),
 .UNSPECIFIED.,.F.,.F.,(3,3),(0.,1.),.UNSPECIFIED.);
#24120=B_SPLINE_CURVE_WITH_KNOTS('',2,(#85474,#85475,#85476),
 .UNSPECIFIED.,.F.,.F.,(3,3),(0.,1.),.UNSPECIFIED.);
#24121=B_SPLINE_CURVE_WITH_KNOTS('',2,(#85479,#85480,#85481),
 .UNSPECIFIED.,.F.,.F.,(3,3),(0.,1.),.UNSPECIFIED.);
#24122=B_SPLINE_CURVE_WITH_KNOTS('',2,(#85488,#85489,#85490),
 .UNSPECIFIED.,.F.,.F.,(3,3),(0.,1.),.UNSPECIFIED.);
#24123=B_SPLINE_CURVE_WITH_KNOTS('',2,(#85491,#85492,#85493),
 .UNSPECIFIED.,.F.,.F.,(3,3),(0.,1.),.UNSPECIFIED.);
#24124=B_SPLINE_CURVE_WITH_KNOTS('',2,(#85503,#85504,#85505),
 .UNSPECIFIED.,.F.,.F.,(3,3),(0.,1.),.UNSPECIFIED.);
#24125=B_SPLINE_CURVE_WITH_KNOTS('',2,(#85509,#85510,#85511),
 .UNSPECIFIED.,.F.,.F.,(3,3),(0.,1.),.UNSPECIFIED.);
#24126=B_SPLINE_CURVE_WITH_KNOTS('',2,(#85520,#85521,#85522),
 .UNSPECIFIED.,.F.,.F.,(3,3),(0.,1.),.UNSPECIFIED.);
#24127=B_SPLINE_CURVE_WITH_KNOTS('',2,(#85525,#85526,#85527),
 .UNSPECIFIED.,.F.,.F.,(3,3),(0.,1.),.UNSPECIFIED.);
#24128=B_SPLINE_CURVE_WITH_KNOTS('',2,(#85535,#85536,#85537),
 .UNSPECIFIED.,.F.,.F.,(3,3),(0.,1.),.UNSPECIFIED.);
#24129=B_SPLINE_CURVE_WITH_KNOTS('',2,(#85540,#85541,#85542),
 .UNSPECIFIED.,.F.,.F.,(3,3),(0.,1.),.UNSPECIFIED.);
#24130=B_SPLINE_CURVE_WITH_KNOTS('',2,(#85556,#85557,#85558),
 .UNSPECIFIED.,.F.,.F.,(3,3),(0.,1.),.UNSPECIFIED.);
#24131=B_SPLINE_CURVE_WITH_KNOTS('',2,(#85561,#85562,#85563),
 .UNSPECIFIED.,.F.,.F.,(3,3),(0.,1.),.UNSPECIFIED.);
#24132=B_SPLINE_CURVE_WITH_KNOTS('',2,(#85571,#85572,#85573),
 .UNSPECIFIED.,.F.,.F.,(3,3),(0.,1.),.UNSPECIFIED.);
#24133=B_SPLINE_CURVE_WITH_KNOTS('',2,(#85576,#85577,#85578),
 .UNSPECIFIED.,.F.,.F.,(3,3),(0.,1.),.UNSPECIFIED.);
#24134=B_SPLINE_CURVE_WITH_KNOTS('',2,(#85586,#85587,#85588),
 .UNSPECIFIED.,.F.,.F.,(3,3),(0.,1.),.UNSPECIFIED.);
#24135=B_SPLINE_CURVE_WITH_KNOTS('',2,(#85591,#85592,#85593),
 .UNSPECIFIED.,.F.,.F.,(3,3),(0.,1.),.UNSPECIFIED.);
#24136=B_SPLINE_CURVE_WITH_KNOTS('',2,(#85625,#85626,#85627),
 .UNSPECIFIED.,.F.,.F.,(3,3),(0.,1.),.UNSPECIFIED.);
#24137=B_SPLINE_CURVE_WITH_KNOTS('',2,(#85631,#85632,#85633),
 .UNSPECIFIED.,.F.,.F.,(3,3),(0.,1.),.UNSPECIFIED.);
#24138=B_SPLINE_CURVE_WITH_KNOTS('',2,(#85642,#85643,#85644),
 .UNSPECIFIED.,.F.,.F.,(3,3),(0.,1.),.UNSPECIFIED.);
#24139=B_SPLINE_CURVE_WITH_KNOTS('',2,(#85647,#85648,#85649),
 .UNSPECIFIED.,.F.,.F.,(3,3),(0.,1.),.UNSPECIFIED.);
#24140=B_SPLINE_CURVE_WITH_KNOTS('',2,(#85657,#85658,#85659),
 .UNSPECIFIED.,.F.,.F.,(3,3),(0.,1.),.UNSPECIFIED.);
#24141=B_SPLINE_CURVE_WITH_KNOTS('',2,(#85662,#85663,#85664),
 .UNSPECIFIED.,.F.,.F.,(3,3),(0.,1.),.UNSPECIFIED.);
#24142=B_SPLINE_CURVE_WITH_KNOTS('',2,(#85672,#85673,#85674),
 .UNSPECIFIED.,.F.,.F.,(3,3),(0.,1.),.UNSPECIFIED.);
#24143=B_SPLINE_CURVE_WITH_KNOTS('',2,(#85677,#85678,#85679),
 .UNSPECIFIED.,.F.,.F.,(3,3),(0.,1.),.UNSPECIFIED.);
#24144=B_SPLINE_CURVE_WITH_KNOTS('',2,(#85687,#85688,#85689),
 .UNSPECIFIED.,.F.,.F.,(3,3),(0.,1.),.UNSPECIFIED.);
#24145=B_SPLINE_CURVE_WITH_KNOTS('',2,(#85692,#85693,#85694),
 .UNSPECIFIED.,.F.,.F.,(3,3),(0.,1.),.UNSPECIFIED.);
#24146=B_SPLINE_CURVE_WITH_KNOTS('',2,(#85702,#85703,#85704),
 .UNSPECIFIED.,.F.,.F.,(3,3),(0.,1.),.UNSPECIFIED.);
#24147=B_SPLINE_CURVE_WITH_KNOTS('',2,(#85707,#85708,#85709),
 .UNSPECIFIED.,.F.,.F.,(3,3),(0.,1.),.UNSPECIFIED.);
#24148=B_SPLINE_CURVE_WITH_KNOTS('',2,(#85717,#85718,#85719),
 .UNSPECIFIED.,.F.,.F.,(3,3),(0.,1.),.UNSPECIFIED.);
#24149=B_SPLINE_CURVE_WITH_KNOTS('',2,(#85722,#85723,#85724),
 .UNSPECIFIED.,.F.,.F.,(3,3),(0.,1.),.UNSPECIFIED.);
#24150=B_SPLINE_CURVE_WITH_KNOTS('',2,(#85731,#85732,#85733),
 .UNSPECIFIED.,.F.,.F.,(3,3),(0.,1.),.UNSPECIFIED.);
#24151=B_SPLINE_CURVE_WITH_KNOTS('',2,(#85734,#85735,#85736),
 .UNSPECIFIED.,.F.,.F.,(3,3),(0.,1.),.UNSPECIFIED.);
#24152=B_SPLINE_CURVE_WITH_KNOTS('',2,(#85745,#85746,#85747),
 .UNSPECIFIED.,.F.,.F.,(3,3),(0.,1.),.UNSPECIFIED.);
#24153=B_SPLINE_CURVE_WITH_KNOTS('',2,(#85751,#85752,#85753),
 .UNSPECIFIED.,.F.,.F.,(3,3),(0.,1.),.UNSPECIFIED.);
#24154=B_SPLINE_CURVE_WITH_KNOTS('',2,(#85762,#85763,#85764),
 .UNSPECIFIED.,.F.,.F.,(3,3),(0.,1.),.UNSPECIFIED.);
#24155=B_SPLINE_CURVE_WITH_KNOTS('',2,(#85767,#85768,#85769),
 .UNSPECIFIED.,.F.,.F.,(3,3),(0.,1.),.UNSPECIFIED.);
#24156=B_SPLINE_CURVE_WITH_KNOTS('',2,(#85777,#85778,#85779),
 .UNSPECIFIED.,.F.,.F.,(3,3),(0.,1.),.UNSPECIFIED.);
#24157=B_SPLINE_CURVE_WITH_KNOTS('',2,(#85782,#85783,#85784),
 .UNSPECIFIED.,.F.,.F.,(3,3),(0.,1.),.UNSPECIFIED.);
#24158=B_SPLINE_CURVE_WITH_KNOTS('',2,(#85792,#85793,#85794),
 .UNSPECIFIED.,.F.,.F.,(3,3),(0.,1.),.UNSPECIFIED.);
#24159=B_SPLINE_CURVE_WITH_KNOTS('',2,(#85797,#85798,#85799),
 .UNSPECIFIED.,.F.,.F.,(3,3),(0.,1.),.UNSPECIFIED.);
#24160=B_SPLINE_CURVE_WITH_KNOTS('',2,(#85807,#85808,#85809),
 .UNSPECIFIED.,.F.,.F.,(3,3),(0.,1.),.UNSPECIFIED.);
#24161=B_SPLINE_CURVE_WITH_KNOTS('',2,(#85812,#85813,#85814),
 .UNSPECIFIED.,.F.,.F.,(3,3),(0.,1.),.UNSPECIFIED.);
#24162=B_SPLINE_CURVE_WITH_KNOTS('',2,(#85822,#85823,#85824),
 .UNSPECIFIED.,.F.,.F.,(3,3),(0.,1.),.UNSPECIFIED.);
#24163=B_SPLINE_CURVE_WITH_KNOTS('',2,(#85827,#85828,#85829),
 .UNSPECIFIED.,.F.,.F.,(3,3),(0.,1.),.UNSPECIFIED.);
#24164=B_SPLINE_CURVE_WITH_KNOTS('',2,(#85837,#85838,#85839),
 .UNSPECIFIED.,.F.,.F.,(3,3),(0.,1.),.UNSPECIFIED.);
#24165=B_SPLINE_CURVE_WITH_KNOTS('',2,(#85842,#85843,#85844),
 .UNSPECIFIED.,.F.,.F.,(3,3),(0.,1.),.UNSPECIFIED.);
#24166=B_SPLINE_CURVE_WITH_KNOTS('',2,(#85852,#85853,#85854),
 .UNSPECIFIED.,.F.,.F.,(3,3),(0.,1.),.UNSPECIFIED.);
#24167=B_SPLINE_CURVE_WITH_KNOTS('',2,(#85857,#85858,#85859),
 .UNSPECIFIED.,.F.,.F.,(3,3),(0.,1.),.UNSPECIFIED.);
#24168=B_SPLINE_CURVE_WITH_KNOTS('',2,(#85867,#85868,#85869),
 .UNSPECIFIED.,.F.,.F.,(3,3),(0.,1.),.UNSPECIFIED.);
#24169=B_SPLINE_CURVE_WITH_KNOTS('',2,(#85872,#85873,#85874),
 .UNSPECIFIED.,.F.,.F.,(3,3),(0.,1.),.UNSPECIFIED.);
#24170=B_SPLINE_CURVE_WITH_KNOTS('',2,(#85882,#85883,#85884),
 .UNSPECIFIED.,.F.,.F.,(3,3),(0.,1.),.UNSPECIFIED.);
#24171=B_SPLINE_CURVE_WITH_KNOTS('',2,(#85887,#85888,#85889),
 .UNSPECIFIED.,.F.,.F.,(3,3),(0.,1.),.UNSPECIFIED.);
#24172=B_SPLINE_CURVE_WITH_KNOTS('',2,(#85897,#85898,#85899),
 .UNSPECIFIED.,.F.,.F.,(3,3),(0.,1.),.UNSPECIFIED.);
#24173=B_SPLINE_CURVE_WITH_KNOTS('',2,(#85902,#85903,#85904),
 .UNSPECIFIED.,.F.,.F.,(3,3),(0.,1.),.UNSPECIFIED.);
#24174=B_SPLINE_CURVE_WITH_KNOTS('',2,(#85911,#85912,#85913),
 .UNSPECIFIED.,.F.,.F.,(3,3),(0.,1.),.UNSPECIFIED.);
#24175=B_SPLINE_CURVE_WITH_KNOTS('',2,(#85914,#85915,#85916),
 .UNSPECIFIED.,.F.,.F.,(3,3),(0.,1.),.UNSPECIFIED.);
#24176=B_SPLINE_CURVE_WITH_KNOTS('',2,(#85926,#85927,#85928),
 .UNSPECIFIED.,.F.,.F.,(3,3),(0.,1.),.UNSPECIFIED.);
#24177=B_SPLINE_CURVE_WITH_KNOTS('',2,(#85932,#85933,#85934),
 .UNSPECIFIED.,.F.,.F.,(3,3),(0.,1.),.UNSPECIFIED.);
#24178=B_SPLINE_CURVE_WITH_KNOTS('',2,(#85943,#85944,#85945),
 .UNSPECIFIED.,.F.,.F.,(3,3),(0.,1.),.UNSPECIFIED.);
#24179=B_SPLINE_CURVE_WITH_KNOTS('',2,(#85948,#85949,#85950),
 .UNSPECIFIED.,.F.,.F.,(3,3),(0.,1.),.UNSPECIFIED.);
#24180=B_SPLINE_CURVE_WITH_KNOTS('',2,(#85958,#85959,#85960),
 .UNSPECIFIED.,.F.,.F.,(3,3),(0.,1.),.UNSPECIFIED.);
#24181=B_SPLINE_CURVE_WITH_KNOTS('',2,(#85963,#85964,#85965),
 .UNSPECIFIED.,.F.,.F.,(3,3),(0.,1.),.UNSPECIFIED.);
#24182=B_SPLINE_CURVE_WITH_KNOTS('',2,(#85973,#85974,#85975),
 .UNSPECIFIED.,.F.,.F.,(3,3),(0.,1.),.UNSPECIFIED.);
#24183=B_SPLINE_CURVE_WITH_KNOTS('',2,(#85978,#85979,#85980),
 .UNSPECIFIED.,.F.,.F.,(3,3),(0.,1.),.UNSPECIFIED.);
#24184=B_SPLINE_CURVE_WITH_KNOTS('',2,(#85988,#85989,#85990),
 .UNSPECIFIED.,.F.,.F.,(3,3),(0.,1.),.UNSPECIFIED.);
#24185=B_SPLINE_CURVE_WITH_KNOTS('',2,(#85993,#85994,#85995),
 .UNSPECIFIED.,.F.,.F.,(3,3),(0.,1.),.UNSPECIFIED.);
#24186=B_SPLINE_CURVE_WITH_KNOTS('',2,(#86003,#86004,#86005),
 .UNSPECIFIED.,.F.,.F.,(3,3),(0.,1.),.UNSPECIFIED.);
#24187=B_SPLINE_CURVE_WITH_KNOTS('',2,(#86008,#86009,#86010),
 .UNSPECIFIED.,.F.,.F.,(3,3),(0.,1.),.UNSPECIFIED.);
#24188=B_SPLINE_CURVE_WITH_KNOTS('',2,(#86018,#86019,#86020),
 .UNSPECIFIED.,.F.,.F.,(3,3),(0.,1.),.UNSPECIFIED.);
#24189=B_SPLINE_CURVE_WITH_KNOTS('',2,(#86023,#86024,#86025),
 .UNSPECIFIED.,.F.,.F.,(3,3),(0.,1.),.UNSPECIFIED.);
#24190=B_SPLINE_CURVE_WITH_KNOTS('',2,(#86032,#86033,#86034),
 .UNSPECIFIED.,.F.,.F.,(3,3),(0.,1.),.UNSPECIFIED.);
#24191=B_SPLINE_CURVE_WITH_KNOTS('',2,(#86035,#86036,#86037),
 .UNSPECIFIED.,.F.,.F.,(3,3),(0.,1.),.UNSPECIFIED.);
#24192=B_SPLINE_CURVE_WITH_KNOTS('',2,(#86046,#86047,#86048),
 .UNSPECIFIED.,.F.,.F.,(3,3),(0.,1.),.UNSPECIFIED.);
#24193=B_SPLINE_CURVE_WITH_KNOTS('',2,(#86052,#86053,#86054),
 .UNSPECIFIED.,.F.,.F.,(3,3),(0.,1.),.UNSPECIFIED.);
#24194=B_SPLINE_CURVE_WITH_KNOTS('',2,(#86063,#86064,#86065),
 .UNSPECIFIED.,.F.,.F.,(3,3),(0.,1.),.UNSPECIFIED.);
#24195=B_SPLINE_CURVE_WITH_KNOTS('',2,(#86068,#86069,#86070),
 .UNSPECIFIED.,.F.,.F.,(3,3),(0.,1.),.UNSPECIFIED.);
#24196=B_SPLINE_CURVE_WITH_KNOTS('',2,(#86078,#86079,#86080),
 .UNSPECIFIED.,.F.,.F.,(3,3),(0.,1.),.UNSPECIFIED.);
#24197=B_SPLINE_CURVE_WITH_KNOTS('',2,(#86083,#86084,#86085),
 .UNSPECIFIED.,.F.,.F.,(3,3),(0.,1.),.UNSPECIFIED.);
#24198=B_SPLINE_CURVE_WITH_KNOTS('',2,(#86093,#86094,#86095),
 .UNSPECIFIED.,.F.,.F.,(3,3),(0.,1.),.UNSPECIFIED.);
#24199=B_SPLINE_CURVE_WITH_KNOTS('',2,(#86098,#86099,#86100),
 .UNSPECIFIED.,.F.,.F.,(3,3),(0.,1.),.UNSPECIFIED.);
#24200=B_SPLINE_CURVE_WITH_KNOTS('',2,(#86108,#86109,#86110),
 .UNSPECIFIED.,.F.,.F.,(3,3),(0.,1.),.UNSPECIFIED.);
#24201=B_SPLINE_CURVE_WITH_KNOTS('',2,(#86113,#86114,#86115),
 .UNSPECIFIED.,.F.,.F.,(3,3),(0.,1.),.UNSPECIFIED.);
#24202=B_SPLINE_CURVE_WITH_KNOTS('',2,(#86123,#86124,#86125),
 .UNSPECIFIED.,.F.,.F.,(3,3),(0.,1.),.UNSPECIFIED.);
#24203=B_SPLINE_CURVE_WITH_KNOTS('',2,(#86128,#86129,#86130),
 .UNSPECIFIED.,.F.,.F.,(3,3),(0.,1.),.UNSPECIFIED.);
#24204=B_SPLINE_CURVE_WITH_KNOTS('',2,(#86138,#86139,#86140),
 .UNSPECIFIED.,.F.,.F.,(3,3),(0.,1.),.UNSPECIFIED.);
#24205=B_SPLINE_CURVE_WITH_KNOTS('',2,(#86143,#86144,#86145),
 .UNSPECIFIED.,.F.,.F.,(3,3),(0.,1.),.UNSPECIFIED.);
#24206=B_SPLINE_CURVE_WITH_KNOTS('',2,(#86153,#86154,#86155),
 .UNSPECIFIED.,.F.,.F.,(3,3),(0.,1.),.UNSPECIFIED.);
#24207=B_SPLINE_CURVE_WITH_KNOTS('',2,(#86158,#86159,#86160),
 .UNSPECIFIED.,.F.,.F.,(3,3),(0.,1.),.UNSPECIFIED.);
#24208=B_SPLINE_CURVE_WITH_KNOTS('',2,(#86167,#86168,#86169),
 .UNSPECIFIED.,.F.,.F.,(3,3),(0.,1.),.UNSPECIFIED.);
#24209=B_SPLINE_CURVE_WITH_KNOTS('',2,(#86170,#86171,#86172),
 .UNSPECIFIED.,.F.,.F.,(3,3),(0.,1.),.UNSPECIFIED.);
#24210=B_SPLINE_CURVE_WITH_KNOTS('',2,(#86181,#86182,#86183),
 .UNSPECIFIED.,.F.,.F.,(3,3),(0.,1.),.UNSPECIFIED.);
#24211=B_SPLINE_CURVE_WITH_KNOTS('',2,(#86187,#86188,#86189),
 .UNSPECIFIED.,.F.,.F.,(3,3),(0.,1.),.UNSPECIFIED.);
#24212=B_SPLINE_CURVE_WITH_KNOTS('',2,(#86198,#86199,#86200),
 .UNSPECIFIED.,.F.,.F.,(3,3),(0.,1.),.UNSPECIFIED.);
#24213=B_SPLINE_CURVE_WITH_KNOTS('',2,(#86203,#86204,#86205),
 .UNSPECIFIED.,.F.,.F.,(3,3),(0.,1.),.UNSPECIFIED.);
#24214=B_SPLINE_CURVE_WITH_KNOTS('',2,(#86213,#86214,#86215),
 .UNSPECIFIED.,.F.,.F.,(3,3),(0.,1.),.UNSPECIFIED.);
#24215=B_SPLINE_CURVE_WITH_KNOTS('',2,(#86218,#86219,#86220),
 .UNSPECIFIED.,.F.,.F.,(3,3),(0.,1.),.UNSPECIFIED.);
#24216=B_SPLINE_CURVE_WITH_KNOTS('',2,(#86228,#86229,#86230),
 .UNSPECIFIED.,.F.,.F.,(3,3),(0.,1.),.UNSPECIFIED.);
#24217=B_SPLINE_CURVE_WITH_KNOTS('',2,(#86233,#86234,#86235),
 .UNSPECIFIED.,.F.,.F.,(3,3),(0.,1.),.UNSPECIFIED.);
#24218=B_SPLINE_CURVE_WITH_KNOTS('',2,(#86243,#86244,#86245),
 .UNSPECIFIED.,.F.,.F.,(3,3),(0.,1.),.UNSPECIFIED.);
#24219=B_SPLINE_CURVE_WITH_KNOTS('',2,(#86248,#86249,#86250),
 .UNSPECIFIED.,.F.,.F.,(3,3),(0.,1.),.UNSPECIFIED.);
#24220=B_SPLINE_CURVE_WITH_KNOTS('',2,(#86258,#86259,#86260),
 .UNSPECIFIED.,.F.,.F.,(3,3),(0.,1.),.UNSPECIFIED.);
#24221=B_SPLINE_CURVE_WITH_KNOTS('',2,(#86263,#86264,#86265),
 .UNSPECIFIED.,.F.,.F.,(3,3),(0.,1.),.UNSPECIFIED.);
#24222=B_SPLINE_CURVE_WITH_KNOTS('',2,(#86273,#86274,#86275),
 .UNSPECIFIED.,.F.,.F.,(3,3),(0.,1.),.UNSPECIFIED.);
#24223=B_SPLINE_CURVE_WITH_KNOTS('',2,(#86278,#86279,#86280),
 .UNSPECIFIED.,.F.,.F.,(3,3),(0.,1.),.UNSPECIFIED.);
#24224=B_SPLINE_CURVE_WITH_KNOTS('',2,(#86288,#86289,#86290),
 .UNSPECIFIED.,.F.,.F.,(3,3),(0.,1.),.UNSPECIFIED.);
#24225=B_SPLINE_CURVE_WITH_KNOTS('',2,(#86293,#86294,#86295),
 .UNSPECIFIED.,.F.,.F.,(3,3),(0.,1.),.UNSPECIFIED.);
#24226=B_SPLINE_CURVE_WITH_KNOTS('',2,(#86303,#86304,#86305),
 .UNSPECIFIED.,.F.,.F.,(3,3),(0.,1.),.UNSPECIFIED.);
#24227=B_SPLINE_CURVE_WITH_KNOTS('',2,(#86308,#86309,#86310),
 .UNSPECIFIED.,.F.,.F.,(3,3),(0.,1.),.UNSPECIFIED.);
#24228=B_SPLINE_CURVE_WITH_KNOTS('',2,(#86318,#86319,#86320),
 .UNSPECIFIED.,.F.,.F.,(3,3),(0.,1.),.UNSPECIFIED.);
#24229=B_SPLINE_CURVE_WITH_KNOTS('',2,(#86323,#86324,#86325),
 .UNSPECIFIED.,.F.,.F.,(3,3),(0.,1.),.UNSPECIFIED.);
#24230=B_SPLINE_CURVE_WITH_KNOTS('',2,(#86333,#86334,#86335),
 .UNSPECIFIED.,.F.,.F.,(3,3),(0.,1.),.UNSPECIFIED.);
#24231=B_SPLINE_CURVE_WITH_KNOTS('',2,(#86338,#86339,#86340),
 .UNSPECIFIED.,.F.,.F.,(3,3),(0.,1.),.UNSPECIFIED.);
#24232=B_SPLINE_CURVE_WITH_KNOTS('',2,(#86348,#86349,#86350),
 .UNSPECIFIED.,.F.,.F.,(3,3),(0.,1.),.UNSPECIFIED.);
#24233=B_SPLINE_CURVE_WITH_KNOTS('',2,(#86353,#86354,#86355),
 .UNSPECIFIED.,.F.,.F.,(3,3),(0.,1.),.UNSPECIFIED.);
#24234=B_SPLINE_CURVE_WITH_KNOTS('',2,(#86363,#86364,#86365),
 .UNSPECIFIED.,.F.,.F.,(3,3),(0.,1.),.UNSPECIFIED.);
#24235=B_SPLINE_CURVE_WITH_KNOTS('',2,(#86368,#86369,#86370),
 .UNSPECIFIED.,.F.,.F.,(3,3),(0.,1.),.UNSPECIFIED.);
#24236=B_SPLINE_CURVE_WITH_KNOTS('',2,(#86378,#86379,#86380),
 .UNSPECIFIED.,.F.,.F.,(3,3),(0.,1.),.UNSPECIFIED.);
#24237=B_SPLINE_CURVE_WITH_KNOTS('',2,(#86383,#86384,#86385),
 .UNSPECIFIED.,.F.,.F.,(3,3),(0.,1.),.UNSPECIFIED.);
#24238=B_SPLINE_CURVE_WITH_KNOTS('',2,(#86393,#86394,#86395),
 .UNSPECIFIED.,.F.,.F.,(3,3),(0.,1.),.UNSPECIFIED.);
#24239=B_SPLINE_CURVE_WITH_KNOTS('',2,(#86398,#86399,#86400),
 .UNSPECIFIED.,.F.,.F.,(3,3),(0.,1.),.UNSPECIFIED.);
#24240=B_SPLINE_CURVE_WITH_KNOTS('',2,(#86407,#86408,#86409),
 .UNSPECIFIED.,.F.,.F.,(3,3),(0.,1.),.UNSPECIFIED.);
#24241=B_SPLINE_CURVE_WITH_KNOTS('',2,(#86410,#86411,#86412),
 .UNSPECIFIED.,.F.,.F.,(3,3),(0.,1.),.UNSPECIFIED.);
#24242=B_SPLINE_CURVE_WITH_KNOTS('',2,(#86425,#86426,#86427),
 .UNSPECIFIED.,.F.,.F.,(3,3),(0.,1.),.UNSPECIFIED.);
#24243=B_SPLINE_CURVE_WITH_KNOTS('',2,(#86431,#86432,#86433),
 .UNSPECIFIED.,.F.,.F.,(3,3),(0.,1.),.UNSPECIFIED.);
#24244=B_SPLINE_CURVE_WITH_KNOTS('',2,(#86442,#86443,#86444),
 .UNSPECIFIED.,.F.,.F.,(3,3),(0.,1.),.UNSPECIFIED.);
#24245=B_SPLINE_CURVE_WITH_KNOTS('',2,(#86447,#86448,#86449),
 .UNSPECIFIED.,.F.,.F.,(3,3),(0.,1.),.UNSPECIFIED.);
#24246=B_SPLINE_CURVE_WITH_KNOTS('',2,(#86457,#86458,#86459),
 .UNSPECIFIED.,.F.,.F.,(3,3),(0.,1.),.UNSPECIFIED.);
#24247=B_SPLINE_CURVE_WITH_KNOTS('',2,(#86462,#86463,#86464),
 .UNSPECIFIED.,.F.,.F.,(3,3),(0.,1.),.UNSPECIFIED.);
#24248=B_SPLINE_CURVE_WITH_KNOTS('',2,(#86472,#86473,#86474),
 .UNSPECIFIED.,.F.,.F.,(3,3),(0.,1.),.UNSPECIFIED.);
#24249=B_SPLINE_CURVE_WITH_KNOTS('',2,(#86477,#86478,#86479),
 .UNSPECIFIED.,.F.,.F.,(3,3),(0.,1.),.UNSPECIFIED.);
#24250=B_SPLINE_CURVE_WITH_KNOTS('',2,(#86487,#86488,#86489),
 .UNSPECIFIED.,.F.,.F.,(3,3),(0.,1.),.UNSPECIFIED.);
#24251=B_SPLINE_CURVE_WITH_KNOTS('',2,(#86492,#86493,#86494),
 .UNSPECIFIED.,.F.,.F.,(3,3),(0.,1.),.UNSPECIFIED.);
#24252=B_SPLINE_CURVE_WITH_KNOTS('',2,(#86502,#86503,#86504),
 .UNSPECIFIED.,.F.,.F.,(3,3),(0.,1.),.UNSPECIFIED.);
#24253=B_SPLINE_CURVE_WITH_KNOTS('',2,(#86507,#86508,#86509),
 .UNSPECIFIED.,.F.,.F.,(3,3),(0.,1.),.UNSPECIFIED.);
#24254=B_SPLINE_CURVE_WITH_KNOTS('',2,(#86517,#86518,#86519),
 .UNSPECIFIED.,.F.,.F.,(3,3),(0.,1.),.UNSPECIFIED.);
#24255=B_SPLINE_CURVE_WITH_KNOTS('',2,(#86522,#86523,#86524),
 .UNSPECIFIED.,.F.,.F.,(3,3),(0.,1.),.UNSPECIFIED.);
#24256=B_SPLINE_CURVE_WITH_KNOTS('',2,(#86531,#86532,#86533),
 .UNSPECIFIED.,.F.,.F.,(3,3),(0.,1.),.UNSPECIFIED.);
#24257=B_SPLINE_CURVE_WITH_KNOTS('',2,(#86534,#86535,#86536),
 .UNSPECIFIED.,.F.,.F.,(3,3),(0.,1.),.UNSPECIFIED.);
#24258=B_SPLINE_CURVE_WITH_KNOTS('',2,(#86545,#86546,#86547),
 .UNSPECIFIED.,.F.,.F.,(3,3),(0.,1.),.UNSPECIFIED.);
#24259=B_SPLINE_CURVE_WITH_KNOTS('',2,(#86551,#86552,#86553),
 .UNSPECIFIED.,.F.,.F.,(3,3),(0.,1.),.UNSPECIFIED.);
#24260=B_SPLINE_CURVE_WITH_KNOTS('',2,(#86562,#86563,#86564),
 .UNSPECIFIED.,.F.,.F.,(3,3),(0.,1.),.UNSPECIFIED.);
#24261=B_SPLINE_CURVE_WITH_KNOTS('',2,(#86567,#86568,#86569),
 .UNSPECIFIED.,.F.,.F.,(3,3),(0.,1.),.UNSPECIFIED.);
#24262=B_SPLINE_CURVE_WITH_KNOTS('',2,(#86577,#86578,#86579),
 .UNSPECIFIED.,.F.,.F.,(3,3),(0.,1.),.UNSPECIFIED.);
#24263=B_SPLINE_CURVE_WITH_KNOTS('',2,(#86582,#86583,#86584),
 .UNSPECIFIED.,.F.,.F.,(3,3),(0.,1.),.UNSPECIFIED.);
#24264=B_SPLINE_CURVE_WITH_KNOTS('',2,(#86592,#86593,#86594),
 .UNSPECIFIED.,.F.,.F.,(3,3),(0.,1.),.UNSPECIFIED.);
#24265=B_SPLINE_CURVE_WITH_KNOTS('',2,(#86597,#86598,#86599),
 .UNSPECIFIED.,.F.,.F.,(3,3),(0.,1.),.UNSPECIFIED.);
#24266=B_SPLINE_CURVE_WITH_KNOTS('',2,(#86607,#86608,#86609),
 .UNSPECIFIED.,.F.,.F.,(3,3),(0.,1.),.UNSPECIFIED.);
#24267=B_SPLINE_CURVE_WITH_KNOTS('',2,(#86612,#86613,#86614),
 .UNSPECIFIED.,.F.,.F.,(3,3),(0.,1.),.UNSPECIFIED.);
#24268=B_SPLINE_CURVE_WITH_KNOTS('',2,(#86622,#86623,#86624),
 .UNSPECIFIED.,.F.,.F.,(3,3),(0.,1.),.UNSPECIFIED.);
#24269=B_SPLINE_CURVE_WITH_KNOTS('',2,(#86627,#86628,#86629),
 .UNSPECIFIED.,.F.,.F.,(3,3),(0.,1.),.UNSPECIFIED.);
#24270=B_SPLINE_CURVE_WITH_KNOTS('',2,(#86637,#86638,#86639),
 .UNSPECIFIED.,.F.,.F.,(3,3),(0.,1.),.UNSPECIFIED.);
#24271=B_SPLINE_CURVE_WITH_KNOTS('',2,(#86642,#86643,#86644),
 .UNSPECIFIED.,.F.,.F.,(3,3),(0.,1.),.UNSPECIFIED.);
#24272=B_SPLINE_CURVE_WITH_KNOTS('',2,(#86652,#86653,#86654),
 .UNSPECIFIED.,.F.,.F.,(3,3),(0.,1.),.UNSPECIFIED.);
#24273=B_SPLINE_CURVE_WITH_KNOTS('',2,(#86657,#86658,#86659),
 .UNSPECIFIED.,.F.,.F.,(3,3),(0.,1.),.UNSPECIFIED.);
#24274=B_SPLINE_CURVE_WITH_KNOTS('',2,(#86667,#86668,#86669),
 .UNSPECIFIED.,.F.,.F.,(3,3),(0.,1.),.UNSPECIFIED.);
#24275=B_SPLINE_CURVE_WITH_KNOTS('',2,(#86672,#86673,#86674),
 .UNSPECIFIED.,.F.,.F.,(3,3),(0.,1.),.UNSPECIFIED.);
#24276=B_SPLINE_CURVE_WITH_KNOTS('',2,(#86682,#86683,#86684),
 .UNSPECIFIED.,.F.,.F.,(3,3),(0.,1.),.UNSPECIFIED.);
#24277=B_SPLINE_CURVE_WITH_KNOTS('',2,(#86687,#86688,#86689),
 .UNSPECIFIED.,.F.,.F.,(3,3),(0.,1.),.UNSPECIFIED.);
#24278=B_SPLINE_CURVE_WITH_KNOTS('',2,(#86697,#86698,#86699),
 .UNSPECIFIED.,.F.,.F.,(3,3),(0.,1.),.UNSPECIFIED.);
#24279=B_SPLINE_CURVE_WITH_KNOTS('',2,(#86702,#86703,#86704),
 .UNSPECIFIED.,.F.,.F.,(3,3),(0.,1.),.UNSPECIFIED.);
#24280=B_SPLINE_CURVE_WITH_KNOTS('',2,(#86711,#86712,#86713),
 .UNSPECIFIED.,.F.,.F.,(3,3),(0.,1.),.UNSPECIFIED.);
#24281=B_SPLINE_CURVE_WITH_KNOTS('',2,(#86714,#86715,#86716),
 .UNSPECIFIED.,.F.,.F.,(3,3),(0.,1.),.UNSPECIFIED.);
#24282=B_SPLINE_CURVE_WITH_KNOTS('',2,(#86726,#86727,#86728),
 .UNSPECIFIED.,.F.,.F.,(3,3),(0.,1.),.UNSPECIFIED.);
#24283=B_SPLINE_CURVE_WITH_KNOTS('',2,(#86732,#86733,#86734),
 .UNSPECIFIED.,.F.,.F.,(3,3),(0.,1.),.UNSPECIFIED.);
#24284=B_SPLINE_CURVE_WITH_KNOTS('',2,(#86743,#86744,#86745),
 .UNSPECIFIED.,.F.,.F.,(3,3),(0.,1.),.UNSPECIFIED.);
#24285=B_SPLINE_CURVE_WITH_KNOTS('',2,(#86748,#86749,#86750),
 .UNSPECIFIED.,.F.,.F.,(3,3),(0.,1.),.UNSPECIFIED.);
#24286=B_SPLINE_CURVE_WITH_KNOTS('',2,(#86758,#86759,#86760),
 .UNSPECIFIED.,.F.,.F.,(3,3),(0.,1.),.UNSPECIFIED.);
#24287=B_SPLINE_CURVE_WITH_KNOTS('',2,(#86763,#86764,#86765),
 .UNSPECIFIED.,.F.,.F.,(3,3),(0.,1.),.UNSPECIFIED.);
#24288=B_SPLINE_CURVE_WITH_KNOTS('',2,(#86773,#86774,#86775),
 .UNSPECIFIED.,.F.,.F.,(3,3),(0.,1.),.UNSPECIFIED.);
#24289=B_SPLINE_CURVE_WITH_KNOTS('',2,(#86778,#86779,#86780),
 .UNSPECIFIED.,.F.,.F.,(3,3),(0.,1.),.UNSPECIFIED.);
#24290=B_SPLINE_CURVE_WITH_KNOTS('',2,(#86788,#86789,#86790),
 .UNSPECIFIED.,.F.,.F.,(3,3),(0.,1.),.UNSPECIFIED.);
#24291=B_SPLINE_CURVE_WITH_KNOTS('',2,(#86793,#86794,#86795),
 .UNSPECIFIED.,.F.,.F.,(3,3),(0.,1.),.UNSPECIFIED.);
#24292=B_SPLINE_CURVE_WITH_KNOTS('',2,(#86803,#86804,#86805),
 .UNSPECIFIED.,.F.,.F.,(3,3),(0.,1.),.UNSPECIFIED.);
#24293=B_SPLINE_CURVE_WITH_KNOTS('',2,(#86808,#86809,#86810),
 .UNSPECIFIED.,.F.,.F.,(3,3),(0.,1.),.UNSPECIFIED.);
#24294=B_SPLINE_CURVE_WITH_KNOTS('',2,(#86818,#86819,#86820),
 .UNSPECIFIED.,.F.,.F.,(3,3),(0.,1.),.UNSPECIFIED.);
#24295=B_SPLINE_CURVE_WITH_KNOTS('',2,(#86823,#86824,#86825),
 .UNSPECIFIED.,.F.,.F.,(3,3),(0.,1.),.UNSPECIFIED.);
#24296=B_SPLINE_CURVE_WITH_KNOTS('',2,(#86832,#86833,#86834),
 .UNSPECIFIED.,.F.,.F.,(3,3),(0.,1.),.UNSPECIFIED.);
#24297=B_SPLINE_CURVE_WITH_KNOTS('',2,(#86835,#86836,#86837),
 .UNSPECIFIED.,.F.,.F.,(3,3),(0.,1.),.UNSPECIFIED.);
#24298=B_SPLINE_CURVE_WITH_KNOTS('',2,(#86846,#86847,#86848),
 .UNSPECIFIED.,.F.,.F.,(3,3),(0.,1.),.UNSPECIFIED.);
#24299=B_SPLINE_CURVE_WITH_KNOTS('',2,(#86852,#86853,#86854),
 .UNSPECIFIED.,.F.,.F.,(3,3),(0.,1.),.UNSPECIFIED.);
#24300=B_SPLINE_CURVE_WITH_KNOTS('',2,(#86863,#86864,#86865),
 .UNSPECIFIED.,.F.,.F.,(3,3),(0.,1.),.UNSPECIFIED.);
#24301=B_SPLINE_CURVE_WITH_KNOTS('',2,(#86868,#86869,#86870),
 .UNSPECIFIED.,.F.,.F.,(3,3),(0.,1.),.UNSPECIFIED.);
#24302=B_SPLINE_CURVE_WITH_KNOTS('',2,(#86878,#86879,#86880),
 .UNSPECIFIED.,.F.,.F.,(3,3),(0.,1.),.UNSPECIFIED.);
#24303=B_SPLINE_CURVE_WITH_KNOTS('',2,(#86883,#86884,#86885),
 .UNSPECIFIED.,.F.,.F.,(3,3),(0.,1.),.UNSPECIFIED.);
#24304=B_SPLINE_CURVE_WITH_KNOTS('',2,(#86893,#86894,#86895),
 .UNSPECIFIED.,.F.,.F.,(3,3),(0.,1.),.UNSPECIFIED.);
#24305=B_SPLINE_CURVE_WITH_KNOTS('',2,(#86898,#86899,#86900),
 .UNSPECIFIED.,.F.,.F.,(3,3),(0.,1.),.UNSPECIFIED.);
#24306=B_SPLINE_CURVE_WITH_KNOTS('',2,(#86908,#86909,#86910),
 .UNSPECIFIED.,.F.,.F.,(3,3),(0.,1.),.UNSPECIFIED.);
#24307=B_SPLINE_CURVE_WITH_KNOTS('',2,(#86913,#86914,#86915),
 .UNSPECIFIED.,.F.,.F.,(3,3),(0.,1.),.UNSPECIFIED.);
#24308=B_SPLINE_CURVE_WITH_KNOTS('',2,(#86923,#86924,#86925),
 .UNSPECIFIED.,.F.,.F.,(3,3),(0.,1.),.UNSPECIFIED.);
#24309=B_SPLINE_CURVE_WITH_KNOTS('',2,(#86928,#86929,#86930),
 .UNSPECIFIED.,.F.,.F.,(3,3),(0.,1.),.UNSPECIFIED.);
#24310=B_SPLINE_CURVE_WITH_KNOTS('',2,(#86938,#86939,#86940),
 .UNSPECIFIED.,.F.,.F.,(3,3),(0.,1.),.UNSPECIFIED.);
#24311=B_SPLINE_CURVE_WITH_KNOTS('',2,(#86943,#86944,#86945),
 .UNSPECIFIED.,.F.,.F.,(3,3),(0.,1.),.UNSPECIFIED.);
#24312=B_SPLINE_CURVE_WITH_KNOTS('',2,(#86953,#86954,#86955),
 .UNSPECIFIED.,.F.,.F.,(3,3),(0.,1.),.UNSPECIFIED.);
#24313=B_SPLINE_CURVE_WITH_KNOTS('',2,(#86958,#86959,#86960),
 .UNSPECIFIED.,.F.,.F.,(3,3),(0.,1.),.UNSPECIFIED.);
#24314=B_SPLINE_CURVE_WITH_KNOTS('',2,(#86968,#86969,#86970),
 .UNSPECIFIED.,.F.,.F.,(3,3),(0.,1.),.UNSPECIFIED.);
#24315=B_SPLINE_CURVE_WITH_KNOTS('',2,(#86973,#86974,#86975),
 .UNSPECIFIED.,.F.,.F.,(3,3),(0.,1.),.UNSPECIFIED.);
#24316=B_SPLINE_CURVE_WITH_KNOTS('',2,(#86983,#86984,#86985),
 .UNSPECIFIED.,.F.,.F.,(3,3),(0.,1.),.UNSPECIFIED.);
#24317=B_SPLINE_CURVE_WITH_KNOTS('',2,(#86988,#86989,#86990),
 .UNSPECIFIED.,.F.,.F.,(3,3),(0.,1.),.UNSPECIFIED.);
#24318=B_SPLINE_CURVE_WITH_KNOTS('',2,(#86998,#86999,#87000),
 .UNSPECIFIED.,.F.,.F.,(3,3),(0.,1.),.UNSPECIFIED.);
#24319=B_SPLINE_CURVE_WITH_KNOTS('',2,(#87003,#87004,#87005),
 .UNSPECIFIED.,.F.,.F.,(3,3),(0.,1.),.UNSPECIFIED.);
#24320=B_SPLINE_CURVE_WITH_KNOTS('',2,(#87013,#87014,#87015),
 .UNSPECIFIED.,.F.,.F.,(3,3),(0.,1.),.UNSPECIFIED.);
#24321=B_SPLINE_CURVE_WITH_KNOTS('',2,(#87018,#87019,#87020),
 .UNSPECIFIED.,.F.,.F.,(3,3),(0.,1.),.UNSPECIFIED.);
#24322=B_SPLINE_CURVE_WITH_KNOTS('',2,(#87028,#87029,#87030),
 .UNSPECIFIED.,.F.,.F.,(3,3),(0.,1.),.UNSPECIFIED.);
#24323=B_SPLINE_CURVE_WITH_KNOTS('',2,(#87033,#87034,#87035),
 .UNSPECIFIED.,.F.,.F.,(3,3),(0.,1.),.UNSPECIFIED.);
#24324=B_SPLINE_CURVE_WITH_KNOTS('',2,(#87043,#87044,#87045),
 .UNSPECIFIED.,.F.,.F.,(3,3),(0.,1.),.UNSPECIFIED.);
#24325=B_SPLINE_CURVE_WITH_KNOTS('',2,(#87048,#87049,#87050),
 .UNSPECIFIED.,.F.,.F.,(3,3),(0.,1.),.UNSPECIFIED.);
#24326=B_SPLINE_CURVE_WITH_KNOTS('',2,(#87058,#87059,#87060),
 .UNSPECIFIED.,.F.,.F.,(3,3),(0.,1.),.UNSPECIFIED.);
#24327=B_SPLINE_CURVE_WITH_KNOTS('',2,(#87063,#87064,#87065),
 .UNSPECIFIED.,.F.,.F.,(3,3),(0.,1.),.UNSPECIFIED.);
#24328=B_SPLINE_CURVE_WITH_KNOTS('',2,(#87073,#87074,#87075),
 .UNSPECIFIED.,.F.,.F.,(3,3),(0.,1.),.UNSPECIFIED.);
#24329=B_SPLINE_CURVE_WITH_KNOTS('',2,(#87078,#87079,#87080),
 .UNSPECIFIED.,.F.,.F.,(3,3),(0.,1.),.UNSPECIFIED.);
#24330=B_SPLINE_CURVE_WITH_KNOTS('',2,(#87088,#87089,#87090),
 .UNSPECIFIED.,.F.,.F.,(3,3),(0.,1.),.UNSPECIFIED.);
#24331=B_SPLINE_CURVE_WITH_KNOTS('',2,(#87093,#87094,#87095),
 .UNSPECIFIED.,.F.,.F.,(3,3),(0.,1.),.UNSPECIFIED.);
#24332=B_SPLINE_CURVE_WITH_KNOTS('',2,(#87103,#87104,#87105),
 .UNSPECIFIED.,.F.,.F.,(3,3),(0.,1.),.UNSPECIFIED.);
#24333=B_SPLINE_CURVE_WITH_KNOTS('',2,(#87108,#87109,#87110),
 .UNSPECIFIED.,.F.,.F.,(3,3),(0.,1.),.UNSPECIFIED.);
#24334=B_SPLINE_CURVE_WITH_KNOTS('',2,(#87118,#87119,#87120),
 .UNSPECIFIED.,.F.,.F.,(3,3),(0.,1.),.UNSPECIFIED.);
#24335=B_SPLINE_CURVE_WITH_KNOTS('',2,(#87123,#87124,#87125),
 .UNSPECIFIED.,.F.,.F.,(3,3),(0.,1.),.UNSPECIFIED.);
#24336=B_SPLINE_CURVE_WITH_KNOTS('',2,(#87133,#87134,#87135),
 .UNSPECIFIED.,.F.,.F.,(3,3),(0.,1.),.UNSPECIFIED.);
#24337=B_SPLINE_CURVE_WITH_KNOTS('',2,(#87138,#87139,#87140),
 .UNSPECIFIED.,.F.,.F.,(3,3),(0.,1.),.UNSPECIFIED.);
#24338=B_SPLINE_CURVE_WITH_KNOTS('',2,(#87153,#87154,#87155),
 .UNSPECIFIED.,.F.,.F.,(3,3),(0.,1.),.UNSPECIFIED.);
#24339=B_SPLINE_CURVE_WITH_KNOTS('',2,(#87156,#87157,#87158),
 .UNSPECIFIED.,.F.,.F.,(3,3),(0.,1.),.UNSPECIFIED.);
#24340=B_SPLINE_CURVE_WITH_KNOTS('',3,(#92665,#92666,#92667,#92668,#92669,
#92670,#92671,#92672,#92673,#92674),.UNSPECIFIED.,.F.,.F.,(4,2,2,2,4),(0.15884064059446,
0.198548710500137,0.238256780405813,0.277969030797367,0.317681281188921),
 .UNSPECIFIED.);
#24341=B_SPLINE_CURVE_WITH_KNOTS('',3,(#92676,#92677,#92678,#92679,#92680,
#92681,#92682,#92683,#92684,#92685,#92686,#92687,#92688,#92689,#92690,#92691,
#92692,#92693,#92694),.UNSPECIFIED.,.F.,.F.,(4,2,2,2,3,2,2,2,4),(0.476521921783381,
0.516229991689058,0.555938061594734,0.595650311986288,0.635362562377842,
0.675074812769396,0.71478706316095,0.754495133066626,0.794203202972302),
 .UNSPECIFIED.);
#24342=B_SPLINE_CURVE_WITH_KNOTS('',3,(#92695,#92696,#92697,#92698,#92699,
#92700,#92701,#92702,#92703,#92704),.UNSPECIFIED.,.F.,.F.,(4,2,2,2,4),(0.317681281188921,
0.357393531580475,0.397105781972029,0.436813851877705,0.476521921783381),
 .UNSPECIFIED.);
#24343=B_SPLINE_CURVE_WITH_KNOTS('',3,(#92709,#92710,#92711,#92712,#92713,
#92714,#92715,#92716,#92717,#92718),.UNSPECIFIED.,.F.,.F.,(4,2,2,2,4),(0.0861737376724399,
0.1203210472132,0.160394592890574,0.200468138567948,0.234615448108708),
 .UNSPECIFIED.);
#24344=B_SPLINE_CURVE_WITH_KNOTS('',3,(#92720,#92721,#92722,#92723,#92724,
#92725,#92726,#92727,#92728,#92729),.UNSPECIFIED.,.F.,.F.,(4,2,2,2,4),(0.406962923453589,
0.441110232994348,0.481183778671723,0.521257324349097,0.555404633889854),
 .UNSPECIFIED.);
#24345=B_SPLINE_CURVE_WITH_KNOTS('',3,(#97729,#97730,#97731,#97732,#97733,
#97734,#97735,#97736,#97737,#97738),.UNSPECIFIED.,.F.,.F.,(4,2,2,2,4),(0.234696888241094,
0.293366413777628,0.352035939314162,0.410714857898175,0.469393776482188),
 .UNSPECIFIED.);
#24346=B_SPLINE_CURVE_WITH_KNOTS('',3,(#97740,#97741,#97742,#97743,#97744,
#97745,#97746,#97747,#97748,#97749,#97750,#97751,#97752,#97753,#97754,#97755,
#97756,#97757,#97758),.UNSPECIFIED.,.F.,.F.,(4,2,2,2,3,2,2,2,4),(0.704090664723282,
0.762760190259816,0.82142971579635,0.880108634380363,0.938787552964375,
0.997466471548388,1.0561453901324,1.11481491566894,1.17348444120547),
 .UNSPECIFIED.);
#24347=B_SPLINE_CURVE_WITH_KNOTS('',3,(#97759,#97760,#97761,#97762,#97763,
#97764,#97765,#97766,#97767,#97768),.UNSPECIFIED.,.F.,.F.,(4,2,2,2,4),(0.469393776482188,
0.5280726950662,0.586751613650213,0.645421139186747,0.704090664723282),
 .UNSPECIFIED.);
#24348=B_SPLINE_CURVE_WITH_KNOTS('',3,(#97771,#97772,#97773,#97774,#97775,
#97776,#97777,#97778,#97779,#97780,#97781,#97782,#97783,#97784,#97785,#97786,
#97787,#97788),.UNSPECIFIED.,.F.,.F.,(4,2,2,2,2,2,2,2,4),(0.0317636912176915,
0.0605992517752672,0.121198503550534,0.181346844389925,0.241495185229315,
0.301643526068706,0.361791866908096,0.422391118683363,0.45122667924094),
 .UNSPECIFIED.);
#24349=B_SPLINE_CURVE_WITH_KNOTS('',3,(#97791,#97792,#97793,#97794,#97795,
#97796,#97797,#97798,#97799,#97800,#97801,#97802,#97803,#97804,#97805,#97806,
#97807,#97808),.UNSPECIFIED.,.F.,.F.,(4,2,2,2,2,2,2,2,4),(0.514754061676322,
0.543589622233898,0.604188874009165,0.664337214848555,0.724485555687945,
0.784633896527336,0.844782237366726,0.905381489141993,0.934217049699569),
 .UNSPECIFIED.);
#24350=B_SPLINE_CURVE_WITH_KNOTS('',3,(#102634,#102635,#102636,#102637,
#102638,#102639,#102640,#102641,#102642,#102643),.UNSPECIFIED.,.F.,.F.,
(4,3,3,4),(-4.09254174883833,-3.9421844604419,-2.95663834533143,-2.06514013327814),
 .UNSPECIFIED.);
#24351=B_SPLINE_CURVE_WITH_KNOTS('',3,(#102646,#102647,#102648,#102649,
#102650,#102651,#102652),.UNSPECIFIED.,.F.,.F.,(4,3,4),(0.,0.985546115110468,
1.11419103802957),.UNSPECIFIED.);
#24352=B_SPLINE_CURVE_WITH_KNOTS('',3,(#102657,#102658,#102659,#102660,
#102661,#102662,#102663,#102664,#102665,#102666,#102667,#102668,#102669,
#102670,#102671,#102672,#102673,#102674,#102675,#102676,#102677,#102678),
 .UNSPECIFIED.,.F.,.F.,(4,3,3,3,3,3,3,4),(-10.3757270560179,-9.85546115110475,
-8.86991503599427,-7.8843689208838,-6.89882280577333,-5.91327669066285,
-4.92773057555237,-4.09254174883833),.UNSPECIFIED.);
#24353=B_SPLINE_CURVE_WITH_KNOTS('',3,(#102679,#102680,#102681,#102682,
#102683,#102684,#102685,#102686,#102687,#102688,#102689,#102690,#102691,
#102692,#102693,#102694,#102695,#102696,#102697,#102698,#102699,#102700),
 .UNSPECIFIED.,.F.,.F.,(4,3,3,3,3,3,3,4),(1.11419103802957,1.97109223022095,
2.95663834533142,3.9421844604419,4.92773057555238,5.91327669066286,6.89882280577334,
7.39737634520915),.UNSPECIFIED.);
#24354=B_SPLINE_CURVE_WITH_KNOTS('',3,(#102705,#102706,#102707,#102708,
#102709,#102710,#102711,#102712,#102713,#102714,#102715,#102716,#102717,
#102718,#102719,#102720,#102721,#102722,#102723,#102724,#102725,#102726),
 .UNSPECIFIED.,.F.,.F.,(4,3,3,3,3,3,3,4),(-16.6589123631975,-15.7687378417676,
-14.7831917266571,-13.7976456115466,-12.8120994964362,-11.8265533813257,
-10.8410072662152,-10.3757270560179),.UNSPECIFIED.);
#24355=B_SPLINE_CURVE_WITH_KNOTS('',3,(#102727,#102728,#102729,#102730,
#102731,#102732,#102733,#102734,#102735,#102736,#102737,#102738,#102739,
#102740,#102741,#102742,#102743,#102744,#102745,#102746,#102747,#102748),
 .UNSPECIFIED.,.F.,.F.,(4,3,3,3,3,3,3,4),(7.39737634520915,7.88436892088381,
8.86991503599429,9.85546115110476,10.8410072662152,11.8265533813257,12.8120994964362,
13.6805616523887),.UNSPECIFIED.);
#24356=B_SPLINE_CURVE_WITH_KNOTS('',3,(#102753,#102754,#102755,#102756,
#102757,#102758,#102759,#102760,#102761,#102762,#102763,#102764,#102765,
#102766,#102767,#102768,#102769,#102770,#102771,#102772,#102773,#102774,
#102775,#102776,#102777),.UNSPECIFIED.,.F.,.F.,(4,3,3,3,3,3,3,3,4),(-22.9420976703771,
-22.6675606475409,-21.6820145324305,-20.69646841732,-19.7109223022095,-18.725376187099,
-17.7398300719886,-16.7542839568781,-16.6589123631975),.UNSPECIFIED.);
#24357=B_SPLINE_CURVE_WITH_KNOTS('',3,(#102778,#102779,#102780,#102781,
#102782,#102783,#102784,#102785,#102786,#102787,#102788,#102789,#102790,
#102791,#102792,#102793,#102794,#102795,#102796,#102797,#102798,#102799,
#102800,#102801,#102802),.UNSPECIFIED.,.F.,.F.,(4,3,3,3,3,3,3,3,4),(13.6805616523887,
13.7976456115467,14.7831917266571,15.7687378417676,16.7542839568781,17.7398300719886,
18.725376187099,19.7109223022095,19.9637469595683),.UNSPECIFIED.);
#24358=B_SPLINE_CURVE_WITH_KNOTS('',3,(#102807,#102808,#102809,#102810,
#102811,#102812,#102813,#102814,#102815,#102816,#102817,#102818,#102819,
#102820,#102821,#102822,#102823,#102824,#102825,#102826,#102827,#102828),
 .UNSPECIFIED.,.F.,.F.,(4,3,3,3,3,3,3,4),(-29.2252829775567,-28.5808373382038,
-27.5952912230933,-26.6097451079828,-25.6241989928724,-24.6386528777619,
-23.6531067626514,-22.9420976703771),.UNSPECIFIED.);
#24359=B_SPLINE_CURVE_WITH_KNOTS('',3,(#102829,#102830,#102831,#102832,
#102833,#102834,#102835,#102836,#102837,#102838,#102839,#102840,#102841,
#102842,#102843,#102844,#102845,#102846,#102847,#102848,#102849,#102850),
 .UNSPECIFIED.,.F.,.F.,(4,3,3,3,3,3,3,4),(19.9637469595683,20.69646841732,
21.6820145324305,22.6675606475409,23.6531067626514,24.6386528777619,25.6241989928724,
26.2469322667479),.UNSPECIFIED.);
#24360=B_SPLINE_CURVE_WITH_KNOTS('',3,(#102855,#102856,#102857,#102858,
#102859,#102860,#102861,#102862,#102863,#102864,#102865,#102866,#102867,
#102868,#102869,#102870,#102871,#102872,#102873,#102874,#102875,#102876,
#102877,#102878,#102879),.UNSPECIFIED.,.F.,.F.,(4,3,3,3,3,3,3,3,4),(-35.5084682847363,
-35.4796601439771,-34.4941140288666,-33.5085679137561,-32.5230217986457,
-31.5374756835352,-30.5519295684247,-29.5663834533142,-29.2252829775567),
 .UNSPECIFIED.);
#24361=B_SPLINE_CURVE_WITH_KNOTS('',3,(#102880,#102881,#102882,#102883,
#102884,#102885,#102886,#102887,#102888,#102889,#102890,#102891,#102892,
#102893,#102894,#102895,#102896,#102897,#102898,#102899,#102900,#102901,
#102902,#102903,#102904),.UNSPECIFIED.,.F.,.F.,(4,3,3,3,3,3,3,3,4),(26.2469322667479,
26.6097451079828,27.5952912230933,28.5808373382038,29.5663834533142,30.5519295684247,
31.5374756835352,32.5230217986457,32.5301175739275),.UNSPECIFIED.);
#24362=B_SPLINE_CURVE_WITH_KNOTS('',3,(#102909,#102910,#102911,#102912,
#102913,#102914,#102915,#102916,#102917,#102918,#102919,#102920,#102921,
#102922,#102923,#102924,#102925,#102926,#102927,#102928,#102929,#102930),
 .UNSPECIFIED.,.F.,.F.,(4,3,3,3,3,3,3,4),(-41.7916535919158,-41.3929368346399,
-40.4073907195295,-39.421844604419,-38.4362984893085,-37.450752374198,-36.4652062590876,
-35.5084682847363),.UNSPECIFIED.);
#24363=B_SPLINE_CURVE_WITH_KNOTS('',3,(#102931,#102932,#102933,#102934,
#102935,#102936,#102937,#102938,#102939,#102940,#102941,#102942,#102943,
#102944,#102945,#102946,#102947,#102948,#102949,#102950,#102951,#102952),
 .UNSPECIFIED.,.F.,.F.,(4,3,3,3,3,3,3,4),(32.5301175739275,33.5085679137562,
34.4941140288666,35.4796601439771,36.4652062590876,37.4507523741981,38.4362984893085,
38.8133028811071),.UNSPECIFIED.);
#24364=B_SPLINE_CURVE_WITH_KNOTS('',3,(#102957,#102958,#102959,#102960,
#102961,#102962,#102963,#102964,#102965,#102966,#102967,#102968,#102969,
#102970,#102971,#102972,#102973,#102974,#102975,#102976,#102977,#102978),
 .UNSPECIFIED.,.F.,.F.,(4,3,3,3,3,3,3,4),(-48.0748388990954,-47.3062135253028,
-46.3206674101923,-45.3351212950818,-44.3495751799714,-43.3640290648609,
-42.3784829497504,-41.7916535919158),.UNSPECIFIED.);
#24365=B_SPLINE_CURVE_WITH_KNOTS('',3,(#102979,#102980,#102981,#102982,
#102983,#102984,#102985,#102986,#102987,#102988,#102989,#102990,#102991,
#102992,#102993,#102994,#102995,#102996,#102997,#102998,#102999,#103000),
 .UNSPECIFIED.,.F.,.F.,(4,3,3,3,3,3,3,4),(38.8133028811071,39.421844604419,
40.4073907195295,41.39293683464,42.3784829497504,43.3640290648609,44.3495751799714,
45.0964881882867),.UNSPECIFIED.);
#24366=B_SPLINE_CURVE_WITH_KNOTS('',3,(#103005,#103006,#103007,#103008,
#103009,#103010,#103011,#103012,#103013,#103014,#103015,#103016,#103017,
#103018,#103019,#103020,#103021,#103022,#103023,#103024,#103025,#103026,
#103027,#103028,#103029),.UNSPECIFIED.,.F.,.F.,(4,3,3,3,3,3,3,3,4),(-54.358024206275,
-54.2050363310761,-53.2194902159656,-52.2339441008552,-51.2483979857447,
-50.2628518706342,-49.2773057555237,-48.2917596404133,-48.0748388990954),
 .UNSPECIFIED.);
#24367=B_SPLINE_CURVE_WITH_KNOTS('',3,(#103030,#103031,#103032,#103033,
#103034,#103035,#103036,#103037,#103038,#103039,#103040,#103041,#103042,
#103043,#103044,#103045,#103046,#103047,#103048,#103049,#103050,#103051,
#103052,#103053,#103054),.UNSPECIFIED.,.F.,.F.,(4,3,3,3,3,3,3,3,4),(45.0964881882867,
45.3351212950819,46.3206674101923,47.3062135253028,48.2917596404133,49.2773057555238,
50.2628518706342,51.2483979857447,51.3796734954663),.UNSPECIFIED.);
#24368=B_SPLINE_CURVE_WITH_KNOTS('',3,(#103059,#103060,#103061,#103062,
#103063,#103064,#103065,#103066,#103067,#103068,#103069,#103070,#103071,
#103072,#103073,#103074,#103075,#103076,#103077,#103078,#103079,#103080),
 .UNSPECIFIED.,.F.,.F.,(4,3,3,3,3,3,3,4),(-60.6412095134546,-60.118313021739,
-59.1327669066285,-58.147220791518,-57.1616746764076,-56.1761285612971,
-55.1905824461866,-54.358024206275),.UNSPECIFIED.);
#24369=B_SPLINE_CURVE_WITH_KNOTS('',3,(#103081,#103082,#103083,#103084,
#103085,#103086,#103087,#103088,#103089,#103090,#103091,#103092,#103093,
#103094,#103095,#103096,#103097,#103098,#103099,#103100,#103101,#103102),
 .UNSPECIFIED.,.F.,.F.,(4,3,3,3,3,3,3,4),(51.3796734954663,52.2339441008552,
53.2194902159657,54.2050363310761,55.1905824461866,56.1761285612971,57.1616746764076,
57.6628588026459),.UNSPECIFIED.);
#24370=B_SPLINE_CURVE_WITH_KNOTS('',3,(#103107,#103108,#103109,#103110,
#103111,#103112,#103113,#103114,#103115,#103116,#103117,#103118,#103119,
#103120,#103121,#103122,#103123,#103124,#103125,#103126,#103127,#103128),
 .UNSPECIFIED.,.F.,.F.,(4,3,3,3,3,3,3,4),(-66.9243948206342,-66.0315897124018,
-65.0460435972913,-64.0604974821809,-63.0749513670704,-62.0894052519599,
-61.1038591368495,-60.6412095134546),.UNSPECIFIED.);
#24371=B_SPLINE_CURVE_WITH_KNOTS('',3,(#103129,#103130,#103131,#103132,
#103133,#103134,#103135,#103136,#103137,#103138,#103139,#103140,#103141,
#103142,#103143,#103144,#103145,#103146,#103147,#103148,#103149,#103150),
 .UNSPECIFIED.,.F.,.F.,(4,3,3,3,3,3,3,4),(57.6628588026459,58.147220791518,
59.1327669066285,60.118313021739,61.1038591368495,62.0894052519599,63.0749513670704,
63.9460441098255),.UNSPECIFIED.);
#24372=B_SPLINE_CURVE_WITH_KNOTS('',3,(#103156,#103157,#103158,#103159,
#103160,#103161,#103162,#103163,#103164),.UNSPECIFIED.,.F.,.F.,(4,1,1,1,
1,1,4),(72.2566310325653,72.71928065596,73.7048267710705,74.690372886181,
75.6759190012915,76.6614651164019,77.5529633284553),.UNSPECIFIED.);
#24373=B_SPLINE_CURVE_WITH_KNOTS('',3,(#103167,#103168,#103169,#103170,
#103171,#103172,#103173,#103174),.UNSPECIFIED.,.F.,.F.,(4,1,1,1,1,4),(72.2566310325652,
72.3710844049206,73.3566305200311,74.3421766351416,75.327722750252,76.3132688653625),
 .UNSPECIFIED.);
#24374=B_SPLINE_CURVE_WITH_KNOTS('',3,(#103179,#103180,#103181,#103182,
#103183,#103184,#103185,#103186,#103187,#103188),.UNSPECIFIED.,.F.,.F.,
(4,1,1,1,1,1,1,4),(65.9734457253856,66.8060039652972,67.7915500804077,68.7770961955181,
69.7626423106286,70.7481884257391,71.7337345408496,72.2566310325653),
 .UNSPECIFIED.);
#24375=B_SPLINE_CURVE_WITH_KNOTS('',3,(#103189,#103190,#103191,#103192,
#103193,#103194,#103195,#103196,#103197,#103198),.UNSPECIFIED.,.F.,.F.,
(4,1,1,1,1,1,1,4),(65.9734457253856,66.4578077142578,67.4433538293682,68.4288999444787,
69.4144460595892,70.3999921746997,71.3855382898101,72.2566310325652),
 .UNSPECIFIED.);
#24376=B_SPLINE_CURVE_WITH_KNOTS('',3,(#103203,#103204,#103205,#103206,
#103207,#103208,#103209,#103210,#103211,#103212,#103213),.UNSPECIFIED.,
 .F.,.F.,(4,1,1,1,1,1,1,1,4),(59.6902604182061,59.9071811595239,60.8927272746343,
61.8782733897448,62.8638195048553,63.8493656199658,64.8349117350762,65.8204578501867,
65.9734457253856),.UNSPECIFIED.);
#24377=B_SPLINE_CURVE_WITH_KNOTS('',3,(#103214,#103215,#103216,#103217,
#103218,#103219,#103220,#103221,#103222,#103223),.UNSPECIFIED.,.F.,.F.,
(4,1,1,1,1,1,1,4),(59.6902604182061,60.5445310235949,61.5300771387054,62.5156232538159,
63.5011693689263,64.4867154840368,65.4722615991473,65.9734457253856),
 .UNSPECIFIED.);
#24378=B_SPLINE_CURVE_WITH_KNOTS('',3,(#103228,#103229,#103230,#103231,
#103232,#103233,#103234,#103235,#103236,#103237),.UNSPECIFIED.,.F.,.F.,
(4,1,1,1,1,1,1,4),(53.4070751110265,53.993904468861,54.9794505839715,55.964996699082,
56.9505428141924,57.9360889293029,58.9216350444134,59.6902604182061),
 .UNSPECIFIED.);
#24379=B_SPLINE_CURVE_WITH_KNOTS('',3,(#103238,#103239,#103240,#103241,
#103242,#103243,#103244,#103245,#103246,#103247,#103248),.UNSPECIFIED.,
 .F.,.F.,(4,1,1,1,1,1,1,1,4),(53.4070751110265,53.6457082178216,54.6312543329321,
55.6168004480425,56.602346563153,57.5878926782635,58.573438793374,59.5589849084844,
59.6902604182061),.UNSPECIFIED.);
#24380=B_SPLINE_CURVE_WITH_KNOTS('',3,(#103253,#103254,#103255,#103256,
#103257,#103258,#103259,#103260,#103261,#103262),.UNSPECIFIED.,.F.,.F.,
(4,1,1,1,1,1,1,4),(47.1238898038469,48.0806277781982,49.0661738933086,50.0517200084191,
51.0372661235296,52.0228122386401,53.0083583537505,53.4070751110265),
 .UNSPECIFIED.);
#24381=B_SPLINE_CURVE_WITH_KNOTS('',3,(#103263,#103264,#103265,#103266,
#103267,#103268,#103269,#103270,#103271,#103272),.UNSPECIFIED.,.F.,.F.,
(4,1,1,1,1,1,1,4),(47.1238898038469,47.7324315271587,48.7179776422692,49.7035237573797,
50.6890698724902,51.6746159876006,52.6601621027111,53.4070751110265),
 .UNSPECIFIED.);
#24382=B_SPLINE_CURVE_WITH_KNOTS('',3,(#103277,#103278,#103279,#103280,
#103281,#103282,#103283,#103284,#103285,#103286,#103287),.UNSPECIFIED.,
 .F.,.F.,(4,1,1,1,1,1,1,1,4),(40.8407044966673,41.1818049724248,42.1673510875353,
43.1528972026458,44.1384433177563,45.1239894328667,46.1095355479772,47.0950816630877,
47.1238898038469),.UNSPECIFIED.);
#24383=B_SPLINE_CURVE_WITH_KNOTS('',3,(#103288,#103289,#103290,#103291,
#103292,#103293,#103294,#103295,#103296,#103297),.UNSPECIFIED.,.F.,.F.,
(4,1,1,1,1,1,1,4),(40.8407044966673,41.8191548364959,42.8047009516064,43.7902470667168,
44.7757931818273,45.7613392969378,46.7468854120483,47.1238898038469),
 .UNSPECIFIED.);
#24384=B_SPLINE_CURVE_WITH_KNOTS('',3,(#103302,#103303,#103304,#103305,
#103306,#103307,#103308,#103309,#103310,#103311),.UNSPECIFIED.,.F.,.F.,
(4,1,1,1,1,1,1,4),(34.5575191894877,35.268528281762,36.2540743968725,37.2396205119829,
38.2251666270934,39.2107127422039,40.1962588573144,40.8407044966673),
 .UNSPECIFIED.);
#24385=B_SPLINE_CURVE_WITH_KNOTS('',3,(#103312,#103313,#103314,#103315,
#103316,#103317,#103318,#103319,#103320,#103321,#103322),.UNSPECIFIED.,
 .F.,.F.,(4,1,1,1,1,1,1,1,4),(34.5575191894877,34.9203320307226,35.905878145833,
36.8914242609435,37.876970376054,38.8625164911645,39.8480626062749,40.8336087213854,
40.8407044966673),.UNSPECIFIED.);
#24386=B_SPLINE_CURVE_WITH_KNOTS('',3,(#103327,#103328,#103329,#103330,
#103331,#103332,#103333,#103334,#103335,#103336,#103337),.UNSPECIFIED.,
 .F.,.F.,(4,1,1,1,1,1,1,1,4),(28.2743338823081,28.3697054759887,29.3552515910991,
30.3407977062096,31.3263438213201,32.3118899364306,33.297436051541,34.2829821666515,
34.5575191894877),.UNSPECIFIED.);
#24387=B_SPLINE_CURVE_WITH_KNOTS('',3,(#103338,#103339,#103340,#103341,
#103342,#103343,#103344,#103345,#103346,#103347),.UNSPECIFIED.,.F.,.F.,
(4,1,1,1,1,1,1,4),(28.2743338823081,29.0070553400597,29.9926014551702,30.9781475702807,
31.9636936853911,32.9492398005016,33.9347859156121,34.5575191894877),
 .UNSPECIFIED.);
#24388=B_SPLINE_CURVE_WITH_KNOTS('',3,(#103352,#103353,#103354,#103355,
#103356,#103357,#103358,#103359,#103360,#103361),.UNSPECIFIED.,.F.,.F.,
(4,1,1,1,1,1,1,4),(21.9911485751285,22.4564287853258,23.4419749004363,24.4275210155468,
25.4130671306572,26.3986132457677,27.3841593608782,28.2743338823081),
 .UNSPECIFIED.);
#24389=B_SPLINE_CURVE_WITH_KNOTS('',3,(#103362,#103363,#103364,#103365,
#103366,#103367,#103368,#103369,#103370,#103371,#103372),.UNSPECIFIED.,
 .F.,.F.,(4,1,1,1,1,1,1,1,4),(21.9911485751285,22.1082325342864,23.0937786493969,
24.0793247645073,25.0648708796178,26.0504169947283,27.0359631098388,28.0215092249492,
28.2743338823081),.UNSPECIFIED.);
#24390=B_SPLINE_CURVE_WITH_KNOTS('',3,(#103377,#103378,#103379,#103380,
#103381,#103382,#103383,#103384,#103385,#103386),.UNSPECIFIED.,.F.,.F.,
(4,1,1,1,1,1,1,4),(15.7079632679489,16.543152094663,17.5286982097734,18.5142443248839,
19.4997904399944,20.4853365551049,21.4708826702153,21.9911485751285),
 .UNSPECIFIED.);
#24391=B_SPLINE_CURVE_WITH_KNOTS('',3,(#103387,#103388,#103389,#103390,
#103391,#103392,#103393,#103394,#103395,#103396),.UNSPECIFIED.,.F.,.F.,
(4,1,1,1,1,1,1,4),(15.7079632679489,16.1949558436235,17.180501958734,18.1660480738445,
19.151594188955,20.1371403040654,21.1226864191759,21.9911485751285),
 .UNSPECIFIED.);
#24392=B_SPLINE_CURVE_WITH_KNOTS('',3,(#103399,#103400,#103401,#103402,
#103403,#103404,#103405,#103406,#103407,#103408,#103409,#103410,#103411,
#103412,#103413,#103414,#103415,#103416,#103417,#103418,#103419,#103420,
#103421,#103422,#103423,#103424,#103425,#103426,#103427,#103428,#103429,
#103430,#103431,#103432,#103433,#103434,#103435,#103436,#103437,#103438,
#103439,#103440,#103441,#103442,#103443,#103444,#103445,#103446,#103447,
#103448,#103449,#103450,#103451,#103452,#103453,#103454,#103455,#103456,
#103457,#103458,#103459,#103460,#103461,#103462,#103463,#103464,#103465,
#103466,#103467,#103468,#103469,#103470,#103471,#103472,#103473,#103474,
#103475,#103476,#103477,#103478,#103479,#103480,#103481,#103482,#103483),
 .UNSPECIFIED.,.F.,.F.,(4,3,3,3,3,3,3,3,3,3,3,3,3,3,3,3,3,3,3,3,3,3,3,3,
3,3,3,3,4),(-0.366397579005812,-0.351492437457111,-0.333436272682045,-0.327541718423651,
-0.321586762936821,-0.302799537357183,-0.288072678932441,-0.281533577517853,
-0.277630627523778,-0.258213375235538,-0.238401773301456,-0.225047497465903,
-0.215841092287883,-0.212852466676624,-0.192423383237538,-0.184984669959245,
-0.165235867770824,-0.154908626035148,-0.149716784328444,-0.14604205573285,
-0.125631137691432,-0.104768267325392,-0.0837068564958923,-0.0753026362798158,
-0.0721925998946417,-0.0505573660781355,-0.0288673280700796,-0.00763422837764629,
0.),.UNSPECIFIED.);
#24393=B_SPLINE_CURVE_WITH_KNOTS('',3,(#103488,#103489,#103490,#103491,
#103492,#103493,#103494,#103495,#103496,#103497,#103498,#103499,#103500,
#103501,#103502,#103503,#103504,#103505,#103506,#103507,#103508,#103509,
#103510,#103511,#103512,#103513,#103514,#103515,#103516,#103517,#103518,
#103519,#103520,#103521,#103522,#103523,#103524,#103525,#103526,#103527,
#103528,#103529,#103530,#103531,#103532,#103533,#103534,#103535,#103536,
#103537,#103538,#103539,#103540,#103541,#103542,#103543,#103544,#103545,
#103546,#103547,#103548,#103549,#103550,#103551,#103552,#103553,#103554,
#103555,#103556,#103557,#103558,#103559,#103560,#103561,#103562,#103563,
#103564,#103565,#103566,#103567,#103568,#103569,#103570,#103571,#103572),
 .UNSPECIFIED.,.F.,.F.,(4,3,3,3,3,3,3,3,3,3,3,3,3,3,3,3,3,3,3,3,3,3,3,3,
3,3,3,3,4),(-0.364629307890707,-0.346303779262462,-0.324667498644849,-0.315327518859617,
-0.310804290329342,-0.289490472824316,-0.273816300085133,-0.265502635085818,
-0.261675347015529,-0.240939232650462,-0.220671164473983,-0.2065276460832,
-0.194625115085288,-0.191251266670405,-0.171660083226589,-0.164097090910852,
-0.143584954546996,-0.134293385868617,-0.12844412724776,-0.12395210201744,
-0.104508817089354,-0.0851257087077866,-0.066128864910575,-0.0618232941908036,
-0.0586106046312514,-0.040025091744189,-0.0217742516347645,-0.00410398101321869,
0.),.UNSPECIFIED.);
#24394=B_SPLINE_CURVE_WITH_KNOTS('',3,(#103861,#103862,#103863,#103864,
#103865,#103866,#103867,#103868,#103869,#103870),.UNSPECIFIED.,.F.,.F.,
(4,3,3,4),(63.9460441098255,64.0604974821809,65.0460435972913,65.9375418093447),
 .UNSPECIFIED.);
#24395=B_SPLINE_CURVE_WITH_KNOTS('',3,(#103872,#103873,#103874,#103875,
#103876,#103877,#103878,#103879,#103880,#103881,#103882,#103883,#103884,
#103885,#103886,#103887,#103888,#103889,#103890,#103891,#103892,#103893,
#103894,#103895,#103896,#103897,#103898,#103899,#103900,#103901,#103902,
#103903,#103904,#103905,#103906,#103907,#103908,#103909,#103910,#103911,
#103912,#103913,#103914,#103915,#103916,#103917,#103918,#103919,#103920,
#103921,#103922,#103923,#103924,#103925,#103926,#103927,#103928,#103929,
#103930,#103931,#103932,#103933,#103934,#103935,#103936,#103937,#103938,
#103939,#103940,#103941,#103942,#103943,#103944,#103945,#103946,#103947,
#103948,#103949,#103950,#103951,#103952,#103953,#103954,#103955,#103956),
 .UNSPECIFIED.,.F.,.F.,(4,3,3,3,3,3,3,3,3,3,3,3,3,3,3,3,3,3,3,3,3,3,3,3,
3,3,3,3,4),(-0.366397579005849,-0.351492437457149,-0.333436262306682,-0.327541704777944,
-0.321586765496969,-0.302799532896208,-0.288072675029088,-0.281533538088545,
-0.277630621502244,-0.258213363775523,-0.238401762886512,-0.225047489654695,
-0.215841075396366,-0.212852442823409,-0.192423360392375,-0.184984669959245,
-0.165235863076095,-0.154908621633839,-0.149716783504717,-0.146042055985856,
-0.125631132714399,-0.104768256578359,-0.0837068447019094,-0.075302640797004,
-0.072192607079805,-0.050557369643571,-0.0288673349885595,-0.00763425242218924,
0.),.UNSPECIFIED.);
#24396=B_SPLINE_CURVE_WITH_KNOTS('',3,(#103957,#103958,#103959,#103960,
#103961,#103962,#103963,#103964,#103965),.UNSPECIFIED.,.F.,.F.,(4,1,1,1,
1,1,4),(10.3757270560178,11.2672252680712,12.2527713831816,13.2383174982921,
14.2238636134026,15.2094097285131,15.7079632679489),.UNSPECIFIED.);
#24397=B_SPLINE_CURVE_WITH_KNOTS('',3,(#103970,#103971,#103972,#103973,
#103974,#103975,#103976,#103977,#103978,#103979,#103980,#103981,#103982,
#103983,#103984,#103985,#103986,#103987,#103988,#103989,#103990,#103991,
#103992,#103993,#103994,#103995,#103996,#103997,#103998,#103999,#104000,
#104001,#104002,#104003,#104004,#104005,#104006,#104007,#104008,#104009,
#104010,#104011,#104012,#104013,#104014,#104015,#104016,#104017,#104018,
#104019,#104020,#104021,#104022,#104023,#104024,#104025,#104026,#104027,
#104028,#104029,#104030,#104031,#104032,#104033,#104034,#104035,#104036,
#104037,#104038,#104039,#104040,#104041,#104042,#104043,#104044,#104045,
#104046,#104047,#104048,#104049,#104050,#104051,#104052,#104053,#104054),
 .UNSPECIFIED.,.F.,.F.,(4,3,3,3,3,3,3,3,3,3,3,3,3,3,3,3,3,3,3,3,3,3,3,3,
3,3,3,3,4),(-0.36462930789068,-0.346303779262419,-0.324667498272067,-0.31532752509782,
-0.310804291325662,-0.289490474122718,-0.273816301221235,-0.265502639044791,
-0.261675347994805,-0.240939235060111,-0.220671177737736,-0.206527656031014,
-0.194625131687881,-0.19125128131443,-0.171660108944315,-0.164097090910849,
-0.143584954546993,-0.13429339168817,-0.128444126445644,-0.123952101242017,
-0.104508818706052,-0.0851257018425322,-0.0661288408609016,-0.0618227582712816,
-0.0586105122485322,-0.0400249876887114,-0.0217741310135354,-0.00410383987904057,
0.),.UNSPECIFIED.);
#24398=B_SPLINE_CURVE_WITH_KNOTS('',3,(#104058,#104059,#104060,#104061,
#104062,#104063,#104064,#104065),.UNSPECIFIED.,.F.,.F.,(4,1,1,1,1,4),(11.6154215191106,
12.6009676342211,13.5865137493315,14.572059864442,15.5576059795525,15.7079632679489),
 .UNSPECIFIED.);
#24399=B_SPLINE_CURVE_WITH_KNOTS('',3,(#104354,#104355,#104356,#104357,
#104358,#104359,#104360),.UNSPECIFIED.,.F.,.F.,(4,3,4),(-68.0026819426228,
-67.0171358275123,-66.9243948206342),.UNSPECIFIED.);
#24400=B_SPLINE_CURVE_WITH_KNOTS('',3,(#104430,#104431,#104432,#104433,
#104434,#104435,#104436,#104437,#104438,#104439),.UNSPECIFIED.,.F.,.F.,
(4,3,3,4),(-4.09202352044854,-3.95310104254947,-2.9648257819121,-2.07317267331967),
 .UNSPECIFIED.);
#24401=B_SPLINE_CURVE_WITH_KNOTS('',3,(#104442,#104443,#104444,#104445,
#104446,#104447,#104448),.UNSPECIFIED.,.F.,.F.,(4,3,4),(0.,0.988275260637351,
1.12274180646091),.UNSPECIFIED.);
#24402=B_SPLINE_CURVE_WITH_KNOTS('',3,(#104453,#104454,#104455,#104456,
#104457,#104458,#104459,#104460,#104461,#104462,#104463,#104464,#104465,
#104466,#104467,#104468,#104469,#104470,#104471,#104472,#104473,#104474),
 .UNSPECIFIED.,.F.,.F.,(4,3,3,3,3,3,3,4),(-10.3752088276281,-9.88275260637366,
-8.8944773457363,-7.90620208509893,-6.91792682446157,-5.9296515638242,-4.94137630318683,
-4.09202352044854),.UNSPECIFIED.);
#24403=B_SPLINE_CURVE_WITH_KNOTS('',3,(#104475,#104476,#104477,#104478,
#104479,#104480,#104481,#104482,#104483,#104484,#104485,#104486,#104487,
#104488,#104489,#104490,#104491,#104492,#104493,#104494,#104495,#104496),
 .UNSPECIFIED.,.F.,.F.,(4,3,3,3,3,3,3,4),(1.12274180646091,1.97655052127471,
2.96482578191208,3.95310104254944,4.94137630318681,5.92965156382417,6.91792682446154,
7.40592711364053),.UNSPECIFIED.);
#24404=B_SPLINE_CURVE_WITH_KNOTS('',3,(#104501,#104502,#104503,#104504,
#104505,#104506,#104507,#104508,#104509,#104510,#104511,#104512,#104513,
#104514,#104515,#104516,#104517,#104518,#104519,#104520,#104521,#104522),
 .UNSPECIFIED.,.F.,.F.,(4,3,3,3,3,3,3,4),(-16.6583941348077,-15.8124041701979,
-14.8241289095605,-13.8358536489231,-12.8475783882858,-11.8593031276484,
-10.871027867011,-10.3752088276281),.UNSPECIFIED.);
#24405=B_SPLINE_CURVE_WITH_KNOTS('',3,(#104523,#104524,#104525,#104526,
#104527,#104528,#104529,#104530,#104531,#104532,#104533,#104534,#104535,
#104536,#104537,#104538,#104539,#104540,#104541,#104542,#104543,#104544),
 .UNSPECIFIED.,.F.,.F.,(4,3,3,3,3,3,3,4),(7.40592711364053,7.9062020850989,
8.89447734573626,9.88275260637363,10.871027867011,11.8593031276484,12.8475783882857,
13.6891124208201),.UNSPECIFIED.);
#24406=B_SPLINE_CURVE_WITH_KNOTS('',3,(#104549,#104550,#104551,#104552,
#104553,#104554,#104555,#104556,#104557,#104558,#104559,#104560,#104561,
#104562,#104563,#104564,#104565,#104566,#104567,#104568,#104569,#104570,
#104571,#104572,#104573),.UNSPECIFIED.,.F.,.F.,(4,3,3,3,3,3,3,3,4),(-22.9415794419873,
-22.7303309946594,-21.742055734022,-20.7537804733847,-19.7655052127473,
-18.77722995211,-17.7889546914726,-16.8006794308352,-16.6583941348077),
 .UNSPECIFIED.);
#24407=B_SPLINE_CURVE_WITH_KNOTS('',3,(#104574,#104575,#104576,#104577,
#104578,#104579,#104580,#104581,#104582,#104583,#104584,#104585,#104586,
#104587,#104588,#104589,#104590,#104591,#104592,#104593,#104594,#104595,
#104596,#104597,#104598),.UNSPECIFIED.,.F.,.F.,(4,3,3,3,3,3,3,3,4),(13.6891124208201,
13.8358536489231,14.8241289095605,15.8124041701978,16.8006794308352,17.7889546914725,
18.7772299521099,19.7655052127473,19.9722977279997),.UNSPECIFIED.);
#24408=B_SPLINE_CURVE_WITH_KNOTS('',3,(#104603,#104604,#104605,#104606,
#104607,#104608,#104609,#104610,#104611,#104612,#104613,#104614,#104615,
#104616,#104617,#104618,#104619,#104620,#104621,#104622,#104623,#104624),
 .UNSPECIFIED.,.F.,.F.,(4,3,3,3,3,3,3,4),(-29.2247647491669,-28.6599825584836,
-27.6717072978462,-26.6834320372089,-25.6951567765715,-24.7068815159341,
-23.7186062552968,-22.9415794419873),.UNSPECIFIED.);
#24409=B_SPLINE_CURVE_WITH_KNOTS('',3,(#104625,#104626,#104627,#104628,
#104629,#104630,#104631,#104632,#104633,#104634,#104635,#104636,#104637,
#104638,#104639,#104640,#104641,#104642,#104643,#104644,#104645,#104646),
 .UNSPECIFIED.,.F.,.F.,(4,3,3,3,3,3,3,4),(19.9722977279997,20.7537804733846,
21.742055734022,22.7303309946594,23.7186062552967,24.7068815159341,25.6951567765715,
26.2554830351793),.UNSPECIFIED.);
#24410=B_SPLINE_CURVE_WITH_KNOTS('',3,(#104652,#104653,#104654,#104655,
#104656,#104657,#104658,#104659,#104660),.UNSPECIFIED.,.F.,.F.,(4,1,1,1,
1,1,4),(34.5575191894877,35.3345460027972,36.3228212634346,37.311096524072,
38.2993717847093,39.2876470453467,40.1793001539391),.UNSPECIFIED.);
#24411=B_SPLINE_CURVE_WITH_KNOTS('',3,(#104663,#104664,#104665,#104666,
#104667,#104668,#104669,#104670),.UNSPECIFIED.,.F.,.F.,(4,1,1,1,1,4),(34.5575191894877,
34.9854681915173,35.9737434521546,36.962018712792,37.9502939734294,38.9385692340667),
 .UNSPECIFIED.);
#24412=B_SPLINE_CURVE_WITH_KNOTS('',3,(#104675,#104676,#104677,#104678,
#104679,#104680,#104681,#104682,#104683,#104684,#104685),.UNSPECIFIED.,
 .F.,.F.,(4,1,1,1,1,1,1,1,4),(28.2743338823081,28.4166191783357,29.404894438973,
30.3931696996104,31.3814449602478,32.3697202208851,33.3579954815225,34.3462707421599,
34.5575191894877),.UNSPECIFIED.);
#24413=B_SPLINE_CURVE_WITH_KNOTS('',3,(#104686,#104687,#104688,#104689,
#104690,#104691,#104692,#104693,#104694,#104695),.UNSPECIFIED.,.F.,.F.,
(4,1,1,1,1,1,1,4),(28.2743338823081,29.0558166276931,30.0440918883304,31.0323671489678,
32.0206424096052,33.0089176702425,33.9971929308799,34.5575191894877),
 .UNSPECIFIED.);
#24414=B_SPLINE_CURVE_WITH_KNOTS('',3,(#104700,#104701,#104702,#104703,
#104704,#104705,#104706,#104707,#104708,#104709),.UNSPECIFIED.,.F.,.F.,
(4,1,1,1,1,1,1,4),(21.9911485751285,22.4869676145115,23.4752428751488,24.4635181357862,
25.4517933964236,26.4400686570609,27.4283439176983,28.2743338823081),
 .UNSPECIFIED.);
#24415=B_SPLINE_CURVE_WITH_KNOTS('',3,(#104710,#104711,#104712,#104713,
#104714,#104715,#104716,#104717,#104718,#104719,#104720),.UNSPECIFIED.,
 .F.,.F.,(4,1,1,1,1,1,1,1,4),(21.9911485751285,22.1378898032315,23.1261650638689,
24.1144403245063,25.1027155851436,26.090990845781,27.0792661064184,28.0675413670557,
28.2743338823081),.UNSPECIFIED.);
#24416=B_SPLINE_CURVE_WITH_KNOTS('',3,(#104725,#104726,#104727,#104728,
#104729,#104730,#104731,#104732,#104733,#104734),.UNSPECIFIED.,.F.,.F.,
(4,1,1,1,1,1,1,4),(15.707963267949,16.5573160506873,17.5455913113246,18.533866571962,
19.5221418325994,20.5104170932367,21.4986923538741,21.9911485751285),
 .UNSPECIFIED.);
#24417=B_SPLINE_CURVE_WITH_KNOTS('',3,(#104735,#104736,#104737,#104738,
#104739,#104740,#104741,#104742,#104743,#104744),.UNSPECIFIED.,.F.,.F.,
(4,1,1,1,1,1,1,4),(15.707963267949,16.2082382394074,17.1965135000447,18.1847887606821,
19.1730640213194,20.1613392819568,21.1496145425942,21.9911485751285),
 .UNSPECIFIED.);
#24418=B_SPLINE_CURVE_WITH_KNOTS('',3,(#104747,#104748,#104749,#104750,
#104751,#104752,#104753,#104754,#104755,#104756,#104757,#104758,#104759,
#104760,#104761,#104762,#104763,#104764,#104765,#104766,#104767,#104768,
#104769,#104770,#104771,#104772,#104773,#104774,#104775,#104776,#104777,
#104778,#104779,#104780,#104781,#104782,#104783,#104784,#104785,#104786,
#104787,#104788,#104789,#104790,#104791,#104792,#104793,#104794,#104795,
#104796,#104797,#104798,#104799,#104800,#104801,#104802,#104803,#104804,
#104805,#104806,#104807,#104808,#104809,#104810,#104811,#104812,#104813,
#104814,#104815,#104816,#104817,#104818,#104819,#104820,#104821,#104822,
#104823,#104824,#104825,#104826,#104827,#104828,#104829,#104830,#104831),
 .UNSPECIFIED.,.F.,.F.,(4,3,3,3,3,3,3,3,3,3,3,3,3,3,3,3,3,3,3,3,3,3,3,3,
3,3,3,3,4),(-0.276631791712739,-0.2650508057708,-0.250374720050919,-0.244981738899123,
-0.241597861612783,-0.226325618458574,-0.215430745967583,-0.211433653093672,
-0.208367227284489,-0.192603496037899,-0.17655849488178,-0.167210530793996,
-0.162395519488002,-0.159507286270078,-0.142982525939046,-0.139166638530642,
-0.123190507759063,-0.115491101024122,-0.110579056300749,-0.107660356137215,
-0.0911092121152923,-0.0741979921205997,-0.0647231249881659,-0.0582712594123912,
-0.0537680561212596,-0.0363099737577034,-0.0181549868788517,-0.00111529705586954,
0.),.UNSPECIFIED.);
#24419=B_SPLINE_CURVE_WITH_KNOTS('',3,(#104836,#104837,#104838,#104839,
#104840,#104841,#104842,#104843,#104844,#104845,#104846,#104847,#104848,
#104849,#104850,#104851,#104852,#104853,#104854,#104855,#104856,#104857,
#104858,#104859,#104860,#104861,#104862,#104863,#104864,#104865,#104866,
#104867,#104868,#104869,#104870,#104871,#104872,#104873,#104874,#104875,
#104876,#104877,#104878,#104879,#104880,#104881,#104882,#104883,#104884,
#104885,#104886,#104887,#104888,#104889,#104890,#104891,#104892,#104893,
#104894,#104895,#104896,#104897,#104898,#104899,#104900,#104901,#104902,
#104903,#104904,#104905,#104906,#104907,#104908,#104909,#104910,#104911,
#104912,#104913,#104914,#104915,#104916,#104917),.UNSPECIFIED.,.F.,.F.,
(4,3,3,3,3,3,3,3,3,3,3,3,3,3,3,3,3,3,3,3,3,3,3,3,3,3,3,4),(-0.275362278356874,
-0.261262622338533,-0.2441203930908,-0.237319173909909,-0.233882184799267,
-0.216686330248896,-0.205116137512367,-0.199379448294571,-0.195960066979035,
-0.179209945634759,-0.162881771419966,-0.153192525654141,-0.147976391807739,
-0.144164595227973,-0.128304665621163,-0.124124788356664,-0.108305429308661,
-0.100913932577369,-0.0956636604654543,-0.0926065387289381,-0.07684180355915,
-0.0611561838178058,-0.0532978747976696,-0.0475122493766209,-0.0447132850322838,
-0.0296095890058339,-0.014804794502917,0.),.UNSPECIFIED.);
#24420=B_SPLINE_CURVE_WITH_KNOTS('',3,(#105054,#105055,#105056,#105057,
#105058,#105059,#105060,#105061,#105062,#105063),.UNSPECIFIED.,.F.,.F.,
(4,3,3,4),(26.2554830351793,26.6834320372088,27.6717072978462,28.5633604064386),
 .UNSPECIFIED.);
#24421=B_SPLINE_CURVE_WITH_KNOTS('',3,(#105065,#105066,#105067,#105068,
#105069,#105070,#105071,#105072,#105073,#105074,#105075,#105076,#105077,
#105078,#105079,#105080,#105081,#105082,#105083,#105084,#105085,#105086,
#105087,#105088,#105089,#105090,#105091,#105092,#105093,#105094,#105095,
#105096,#105097,#105098,#105099,#105100,#105101,#105102,#105103,#105104,
#105105,#105106,#105107,#105108,#105109,#105110,#105111,#105112,#105113,
#105114,#105115,#105116,#105117,#105118,#105119,#105120,#105121,#105122,
#105123,#105124,#105125,#105126,#105127,#105128,#105129,#105130,#105131,
#105132,#105133,#105134,#105135,#105136,#105137,#105138,#105139,#105140,
#105141,#105142,#105143,#105144,#105145,#105146,#105147,#105148,#105149),
 .UNSPECIFIED.,.F.,.F.,(4,3,3,3,3,3,3,3,3,3,3,3,3,3,3,3,3,3,3,3,3,3,3,3,
3,3,3,3,4),(-0.276631791712748,-0.265050805770798,-0.250374723435734,-0.244981746785586,
-0.241597874545741,-0.226325633648081,-0.215430759258399,-0.211433696526451,
-0.208367237866174,-0.19260350809475,-0.176558506096897,-0.16721053920533,
-0.162395532418839,-0.159507299794083,-0.142982538633566,-0.139166638530629,
-0.12319050981671,-0.115491102953166,-0.110579056502434,-0.107660355608141,
-0.0911092140004719,-0.0741979961655583,-0.0647231241069456,-0.0582712562698588,
-0.0537680567287938,-0.0363099755898647,-0.0181549877949324,-0.00111528832129344,
0.),.UNSPECIFIED.);
#24422=B_SPLINE_CURVE_WITH_KNOTS('',3,(#105150,#105151,#105152,#105153,
#105154,#105155,#105156,#105157,#105158),.UNSPECIFIED.,.F.,.F.,(4,1,1,1,
1,1,4),(10.3752088276281,11.2668619362205,12.2551371968579,13.2434124574953,
14.2316877181326,15.21996297877,15.707963267949),.UNSPECIFIED.);
#24423=B_SPLINE_CURVE_WITH_KNOTS('',3,(#105164,#105165,#105166,#105167,
#105168,#105169,#105170,#105171,#105172,#105173,#105174,#105175,#105176,
#105177,#105178,#105179,#105180,#105181,#105182,#105183,#105184,#105185,
#105186,#105187,#105188,#105189,#105190,#105191,#105192,#105193,#105194,
#105195,#105196,#105197,#105198,#105199,#105200,#105201,#105202,#105203,
#105204,#105205,#105206,#105207,#105208,#105209,#105210,#105211,#105212,
#105213,#105214,#105215,#105216,#105217,#105218,#105219,#105220,#105221,
#105222,#105223,#105224,#105225,#105226,#105227,#105228,#105229,#105230,
#105231,#105232,#105233,#105234,#105235,#105236,#105237,#105238,#105239,
#105240,#105241,#105242,#105243,#105244,#105245),.UNSPECIFIED.,.F.,.F.,
(4,3,3,3,3,3,3,3,3,3,3,3,3,3,3,3,3,3,3,3,3,3,3,3,3,3,3,4),(-0.275362278356834,
-0.26126262233849,-0.244120393090759,-0.237319172495777,-0.233882181431016,
-0.216686326788785,-0.205116134484767,-0.199379437148685,-0.195960065205097,
-0.179209943129133,-0.162881764024476,-0.153192520107518,-0.147976388388869,
-0.144164594732856,-0.128304660393989,-0.124124788356646,-0.108305426694355,
-0.10091392976967,-0.0956636612369917,-0.0926065395413023,-0.0768418040865203,
-0.0611561896722693,-0.0532978771833044,-0.0475122544869175,-0.0447132896032582,
-0.0296096002398782,-0.0148048001199391,0.),.UNSPECIFIED.);
#24424=B_SPLINE_CURVE_WITH_KNOTS('',3,(#105248,#105249,#105250,#105251,
#105252,#105253,#105254,#105255),.UNSPECIFIED.,.F.,.F.,(4,1,1,1,1,4),(11.6159397475005,
12.6042150081378,13.5924902687752,14.5807655294126,15.5690407900499,15.707963267949),
 .UNSPECIFIED.);
#24425=B_SPLINE_CURVE_WITH_KNOTS('',3,(#105392,#105393,#105394,#105395,
#105396,#105397,#105398),.UNSPECIFIED.,.F.,.F.,(4,3,4),(-30.6365330797583,
-29.648257819121,-29.2247647491669),.UNSPECIFIED.);
#24426=B_SPLINE_CURVE_WITH_KNOTS('',3,(#105568,#105569,#105570,#105571,
#105572,#105573,#105574,#105575,#105576,#105577),.UNSPECIFIED.,.F.,.F.,
(4,3,3,4),(-4.09157007060749,-3.98296996538366,-2.98722747403775,-2.06546402602184),
 .UNSPECIFIED.);
#24427=B_SPLINE_CURVE_WITH_KNOTS('',3,(#105580,#105581,#105582,#105583,
#105584,#105585,#105586),.UNSPECIFIED.,.F.,.F.,(4,3,4),(0.,0.995742491345911,
1.11548660900407),.UNSPECIFIED.);
#24428=B_SPLINE_CURVE_WITH_KNOTS('',3,(#105591,#105592,#105593,#105594,
#105595,#105596,#105597,#105598,#105599,#105600,#105601,#105602,#105603,
#105604,#105605,#105606,#105607,#105608,#105609,#105610,#105611,#105612),
 .UNSPECIFIED.,.F.,.F.,(4,3,3,3,3,3,3,4),(-10.3747553777871,-9.95742491345914,
-8.96168242211323,-7.96593993076731,-6.9701974394214,-5.97445494807549,
-4.97871245672958,-4.09157007060749),.UNSPECIFIED.);
#24429=B_SPLINE_CURVE_WITH_KNOTS('',3,(#105613,#105614,#105615,#105616,
#105617,#105618,#105619,#105620,#105621,#105622,#105623,#105624,#105625,
#105626,#105627,#105628,#105629,#105630,#105631,#105632,#105633,#105634),
 .UNSPECIFIED.,.F.,.F.,(4,3,3,3,3,3,3,4),(1.11548660900407,1.99148498269182,
2.98722747403774,3.98296996538365,4.97871245672956,5.97445494807547,6.97019743942139,
7.39867191618366),.UNSPECIFIED.);
#24430=B_SPLINE_CURVE_WITH_KNOTS('',3,(#105639,#105640,#105641,#105642,
#105643,#105644,#105645,#105646,#105647,#105648,#105649,#105650,#105651,
#105652,#105653,#105654,#105655,#105656,#105657,#105658,#105659,#105660),
 .UNSPECIFIED.,.F.,.F.,(4,3,3,3,3,3,3,4),(-16.6579406849667,-15.9318798615346,
-14.9361373701887,-13.9403948788428,-12.9446523874969,-11.948909896151,
-10.9531674048051,-10.3747553777871),.UNSPECIFIED.);
#24431=B_SPLINE_CURVE_WITH_KNOTS('',3,(#105661,#105662,#105663,#105664,
#105665,#105666,#105667,#105668,#105669,#105670,#105671,#105672,#105673,
#105674,#105675,#105676,#105677,#105678,#105679,#105680,#105681,#105682),
 .UNSPECIFIED.,.F.,.F.,(4,3,3,3,3,3,3,4),(7.39867191618366,7.9659399307673,
8.96168242211322,9.95742491345913,10.953167404805,11.948909896151,12.9446523874969,
13.6818572233633),.UNSPECIFIED.);
#24432=B_SPLINE_CURVE_WITH_KNOTS('',3,(#105689,#105690,#105691,#105692,
#105693,#105694,#105695,#105696,#105697,#105698,#105699,#105700,#105701,
#105702,#105703,#105704,#105705,#105706,#105707,#105708,#105709,#105710),
 .UNSPECIFIED.,.F.,.F.,(4,3,3,3,3,3,3,4),(-22.902077300956,-21.9063348096101,
-20.9105923182642,-19.9148498269183,-18.9191073355724,-17.9233648442264,
-16.9276223528805,-16.6579406849667),.UNSPECIFIED.);
#24433=B_SPLINE_CURVE_WITH_KNOTS('',3,(#105711,#105712,#105713,#105714,
#105715,#105716,#105717,#105718,#105719,#105720,#105721,#105722,#105723,
#105724,#105725,#105726,#105727,#105728,#105729,#105730,#105731,#105732,
#105733,#105734,#105735),.UNSPECIFIED.,.F.,.F.,(4,3,3,3,3,3,3,3,4),(13.6818572233633,
13.9403948788428,14.9361373701887,15.9318798615346,16.9276223528805,17.9233648442264,
18.9191073355724,19.9148498269183,19.9650425305428),.UNSPECIFIED.);
#24434=B_SPLINE_CURVE_WITH_KNOTS('',3,(#105741,#105742,#105743,#105744,
#105745,#105746,#105747,#105748),.UNSPECIFIED.,.F.,.F.,(4,1,1,1,1,4),(28.2743338823082,
28.544015550222,29.5397580415679,30.5355005329138,31.5312430242597,32.4530064722757),
 .UNSPECIFIED.);
#24435=B_SPLINE_CURVE_WITH_KNOTS('',3,(#105751,#105752,#105753,#105754,
#105755,#105756),.UNSPECIFIED.,.F.,.F.,(4,1,1,4),(28.2743338823082,29.2198836700295,
30.2156261613754,31.2113686527213),.UNSPECIFIED.);
#24436=B_SPLINE_CURVE_WITH_KNOTS('',3,(#105761,#105762,#105763,#105764,
#105765,#105766,#105767,#105768,#105769,#105770),.UNSPECIFIED.,.F.,.F.,
(4,1,1,1,1,1,1,4),(21.9911485751286,22.5695606021465,23.5653030934924,24.5610455848383,
25.5567880761843,26.5525305675302,27.5482730588761,28.2743338823082),
 .UNSPECIFIED.);
#24437=B_SPLINE_CURVE_WITH_KNOTS('',3,(#105771,#105772,#105773,#105774,
#105775,#105776,#105777,#105778,#105779,#105780,#105781),.UNSPECIFIED.,
 .F.,.F.,(4,1,1,1,1,1,1,1,4),(21.9911485751286,22.2496862306081,23.245428721954,
24.2411712132999,25.2369137046458,26.2326561959917,27.2283986873376,28.2241411786836,
28.2743338823082),.UNSPECIFIED.);
#24438=B_SPLINE_CURVE_WITH_KNOTS('',3,(#105786,#105787,#105788,#105789,
#105790,#105791,#105792,#105793,#105794,#105795),.UNSPECIFIED.,.F.,.F.,
(4,1,1,1,1,1,1,4),(15.707963267949,16.595105654071,17.590848145417,18.5865906367629,
19.5823331281088,20.5780756194547,21.5738181108006,21.9911485751286),
 .UNSPECIFIED.);
#24439=B_SPLINE_CURVE_WITH_KNOTS('',3,(#105796,#105797,#105798,#105799,
#105800,#105801,#105802,#105803,#105804,#105805),.UNSPECIFIED.,.F.,.F.,
(4,1,1,1,1,1,1,4),(15.707963267949,16.2752312825326,17.2709737738785,18.2667162652244,
19.2624587565703,20.2582012479163,21.2539437392622,21.9911485751286),
 .UNSPECIFIED.);
#24440=B_SPLINE_CURVE_WITH_KNOTS('',3,(#105807,#105808,#105809,#105810,
#105811,#105812,#105813,#105814,#105815,#105816,#105817,#105818,#105819,
#105820,#105821,#105822,#105823,#105824,#105825,#105826,#105827,#105828,
#105829,#105830,#105831,#105832,#105833,#105834,#105835,#105836,#105837,
#105838,#105839,#105840,#105841,#105842,#105843,#105844,#105845,#105846,
#105847,#105848,#105849,#105850,#105851,#105852,#105853,#105854,#105855,
#105856,#105857,#105858,#105859,#105860,#105861,#105862,#105863,#105864,
#105865,#105866,#105867,#105868,#105869,#105870,#105871,#105872,#105873,
#105874,#105875,#105876,#105877,#105878,#105879),.UNSPECIFIED.,.F.,.F.,
(4,3,3,3,3,3,3,3,3,3,3,3,3,3,3,3,3,3,3,3,3,3,3,3,4),(-0.178587760439472,
-0.172997303911014,-0.162856682864992,-0.158716158534057,-0.156203682331329,
-0.145417506956393,-0.137581747775137,-0.135179453906191,-0.123829626631807,
-0.112395948228162,-0.106524699914796,-0.103647422367158,-0.0918723355428386,
-0.0803882935999837,-0.0750511880536326,-0.0723197039144465,-0.0701559845024732,
-0.058210449571605,-0.0459784728235496,-0.0402311637206059,-0.0370748175850279,
-0.0346544230216544,-0.0219633623116217,-0.0093557654079626,0.),
 .UNSPECIFIED.);
#24441=B_SPLINE_CURVE_WITH_KNOTS('',3,(#105882,#105883,#105884,#105885,
#105886,#105887,#105888,#105889,#105890,#105891,#105892,#105893,#105894,
#105895,#105896,#105897,#105898,#105899,#105900,#105901,#105902,#105903,
#105904,#105905,#105906,#105907,#105908,#105909,#105910,#105911,#105912,
#105913,#105914,#105915,#105916,#105917,#105918,#105919,#105920,#105921,
#105922,#105923,#105924,#105925,#105926,#105927,#105928,#105929,#105930,
#105931,#105932,#105933,#105934,#105935,#105936,#105937,#105938,#105939,
#105940,#105941,#105942,#105943,#105944,#105945,#105946,#105947,#105948,
#105949,#105950,#105951,#105952,#105953,#105954,#105955,#105956,#105957),
 .UNSPECIFIED.,.F.,.F.,(4,3,3,3,3,3,3,3,3,3,3,3,3,3,3,3,3,3,3,3,3,3,3,3,
3,4),(-0.177567088092108,-0.170427641780406,-0.159117078668393,-0.152710961416868,
-0.149808705938898,-0.137348063727474,-0.130172447872078,-0.127139016091628,
-0.12464907937053,-0.11270555837298,-0.1010409933116,-0.0954973026492411,
-0.093049358993514,-0.0906377927723942,-0.079943136884305,-0.0699502447737669,
-0.0648815661545737,-0.0614861704592656,-0.0586741810352214,-0.0474857631257267,
-0.0364249809192207,-0.0314310426811734,-0.0291079279156276,-0.0185054507233679,
-0.00828997057237845,0.),.UNSPECIFIED.);
#24442=B_SPLINE_CURVE_WITH_KNOTS('',3,(#106062,#106063,#106064,#106065),
 .UNSPECIFIED.,.F.,.F.,(4,4),(19.9650425305428,20.8366132749342),
 .UNSPECIFIED.);
#24443=B_SPLINE_CURVE_WITH_KNOTS('',3,(#106067,#106068,#106069,#106070,
#106071,#106072,#106073,#106074,#106075,#106076,#106077,#106078,#106079,
#106080,#106081,#106082,#106083,#106084,#106085,#106086,#106087,#106088,
#106089,#106090,#106091,#106092,#106093,#106094,#106095,#106096,#106097,
#106098,#106099,#106100,#106101,#106102,#106103,#106104,#106105,#106106,
#106107,#106108,#106109,#106110,#106111,#106112,#106113,#106114,#106115,
#106116,#106117,#106118,#106119,#106120,#106121,#106122,#106123,#106124,
#106125,#106126,#106127,#106128,#106129,#106130,#106131,#106132,#106133,
#106134,#106135,#106136,#106137,#106138,#106139),.UNSPECIFIED.,.F.,.F.,
(4,3,3,3,3,3,3,3,3,3,3,3,3,3,3,3,3,3,3,3,3,3,3,3,4),(-0.178587760439474,
-0.172997303911017,-0.162856682864998,-0.158716160609124,-0.156203687475286,
-0.145417513860255,-0.137581761131997,-0.135179479570029,-0.123829652805094,
-0.112395973547909,-0.106524733023587,-0.103647430899797,-0.0918723355428663,
-0.080388293600008,-0.0750511865962201,-0.0723196871235457,-0.070155957327666,
-0.0582104228184783,-0.0459784469741407,-0.0402311411023731,-0.0370747430924057,
-0.0346543091754803,-0.021963248077658,-0.00935564841229983,0.),
 .UNSPECIFIED.);
#24444=B_SPLINE_CURVE_WITH_KNOTS('',3,(#106140,#106141,#106142,#106143,
#106144,#106145,#106146,#106147,#106148),.UNSPECIFIED.,.F.,.F.,(4,1,1,1,
1,1,4),(10.3747553777871,11.296518825803,12.2922613171489,13.2880038084949,
14.2837462998408,15.2794887911867,15.707963267949),.UNSPECIFIED.);
#24445=B_SPLINE_CURVE_WITH_KNOTS('',3,(#106154,#106155,#106156,#106157,
#106158,#106159,#106160,#106161,#106162,#106163,#106164,#106165,#106166,
#106167,#106168,#106169,#106170,#106171,#106172,#106173,#106174,#106175,
#106176,#106177,#106178,#106179,#106180,#106181,#106182,#106183,#106184,
#106185,#106186,#106187,#106188,#106189,#106190,#106191,#106192,#106193,
#106194,#106195,#106196,#106197,#106198,#106199,#106200,#106201,#106202,
#106203,#106204,#106205,#106206,#106207,#106208,#106209,#106210,#106211,
#106212,#106213,#106214,#106215,#106216,#106217,#106218,#106219,#106220,
#106221,#106222,#106223,#106224,#106225,#106226,#106227,#106228,#106229),
 .UNSPECIFIED.,.F.,.F.,(4,3,3,3,3,3,3,3,3,3,3,3,3,3,3,3,3,3,3,3,3,3,3,3,
3,4),(-0.177567088092073,-0.170427641780375,-0.159117078668367,-0.15271096033015,
-0.149808704260947,-0.137348061616469,-0.13017244602495,-0.127139026932459,
-0.124649081110899,-0.112705557810677,-0.101040988585173,-0.0954972972813229,
-0.0930493469528739,-0.0906377909408365,-0.079943136884317,-0.0699502447737774,
-0.06488156611803,-0.061486171730566,-0.058674181915544,-0.047485764632209,
-0.0364249872579639,-0.0314310514931735,-0.0291079329386753,-0.0185054606443194,
-0.00828998776203388,0.),.UNSPECIFIED.);
#24446=B_SPLINE_CURVE_WITH_KNOTS('',3,(#106232,#106233,#106234,#106235,
#106236,#106237,#106238,#106239),.UNSPECIFIED.,.F.,.F.,(4,1,1,1,1,4),(11.6163931973415,
12.6121356886874,13.6078781800333,14.6036206713792,15.5993631627251,15.707963267949),
 .UNSPECIFIED.);
#24447=B_SPLINE_CURVE_WITH_KNOTS('',3,(#106513,#106514,#106515,#106516,
#106517,#106518,#106519,#106520,#106521,#106522),.UNSPECIFIED.,.F.,.F.,
(4,3,3,4),(-4.09202352044855,-3.96148666219335,-2.97111499664502,-2.07317267331975),
 .UNSPECIFIED.);
#24448=B_SPLINE_CURVE_WITH_KNOTS('',3,(#106525,#106526,#106527,#106528,
#106529,#106530,#106531),.UNSPECIFIED.,.F.,.F.,(4,3,4),(0.,0.990371665548332,
1.12274180646094),.UNSPECIFIED.);
#24449=B_SPLINE_CURVE_WITH_KNOTS('',3,(#106536,#106537,#106538,#106539,
#106540,#106541,#106542,#106543,#106544,#106545,#106546,#106547,#106548,
#106549,#106550,#106551,#106552,#106553,#106554,#106555,#106556,#106557),
 .UNSPECIFIED.,.F.,.F.,(4,3,3,3,3,3,3,4),(-10.3752088276281,-9.90371665548338,
-8.91334498993504,-7.9229733243867,-6.93260165883837,-5.94222999329003,
-4.95185832774169,-4.09202352044855),.UNSPECIFIED.);
#24450=B_SPLINE_CURVE_WITH_KNOTS('',3,(#106558,#106559,#106560,#106561,
#106562,#106563,#106564,#106565,#106566,#106567,#106568,#106569,#106570,
#106571,#106572,#106573,#106574,#106575,#106576,#106577,#106578,#106579),
 .UNSPECIFIED.,.F.,.F.,(4,3,3,3,3,3,3,4),(1.12274180646094,1.98074333109667,
2.97111499664501,3.96148666219335,4.95185832774168,5.94222999329002,6.93260165883836,
7.40592711364053),.UNSPECIFIED.);
#24451=B_SPLINE_CURVE_WITH_KNOTS('',3,(#106584,#106585,#106586,#106587,
#106588,#106589,#106590,#106591,#106592,#106593,#106594,#106595,#106596,
#106597,#106598,#106599,#106600,#106601,#106602,#106603,#106604,#106605),
 .UNSPECIFIED.,.F.,.F.,(4,3,3,3,3,3,3,4),(-16.6583941348077,-15.8459466487734,
-14.8555749832251,-13.8652033176767,-12.8748316521284,-11.8844599865801,
-10.8940883210317,-10.3752088276281),.UNSPECIFIED.);
#24452=B_SPLINE_CURVE_WITH_KNOTS('',3,(#106606,#106607,#106608,#106609,
#106610,#106611,#106612,#106613,#106614,#106615,#106616,#106617,#106618,
#106619,#106620,#106621,#106622,#106623,#106624,#106625,#106626,#106627),
 .UNSPECIFIED.,.F.,.F.,(4,3,3,3,3,3,3,4),(7.40592711364053,7.92297332438669,
8.91334498993503,9.90371665548337,10.8940883210317,11.88445998658,12.8748316521284,
13.6891124208201),.UNSPECIFIED.);
#24453=B_SPLINE_CURVE_WITH_KNOTS('',3,(#106632,#106633,#106634,#106635,
#106636,#106637,#106638,#106639,#106640,#106641,#106642,#106643,#106644,
#106645,#106646,#106647,#106648,#106649,#106650,#106651,#106652,#106653,
#106654,#106655,#106656),.UNSPECIFIED.,.F.,.F.,(4,3,3,3,3,3,3,3,4),(-22.9415794419873,
-22.7785483076118,-21.7881766420634,-20.7978049765151,-19.8074333109668,
-18.8170616454184,-17.8266899798701,-16.8363183143217,-16.6583941348077),
 .UNSPECIFIED.);
#24454=B_SPLINE_CURVE_WITH_KNOTS('',3,(#106657,#106658,#106659,#106660,
#106661,#106662,#106663,#106664,#106665,#106666,#106667,#106668,#106669,
#106670,#106671,#106672,#106673,#106674,#106675,#106676,#106677,#106678,
#106679,#106680,#106681),.UNSPECIFIED.,.F.,.F.,(4,3,3,3,3,3,3,3,4),(13.6891124208201,
13.8652033176767,14.8555749832251,15.8459466487734,16.8363183143217,17.8266899798701,
18.8170616454184,19.8074333109667,19.9722977279997),.UNSPECIFIED.);
#24455=B_SPLINE_CURVE_WITH_KNOTS('',3,(#106686,#106687,#106688,#106689,
#106690,#106691,#106692,#106693,#106694,#106695,#106696,#106697,#106698,
#106699,#106700,#106701,#106702,#106703,#106704,#106705,#106706,#106707),
 .UNSPECIFIED.,.F.,.F.,(4,3,3,3,3,3,3,4),(-29.2247647491669,-28.7207783009018,
-27.7304066353535,-26.7400349698051,-25.7496633042568,-24.7592916387085,
-23.7689199731601,-22.9415794419873),.UNSPECIFIED.);
#24456=B_SPLINE_CURVE_WITH_KNOTS('',3,(#106708,#106709,#106710,#106711,
#106712,#106713,#106714,#106715,#106716,#106717,#106718,#106719,#106720,
#106721,#106722,#106723,#106724,#106725,#106726,#106727,#106728,#106729),
 .UNSPECIFIED.,.F.,.F.,(4,3,3,3,3,3,3,4),(19.9722977279997,20.7978049765151,
21.7881766420634,22.7785483076118,23.7689199731601,24.7592916387084,25.7496633042568,
26.2554830351793),.UNSPECIFIED.);
#24457=B_SPLINE_CURVE_WITH_KNOTS('',3,(#106734,#106735,#106736,#106737,
#106738,#106739,#106740,#106741,#106742,#106743,#106744,#106745,#106746,
#106747,#106748,#106749,#106750,#106751,#106752,#106753,#106754,#106755),
 .UNSPECIFIED.,.F.,.F.,(4,3,3,3,3,3,3,4),(-35.5079500563465,-34.6630082941918,
-33.6726366286435,-32.6822649630952,-31.6918932975468,-30.7015216319985,
-29.7111499664501,-29.2247647491669),.UNSPECIFIED.);
#24458=B_SPLINE_CURVE_WITH_KNOTS('',3,(#106756,#106757,#106758,#106759,
#106760,#106761,#106762,#106763,#106764,#106765,#106766,#106767,#106768,
#106769,#106770,#106771,#106772,#106773,#106774,#106775,#106776,#106777),
 .UNSPECIFIED.,.F.,.F.,(4,3,3,3,3,3,3,4),(26.2554830351793,26.7400349698051,
27.7304066353534,28.7207783009018,29.7111499664501,30.7015216319985,31.6918932975468,
32.5386683423589),.UNSPECIFIED.);
#24459=B_SPLINE_CURVE_WITH_KNOTS('',3,(#106782,#106783,#106784,#106785,
#106786,#106787,#106788,#106789,#106790,#106791,#106792,#106793,#106794,
#106795,#106796,#106797,#106798,#106799,#106800,#106801,#106802,#106803,
#106804,#106805,#106806),.UNSPECIFIED.,.F.,.F.,(4,3,3,3,3,3,3,3,4),(-41.7911353635261,
-41.5956099530302,-40.6052382874819,-39.6148666219335,-38.6244949563852,
-37.6341232908368,-36.6437516252885,-35.6533799597402,-35.5079500563465),
 .UNSPECIFIED.);
#24460=B_SPLINE_CURVE_WITH_KNOTS('',3,(#106807,#106808,#106809,#106810,
#106811,#106812,#106813,#106814,#106815,#106816,#106817,#106818,#106819,
#106820,#106821,#106822,#106823,#106824,#106825,#106826,#106827,#106828,
#106829,#106830,#106831),.UNSPECIFIED.,.F.,.F.,(4,3,3,3,3,3,3,3,4),(32.5386683423589,
32.6822649630951,33.6726366286435,34.6630082941918,35.6533799597401,36.6437516252885,
37.6341232908368,38.6244949563852,38.8218536495385),.UNSPECIFIED.);
#24461=B_SPLINE_CURVE_WITH_KNOTS('',3,(#106836,#106837,#106838,#106839,
#106840,#106841,#106842,#106843,#106844,#106845,#106846,#106847,#106848,
#106849,#106850,#106851,#106852,#106853,#106854,#106855,#106856,#106857),
 .UNSPECIFIED.,.F.,.F.,(4,3,3,3,3,3,3,4),(-48.0743206707057,-47.5378399463202,
-46.5474682807719,-45.5570966152235,-44.5667249496752,-43.5763532841269,
-42.5859816185785,-41.7911353635261),.UNSPECIFIED.);
#24462=B_SPLINE_CURVE_WITH_KNOTS('',3,(#106858,#106859,#106860,#106861,
#106862,#106863,#106864,#106865,#106866,#106867,#106868,#106869,#106870,
#106871,#106872,#106873,#106874,#106875,#106876,#106877,#106878,#106879),
 .UNSPECIFIED.,.F.,.F.,(4,3,3,3,3,3,3,4),(38.8218536495385,39.6148666219335,
40.6052382874818,41.5956099530302,42.5859816185785,43.5763532841269,44.5667249496752,
45.1050389567181),.UNSPECIFIED.);
#24463=B_SPLINE_CURVE_WITH_KNOTS('',3,(#106884,#106885,#106886,#106887,
#106888,#106889,#106890,#106891,#106892,#106893,#106894,#106895,#106896,
#106897,#106898,#106899,#106900,#106901,#106902,#106903,#106904,#106905),
 .UNSPECIFIED.,.F.,.F.,(4,3,3,3,3,3,3,4),(-54.3575059778853,-53.4800699396103,
-52.4896982740619,-51.4993266085136,-50.5089549429652,-49.5185832774169,
-48.5282116118686,-48.0743206707057),.UNSPECIFIED.);
#24464=B_SPLINE_CURVE_WITH_KNOTS('',3,(#106906,#106907,#106908,#106909,
#106910,#106911,#106912,#106913,#106914,#106915,#106916,#106917,#106918,
#106919,#106920,#106921,#106922,#106923,#106924,#106925,#106926,#106927),
 .UNSPECIFIED.,.F.,.F.,(4,3,3,3,3,3,3,4),(45.1050389567181,45.5570966152235,
46.5474682807719,47.5378399463202,48.5282116118685,49.5185832774169,50.5089549429652,
51.3882242638976),.UNSPECIFIED.);
#24465=B_SPLINE_CURVE_WITH_KNOTS('',3,(#106932,#106933,#106934,#106935,
#106936,#106937,#106938,#106939,#106940,#106941,#106942,#106943,#106944,
#106945,#106946,#106947,#106948,#106949,#106950,#106951,#106952,#106953,
#106954,#106955,#106956),.UNSPECIFIED.,.F.,.F.,(4,3,3,3,3,3,3,3,4),(-60.6406912850649,
-60.4126715984486,-59.4222999329003,-58.4319282673519,-57.4415566018036,
-56.4511849362553,-55.4608132707069,-54.4704416051586,-54.3575059778853),
 .UNSPECIFIED.);
#24466=B_SPLINE_CURVE_WITH_KNOTS('',3,(#106957,#106958,#106959,#106960,
#106961,#106962,#106963,#106964,#106965,#106966,#106967,#106968,#106969,
#106970,#106971,#106972,#106973,#106974,#106975,#106976,#106977,#106978,
#106979,#106980,#106981),.UNSPECIFIED.,.F.,.F.,(4,3,3,3,3,3,3,3,4),(51.3882242638976,
51.4993266085136,52.4896982740619,53.4800699396102,54.4704416051586,55.4608132707069,
56.4511849362552,57.4415566018036,57.6714095710772),.UNSPECIFIED.);
#24467=B_SPLINE_CURVE_WITH_KNOTS('',3,(#106986,#106987,#106988,#106989,
#106990,#106991,#106992,#106993,#106994,#106995,#106996,#106997,#106998,
#106999,#107000,#107001,#107002,#107003,#107004,#107005,#107006,#107007),
 .UNSPECIFIED.,.F.,.F.,(4,3,3,3,3,3,3,4),(-66.9238765922444,-66.3549015917386,
-65.3645299261903,-64.374158260642,-63.3837865950936,-62.3934149295453,
-61.403043263997,-60.6406912850649),.UNSPECIFIED.);
#24468=B_SPLINE_CURVE_WITH_KNOTS('',3,(#107008,#107009,#107010,#107011,
#107012,#107013,#107014,#107015,#107016,#107017,#107018,#107019,#107020,
#107021,#107022,#107023,#107024,#107025,#107026,#107027,#107028,#107029),
 .UNSPECIFIED.,.F.,.F.,(4,3,3,3,3,3,3,4),(57.6714095710772,58.4319282673519,
59.4222999329003,60.4126715984486,61.4030432639969,62.3934149295453,63.3837865950936,
63.9545948782568),.UNSPECIFIED.);
#24469=B_SPLINE_CURVE_WITH_KNOTS('',3,(#107035,#107036,#107037,#107038,
#107039,#107040,#107041,#107042,#107043),.UNSPECIFIED.,.F.,.F.,(4,1,1,1,
1,1,4),(72.2566310325652,73.0189830114973,74.0093546770456,74.999726342594,
75.9900980081423,76.9804696736907,77.878411997016),.UNSPECIFIED.);
#24470=B_SPLINE_CURVE_WITH_KNOTS('',3,(#107046,#107047,#107048,#107049,
#107050,#107051,#107052,#107053),.UNSPECIFIED.,.F.,.F.,(4,1,1,1,1,4),(72.2566310325652,
72.6761944149503,73.6665660804986,74.656937746047,75.6473094115953,76.6376810771436),
 .UNSPECIFIED.);
#24471=B_SPLINE_CURVE_WITH_KNOTS('',3,(#107058,#107059,#107060,#107061,
#107062,#107063,#107064,#107065,#107066,#107067,#107068),.UNSPECIFIED.,
 .F.,.F.,(4,1,1,1,1,1,1,1,4),(65.9734457253857,66.0863813526589,67.0767530182073,
68.0671246837556,69.057496349304,70.0478680148523,71.0382396804006,72.028611345949,
72.2566310325652),.UNSPECIFIED.);
#24472=B_SPLINE_CURVE_WITH_KNOTS('',3,(#107069,#107070,#107071,#107072,
#107073,#107074,#107075,#107076,#107077,#107078),.UNSPECIFIED.,.F.,.F.,
(4,1,1,1,1,1,1,4),(65.9734457253856,66.7339644216603,67.7243360872086,68.7147077527569,
69.7050794183053,70.6954510838536,71.685822749402,72.2566310325652),
 .UNSPECIFIED.);
#24473=B_SPLINE_CURVE_WITH_KNOTS('',3,(#107083,#107084,#107085,#107086,
#107087,#107088,#107089,#107090,#107091,#107092),.UNSPECIFIED.,.F.,.F.,
(4,1,1,1,1,1,1,4),(59.6902604182061,60.1441513593689,61.1345230249173,62.1248946904656,
63.1152663560139,64.1056380215623,65.0960096871106,65.9734457253857),
 .UNSPECIFIED.);
#24474=B_SPLINE_CURVE_WITH_KNOTS('',3,(#107093,#107094,#107095,#107096,
#107097,#107098,#107099,#107100,#107101,#107102,#107103),.UNSPECIFIED.,
 .F.,.F.,(4,1,1,1,1,1,1,1,4),(59.690260418206,59.8013627628219,60.7917344283702,
61.7821060939186,62.7724777594669,63.7628494250152,64.7532210905636,65.7435927561119,
65.9734457253856),.UNSPECIFIED.);
#24475=B_SPLINE_CURVE_WITH_KNOTS('',3,(#107108,#107109,#107110,#107111,
#107112,#107113,#107114,#107115,#107116,#107117),.UNSPECIFIED.,.F.,.F.,
(4,1,1,1,1,1,1,4),(53.4070751110265,54.2019213660789,55.1922930316272,56.1826646971756,
57.1730363627239,58.1634080282722,59.1537796938206,59.6902604182061),
 .UNSPECIFIED.);
#24476=B_SPLINE_CURVE_WITH_KNOTS('',3,(#107118,#107119,#107120,#107121,
#107122,#107123,#107124,#107125,#107126,#107127),.UNSPECIFIED.,.F.,.F.,
(4,1,1,1,1,1,1,4),(53.4070751110265,53.8591327695319,54.8495044350802,55.8398761006285,
56.8302477661769,57.8206194317252,58.8109910972736,59.690260418206),
 .UNSPECIFIED.);
#24477=B_SPLINE_CURVE_WITH_KNOTS('',3,(#107132,#107133,#107134,#107135,
#107136,#107137,#107138,#107139,#107140,#107141,#107142),.UNSPECIFIED.,
 .F.,.F.,(4,1,1,1,1,1,1,1,4),(47.1238898038469,47.2693197072405,48.2596913727889,
49.2500630383372,50.2404347038855,51.2308063694339,52.2211780349822,53.2115497005306,
53.4070751110265),.UNSPECIFIED.);
#24478=B_SPLINE_CURVE_WITH_KNOTS('',3,(#107143,#107144,#107145,#107146,
#107147,#107148,#107149,#107150,#107151,#107152),.UNSPECIFIED.,.F.,.F.,
(4,1,1,1,1,1,1,4),(47.1238898038469,47.9169027762418,48.9072744417902,49.8976461073385,
50.8880177728869,51.8783894384352,52.8687611039835,53.4070751110265),
 .UNSPECIFIED.);
#24479=B_SPLINE_CURVE_WITH_KNOTS('',3,(#107157,#107158,#107159,#107160,
#107161,#107162,#107163,#107164,#107165,#107166),.UNSPECIFIED.,.F.,.F.,
(4,1,1,1,1,1,1,4),(40.8407044966673,41.3270897139505,42.3174613794988,43.3078330450472,
44.2982047105955,45.2885763761439,46.2789480416922,47.1238898038469),
 .UNSPECIFIED.);
#24480=B_SPLINE_CURVE_WITH_KNOTS('',3,(#107167,#107168,#107169,#107170,
#107171,#107172,#107173,#107174,#107175,#107176,#107177),.UNSPECIFIED.,
 .F.,.F.,(4,1,1,1,1,1,1,1,4),(40.8407044966673,40.9843011174035,41.9746727829518,
42.9650444485002,43.9554161140485,44.9457877795968,45.9361594451452,46.9265311106935,
47.1238898038469),.UNSPECIFIED.);
#24481=B_SPLINE_CURVE_WITH_KNOTS('',3,(#107182,#107183,#107184,#107185,
#107186,#107187,#107188,#107189,#107190,#107191),.UNSPECIFIED.,.F.,.F.,
(4,1,1,1,1,1,1,4),(34.5575191894877,35.3848597206605,36.3752313862088,37.3656030517571,
38.3559747173055,39.3463463828538,40.3367180484022,40.8407044966673),
 .UNSPECIFIED.);
#24482=B_SPLINE_CURVE_WITH_KNOTS('',3,(#107192,#107193,#107194,#107195,
#107196,#107197,#107198,#107199,#107200,#107201),.UNSPECIFIED.,.F.,.F.,
(4,1,1,1,1,1,1,4),(34.5575191894877,35.0420711241134,36.0324427896618,37.0228144552101,
38.0131861207585,39.0035577863068,39.9939294518551,40.8407044966673),
 .UNSPECIFIED.);
#24483=B_SPLINE_CURVE_WITH_KNOTS('',3,(#107206,#107207,#107208,#107209,
#107210,#107211,#107212,#107213,#107214,#107215,#107216),.UNSPECIFIED.,
 .F.,.F.,(4,1,1,1,1,1,1,1,4),(28.2743338823081,28.4522580618221,29.4426297273704,
30.4330013929188,31.4233730584671,32.4137447240155,33.4041163895638,34.3944880551121,
34.5575191894877),.UNSPECIFIED.);
#24484=B_SPLINE_CURVE_WITH_KNOTS('',3,(#107217,#107218,#107219,#107220,
#107221,#107222,#107223,#107224,#107225,#107226),.UNSPECIFIED.,.F.,.F.,
(4,1,1,1,1,1,1,4),(28.2743338823081,29.0998411308234,30.0902127963718,31.0805844619201,
32.0709561274684,33.0613277930168,34.0516994585651,34.5575191894877),
 .UNSPECIFIED.);
#24485=B_SPLINE_CURVE_WITH_KNOTS('',3,(#107231,#107232,#107233,#107234,
#107235,#107236,#107237,#107238,#107239,#107240),.UNSPECIFIED.,.F.,.F.,
(4,1,1,1,1,1,1,4),(21.9911485751285,22.5100280685321,23.5003997340804,24.4907713996288,
25.4811430651771,26.4715147307254,27.4618863962738,28.2743338823081),
 .UNSPECIFIED.);
#24486=B_SPLINE_CURVE_WITH_KNOTS('',3,(#107241,#107242,#107243,#107244,
#107245,#107246,#107247,#107248,#107249,#107250,#107251),.UNSPECIFIED.,
 .F.,.F.,(4,1,1,1,1,1,1,1,4),(21.9911485751285,22.1672394719851,23.1576111375334,
24.1479828030817,25.1383544686301,26.1287261341784,27.1190977997268,28.1094694652751,
28.2743338823081),.UNSPECIFIED.);
#24487=B_SPLINE_CURVE_WITH_KNOTS('',3,(#107256,#107257,#107258,#107259,
#107260,#107261,#107262,#107263,#107264,#107265),.UNSPECIFIED.,.F.,.F.,
(4,1,1,1,1,1,1,4),(15.7079632679489,16.5677980752421,17.5581697407904,18.5485414063387,
19.5389130718871,20.5292847374354,21.5196564029837,21.9911485751285),
 .UNSPECIFIED.);
#24488=B_SPLINE_CURVE_WITH_KNOTS('',3,(#107266,#107267,#107268,#107269,
#107270,#107271,#107272,#107273,#107274,#107275),.UNSPECIFIED.,.F.,.F.,
(4,1,1,1,1,1,1,4),(15.7079632679489,16.225009478695,17.2153811442434,18.2057528097917,
19.19612447534,20.1864961408884,21.1768678064367,21.9911485751285),
 .UNSPECIFIED.);
#24489=B_SPLINE_CURVE_WITH_KNOTS('',3,(#107278,#107279,#107280,#107281,
#107282,#107283,#107284,#107285,#107286,#107287,#107288,#107289,#107290,
#107291,#107292,#107293,#107294,#107295,#107296,#107297,#107298,#107299,
#107300,#107301,#107302,#107303,#107304,#107305,#107306,#107307,#107308,
#107309,#107310,#107311,#107312,#107313,#107314,#107315,#107316,#107317,
#107318,#107319,#107320,#107321,#107322,#107323,#107324,#107325,#107326,
#107327,#107328,#107329,#107330,#107331,#107332,#107333,#107334,#107335,
#107336,#107337,#107338,#107339,#107340,#107341,#107342,#107343,#107344,
#107345,#107346,#107347,#107348,#107349,#107350,#107351,#107352,#107353,
#107354,#107355,#107356,#107357,#107358,#107359,#107360,#107361,#107362),
 .UNSPECIFIED.,.F.,.F.,(4,3,3,3,3,3,3,3,3,3,3,3,3,3,3,3,3,3,3,3,3,3,3,3,
3,3,3,3,4),(-0.276631791712726,-0.265556404172054,-0.250893761334244,-0.246326614508792,
-0.242071276684929,-0.226809496625315,-0.215889342634413,-0.212053933697475,
-0.209215860671437,-0.193472099741198,-0.177422787794644,-0.167929157020507,
-0.163043036473233,-0.159563271570797,-0.143037655072155,-0.139448264698093,
-0.123479171928492,-0.115761723682961,-0.11087518000946,-0.107810715979693,
-0.0912632113418131,-0.0743540660658942,-0.0648503094985542,-0.0586274039788276,
-0.0554898421713441,-0.038048405855375,-0.0205610872293301,-0.00347583643527304,
0.),.UNSPECIFIED.);
#24490=B_SPLINE_CURVE_WITH_KNOTS('',3,(#107367,#107368,#107369,#107370,
#107371,#107372,#107373,#107374,#107375,#107376,#107377,#107378,#107379,
#107380,#107381,#107382,#107383,#107384,#107385,#107386,#107387,#107388,
#107389,#107390,#107391,#107392,#107393,#107394,#107395,#107396,#107397,
#107398,#107399,#107400,#107401,#107402,#107403,#107404,#107405,#107406,
#107407,#107408,#107409,#107410,#107411,#107412,#107413,#107414,#107415,
#107416,#107417,#107418,#107419,#107420,#107421,#107422,#107423,#107424,
#107425,#107426,#107427,#107428,#107429,#107430,#107431,#107432,#107433,
#107434,#107435,#107436,#107437,#107438,#107439,#107440,#107441,#107442,
#107443,#107444,#107445,#107446,#107447,#107448),.UNSPECIFIED.,.F.,.F.,
(4,3,3,3,3,3,3,3,3,3,3,3,3,3,3,3,3,3,3,3,3,3,3,3,3,3,3,4),(-0.275362278356893,
-0.261872343204998,-0.24468860577658,-0.238154470087611,-0.234296428116099,
-0.217100289999107,-0.205513059221426,-0.20049709699629,-0.197078549988272,
-0.180325629008319,-0.163976579024965,-0.154083045213138,-0.146647746749225,
-0.143758439830075,-0.127907386038086,-0.124402443777657,-0.107856521591035,
-0.100778967419367,-0.0955723543570963,-0.09258481164279,-0.0768191855824136,
-0.0611312890502507,-0.053290039364698,-0.0475073352526531,-0.0447090506925457,
-0.029602296160261,-0.0148011480801305,0.),.UNSPECIFIED.);
#24491=B_SPLINE_CURVE_WITH_KNOTS('',3,(#107737,#107738,#107739,#107740,
#107741,#107742,#107743,#107744,#107745,#107746),.UNSPECIFIED.,.F.,.F.,
(4,3,3,4),(63.9545948782568,64.374158260642,65.3645299261903,66.2624722495156),
 .UNSPECIFIED.);
#24492=B_SPLINE_CURVE_WITH_KNOTS('',3,(#107748,#107749,#107750,#107751,
#107752,#107753,#107754,#107755,#107756,#107757,#107758,#107759,#107760,
#107761,#107762,#107763,#107764,#107765,#107766,#107767,#107768,#107769,
#107770,#107771,#107772,#107773,#107774,#107775,#107776,#107777,#107778,
#107779,#107780,#107781,#107782,#107783,#107784,#107785,#107786,#107787,
#107788,#107789,#107790,#107791,#107792,#107793,#107794,#107795,#107796,
#107797,#107798,#107799,#107800,#107801,#107802,#107803,#107804,#107805,
#107806,#107807,#107808,#107809,#107810,#107811,#107812,#107813,#107814,
#107815,#107816,#107817,#107818,#107819,#107820,#107821,#107822,#107823,
#107824,#107825,#107826,#107827,#107828,#107829,#107830,#107831,#107832),
 .UNSPECIFIED.,.F.,.F.,(4,3,3,3,3,3,3,3,3,3,3,3,3,3,3,3,3,3,3,3,3,3,3,3,
3,3,3,3,4),(-0.276631791712751,-0.265556404172093,-0.250893754106259,-0.246326629283502,
-0.242071279945798,-0.22680949525836,-0.215889341438329,-0.212053930423597,
-0.209215853958591,-0.193472089270526,-0.177422778058093,-0.167929149718099,
-0.163043027431145,-0.159563268993254,-0.143037653194888,-0.139448264698117,
-0.123479168511542,-0.11576172047957,-0.110875178909016,-0.10781071624844,
-0.0912632076335315,-0.0743540586873285,-0.0648503081023367,-0.0586274009532849,
-0.0554898388596249,-0.0380483998101587,-0.0205610837999868,-0.00347584549412929,
0.),.UNSPECIFIED.);
#24493=B_SPLINE_CURVE_WITH_KNOTS('',3,(#107833,#107834,#107835,#107836,
#107837,#107838,#107839,#107840,#107841),.UNSPECIFIED.,.F.,.F.,(4,1,1,1,
1,1,4),(10.375208827628,11.2731511509533,12.2635228165017,13.25389448205,
14.2442661475984,15.2346378131467,15.7079632679489),.UNSPECIFIED.);
#24494=B_SPLINE_CURVE_WITH_KNOTS('',3,(#107847,#107848,#107849,#107850,
#107851,#107852,#107853,#107854,#107855,#107856,#107857,#107858,#107859,
#107860,#107861,#107862,#107863,#107864,#107865,#107866,#107867,#107868,
#107869,#107870,#107871,#107872,#107873,#107874,#107875,#107876,#107877,
#107878,#107879,#107880,#107881,#107882,#107883,#107884,#107885,#107886,
#107887,#107888,#107889,#107890,#107891,#107892,#107893,#107894,#107895,
#107896,#107897,#107898,#107899,#107900,#107901,#107902,#107903,#107904,
#107905,#107906,#107907,#107908,#107909,#107910,#107911,#107912,#107913,
#107914,#107915,#107916,#107917,#107918,#107919,#107920,#107921,#107922,
#107923,#107924,#107925,#107926,#107927,#107928),.UNSPECIFIED.,.F.,.F.,
(4,3,3,3,3,3,3,3,3,3,3,3,3,3,3,3,3,3,3,3,3,3,3,3,3,3,3,4),(-0.275362278356958,
-0.261872343205071,-0.244688605776648,-0.238154479469242,-0.234296429189573,
-0.217100291206748,-0.205513060278116,-0.200497101796343,-0.197078550198523,
-0.180325630119186,-0.163976587765092,-0.154083051768242,-0.14664777167162,
-0.143758474849684,-0.127907428224212,-0.124402443777692,-0.107856504661946,
-0.100778964786935,-0.0955723501300554,-0.0925848098741145,-0.0768191852239964,
-0.0611312820723457,-0.053290036945375,-0.047507330004606,-0.0447090458564731,
-0.0296022827355091,-0.0148011413677545,0.),.UNSPECIFIED.);
#24495=B_SPLINE_CURVE_WITH_KNOTS('',3,(#107931,#107932,#107933,#107934,
#107935,#107936,#107937,#107938),.UNSPECIFIED.,.F.,.F.,(4,1,1,1,1,4),(11.6159397475004,
12.6063114130487,13.596683078597,14.5870547441454,15.5774264096937,15.7079632679489),
 .UNSPECIFIED.);
#24496=B_SPLINE_CURVE_WITH_KNOTS('',3,(#108227,#108228,#108229,#108230,
#108231,#108232,#108233),.UNSPECIFIED.,.F.,.F.,(4,3,4),(-68.3356449228353,
-67.345273257287,-66.9238765922444),.UNSPECIFIED.);
#24497=B_SPLINE_CURVE_WITH_KNOTS('',3,(#108403,#108404,#108405,#108406,
#108407,#108408,#108409,#108410,#108411,#108412),.UNSPECIFIED.,.F.,.F.,
(4,3,3,4),(-4.09157007060749,-3.96000416091332,-2.97000312068499,-2.06546402602184),
 .UNSPECIFIED.);
#24498=B_SPLINE_CURVE_WITH_KNOTS('',3,(#108415,#108416,#108417,#108418,
#108419,#108420,#108421),.UNSPECIFIED.,.F.,.F.,(4,3,4),(0.,0.990001040228323,
1.11548660900407),.UNSPECIFIED.);
#24499=B_SPLINE_CURVE_WITH_KNOTS('',3,(#108426,#108427,#108428,#108429,
#108430,#108431,#108432,#108433,#108434,#108435,#108436,#108437,#108438,
#108439,#108440,#108441,#108442,#108443,#108444,#108445,#108446,#108447),
 .UNSPECIFIED.,.F.,.F.,(4,3,3,3,3,3,3,4),(-10.3747553777871,-9.90001040228329,
-8.91000936205496,-7.92000832182663,-6.93000728159831,-5.94000624136997,
-4.95000520114165,-4.09157007060749),.UNSPECIFIED.);
#24500=B_SPLINE_CURVE_WITH_KNOTS('',3,(#108448,#108449,#108450,#108451,
#108452,#108453,#108454,#108455,#108456,#108457,#108458,#108459,#108460,
#108461,#108462,#108463,#108464,#108465,#108466,#108467,#108468,#108469),
 .UNSPECIFIED.,.F.,.F.,(4,3,3,3,3,3,3,4),(1.11548660900407,1.98000208045665,
2.97000312068498,3.96000416091331,4.95000520114164,5.94000624136997,6.9300072815983,
7.39867191618366),.UNSPECIFIED.);
#24501=B_SPLINE_CURVE_WITH_KNOTS('',3,(#108474,#108475,#108476,#108477,
#108478,#108479,#108480,#108481,#108482,#108483,#108484,#108485,#108486,
#108487,#108488,#108489,#108490,#108491,#108492,#108493,#108494,#108495),
 .UNSPECIFIED.,.F.,.F.,(4,3,3,3,3,3,3,4),(-16.6579406849667,-15.8400166436532,
-14.8500156034249,-13.8600145631966,-12.8700135229683,-11.8800124827399,
-10.8900114425116,-10.3747553777871),.UNSPECIFIED.);
#24502=B_SPLINE_CURVE_WITH_KNOTS('',3,(#108496,#108497,#108498,#108499,
#108500,#108501,#108502,#108503,#108504,#108505,#108506,#108507,#108508,
#108509,#108510,#108511,#108512,#108513,#108514,#108515,#108516,#108517),
 .UNSPECIFIED.,.F.,.F.,(4,3,3,3,3,3,3,4),(7.39867191618366,7.92000832182662,
8.91000936205495,9.90001040228327,10.8900114425116,11.8800124827399,12.8700135229683,
13.6818572233633),.UNSPECIFIED.);
#24503=B_SPLINE_CURVE_WITH_KNOTS('',3,(#108522,#108523,#108524,#108525,
#108526,#108527,#108528,#108529,#108530,#108531,#108532,#108533,#108534,
#108535,#108536,#108537,#108538,#108539,#108540,#108541,#108542,#108543,
#108544,#108545,#108546),.UNSPECIFIED.,.F.,.F.,(4,3,3,3,3,3,3,3,4),(-22.9411259921463,
-22.7700239252515,-21.7800228850232,-20.7900218447949,-19.8000208045666,
-18.8100197643382,-17.8200187241099,-16.8300176838816,-16.6579406849667),
 .UNSPECIFIED.);
#24504=B_SPLINE_CURVE_WITH_KNOTS('',3,(#108547,#108548,#108549,#108550,
#108551,#108552,#108553,#108554,#108555,#108556,#108557,#108558,#108559,
#108560,#108561,#108562,#108563,#108564,#108565,#108566,#108567,#108568,
#108569,#108570,#108571),.UNSPECIFIED.,.F.,.F.,(4,3,3,3,3,3,3,3,4),(13.6818572233633,
13.8600145631966,14.8500156034249,15.8400166436532,16.8300176838816,17.8200187241099,
18.8100197643382,19.8000208045666,19.9650425305428),.UNSPECIFIED.);
#24505=B_SPLINE_CURVE_WITH_KNOTS('',3,(#108576,#108577,#108578,#108579,
#108580,#108581,#108582,#108583,#108584,#108585,#108586,#108587,#108588,
#108589,#108590,#108591,#108592,#108593,#108594,#108595,#108596,#108597),
 .UNSPECIFIED.,.F.,.F.,(4,3,3,3,3,3,3,4),(-29.2243112993259,-28.7100301666215,
-27.7200291263932,-26.7300280861648,-25.7400270459365,-24.7500260057082,
-23.7600249654799,-22.9411259921463),.UNSPECIFIED.);
#24506=B_SPLINE_CURVE_WITH_KNOTS('',3,(#108598,#108599,#108600,#108601,
#108602,#108603,#108604,#108605,#108606,#108607,#108608,#108609,#108610,
#108611,#108612,#108613,#108614,#108615,#108616,#108617,#108618,#108619),
 .UNSPECIFIED.,.F.,.F.,(4,3,3,3,3,3,3,4),(19.9650425305428,20.7900218447949,
21.7800228850232,22.7700239252515,23.7600249654799,24.7500260057082,25.7400270459365,
26.2482278377224),.UNSPECIFIED.);
#24507=B_SPLINE_CURVE_WITH_KNOTS('',3,(#108624,#108625,#108626,#108627,
#108628,#108629,#108630,#108631,#108632,#108633,#108634,#108635,#108636,
#108637,#108638,#108639,#108640,#108641,#108642,#108643,#108644,#108645),
 .UNSPECIFIED.,.F.,.F.,(4,3,3,3,3,3,3,4),(-35.5074966065054,-34.6500364079915,
-33.6600353677631,-32.6700343275348,-31.6800332873065,-30.6900322470782,
-29.7000312068498,-29.2243112993259),.UNSPECIFIED.);
#24508=B_SPLINE_CURVE_WITH_KNOTS('',3,(#108646,#108647,#108648,#108649,
#108650,#108651,#108652,#108653,#108654,#108655,#108656,#108657,#108658,
#108659,#108660,#108661,#108662,#108663,#108664,#108665,#108666,#108667),
 .UNSPECIFIED.,.F.,.F.,(4,3,3,3,3,3,3,4),(26.2482278377224,26.7300280861648,
27.7200291263932,28.7100301666215,29.7000312068498,30.6900322470781,31.6800332873065,
32.531413144902),.UNSPECIFIED.);
#24509=B_SPLINE_CURVE_WITH_KNOTS('',3,(#108673,#108674,#108675,#108676,
#108677),.UNSPECIFIED.,.F.,.F.,(4,1,4),(47.1238898038469,47.2564306455613,
48.1609697402245),.UNSPECIFIED.);
#24510=B_SPLINE_CURVE_WITH_KNOTS('',3,(#108683,#108684,#108685,#108686,
#108687,#108688,#108689,#108690,#108691,#108692),.UNSPECIFIED.,.F.,.F.,
(4,1,1,1,1,1,1,4),(40.8407044966673,41.3164244041913,42.3064254444196,43.296426484648,
44.2864275248763,45.2764285651046,46.2664296053329,47.1238898038469),
 .UNSPECIFIED.);
#24511=B_SPLINE_CURVE_WITH_KNOTS('',3,(#108695,#108696,#108697,#108698,
#108699,#108700,#108701,#108702,#108703,#108704),.UNSPECIFIED.,.F.,.F.,
(4,1,1,1,1,1,1,4),(40.8407044966673,40.9793256793001,41.9693267195284,42.9593277597568,
43.9493287999851,44.9393298402134,45.9293308804417,46.9193319206701),
 .UNSPECIFIED.);
#24512=B_SPLINE_CURVE_WITH_KNOTS('',3,(#108709,#108710,#108711,#108712,
#108713,#108714,#108715,#108716,#108717,#108718),.UNSPECIFIED.,.F.,.F.,
(4,1,1,1,1,1,1,4),(34.5575191894877,35.3764181628213,36.3664192030497,37.356420243278,
38.3464212835063,39.3364223237347,40.326423363963,40.8407044966673),
 .UNSPECIFIED.);
#24513=B_SPLINE_CURVE_WITH_KNOTS('',3,(#108719,#108720,#108721,#108722,
#108723,#108724,#108725,#108726,#108727,#108728),.UNSPECIFIED.,.F.,.F.,
(4,1,1,1,1,1,1,4),(34.5575191894877,35.0393194379301,36.0293204781585,37.0193215183868,
38.0093225586151,38.9993235988434,39.9893246390718,40.8407044966673),
 .UNSPECIFIED.);
#24514=B_SPLINE_CURVE_WITH_KNOTS('',3,(#108733,#108734,#108735,#108736,
#108737,#108738,#108739,#108740,#108741,#108742,#108743),.UNSPECIFIED.,
 .F.,.F.,(4,1,1,1,1,1,1,1,4),(28.2743338823082,28.4464108812231,29.4364119214514,
30.4264129616797,31.416414001908,32.4064150421364,33.3964160823647,34.386417122593,
34.5575191894877),.UNSPECIFIED.);
#24515=B_SPLINE_CURVE_WITH_KNOTS('',3,(#108744,#108745,#108746,#108747,
#108748,#108749,#108750,#108751,#108752,#108753),.UNSPECIFIED.,.F.,.F.,
(4,1,1,1,1,1,1,4),(28.2743338823081,29.0993131965602,30.0893142367885,31.0793152770168,
32.0693163172452,33.0593173574735,34.0493183977018,34.5575191894877),
 .UNSPECIFIED.);
#24516=B_SPLINE_CURVE_WITH_KNOTS('',3,(#108758,#108759,#108760,#108761,
#108762,#108763,#108764,#108765,#108766,#108767),.UNSPECIFIED.,.F.,.F.,
(4,1,1,1,1,1,1,4),(21.9911485751286,22.5064046398531,23.4964056800814,24.4864067203097,
25.4764077605381,26.4664088007664,27.4564098409947,28.2743338823082),
 .UNSPECIFIED.);
#24517=B_SPLINE_CURVE_WITH_KNOTS('',3,(#108768,#108769,#108770,#108771,
#108772,#108773,#108774,#108775,#108776,#108777,#108778),.UNSPECIFIED.,
 .F.,.F.,(4,1,1,1,1,1,1,1,4),(21.9911485751286,22.1693059149619,23.1593069551902,
24.1493079954185,25.1393090356469,26.1293100758752,27.1193111161035,28.1093121563318,
28.2743338823081),.UNSPECIFIED.);
#24518=B_SPLINE_CURVE_WITH_KNOTS('',3,(#108783,#108784,#108785,#108786,
#108787,#108788,#108789,#108790,#108791,#108792),.UNSPECIFIED.,.F.,.F.,
(4,1,1,1,1,1,1,4),(15.707963267949,16.5663983984831,17.5563994387115,18.5464004789398,
19.5364015191681,20.5264025593964,21.5164035996248,21.9911485751286),
 .UNSPECIFIED.);
#24519=B_SPLINE_CURVE_WITH_KNOTS('',3,(#108793,#108794,#108795,#108796,
#108797,#108798,#108799,#108800,#108801,#108802),.UNSPECIFIED.,.F.,.F.,
(4,1,1,1,1,1,1,4),(15.707963267949,16.2292996735919,17.2193007138202,18.2093017540486,
19.1993027942769,20.1893038345052,21.1793048747336,21.9911485751286),
 .UNSPECIFIED.);
#24520=B_SPLINE_CURVE_WITH_KNOTS('',3,(#108805,#108806,#108807,#108808,
#108809,#108810,#108811,#108812,#108813,#108814,#108815,#108816,#108817,
#108818,#108819,#108820,#108821,#108822,#108823,#108824,#108825,#108826,
#108827,#108828,#108829,#108830,#108831,#108832,#108833,#108834,#108835,
#108836,#108837,#108838,#108839,#108840,#108841,#108842,#108843,#108844,
#108845,#108846,#108847,#108848,#108849,#108850,#108851,#108852,#108853,
#108854,#108855,#108856,#108857,#108858,#108859,#108860,#108861,#108862,
#108863,#108864,#108865,#108866,#108867,#108868,#108869,#108870,#108871,
#108872,#108873,#108874,#108875,#108876,#108877),.UNSPECIFIED.,.F.,.F.,
(4,3,3,3,3,3,3,3,3,3,3,3,3,3,3,3,3,3,3,3,3,3,3,3,4),(-0.178587760439576,
-0.172123484066144,-0.162029610797555,-0.158960076316314,-0.156277673116426,
-0.145500175528421,-0.137612438657249,-0.135052164839013,-0.123703644030005,
-0.112271443891481,-0.106158017111512,-0.103756352114049,-0.0913724979174295,
-0.0799509356777508,-0.0747329310245961,-0.0722089888096775,-0.0698495451559696,
-0.0578987267473855,-0.0456650852971465,-0.0398988500531476,-0.0369271031414654,
-0.034358735828395,-0.0216670048239294,-0.00906125808895899,0.),
 .UNSPECIFIED.);
#24521=B_SPLINE_CURVE_WITH_KNOTS('',3,(#108882,#108883,#108884,#108885,
#108886,#108887,#108888,#108889,#108890,#108891,#108892,#108893,#108894,
#108895,#108896,#108897,#108898,#108899,#108900,#108901,#108902,#108903,
#108904,#108905,#108906,#108907,#108908,#108909,#108910,#108911,#108912,
#108913,#108914,#108915,#108916,#108917,#108918,#108919,#108920,#108921,
#108922,#108923,#108924,#108925,#108926,#108927,#108928,#108929,#108930,
#108931,#108932,#108933,#108934,#108935,#108936,#108937,#108938,#108939,
#108940,#108941,#108942,#108943,#108944,#108945,#108946,#108947,#108948,
#108949,#108950,#108951,#108952,#108953,#108954,#108955,#108956,#108957),
 .UNSPECIFIED.,.F.,.F.,(4,3,3,3,3,3,3,3,3,3,3,3,3,3,3,3,3,3,3,3,3,3,3,3,
3,4),(-0.177567088092011,-0.169323782934868,-0.158089696666802,-0.153262207767463,
-0.149988677353406,-0.137528660299912,-0.130268964361215,-0.127199953384994,
-0.124659149705796,-0.112713138690929,-0.101044919579301,-0.0953407172754274,
-0.0930414661610526,-0.0906321687534946,-0.0794510927903374,-0.0687820057106859,
-0.063254327381541,-0.0606631966659519,-0.0584063594980229,-0.0472188556442702,
-0.0361621989269624,-0.0310713136030704,-0.027770944652939,-0.0171899085459505,
-0.0069942035205897,0.),.UNSPECIFIED.);
#24522=B_SPLINE_CURVE_WITH_KNOTS('',3,(#109126,#109127,#109128,#109129,
#109130,#109131,#109132,#109133,#109134,#109135,#109136,#109137,#109138,
#109139,#109140,#109141),.UNSPECIFIED.,.F.,.F.,(4,3,3,3,3,4),(32.531413144902,
32.6700343275348,33.6600353677631,34.6500364079915,35.6400374482198,36.5445765428829),
 .UNSPECIFIED.);
#24523=B_SPLINE_CURVE_WITH_KNOTS('',3,(#109143,#109144,#109145,#109146,
#109147,#109148,#109149,#109150,#109151,#109152,#109153,#109154,#109155,
#109156,#109157,#109158,#109159,#109160,#109161,#109162,#109163,#109164,
#109165,#109166,#109167,#109168,#109169,#109170,#109171,#109172,#109173,
#109174,#109175,#109176,#109177,#109178,#109179,#109180,#109181,#109182,
#109183,#109184,#109185,#109186,#109187,#109188,#109189,#109190,#109191,
#109192,#109193,#109194,#109195,#109196,#109197,#109198,#109199,#109200,
#109201,#109202,#109203,#109204,#109205,#109206,#109207,#109208,#109209,
#109210,#109211,#109212,#109213,#109214,#109215),.UNSPECIFIED.,.F.,.F.,
(4,3,3,3,3,3,3,3,3,3,3,3,3,3,3,3,3,3,3,3,3,3,3,3,4),(-0.17858776043949,
-0.172123484066062,-0.162029610797479,-0.158960078532571,-0.156277675821071,
-0.145500180136282,-0.137612447812564,-0.135052182725417,-0.123703662522982,
-0.112271461769566,-0.106158041900681,-0.103756358640701,-0.0913724979173968,
-0.0799509356777222,-0.0747329304622504,-0.0722089814481734,-0.0698495348147565,
-0.0578987173311656,-0.0456650770053533,-0.0398988390332298,-0.0369269838058204,
-0.0343587144614106,-0.0216669841604778,-0.00906123403203008,0.),
 .UNSPECIFIED.);
#24524=B_SPLINE_CURVE_WITH_KNOTS('',3,(#109216,#109217,#109218,#109219,
#109220,#109221,#109222,#109223,#109224),.UNSPECIFIED.,.F.,.F.,(4,1,1,1,
1,1,4),(10.3747553777871,11.2792944724503,12.2692955126786,13.2592965529069,
14.2492975931353,15.2392986333636,15.707963267949),.UNSPECIFIED.);
#24525=B_SPLINE_CURVE_WITH_KNOTS('',3,(#109230,#109231,#109232,#109233,
#109234,#109235,#109236,#109237,#109238,#109239,#109240,#109241,#109242,
#109243,#109244,#109245,#109246,#109247,#109248,#109249,#109250,#109251,
#109252,#109253,#109254,#109255,#109256,#109257,#109258,#109259,#109260,
#109261,#109262,#109263,#109264,#109265,#109266,#109267,#109268,#109269,
#109270,#109271,#109272,#109273,#109274,#109275,#109276,#109277,#109278,
#109279,#109280,#109281,#109282,#109283,#109284,#109285,#109286,#109287,
#109288,#109289,#109290,#109291,#109292,#109293,#109294,#109295,#109296,
#109297,#109298,#109299,#109300,#109301,#109302,#109303,#109304,#109305),
 .UNSPECIFIED.,.F.,.F.,(4,3,3,3,3,3,3,3,3,3,3,3,3,3,3,3,3,3,3,3,3,3,3,3,
3,4),(-0.177567088092203,-0.169323782935046,-0.158089696666967,-0.153262206421705,
-0.149988677397371,-0.137528659982041,-0.130268964083088,-0.127199950909321,
-0.124659148761581,-0.112713135669775,-0.101044912712987,-0.0953407090796688,
-0.0930414624834283,-0.0906321680944933,-0.0794510927904141,-0.0687820319799606,
-0.0632543486467741,-0.0606634285098871,-0.0584066697739641,-0.0472191669545651,
-0.0361625070709391,-0.0310717437638542,-0.0277708925982038,-0.0171898619043016,
-0.00699416415736055,0.),.UNSPECIFIED.);
#24526=B_SPLINE_CURVE_WITH_KNOTS('',3,(#109308,#109309,#109310,#109311,
#109312,#109313,#109314,#109315),.UNSPECIFIED.,.F.,.F.,(4,1,1,1,1,4),(11.6163931973415,
12.6063942375698,13.5963952777981,14.5863963180265,15.5763973582548,15.707963267949),
 .UNSPECIFIED.);
#24527=B_SPLINE_CURVE_WITH_KNOTS('',3,(#109484,#109485,#109486,#109487,
#109488,#109489,#109490,#109491,#109492,#109493,#109494,#109495,#109496),
 .UNSPECIFIED.,.F.,.F.,(4,3,3,3,4),(-38.6100405689048,-37.6200395286764,
-36.6300384884481,-35.6400374482198,-35.5074966065054),.UNSPECIFIED.);
#24528=B_SPLINE_CURVE_WITH_KNOTS('',3,(#109666,#109667,#109668,#109669,
#109670,#109671,#109672,#109673,#109674,#109675),.UNSPECIFIED.,.F.,.F.,
(4,3,3,4),(-4.09157007060749,-3.96821312525615,-2.97615984394211,-2.0654640260217),
 .UNSPECIFIED.);
#24529=B_SPLINE_CURVE_WITH_KNOTS('',3,(#109678,#109679,#109680,#109681,
#109682,#109683,#109684),.UNSPECIFIED.,.F.,.F.,(4,3,4),(0.,0.992053281314042,
1.11548660900393),.UNSPECIFIED.);
#24530=B_SPLINE_CURVE_WITH_KNOTS('',3,(#109689,#109690,#109691,#109692,
#109693,#109694,#109695,#109696,#109697,#109698,#109699,#109700,#109701,
#109702,#109703,#109704,#109705,#109706,#109707,#109708,#109709,#109710),
 .UNSPECIFIED.,.F.,.F.,(4,3,3,3,3,3,3,4),(-10.3747553777871,-9.92053281314039,
-8.92847953182635,-7.93642625051231,-6.94437296919827,-5.95231968788423,
-4.96026640657019,-4.09157007060749),.UNSPECIFIED.);
#24531=B_SPLINE_CURVE_WITH_KNOTS('',3,(#109711,#109712,#109713,#109714,
#109715,#109716,#109717,#109718,#109719,#109720,#109721,#109722,#109723,
#109724,#109725,#109726,#109727,#109728,#109729,#109730,#109731,#109732),
 .UNSPECIFIED.,.F.,.F.,(4,3,3,3,3,3,3,4),(1.11548660900393,1.98410656262808,
2.97615984394212,3.96821312525616,4.9602664065702,5.95231968788424,6.94437296919828,
7.39867191618352),.UNSPECIFIED.);
#24532=B_SPLINE_CURVE_WITH_KNOTS('',3,(#109737,#109738,#109739,#109740,
#109741,#109742,#109743,#109744,#109745,#109746,#109747,#109748,#109749,
#109750,#109751,#109752,#109753,#109754,#109755,#109756,#109757,#109758),
 .UNSPECIFIED.,.F.,.F.,(4,3,3,3,3,3,3,4),(-16.6579406849665,-15.8728525010246,
-14.8807992197106,-13.8887459383965,-12.8966926570825,-11.9046393757685,
-10.9125860944544,-10.3747553777871),.UNSPECIFIED.);
#24533=B_SPLINE_CURVE_WITH_KNOTS('',3,(#109759,#109760,#109761,#109762,
#109763,#109764,#109765,#109766,#109767,#109768,#109769,#109770,#109771,
#109772,#109773,#109774,#109775,#109776,#109777,#109778,#109779,#109780),
 .UNSPECIFIED.,.F.,.F.,(4,3,3,3,3,3,3,4),(7.39867191618352,7.93642625051232,
8.92847953182636,9.9205328131404,10.9125860944544,11.9046393757685,12.8966926570825,
13.6818572233631),.UNSPECIFIED.);
#24534=B_SPLINE_CURVE_WITH_KNOTS('',3,(#109785,#109786,#109787,#109788,
#109789,#109790,#109791,#109792,#109793,#109794,#109795,#109796,#109797,
#109798,#109799,#109800,#109801,#109802,#109803,#109804,#109805,#109806,
#109807,#109808,#109809),.UNSPECIFIED.,.F.,.F.,(4,3,3,3,3,3,3,3,4),(-22.9411259921461,
-22.8172254702229,-21.8251721889089,-20.8331189075948,-19.8410656262808,
-18.8490123449667,-17.8569590636527,-16.8649057823387,-16.6579406849665),
 .UNSPECIFIED.);
#24535=B_SPLINE_CURVE_WITH_KNOTS('',3,(#109810,#109811,#109812,#109813,
#109814,#109815,#109816,#109817,#109818,#109819,#109820,#109821,#109822,
#109823,#109824,#109825,#109826,#109827,#109828,#109829,#109830,#109831,
#109832,#109833,#109834),.UNSPECIFIED.,.F.,.F.,(4,3,3,3,3,3,3,3,4),(13.6818572233631,
13.8887459383966,14.8807992197106,15.8728525010246,16.8649057823387,17.8569590636527,
18.8490123449668,19.8410656262808,19.9650425305427),.UNSPECIFIED.);
#24536=B_SPLINE_CURVE_WITH_KNOTS('',3,(#109839,#109840,#109841,#109842,
#109843,#109844,#109845,#109846,#109847,#109848,#109849,#109850,#109851,
#109852,#109853,#109854,#109855,#109856,#109857,#109858,#109859,#109860),
 .UNSPECIFIED.,.F.,.F.,(4,3,3,3,3,3,3,4),(-29.2243112993257,-28.7695451581071,
-27.7774918767931,-26.7854385954791,-25.793385314165,-24.801332032851,-23.8092787515369,
-22.9411259921461),.UNSPECIFIED.);
#24537=B_SPLINE_CURVE_WITH_KNOTS('',3,(#109861,#109862,#109863,#109864,
#109865,#109866,#109867,#109868,#109869,#109870,#109871,#109872,#109873,
#109874,#109875,#109876,#109877,#109878,#109879,#109880,#109881,#109882),
 .UNSPECIFIED.,.F.,.F.,(4,3,3,3,3,3,3,4),(19.9650425305427,20.8331189075948,
21.8251721889089,22.8172254702229,23.8092787515369,24.801332032851,25.793385314165,
26.2482278377223),.UNSPECIFIED.);
#24538=B_SPLINE_CURVE_WITH_KNOTS('',3,(#109887,#109888,#109889,#109890,
#109891,#109892,#109893,#109894,#109895,#109896,#109897,#109898,#109899,
#109900,#109901,#109902,#109903,#109904,#109905,#109906,#109907,#109908),
 .UNSPECIFIED.,.F.,.F.,(4,3,3,3,3,3,3,4),(-35.5074966065053,-34.7218648459914,
-33.7298115646773,-32.7377582833633,-31.7457050020492,-30.7536517207352,
-29.7615984394212,-29.2243112993257),.UNSPECIFIED.);
#24539=B_SPLINE_CURVE_WITH_KNOTS('',3,(#109909,#109910,#109911,#109912,
#109913,#109914,#109915,#109916,#109917,#109918,#109919,#109920,#109921,
#109922,#109923,#109924,#109925,#109926,#109927,#109928,#109929,#109930),
 .UNSPECIFIED.,.F.,.F.,(4,3,3,3,3,3,3,4),(26.2482278377223,26.7854385954791,
27.7774918767931,28.7695451581071,29.7615984394212,30.7536517207352,31.7457050020493,
32.5314131449019),.UNSPECIFIED.);
#24540=B_SPLINE_CURVE_WITH_KNOTS('',3,(#109935,#109936,#109937,#109938,
#109939,#109940,#109941,#109942,#109943,#109944,#109945,#109946,#109947,
#109948,#109949,#109950,#109951,#109952,#109953,#109954,#109955,#109956,
#109957,#109958,#109959),.UNSPECIFIED.,.F.,.F.,(4,3,3,3,3,3,3,3,4),(-41.7906819136849,
-41.6662378151896,-40.6741845338756,-39.6821312525616,-38.6900779712475,
-37.6980246899335,-36.7059714086194,-35.7139181273054,-35.5074966065053),
 .UNSPECIFIED.);
#24541=B_SPLINE_CURVE_WITH_KNOTS('',3,(#109960,#109961,#109962,#109963,
#109964,#109965,#109966,#109967,#109968,#109969,#109970,#109971,#109972,
#109973,#109974,#109975,#109976,#109977,#109978,#109979,#109980,#109981,
#109982,#109983,#109984),.UNSPECIFIED.,.F.,.F.,(4,3,3,3,3,3,3,3,4),(32.5314131449019,
32.7377582833633,33.7298115646773,34.7218648459914,35.7139181273054,36.7059714086195,
37.6980246899335,38.6900779712475,38.8145984520815),.UNSPECIFIED.);
#24542=B_SPLINE_CURVE_WITH_KNOTS('',3,(#109991,#109992,#109993,#109994,
#109995,#109996,#109997,#109998,#109999,#110000,#110001,#110002,#110003,
#110004,#110005,#110006,#110007,#110008,#110009),.UNSPECIFIED.,.F.,.F.,
(4,3,3,3,3,3,4),(-47.6185575030738,-46.6265042217598,-45.6344509404458,
-44.6423976591318,-43.6503443778177,-42.6582910965037,-41.7906819136849),
 .UNSPECIFIED.);
#24543=B_SPLINE_CURVE_WITH_KNOTS('',3,(#110010,#110011,#110012,#110013,
#110014,#110015,#110016,#110017,#110018,#110019,#110020,#110021,#110022,
#110023,#110024,#110025,#110026,#110027,#110028,#110029,#110030,#110031),
 .UNSPECIFIED.,.F.,.F.,(4,3,3,3,3,3,3,4),(38.8145984520815,39.6821312525616,
40.6741845338756,41.6662378151897,42.6582910965037,43.6503443778177,44.6423976591318,
45.0977837592611),.UNSPECIFIED.);
#24544=B_SPLINE_CURVE_WITH_KNOTS('',3,(#110037,#110038,#110039,#110040,
#110041,#110042,#110043),.UNSPECIFIED.,.F.,.F.,(4,1,1,1,4),(53.4070751110264,
54.2746842938452,55.2667375751592,56.2587908564733,57.1694866743937),
 .UNSPECIFIED.);
#24545=B_SPLINE_CURVE_WITH_KNOTS('',3,(#110046,#110047,#110048,#110049,
#110050,#110051),.UNSPECIFIED.,.F.,.F.,(4,1,1,4),(53.4070751110264,53.9437422922112,
54.9357955735252,55.9278488548392),.UNSPECIFIED.);
#24546=B_SPLINE_CURVE_WITH_KNOTS('',3,(#110056,#110057,#110058,#110059,
#110060,#110061,#110062,#110063,#110064,#110065,#110066),.UNSPECIFIED.,
 .F.,.F.,(4,1,1,1,1,1,1,1,4),(47.1238898038469,47.3303113246469,48.322364605961,
49.314417887275,50.306471168589,51.2985244499031,52.2905777312171,53.2826310125312,
53.4070751110264),.UNSPECIFIED.);
#24547=B_SPLINE_CURVE_WITH_KNOTS('',3,(#110067,#110068,#110069,#110070,
#110071,#110072,#110073,#110074,#110075,#110076),.UNSPECIFIED.,.F.,.F.,
(4,1,1,1,1,1,1,4),(47.1238898038469,47.9914226043269,48.983475885641,49.975529166955,
50.967582448269,51.9596357295831,52.9516890108971,53.4070751110264),
 .UNSPECIFIED.);
#24548=B_SPLINE_CURVE_WITH_KNOTS('',3,(#110081,#110082,#110083,#110084,
#110085,#110086,#110087,#110088,#110089,#110090),.UNSPECIFIED.,.F.,.F.,
(4,1,1,1,1,1,1,4),(40.8407044966673,41.3779916367627,42.3700449180767,43.3620981993908,
44.3541514807048,45.3462047620188,46.3382580433329,47.1238898038469),
 .UNSPECIFIED.);
#24549=B_SPLINE_CURVE_WITH_KNOTS('',3,(#110091,#110092,#110093,#110094,
#110095,#110096,#110097,#110098,#110099,#110100,#110101),.UNSPECIFIED.,
 .F.,.F.,(4,1,1,1,1,1,1,1,4),(40.8407044966673,41.0470496351287,42.0391029164427,
43.0311561977567,44.0232094790708,45.0152627603848,46.0073160416989,46.9993693230129,
47.1238898038469),.UNSPECIFIED.);
#24550=B_SPLINE_CURVE_WITH_KNOTS('',3,(#110106,#110107,#110108,#110109,
#110110,#110111,#110112,#110113,#110114,#110115),.UNSPECIFIED.,.F.,.F.,
(4,1,1,1,1,1,1,4),(34.5575191894877,35.4256719488784,36.4177252301925,37.4097785115065,
38.4018317928206,39.3938850741346,40.3859383554486,40.8407044966673),
 .UNSPECIFIED.);
#24551=B_SPLINE_CURVE_WITH_KNOTS('',3,(#110116,#110117,#110118,#110119,
#110120,#110121,#110122,#110123,#110124,#110125),.UNSPECIFIED.,.F.,.F.,
(4,1,1,1,1,1,1,4),(34.5575191894877,35.0947299472444,36.0867832285585,37.0788365098725,
38.0708897911865,39.0629430725006,40.0549963538146,40.8407044966673),
 .UNSPECIFIED.);
#24552=B_SPLINE_CURVE_WITH_KNOTS('',3,(#110130,#110131,#110132,#110133,
#110134,#110135,#110136,#110137,#110138,#110139,#110140),.UNSPECIFIED.,
 .F.,.F.,(4,1,1,1,1,1,1,1,4),(28.2743338823081,28.4812989796802,29.4733522609942,
30.4654055423083,31.4574588236223,32.4495121049363,33.4415653862504,34.4336186675644,
34.5575191894877),.UNSPECIFIED.);
#24553=B_SPLINE_CURVE_WITH_KNOTS('',3,(#110141,#110142,#110143,#110144,
#110145,#110146,#110147,#110148,#110149,#110150),.UNSPECIFIED.,.F.,.F.,
(4,1,1,1,1,1,1,4),(28.2743338823081,29.1424102593602,30.1344635406742,31.1265168219883,
32.1185701033023,33.1106233846163,34.1026766659304,34.5575191894877),
 .UNSPECIFIED.);
#24554=B_SPLINE_CURVE_WITH_KNOTS('',3,(#110155,#110156,#110157,#110158,
#110159,#110160,#110161,#110162,#110163,#110164),.UNSPECIFIED.,.F.,.F.,
(4,1,1,1,1,1,1,4),(21.9911485751285,22.5289792917959,23.52103257311,24.513085854424,
25.5051391357381,26.4971924170521,27.4892456983661,28.2743338823081),
 .UNSPECIFIED.);
#24555=B_SPLINE_CURVE_WITH_KNOTS('',3,(#110165,#110166,#110167,#110168,
#110169,#110170,#110171,#110172,#110173,#110174,#110175),.UNSPECIFIED.,
 .F.,.F.,(4,1,1,1,1,1,1,1,4),(21.9911485751285,22.1980372901619,23.1900905714759,
24.18214385279,25.174197134104,26.1662504154181,27.1583036967321,28.1503569780461,
28.2743338823081),.UNSPECIFIED.);
#24556=B_SPLINE_CURVE_WITH_KNOTS('',3,(#110180,#110181,#110182,#110183,
#110184,#110185,#110186,#110187,#110188,#110189),.UNSPECIFIED.,.F.,.F.,
(4,1,1,1,1,1,1,4),(15.7079632679489,16.5766596039117,17.5687128852257,18.5607661665398,
19.5528194478538,20.5448727291679,21.5369260104819,21.9911485751285),
 .UNSPECIFIED.);
#24557=B_SPLINE_CURVE_WITH_KNOTS('',3,(#110190,#110191,#110192,#110193,
#110194,#110195,#110196,#110197,#110198,#110199),.UNSPECIFIED.,.F.,.F.,
(4,1,1,1,1,1,1,4),(15.7079632679489,16.2457176022777,17.2377708835917,18.2298241649058,
19.2218774462198,20.2139307275338,21.2059840088479,21.9911485751285),
 .UNSPECIFIED.);
#24558=B_SPLINE_CURVE_WITH_KNOTS('',3,(#110201,#110202,#110203,#110204,
#110205,#110206,#110207,#110208,#110209,#110210,#110211,#110212,#110213,
#110214,#110215,#110216,#110217,#110218,#110219,#110220,#110221,#110222,
#110223,#110224,#110225,#110226,#110227,#110228,#110229,#110230,#110231,
#110232,#110233,#110234,#110235,#110236,#110237,#110238,#110239,#110240,
#110241,#110242,#110243,#110244,#110245,#110246,#110247,#110248,#110249,
#110250,#110251,#110252,#110253,#110254,#110255,#110256,#110257,#110258,
#110259,#110260,#110261,#110262,#110263,#110264,#110265,#110266,#110267,
#110268,#110269,#110270,#110271,#110272,#110273),.UNSPECIFIED.,.F.,.F.,
(4,3,3,3,3,3,3,3,3,3,3,3,3,3,3,3,3,3,3,3,3,3,3,3,4),(-0.178587760439504,
-0.172436005266845,-0.162325405279674,-0.158983610121922,-0.156300142716475,
-0.145521462210125,-0.137695659081724,-0.13518810584043,-0.123840773922177,
-0.112407563090991,-0.106415995852445,-0.103612144676863,-0.0915512053694793,
-0.0801073046982944,-0.0748685857871388,-0.0720605549642836,-0.0695158393189569,
-0.057554069888016,-0.0453143736546683,-0.0394431135780157,-0.0369681942630705,
-0.0343654591089171,-0.0216730559581644,-0.0090670142413088,0.),
 .UNSPECIFIED.);
#24559=B_SPLINE_CURVE_WITH_KNOTS('',3,(#110276,#110277,#110278,#110279,
#110280,#110281,#110282,#110283,#110284,#110285,#110286,#110287,#110288,
#110289,#110290,#110291,#110292,#110293,#110294,#110295,#110296,#110297,
#110298,#110299,#110300,#110301,#110302,#110303,#110304,#110305,#110306,
#110307,#110308,#110309,#110310,#110311,#110312,#110313,#110314,#110315,
#110316,#110317,#110318,#110319,#110320,#110321,#110322,#110323,#110324,
#110325,#110326,#110327,#110328,#110329,#110330,#110331,#110332,#110333,
#110334,#110335,#110336,#110337,#110338,#110339,#110340,#110341,#110342,
#110343,#110344,#110345,#110346,#110347,#110348,#110349,#110350,#110351),
 .UNSPECIFIED.,.F.,.F.,(4,3,3,3,3,3,3,3,3,3,3,3,3,3,3,3,3,3,3,3,3,3,3,3,
3,4),(-0.177567088092197,-0.169718205449901,-0.158456796357131,-0.154087938332518,
-0.149901326685707,-0.137441206344475,-0.130214422139883,-0.127484197404693,
-0.124915045826681,-0.112965831709766,-0.101293012250859,-0.0956918677235842,
-0.0932236527120616,-0.0908269354509327,-0.0796269327077398,-0.0694129961400613,
-0.0639913339275198,-0.0605457458673101,-0.0580972397750422,-0.0469085861859489,
-0.0358589547005544,-0.0306372080887885,-0.0277838560902035,-0.017202291045908,
-0.00700607863093054,0.),.UNSPECIFIED.);
#24560=B_SPLINE_CURVE_WITH_KNOTS('',3,(#110556,#110557,#110558,#110559),
 .UNSPECIFIED.,.F.,.F.,(4,4),(45.0977837592611,45.553093477052),
 .UNSPECIFIED.);
#24561=B_SPLINE_CURVE_WITH_KNOTS('',3,(#110561,#110562,#110563,#110564,
#110565,#110566,#110567,#110568,#110569,#110570,#110571,#110572,#110573,
#110574,#110575,#110576,#110577,#110578,#110579,#110580,#110581,#110582,
#110583,#110584,#110585,#110586,#110587,#110588,#110589,#110590,#110591,
#110592,#110593,#110594,#110595,#110596,#110597,#110598,#110599,#110600,
#110601,#110602,#110603,#110604,#110605,#110606,#110607,#110608,#110609,
#110610,#110611,#110612,#110613,#110614,#110615,#110616,#110617,#110618,
#110619,#110620,#110621,#110622,#110623,#110624,#110625,#110626,#110627,
#110628,#110629,#110630,#110631,#110632,#110633),.UNSPECIFIED.,.F.,.F.,
(4,3,3,3,3,3,3,3,3,3,3,3,3,3,3,3,3,3,3,3,3,3,3,3,4),(-0.17858776043956,
-0.172436005266898,-0.162325405279723,-0.158983610459464,-0.156300143130782,
-0.14552146303087,-0.137695660713911,-0.135188108280273,-0.123840776492776,
-0.112407565558593,-0.10641599916013,-0.103612145963209,-0.091551205369502,
-0.0801073046983142,-0.0748685855925244,-0.0720605538167012,-0.0695158390600375,
-0.0575540698726435,-0.0453143738867585,-0.0394431138098223,-0.0369681938209412,
-0.0343654589710512,-0.0216730560122649,-0.00906701360523848,0.),
 .UNSPECIFIED.);
#24562=B_SPLINE_CURVE_WITH_KNOTS('',3,(#110634,#110635,#110636,#110637,
#110638,#110639,#110640,#110641,#110642),.UNSPECIFIED.,.F.,.F.,(4,1,1,1,
1,1,4),(10.3747553777871,11.2854511957075,12.2775044770215,13.2695577583356,
14.2616110396496,15.2536643209636,15.7079632679489),.UNSPECIFIED.);
#24563=B_SPLINE_CURVE_WITH_KNOTS('',3,(#110648,#110649,#110650,#110651,
#110652,#110653,#110654,#110655,#110656,#110657,#110658,#110659,#110660,
#110661,#110662,#110663,#110664,#110665,#110666,#110667,#110668,#110669,
#110670,#110671,#110672,#110673,#110674,#110675,#110676,#110677,#110678,
#110679,#110680,#110681,#110682,#110683,#110684,#110685,#110686,#110687,
#110688,#110689,#110690,#110691,#110692,#110693,#110694,#110695,#110696,
#110697,#110698,#110699,#110700,#110701,#110702,#110703,#110704,#110705,
#110706,#110707,#110708,#110709,#110710,#110711,#110712,#110713,#110714,
#110715,#110716,#110717,#110718,#110719,#110720,#110721,#110722,#110723),
 .UNSPECIFIED.,.F.,.F.,(4,3,3,3,3,3,3,3,3,3,3,3,3,3,3,3,3,3,3,3,3,3,3,3,
3,4),(-0.177567088092152,-0.169718205449872,-0.158456796357106,-0.154087938106763,
-0.149901326639656,-0.137441206226106,-0.130214422036311,-0.127484196657443,
-0.124915044564136,-0.112965830066187,-0.101293009880069,-0.0956918649462959,
-0.0932236438564468,-0.0908269205250241,-0.0796269327077417,-0.0694130001063571,
-0.0639913397708145,-0.0605456801771174,-0.0580972309446734,-0.046908577415714,
-0.0358589469260566,-0.0306371966909039,-0.0277838544508456,-0.01720229026982,
-0.00700607908527243,0.),.UNSPECIFIED.);
#24564=B_SPLINE_CURVE_WITH_KNOTS('',3,(#110726,#110727,#110728,#110729,
#110730,#110731,#110732,#110733),.UNSPECIFIED.,.F.,.F.,(4,1,1,1,1,4),(11.6163931973415,
12.6084464786556,13.6004997599696,14.5925530412836,15.5846063225977,15.7079632679489),
 .UNSPECIFIED.);
#24565=B_SPLINE_CURVE_WITH_KNOTS('',3,(#110993,#110994,#110995,#110996,
#110997,#110998,#110999,#111000,#111001,#111002),.UNSPECIFIED.,.F.,.F.,
(4,3,3,4),(-4.09282965349932,-3.97811826982011,-2.98358870236508,-2.06974660785394),
 .UNSPECIFIED.);
#24566=B_SPLINE_CURVE_WITH_KNOTS('',3,(#111005,#111006,#111007,#111008,
#111009,#111010,#111011),.UNSPECIFIED.,.F.,.F.,(4,3,4),(0.,0.99452956745502,
1.11850960794437),.UNSPECIFIED.);
#24567=B_SPLINE_CURVE_WITH_KNOTS('',3,(#111016,#111017,#111018,#111019,
#111020,#111021,#111022,#111023,#111024,#111025,#111026,#111027,#111028,
#111029,#111030,#111031,#111032,#111033,#111034,#111035,#111036,#111037),
 .UNSPECIFIED.,.F.,.F.,(4,3,3,3,3,3,3,4),(-10.3760149606789,-9.94529567455027,
-8.95076610709525,-7.95623653964022,-6.96170697218519,-5.96717740473016,
-4.97264783727514,-4.09282965349932),.UNSPECIFIED.);
#24568=B_SPLINE_CURVE_WITH_KNOTS('',3,(#111038,#111039,#111040,#111041,
#111042,#111043,#111044,#111045,#111046,#111047,#111048,#111049,#111050,
#111051,#111052,#111053,#111054,#111055,#111056,#111057,#111058,#111059),
 .UNSPECIFIED.,.F.,.F.,(4,3,3,3,3,3,3,4),(1.11850960794437,1.98905913491005,
2.98358870236508,3.97811826982011,4.97264783727514,5.96717740473017,6.9617069721852,
7.40169491512398),.UNSPECIFIED.);
#24569=B_SPLINE_CURVE_WITH_KNOTS('',3,(#111064,#111065,#111066,#111067,
#111068,#111069,#111070,#111071,#111072,#111073,#111074,#111075,#111076,
#111077,#111078,#111079,#111080,#111081,#111082,#111083,#111084,#111085),
 .UNSPECIFIED.,.F.,.F.,(4,3,3,3,3,3,3,4),(-16.6592002678585,-15.9124730792804,
-14.9179435118254,-13.9234139443704,-12.9288843769154,-11.9343548094603,
-10.9398252420053,-10.3760149606789),.UNSPECIFIED.);
#24570=B_SPLINE_CURVE_WITH_KNOTS('',3,(#111086,#111087,#111088,#111089,
#111090,#111091,#111092,#111093,#111094,#111095,#111096,#111097,#111098,
#111099,#111100,#111101,#111102,#111103,#111104,#111105,#111106,#111107),
 .UNSPECIFIED.,.F.,.F.,(4,3,3,3,3,3,3,4),(7.40169491512398,7.95623653964023,
8.95076610709526,9.94529567455028,10.9398252420053,11.9343548094603,12.9288843769154,
13.6848802223036),.UNSPECIFIED.);
#24571=B_SPLINE_CURVE_WITH_KNOTS('',3,(#111112,#111113,#111114,#111115,
#111116,#111117,#111118,#111119,#111120,#111121,#111122,#111123,#111124,
#111125,#111126,#111127,#111128,#111129,#111130,#111131,#111132,#111133,
#111134,#111135,#111136),.UNSPECIFIED.,.F.,.F.,(4,3,3,3,3,3,3,3,4),(-22.9423855750381,
-22.8741800514656,-21.8796504840106,-20.8851209165556,-19.8905913491005,
-18.8960617816455,-17.9015322141905,-16.9070026467355,-16.6592002678585),
 .UNSPECIFIED.);
#24572=B_SPLINE_CURVE_WITH_KNOTS('',3,(#111137,#111138,#111139,#111140,
#111141,#111142,#111143,#111144,#111145,#111146,#111147,#111148,#111149,
#111150,#111151,#111152,#111153,#111154,#111155,#111156,#111157,#111158,
#111159,#111160,#111161),.UNSPECIFIED.,.F.,.F.,(4,3,3,3,3,3,3,3,4),(13.6848802223036,
13.9234139443704,14.9179435118254,15.9124730792804,16.9070026467355,17.9015322141905,
18.8960617816455,19.8905913491005,19.9680655294831),.UNSPECIFIED.);
#24573=B_SPLINE_CURVE_WITH_KNOTS('',3,(#111166,#111167,#111168,#111169,
#111170,#111171,#111172,#111173,#111174,#111175,#111176,#111177,#111178,
#111179,#111180,#111181,#111182,#111183,#111184,#111185,#111186,#111187),
 .UNSPECIFIED.,.F.,.F.,(4,3,3,3,3,3,3,4),(-29.2255708822177,-28.8413574561958,
-27.8468278887408,-26.8522983212857,-25.8577687538307,-24.8632391863757,
-23.8687096189207,-22.9423855750381),.UNSPECIFIED.);
#24574=B_SPLINE_CURVE_WITH_KNOTS('',3,(#111188,#111189,#111190,#111191,
#111192,#111193,#111194,#111195,#111196,#111197,#111198,#111199,#111200,
#111201,#111202,#111203,#111204,#111205,#111206,#111207,#111208,#111209),
 .UNSPECIFIED.,.F.,.F.,(4,3,3,3,3,3,3,4),(19.9680655294831,20.8851209165556,
21.8796504840106,22.8741800514656,23.8687096189207,24.8632391863757,25.8577687538307,
26.2512508366627),.UNSPECIFIED.);
#24575=B_SPLINE_CURVE_WITH_KNOTS('',3,(#111214,#111215,#111216,#111217,
#111218,#111219,#111220,#111221,#111222,#111223,#111224,#111225,#111226,
#111227,#111228,#111229,#111230,#111231,#111232,#111233,#111234,#111235),
 .UNSPECIFIED.,.F.,.F.,(4,3,3,3,3,3,3,4),(-35.5087561893973,-34.808534860926,
-33.8140052934709,-32.8194757260159,-31.8249461585609,-30.8304165911058,
-29.8358870236508,-29.2255708822177),.UNSPECIFIED.);
#24576=B_SPLINE_CURVE_WITH_KNOTS('',3,(#111236,#111237,#111238,#111239,
#111240,#111241,#111242,#111243,#111244,#111245,#111246,#111247,#111248,
#111249,#111250,#111251,#111252,#111253,#111254,#111255,#111256,#111257),
 .UNSPECIFIED.,.F.,.F.,(4,3,3,3,3,3,3,4),(26.2512508366627,26.8522983212857,
27.8468278887408,28.8413574561958,29.8358870236508,30.8304165911058,31.8249461585609,
32.5344361438423),.UNSPECIFIED.);
#24577=B_SPLINE_CURVE_WITH_KNOTS('',3,(#111262,#111263,#111264,#111265,
#111266,#111267,#111268,#111269,#111270,#111271,#111272,#111273,#111274,
#111275,#111276,#111277,#111278,#111279,#111280,#111281,#111282,#111283,
#111284,#111285,#111286),.UNSPECIFIED.,.F.,.F.,(4,3,3,3,3,3,3,3,4),(-41.7919414965769,
-41.7702418331111,-40.7757122656561,-39.7811826982011,-38.7866531307461,
-37.792123563291,-36.797593995836,-35.803064428381,-35.5087561893973),
 .UNSPECIFIED.);
#24578=B_SPLINE_CURVE_WITH_KNOTS('',3,(#111287,#111288,#111289,#111290,
#111291,#111292,#111293,#111294,#111295,#111296,#111297,#111298,#111299,
#111300,#111301,#111302,#111303,#111304,#111305,#111306,#111307,#111308,
#111309,#111310,#111311),.UNSPECIFIED.,.F.,.F.,(4,3,3,3,3,3,3,3,4),(32.5344361438423,
32.8194757260159,33.8140052934709,34.808534860926,35.803064428381,36.797593995836,
37.792123563291,38.7866531307461,38.8176214510219),.UNSPECIFIED.);
#24579=B_SPLINE_CURVE_WITH_KNOTS('',3,(#111316,#111317,#111318,#111319,
#111320,#111321,#111322,#111323,#111324,#111325,#111326,#111327,#111328,
#111329,#111330,#111331,#111332,#111333,#111334,#111335,#111336,#111337),
 .UNSPECIFIED.,.F.,.F.,(4,3,3,3,3,3,3,4),(-48.0751268037564,-47.7374192378413,
-46.7428896703863,-45.7483601029313,-44.7538305354762,-43.7593009680212,
-42.7647714005662,-41.7919414965769),.UNSPECIFIED.);
#24580=B_SPLINE_CURVE_WITH_KNOTS('',3,(#111338,#111339,#111340,#111341,
#111342,#111343,#111344,#111345,#111346,#111347,#111348,#111349,#111350,
#111351,#111352,#111353,#111354,#111355,#111356,#111357,#111358,#111359),
 .UNSPECIFIED.,.F.,.F.,(4,3,3,3,3,3,3,4),(38.8176214510219,39.7811826982011,
40.7757122656561,41.7702418331111,42.7647714005662,43.7593009680212,44.7538305354762,
45.1008067582015),.UNSPECIFIED.);
#24581=B_SPLINE_CURVE_WITH_KNOTS('',3,(#111364,#111365,#111366,#111367,
#111368,#111369,#111370,#111371,#111372,#111373,#111374,#111375,#111376,
#111377,#111378,#111379,#111380,#111381,#111382,#111383,#111384,#111385),
 .UNSPECIFIED.,.F.,.F.,(4,3,3,3,3,3,3,4),(-54.358312110936,-53.7045966425715,
-52.7100670751164,-51.7155375076614,-50.7210079402064,-49.7264783727514,
-48.7319488052963,-48.0751268037564),.UNSPECIFIED.);
#24582=B_SPLINE_CURVE_WITH_KNOTS('',3,(#111386,#111387,#111388,#111389,
#111390,#111391,#111392,#111393,#111394,#111395,#111396,#111397,#111398,
#111399,#111400,#111401,#111402,#111403,#111404,#111405,#111406,#111407),
 .UNSPECIFIED.,.F.,.F.,(4,3,3,3,3,3,3,4),(45.1008067582015,45.7483601029313,
46.7428896703863,47.7374192378413,48.7319488052963,49.7264783727514,50.7210079402064,
51.3839920653811),.UNSPECIFIED.);
#24583=B_SPLINE_CURVE_WITH_KNOTS('',3,(#111412,#111413,#111414,#111415,
#111416,#111417,#111418,#111419,#111420,#111421,#111422,#111423,#111424,
#111425,#111426,#111427,#111428,#111429,#111430,#111431,#111432,#111433),
 .UNSPECIFIED.,.F.,.F.,(4,3,3,3,3,3,3,4),(-60.6414974181156,-59.6717740473017,
-58.6772444798466,-57.6827149123916,-56.6881853449366,-55.6936557774815,
-54.6991262100265,-54.358312110936),.UNSPECIFIED.);
#24584=B_SPLINE_CURVE_WITH_KNOTS('',3,(#111434,#111435,#111436,#111437,
#111438,#111439,#111440,#111441,#111442,#111443,#111444,#111445,#111446,
#111447,#111448,#111449,#111450,#111451,#111452,#111453,#111454,#111455),
 .UNSPECIFIED.,.F.,.F.,(4,3,3,3,3,3,3,4),(51.3839920653811,51.7155375076614,
52.7100670751164,53.7045966425715,54.6991262100265,55.6936557774815,56.6881853449365,
57.6671773725607),.UNSPECIFIED.);
#24585=B_SPLINE_CURVE_WITH_KNOTS('',3,(#111460,#111461,#111462,#111463,
#111464,#111465,#111466,#111467,#111468,#111469,#111470,#111471,#111472,
#111473,#111474,#111475,#111476,#111477,#111478,#111479,#111480,#111481,
#111482,#111483,#111484),.UNSPECIFIED.,.F.,.F.,(4,3,3,3,3,3,3,3,4),(-66.9246827252952,
-66.6334810194868,-65.6389514520318,-64.6444218845768,-63.6498923171218,
-62.6553627496667,-61.6608331822117,-60.6663036147567,-60.6414974181156),
 .UNSPECIFIED.);
#24586=B_SPLINE_CURVE_WITH_KNOTS('',3,(#111485,#111486,#111487,#111488,
#111489,#111490,#111491,#111492,#111493,#111494,#111495,#111496,#111497,
#111498,#111499,#111500,#111501,#111502,#111503,#111504,#111505,#111506,
#111507,#111508,#111509),.UNSPECIFIED.,.F.,.F.,(4,3,3,3,3,3,3,3,4),(57.6671773725607,
57.6827149123916,58.6772444798466,59.6717740473016,60.6663036147567,61.6608331822117,
62.6553627496667,63.6498923171217,63.9503626797403),.UNSPECIFIED.);
#24587=B_SPLINE_CURVE_WITH_KNOTS('',3,(#111514,#111515,#111516,#111517,
#111518,#111519,#111520,#111521,#111522,#111523,#111524,#111525,#111526,
#111527,#111528,#111529,#111530,#111531,#111532,#111533,#111534,#111535),
 .UNSPECIFIED.,.F.,.F.,(4,3,3,3,3,3,3,4),(-73.2078680324748,-72.600658424217,
-71.606128856762,-70.6115992893069,-69.6170697218519,-68.6225401543969,
-67.6280105869419,-66.9246827252952),.UNSPECIFIED.);
#24588=B_SPLINE_CURVE_WITH_KNOTS('',3,(#111536,#111537,#111538,#111539,
#111540,#111541,#111542,#111543,#111544,#111545,#111546,#111547,#111548,
#111549,#111550,#111551,#111552,#111553,#111554,#111555,#111556,#111557),
 .UNSPECIFIED.,.F.,.F.,(4,3,3,3,3,3,3,4),(63.9503626797403,64.6444218845768,
65.6389514520318,66.6334810194868,67.6280105869419,68.6225401543969,69.6170697218519,
70.2335479869199),.UNSPECIFIED.);
#24589=B_SPLINE_CURVE_WITH_KNOTS('',3,(#111562,#111563,#111564,#111565,
#111566,#111567,#111568,#111569,#111570,#111571,#111572,#111573,#111574,
#111575,#111576,#111577,#111578,#111579,#111580,#111581,#111582,#111583),
 .UNSPECIFIED.,.F.,.F.,(4,3,3,3,3,3,3,4),(-79.4910533396544,-78.5678358289472,
-77.5733062614921,-76.5787766940371,-75.5842471265821,-74.5897175591271,
-73.595187991672,-73.2078680324748),.UNSPECIFIED.);
#24590=B_SPLINE_CURVE_WITH_KNOTS('',3,(#111584,#111585,#111586,#111587,
#111588,#111589,#111590,#111591,#111592,#111593,#111594,#111595,#111596,
#111597,#111598,#111599,#111600,#111601,#111602,#111603,#111604,#111605),
 .UNSPECIFIED.,.F.,.F.,(4,3,3,3,3,3,3,4),(70.2335479869199,70.6115992893069,
71.606128856762,72.600658424217,73.595187991672,74.589717559127,75.5842471265821,
76.5167332940995),.UNSPECIFIED.);
#24591=B_SPLINE_CURVE_WITH_KNOTS('',3,(#111611,#111612,#111613,#111614,
#111615,#111616,#111617,#111618),.UNSPECIFIED.,.F.,.F.,(4,1,1,1,1,4),(84.8230016469244,
85.2103216061216,86.2048511735766,87.1993807410316,88.1939103084867,89.1077524029978),
 .UNSPECIFIED.);
#24592=B_SPLINE_CURVE_WITH_KNOTS('',3,(#111621,#111622,#111623,#111624,
#111625,#111626,#111627),.UNSPECIFIED.,.F.,.F.,(4,1,1,1,4),(84.8230016469244,
84.8850450468619,85.879574614317,86.874104181772,87.868633749227),
 .UNSPECIFIED.);
#24593=B_SPLINE_CURVE_WITH_KNOTS('',3,(#111632,#111633,#111634,#111635,
#111636,#111637,#111638,#111639,#111640,#111641),.UNSPECIFIED.,.F.,.F.,
(4,1,1,1,1,1,1,4),(78.5398163397448,79.2431442013914,80.2376737688465,81.2322033363015,
82.2267329037565,83.2212624712115,84.2157920386666,84.8230016469244),
 .UNSPECIFIED.);
#24594=B_SPLINE_CURVE_WITH_KNOTS('',3,(#111642,#111643,#111644,#111645,
#111646,#111647,#111648,#111649,#111650,#111651),.UNSPECIFIED.,.F.,.F.,
(4,1,1,1,1,1,1,4),(78.5398163397448,78.9178676421318,79.9123972095868,80.9069267770418,
81.9014563444969,82.8959859119519,83.8905154794069,84.8230016469244),
 .UNSPECIFIED.);
#24595=B_SPLINE_CURVE_WITH_KNOTS('',3,(#111656,#111657,#111658,#111659,
#111660,#111661,#111662,#111663,#111664,#111665,#111666),.UNSPECIFIED.,
 .F.,.F.,(4,1,1,1,1,1,1,1,4),(72.2566310325652,72.2814372292062,73.2759667966613,
74.2704963641163,75.2650259315713,76.2595554990263,77.2540850664814,78.2486146339364,
78.5398163397448),.UNSPECIFIED.);
#24596=B_SPLINE_CURVE_WITH_KNOTS('',3,(#111667,#111668,#111669,#111670,
#111671,#111672,#111673,#111674,#111675,#111676),.UNSPECIFIED.,.F.,.F.,
(4,1,1,1,1,1,1,4),(72.2566310325652,72.9506902374016,73.9452198048566,74.9397493723117,
75.9342789397667,76.9288085072217,77.9233380746768,78.5398163397448),
 .UNSPECIFIED.);
#24597=B_SPLINE_CURVE_WITH_KNOTS('',3,(#111681,#111682,#111683,#111684,
#111685,#111686,#111687,#111688,#111689,#111690),.UNSPECIFIED.,.F.,.F.,
(4,1,1,1,1,1,1,4),(65.9734457253856,66.3142598244761,67.3087893919311,68.3033189593861,
69.2978485268412,70.2923780942962,71.2869076617512,72.2566310325652),
 .UNSPECIFIED.);
#24598=B_SPLINE_CURVE_WITH_KNOTS('',3,(#111691,#111692,#111693,#111694,
#111695,#111696,#111697,#111698,#111699,#111700,#111701),.UNSPECIFIED.,
 .F.,.F.,(4,1,1,1,1,1,1,1,4),(65.9734457253856,65.9889832652164,66.9835128326715,
67.9780424001265,68.9725719675815,69.9671015350365,70.9616311024916,71.9561606699466,
72.2566310325652),.UNSPECIFIED.);
#24599=B_SPLINE_CURVE_WITH_KNOTS('',3,(#111706,#111707,#111708,#111709,
#111710,#111711,#111712,#111713,#111714,#111715),.UNSPECIFIED.,.F.,.F.,
(4,1,1,1,1,1,1,4),(59.6902604182061,60.3470824197459,61.3416119872009,62.336141554656,
63.330671122111,64.325200689566,65.319730257021,65.9734457253856),
 .UNSPECIFIED.);
#24600=B_SPLINE_CURVE_WITH_KNOTS('',3,(#111716,#111717,#111718,#111719,
#111720,#111721,#111722,#111723,#111724,#111725),.UNSPECIFIED.,.F.,.F.,
(4,1,1,1,1,1,1,4),(59.690260418206,60.0218058604863,61.0163354279413,62.0108649953963,
63.0053945628514,63.9999241303064,64.9944536977614,65.9734457253856),
 .UNSPECIFIED.);
#24601=B_SPLINE_CURVE_WITH_KNOTS('',3,(#111730,#111731,#111732,#111733,
#111734,#111735,#111736,#111737,#111738,#111739),.UNSPECIFIED.,.F.,.F.,
(4,1,1,1,1,1,1,4),(53.4070751110265,54.3799050150157,55.3744345824708,56.3689641499258,
57.3634937173808,58.3580232848359,59.3525528522909,59.6902604182061),
 .UNSPECIFIED.);
#24602=B_SPLINE_CURVE_WITH_KNOTS('',3,(#111740,#111741,#111742,#111743,
#111744,#111745,#111746,#111747,#111748,#111749),.UNSPECIFIED.,.F.,.F.,
(4,1,1,1,1,1,1,4),(53.4070751110265,54.0546284557561,55.0491580232111,56.0436875906662,
57.0382171581212,58.0327467255762,59.0272762930312,59.690260418206),
 .UNSPECIFIED.);
#24603=B_SPLINE_CURVE_WITH_KNOTS('',3,(#111754,#111755,#111756,#111757,
#111758,#111759,#111760,#111761,#111762,#111763,#111764),.UNSPECIFIED.,
 .F.,.F.,(4,1,1,1,1,1,1,1,4),(47.1238898038469,47.4181980428306,48.4127276102856,
49.4072571777406,50.4017867451956,51.3963163126507,52.3908458801057,53.3853754475607,
53.4070751110265),.UNSPECIFIED.);
#24604=B_SPLINE_CURVE_WITH_KNOTS('',3,(#111765,#111766,#111767,#111768,
#111769,#111770,#111771,#111772,#111773,#111774),.UNSPECIFIED.,.F.,.F.,
(4,1,1,1,1,1,1,4),(47.1238898038468,48.0874510510259,49.081980618481,50.076510185936,
51.071039753391,52.0655693208461,53.0600988883011,53.4070751110265),
 .UNSPECIFIED.);
#24605=B_SPLINE_CURVE_WITH_KNOTS('',3,(#111779,#111780,#111781,#111782,
#111783,#111784,#111785,#111786,#111787,#111788),.UNSPECIFIED.,.F.,.F.,
(4,1,1,1,1,1,1,4),(40.8407044966673,41.4510206381004,42.4455502055554,43.4400797730104,
44.4346093404655,45.4291389079205,46.4236684753755,47.1238898038469),
 .UNSPECIFIED.);
#24606=B_SPLINE_CURVE_WITH_KNOTS('',3,(#111789,#111790,#111791,#111792,
#111793,#111794,#111795,#111796,#111797,#111798,#111799),.UNSPECIFIED.,
 .F.,.F.,(4,1,1,1,1,1,1,1,4),(40.8407044966673,41.1257440788408,42.1202736462958,
43.1148032137508,44.1093327812058,45.1038623486609,46.0983919161159,47.0929214835709,
47.1238898038468),.UNSPECIFIED.);
#24607=B_SPLINE_CURVE_WITH_KNOTS('',3,(#111804,#111805,#111806,#111807,
#111808,#111809,#111810,#111811,#111812,#111813),.UNSPECIFIED.,.F.,.F.,
(4,1,1,1,1,1,1,4),(34.5575191894877,35.4838432333702,36.4783728008253,37.4729023682803,
38.4674319357353,39.4619615031903,40.4564910706454,40.8407044966673),
 .UNSPECIFIED.);
#24608=B_SPLINE_CURVE_WITH_KNOTS('',3,(#111814,#111815,#111816,#111817,
#111818,#111819,#111820,#111821,#111822,#111823),.UNSPECIFIED.,.F.,.F.,
(4,1,1,1,1,1,1,4),(34.5575191894877,35.1585666741106,36.1530962415656,37.1476258090206,
38.1421553764757,39.1366849439307,40.1312145113857,40.8407044966673),
 .UNSPECIFIED.);
#24609=B_SPLINE_CURVE_WITH_KNOTS('',3,(#111828,#111829,#111830,#111831,
#111832,#111833,#111834,#111835,#111836,#111837,#111838),.UNSPECIFIED.,
 .F.,.F.,(4,1,1,1,1,1,1,1,4),(28.2743338823081,28.522136261185,29.5166658286401,
30.5111953960951,31.5057249635501,32.5002545310051,33.4947840984602,34.4893136659152,
34.5575191894877),.UNSPECIFIED.);
#24610=B_SPLINE_CURVE_WITH_KNOTS('',3,(#111839,#111840,#111841,#111842,
#111843,#111844,#111845,#111846,#111847,#111848),.UNSPECIFIED.,.F.,.F.,
(4,1,1,1,1,1,1,4),(28.2743338823081,29.1913892693804,30.1859188368355,31.1804484042905,
32.1749779717455,33.1695075392005,34.1640371066556,34.5575191894877),
 .UNSPECIFIED.);
#24611=B_SPLINE_CURVE_WITH_KNOTS('',3,(#111853,#111854,#111855,#111856,
#111857,#111858,#111859,#111860,#111861,#111862),.UNSPECIFIED.,.F.,.F.,
(4,1,1,1,1,1,1,4),(21.9911485751285,22.5549588564549,23.5494884239099,24.5440179913649,
25.53854755882,26.533077126275,27.52760669373,28.2743338823081),
 .UNSPECIFIED.);
#24612=B_SPLINE_CURVE_WITH_KNOTS('',3,(#111863,#111864,#111865,#111866,
#111867,#111868,#111869,#111870,#111871,#111872,#111873),.UNSPECIFIED.,
 .F.,.F.,(4,1,1,1,1,1,1,1,4),(21.9911485751285,22.2296822971952,23.2242118646503,
24.2187414321053,25.2132709995603,26.2078005670153,27.2023301344704,28.1968597019254,
28.2743338823081),.UNSPECIFIED.);
#24613=B_SPLINE_CURVE_WITH_KNOTS('',3,(#111878,#111879,#111880,#111881,
#111882,#111883,#111884,#111885,#111886,#111887),.UNSPECIFIED.,.F.,.F.,
(4,1,1,1,1,1,1,4),(15.7079632679489,16.5877814517247,17.5823110191797,18.5768405866348,
19.5713701540898,20.5658997215448,21.5604292889998,21.9911485751285),
 .UNSPECIFIED.);
#24614=B_SPLINE_CURVE_WITH_KNOTS('',3,(#111888,#111889,#111890,#111891,
#111892,#111893,#111894,#111895,#111896,#111897),.UNSPECIFIED.,.F.,.F.,
(4,1,1,1,1,1,1,4),(15.7079632679489,16.2625048924651,17.2570344599201,18.2515640273751,
19.2460935948302,20.2406231622852,21.2351527297402,21.9911485751285),
 .UNSPECIFIED.);
#24615=B_SPLINE_CURVE_WITH_KNOTS('',3,(#111900,#111901,#111902,#111903,
#111904,#111905,#111906,#111907,#111908,#111909,#111910,#111911,#111912,
#111913,#111914,#111915,#111916,#111917,#111918,#111919,#111920,#111921,
#111922,#111923,#111924,#111925,#111926,#111927,#111928,#111929,#111930,
#111931,#111932,#111933,#111934,#111935,#111936,#111937,#111938,#111939,
#111940,#111941,#111942,#111943,#111944,#111945,#111946,#111947,#111948,
#111949,#111950,#111951,#111952,#111953,#111954,#111955,#111956,#111957,
#111958,#111959,#111960,#111961,#111962,#111963,#111964,#111965,#111966,
#111967,#111968,#111969,#111970,#111971,#111972,#111973,#111974,#111975,
#111976,#111977,#111978,#111979,#111980,#111981),.UNSPECIFIED.,.F.,.F.,
(4,3,3,3,3,3,3,3,3,3,3,3,3,3,3,3,3,3,3,3,3,3,3,3,3,3,3,4),(-0.22752384543732,
-0.219644941593229,-0.206672788411731,-0.201988504816839,-0.199228673818224,
-0.186142187643616,-0.17735787870582,-0.174280837207973,-0.171522085977862,
-0.157608493518707,-0.143805082530456,-0.136820740933153,-0.133782689272465,
-0.130929890576033,-0.116671801511094,-0.115867716141243,-0.10211356834673,
-0.0955239922338215,-0.0919125451791094,-0.0890238524864623,-0.0747164121491554,
-0.0600826688674195,-0.0525723352589921,-0.0471438779813513,-0.044400099706211,
-0.0292633397771947,-0.0142357759108071,0.),.UNSPECIFIED.);
#24616=B_SPLINE_CURVE_WITH_KNOTS('',3,(#111986,#111987,#111988,#111989,
#111990,#111991,#111992,#111993,#111994,#111995,#111996,#111997,#111998,
#111999,#112000,#112001,#112002,#112003,#112004,#112005,#112006,#112007,
#112008,#112009,#112010,#112011,#112012,#112013,#112014,#112015,#112016,
#112017,#112018,#112019,#112020,#112021,#112022,#112023,#112024,#112025,
#112026,#112027,#112028,#112029,#112030,#112031,#112032,#112033,#112034,
#112035,#112036,#112037,#112038,#112039,#112040,#112041,#112042,#112043,
#112044,#112045,#112046,#112047,#112048,#112049,#112050,#112051,#112052,
#112053,#112054,#112055,#112056,#112057,#112058,#112059,#112060,#112061,
#112062,#112063,#112064,#112065,#112066,#112067),.UNSPECIFIED.,.F.,.F.,
(4,3,3,3,3,3,3,3,3,3,3,3,3,3,3,3,3,3,3,3,3,3,3,3,3,3,3,4),(-0.226379821609573,
-0.216598310100724,-0.202320352416955,-0.197194587028726,-0.193788187974472,
-0.178894738696219,-0.169329727438014,-0.165216054886868,-0.161050933351805,
-0.146381862171498,-0.132316768710259,-0.124831238690339,-0.120870158045062,
-0.117643417161341,-0.104003776331328,-0.102374648630577,-0.0883202432056002,
-0.0820195682337035,-0.0785432646891857,-0.0759675957890928,-0.062423681066772,
-0.0489709890027446,-0.0428226697475022,-0.0393194641576752,-0.0361992866354357,
-0.0232864813778267,-0.0108353570978016,0.),.UNSPECIFIED.);
#24617=B_SPLINE_CURVE_WITH_KNOTS('',3,(#112400,#112401,#112402,#112403,
#112404,#112405,#112406),.UNSPECIFIED.,.F.,.F.,(4,3,4),(76.5167332940995,
76.5787766940371,77.4926187885482),.UNSPECIFIED.);
#24618=B_SPLINE_CURVE_WITH_KNOTS('',3,(#112408,#112409,#112410,#112411,
#112412,#112413,#112414,#112415,#112416,#112417,#112418,#112419,#112420,
#112421,#112422,#112423,#112424,#112425,#112426,#112427,#112428,#112429,
#112430,#112431,#112432,#112433,#112434,#112435,#112436,#112437,#112438,
#112439,#112440,#112441,#112442,#112443,#112444,#112445,#112446,#112447,
#112448,#112449,#112450,#112451,#112452,#112453,#112454,#112455,#112456,
#112457,#112458,#112459,#112460,#112461,#112462,#112463,#112464,#112465,
#112466,#112467,#112468,#112469,#112470,#112471,#112472,#112473,#112474,
#112475,#112476,#112477,#112478,#112479,#112480,#112481,#112482,#112483,
#112484,#112485,#112486,#112487,#112488,#112489),.UNSPECIFIED.,.F.,.F.,
(4,3,3,3,3,3,3,3,3,3,3,3,3,3,3,3,3,3,3,3,3,3,3,3,3,3,3,4),(-0.227523845437304,
-0.219644941593212,-0.206672788411716,-0.201988507240929,-0.199228678135215,
-0.186142197116225,-0.177357886994353,-0.174280886377888,-0.171522097642482,
-0.157608502267172,-0.143805090711497,-0.136820747068934,-0.133782715582441,
-0.130929893645298,-0.116671804148527,-0.115867716141243,-0.102113570864824,
-0.0955239927945993,-0.0919125441244498,-0.0890238521567004,-0.0747164149647553,
-0.0600826747802964,-0.0525723404327594,-0.0471438710041018,-0.0444000939394238,
-0.0292633362002102,-0.0142357658394895,0.),.UNSPECIFIED.);
#24619=B_SPLINE_CURVE_WITH_KNOTS('',3,(#112490,#112491,#112492,#112493,
#112494,#112495,#112496,#112497,#112498),.UNSPECIFIED.,.F.,.F.,(4,1,1,1,
1,1,4),(10.3760149606788,11.2898570551899,12.284386622645,13.2789161901,
14.273445757555,15.26797532501,15.7079632679489),.UNSPECIFIED.);
#24620=B_SPLINE_CURVE_WITH_KNOTS('',3,(#112503,#112504,#112505,#112506,
#112507,#112508,#112509,#112510,#112511,#112512,#112513,#112514,#112515,
#112516,#112517,#112518,#112519,#112520,#112521,#112522,#112523,#112524,
#112525,#112526,#112527,#112528,#112529,#112530,#112531,#112532,#112533,
#112534,#112535,#112536,#112537,#112538,#112539,#112540,#112541,#112542,
#112543,#112544,#112545,#112546,#112547,#112548,#112549,#112550,#112551,
#112552,#112553,#112554,#112555,#112556,#112557,#112558,#112559,#112560,
#112561,#112562,#112563,#112564,#112565,#112566,#112567,#112568,#112569,
#112570,#112571,#112572,#112573,#112574,#112575,#112576,#112577,#112578,
#112579,#112580,#112581,#112582,#112583,#112584),.UNSPECIFIED.,.F.,.F.,
(4,3,3,3,3,3,3,3,3,3,3,3,3,3,3,3,3,3,3,3,3,3,3,3,3,3,3,4),(-0.226379821609617,
-0.216598310100761,-0.202320352416989,-0.197194584463025,-0.193788183076757,
-0.178894733706718,-0.169329723072201,-0.165216045592835,-0.161050933697972,
-0.146381862431125,-0.132316761525014,-0.124831233301406,-0.120870151653617,
-0.117643414358862,-0.104003766621399,-0.102374648630583,-0.0883203225023742,
-0.0820195870500072,-0.0785433310585492,-0.0759676655609074,-0.0624237500455779,
-0.0489710625427503,-0.0428226961256205,-0.0393194822861717,-0.0361992934244102,
-0.0232864953899939,-0.0108353829046375,0.),.UNSPECIFIED.);
#24621=B_SPLINE_CURVE_WITH_KNOTS('',3,(#112588,#112589,#112590,#112591,
#112592,#112593,#112594,#112595),.UNSPECIFIED.,.F.,.F.,(4,1,1,1,1,4),(11.6151336144496,
12.6096631819046,13.6041927493596,14.5987223168147,15.5932518842697,15.7079632679489),
 .UNSPECIFIED.);
#24622=B_SPLINE_CURVE_WITH_KNOTS('',3,(#112928,#112929,#112930,#112931),
 .UNSPECIFIED.,.F.,.F.,(4,4),(-79.5623653964022,-79.4910533396544),
 .UNSPECIFIED.);
#24623=VERTEX_POINT('',#76152);
#24624=VERTEX_POINT('',#76153);
#24625=VERTEX_POINT('',#76157);
#24626=VERTEX_POINT('',#76159);
#24627=VERTEX_POINT('',#76170);
#24628=VERTEX_POINT('',#76174);
#24629=VERTEX_POINT('',#76185);
#24630=VERTEX_POINT('',#76189);
#24631=VERTEX_POINT('',#76200);
#24632=VERTEX_POINT('',#76204);
#24633=VERTEX_POINT('',#76215);
#24634=VERTEX_POINT('',#76219);
#24635=VERTEX_POINT('',#76230);
#24636=VERTEX_POINT('',#76234);
#24637=VERTEX_POINT('',#76245);
#24638=VERTEX_POINT('',#76249);
#24639=VERTEX_POINT('',#76272);
#24640=VERTEX_POINT('',#76273);
#24641=VERTEX_POINT('',#76277);
#24642=VERTEX_POINT('',#76279);
#24643=VERTEX_POINT('',#76290);
#24644=VERTEX_POINT('',#76294);
#24645=VERTEX_POINT('',#76305);
#24646=VERTEX_POINT('',#76309);
#24647=VERTEX_POINT('',#76320);
#24648=VERTEX_POINT('',#76324);
#24649=VERTEX_POINT('',#76335);
#24650=VERTEX_POINT('',#76339);
#24651=VERTEX_POINT('',#76350);
#24652=VERTEX_POINT('',#76354);
#24653=VERTEX_POINT('',#76365);
#24654=VERTEX_POINT('',#76369);
#24655=VERTEX_POINT('',#76380);
#24656=VERTEX_POINT('',#76384);
#24657=VERTEX_POINT('',#76395);
#24658=VERTEX_POINT('',#76399);
#24659=VERTEX_POINT('',#76410);
#24660=VERTEX_POINT('',#76414);
#24661=VERTEX_POINT('',#76425);
#24662=VERTEX_POINT('',#76429);
#24663=VERTEX_POINT('',#76453);
#24664=VERTEX_POINT('',#76454);
#24665=VERTEX_POINT('',#76458);
#24666=VERTEX_POINT('',#76460);
#24667=VERTEX_POINT('',#76471);
#24668=VERTEX_POINT('',#76475);
#24669=VERTEX_POINT('',#76486);
#24670=VERTEX_POINT('',#76490);
#24671=VERTEX_POINT('',#76501);
#24672=VERTEX_POINT('',#76505);
#24673=VERTEX_POINT('',#76516);
#24674=VERTEX_POINT('',#76520);
#24675=VERTEX_POINT('',#76531);
#24676=VERTEX_POINT('',#76535);
#24677=VERTEX_POINT('',#76546);
#24678=VERTEX_POINT('',#76550);
#24679=VERTEX_POINT('',#76573);
#24680=VERTEX_POINT('',#76574);
#24681=VERTEX_POINT('',#76578);
#24682=VERTEX_POINT('',#76580);
#24683=VERTEX_POINT('',#76591);
#24684=VERTEX_POINT('',#76595);
#24685=VERTEX_POINT('',#76606);
#24686=VERTEX_POINT('',#76610);
#24687=VERTEX_POINT('',#76621);
#24688=VERTEX_POINT('',#76625);
#24689=VERTEX_POINT('',#76636);
#24690=VERTEX_POINT('',#76640);
#24691=VERTEX_POINT('',#76651);
#24692=VERTEX_POINT('',#76655);
#24693=VERTEX_POINT('',#76666);
#24694=VERTEX_POINT('',#76670);
#24695=VERTEX_POINT('',#76681);
#24696=VERTEX_POINT('',#76685);
#24697=VERTEX_POINT('',#76696);
#24698=VERTEX_POINT('',#76700);
#24699=VERTEX_POINT('',#76711);
#24700=VERTEX_POINT('',#76715);
#24701=VERTEX_POINT('',#76726);
#24702=VERTEX_POINT('',#76730);
#24703=VERTEX_POINT('',#76741);
#24704=VERTEX_POINT('',#76745);
#24705=VERTEX_POINT('',#76756);
#24706=VERTEX_POINT('',#76760);
#24707=VERTEX_POINT('',#76771);
#24708=VERTEX_POINT('',#76775);
#24709=VERTEX_POINT('',#76786);
#24710=VERTEX_POINT('',#76790);
#24711=VERTEX_POINT('',#76801);
#24712=VERTEX_POINT('',#76805);
#24713=VERTEX_POINT('',#76816);
#24714=VERTEX_POINT('',#76820);
#24715=VERTEX_POINT('',#76831);
#24716=VERTEX_POINT('',#76835);
#24717=VERTEX_POINT('',#76846);
#24718=VERTEX_POINT('',#76850);
#24719=VERTEX_POINT('',#76861);
#24720=VERTEX_POINT('',#76865);
#24721=VERTEX_POINT('',#76871);
#24722=VERTEX_POINT('',#76873);
#24723=VERTEX_POINT('',#76897);
#24724=VERTEX_POINT('',#76898);
#24725=VERTEX_POINT('',#76902);
#24726=VERTEX_POINT('',#76904);
#24727=VERTEX_POINT('',#76915);
#24728=VERTEX_POINT('',#76919);
#24729=VERTEX_POINT('',#76930);
#24730=VERTEX_POINT('',#76934);
#24731=VERTEX_POINT('',#76945);
#24732=VERTEX_POINT('',#76949);
#24733=VERTEX_POINT('',#76960);
#24734=VERTEX_POINT('',#76964);
#24735=VERTEX_POINT('',#76975);
#24736=VERTEX_POINT('',#76979);
#24737=VERTEX_POINT('',#76990);
#24738=VERTEX_POINT('',#76994);
#24739=VERTEX_POINT('',#77017);
#24740=VERTEX_POINT('',#77018);
#24741=VERTEX_POINT('',#77022);
#24742=VERTEX_POINT('',#77024);
#24743=VERTEX_POINT('',#77035);
#24744=VERTEX_POINT('',#77039);
#24745=VERTEX_POINT('',#77050);
#24746=VERTEX_POINT('',#77054);
#24747=VERTEX_POINT('',#77065);
#24748=VERTEX_POINT('',#77069);
#24749=VERTEX_POINT('',#77080);
#24750=VERTEX_POINT('',#77084);
#24751=VERTEX_POINT('',#77095);
#24752=VERTEX_POINT('',#77099);
#24753=VERTEX_POINT('',#77110);
#24754=VERTEX_POINT('',#77114);
#24755=VERTEX_POINT('',#77125);
#24756=VERTEX_POINT('',#77129);
#24757=VERTEX_POINT('',#77140);
#24758=VERTEX_POINT('',#77144);
#24759=VERTEX_POINT('',#77155);
#24760=VERTEX_POINT('',#77159);
#24761=VERTEX_POINT('',#77170);
#24762=VERTEX_POINT('',#77174);
#24763=VERTEX_POINT('',#77198);
#24764=VERTEX_POINT('',#77199);
#24765=VERTEX_POINT('',#77203);
#24766=VERTEX_POINT('',#77205);
#24767=VERTEX_POINT('',#77216);
#24768=VERTEX_POINT('',#77220);
#24769=VERTEX_POINT('',#77231);
#24770=VERTEX_POINT('',#77235);
#24771=VERTEX_POINT('',#77246);
#24772=VERTEX_POINT('',#77250);
#24773=VERTEX_POINT('',#77261);
#24774=VERTEX_POINT('',#77265);
#24775=VERTEX_POINT('',#77276);
#24776=VERTEX_POINT('',#77280);
#24777=VERTEX_POINT('',#77291);
#24778=VERTEX_POINT('',#77295);
#24779=VERTEX_POINT('',#77318);
#24780=VERTEX_POINT('',#77319);
#24781=VERTEX_POINT('',#77323);
#24782=VERTEX_POINT('',#77325);
#24783=VERTEX_POINT('',#77336);
#24784=VERTEX_POINT('',#77340);
#24785=VERTEX_POINT('',#77351);
#24786=VERTEX_POINT('',#77355);
#24787=VERTEX_POINT('',#77366);
#24788=VERTEX_POINT('',#77370);
#24789=VERTEX_POINT('',#77381);
#24790=VERTEX_POINT('',#77385);
#24791=VERTEX_POINT('',#77396);
#24792=VERTEX_POINT('',#77400);
#24793=VERTEX_POINT('',#77411);
#24794=VERTEX_POINT('',#77415);
#24795=VERTEX_POINT('',#77426);
#24796=VERTEX_POINT('',#77430);
#24797=VERTEX_POINT('',#77453);
#24798=VERTEX_POINT('',#77454);
#24799=VERTEX_POINT('',#77458);
#24800=VERTEX_POINT('',#77460);
#24801=VERTEX_POINT('',#77471);
#24802=VERTEX_POINT('',#77475);
#24803=VERTEX_POINT('',#77486);
#24804=VERTEX_POINT('',#77490);
#24805=VERTEX_POINT('',#77501);
#24806=VERTEX_POINT('',#77505);
#24807=VERTEX_POINT('',#77516);
#24808=VERTEX_POINT('',#77520);
#24809=VERTEX_POINT('',#77531);
#24810=VERTEX_POINT('',#77535);
#24811=VERTEX_POINT('',#77546);
#24812=VERTEX_POINT('',#77550);
#24813=VERTEX_POINT('',#77561);
#24814=VERTEX_POINT('',#77565);
#24815=VERTEX_POINT('',#77576);
#24816=VERTEX_POINT('',#77580);
#24817=VERTEX_POINT('',#77591);
#24818=VERTEX_POINT('',#77595);
#24819=VERTEX_POINT('',#77606);
#24820=VERTEX_POINT('',#77610);
#24821=VERTEX_POINT('',#77621);
#24822=VERTEX_POINT('',#77625);
#24823=VERTEX_POINT('',#77636);
#24824=VERTEX_POINT('',#77640);
#24825=VERTEX_POINT('',#77651);
#24826=VERTEX_POINT('',#77655);
#24827=VERTEX_POINT('',#77666);
#24828=VERTEX_POINT('',#77670);
#24829=VERTEX_POINT('',#77697);
#24830=VERTEX_POINT('',#77698);
#24831=VERTEX_POINT('',#77702);
#24832=VERTEX_POINT('',#77704);
#24833=VERTEX_POINT('',#77715);
#24834=VERTEX_POINT('',#77719);
#24835=VERTEX_POINT('',#77730);
#24836=VERTEX_POINT('',#77734);
#24837=VERTEX_POINT('',#77745);
#24838=VERTEX_POINT('',#77749);
#24839=VERTEX_POINT('',#77760);
#24840=VERTEX_POINT('',#77764);
#24841=VERTEX_POINT('',#77775);
#24842=VERTEX_POINT('',#77779);
#24843=VERTEX_POINT('',#77790);
#24844=VERTEX_POINT('',#77794);
#24845=VERTEX_POINT('',#77817);
#24846=VERTEX_POINT('',#77818);
#24847=VERTEX_POINT('',#77822);
#24848=VERTEX_POINT('',#77824);
#24849=VERTEX_POINT('',#77835);
#24850=VERTEX_POINT('',#77839);
#24851=VERTEX_POINT('',#77850);
#24852=VERTEX_POINT('',#77854);
#24853=VERTEX_POINT('',#77865);
#24854=VERTEX_POINT('',#77869);
#24855=VERTEX_POINT('',#77880);
#24856=VERTEX_POINT('',#77884);
#24857=VERTEX_POINT('',#77895);
#24858=VERTEX_POINT('',#77899);
#24859=VERTEX_POINT('',#77910);
#24860=VERTEX_POINT('',#77914);
#24861=VERTEX_POINT('',#77925);
#24862=VERTEX_POINT('',#77929);
#24863=VERTEX_POINT('',#77940);
#24864=VERTEX_POINT('',#77944);
#24865=VERTEX_POINT('',#77955);
#24866=VERTEX_POINT('',#77959);
#24867=VERTEX_POINT('',#77970);
#24868=VERTEX_POINT('',#77974);
#24869=VERTEX_POINT('',#77998);
#24870=VERTEX_POINT('',#77999);
#24871=VERTEX_POINT('',#78003);
#24872=VERTEX_POINT('',#78005);
#24873=VERTEX_POINT('',#78016);
#24874=VERTEX_POINT('',#78020);
#24875=VERTEX_POINT('',#78031);
#24876=VERTEX_POINT('',#78035);
#24877=VERTEX_POINT('',#78041);
#24878=VERTEX_POINT('',#78043);
#24879=VERTEX_POINT('',#78052);
#24880=VERTEX_POINT('',#78056);
#24881=VERTEX_POINT('',#78067);
#24882=VERTEX_POINT('',#78071);
#24883=VERTEX_POINT('',#78082);
#24884=VERTEX_POINT('',#78086);
#24885=VERTEX_POINT('',#78092);
#24886=VERTEX_POINT('',#78094);
#24887=VERTEX_POINT('',#78098);
#24888=VERTEX_POINT('',#78100);
#24889=VERTEX_POINT('',#78104);
#24890=VERTEX_POINT('',#78106);
#24891=VERTEX_POINT('',#78120);
#24892=VERTEX_POINT('',#78121);
#24893=VERTEX_POINT('',#78125);
#24894=VERTEX_POINT('',#78127);
#24895=VERTEX_POINT('',#78138);
#24896=VERTEX_POINT('',#78142);
#24897=VERTEX_POINT('',#78153);
#24898=VERTEX_POINT('',#78157);
#24899=VERTEX_POINT('',#78168);
#24900=VERTEX_POINT('',#78172);
#24901=VERTEX_POINT('',#78183);
#24902=VERTEX_POINT('',#78187);
#24903=VERTEX_POINT('',#78198);
#24904=VERTEX_POINT('',#78202);
#24905=VERTEX_POINT('',#78213);
#24906=VERTEX_POINT('',#78217);
#24907=VERTEX_POINT('',#78240);
#24908=VERTEX_POINT('',#78241);
#24909=VERTEX_POINT('',#78245);
#24910=VERTEX_POINT('',#78247);
#24911=VERTEX_POINT('',#78258);
#24912=VERTEX_POINT('',#78262);
#24913=VERTEX_POINT('',#78273);
#24914=VERTEX_POINT('',#78277);
#24915=VERTEX_POINT('',#78288);
#24916=VERTEX_POINT('',#78292);
#24917=VERTEX_POINT('',#78303);
#24918=VERTEX_POINT('',#78307);
#24919=VERTEX_POINT('',#78318);
#24920=VERTEX_POINT('',#78322);
#24921=VERTEX_POINT('',#78333);
#24922=VERTEX_POINT('',#78337);
#24923=VERTEX_POINT('',#78348);
#24924=VERTEX_POINT('',#78352);
#24925=VERTEX_POINT('',#78363);
#24926=VERTEX_POINT('',#78367);
#24927=VERTEX_POINT('',#78378);
#24928=VERTEX_POINT('',#78382);
#24929=VERTEX_POINT('',#78393);
#24930=VERTEX_POINT('',#78397);
#24931=VERTEX_POINT('',#78421);
#24932=VERTEX_POINT('',#78422);
#24933=VERTEX_POINT('',#78426);
#24934=VERTEX_POINT('',#78428);
#24935=VERTEX_POINT('',#78439);
#24936=VERTEX_POINT('',#78443);
#24937=VERTEX_POINT('',#78454);
#24938=VERTEX_POINT('',#78458);
#24939=VERTEX_POINT('',#78469);
#24940=VERTEX_POINT('',#78473);
#24941=VERTEX_POINT('',#78484);
#24942=VERTEX_POINT('',#78488);
#24943=VERTEX_POINT('',#78499);
#24944=VERTEX_POINT('',#78503);
#24945=VERTEX_POINT('',#78514);
#24946=VERTEX_POINT('',#78518);
#24947=VERTEX_POINT('',#78529);
#24948=VERTEX_POINT('',#78533);
#24949=VERTEX_POINT('',#78556);
#24950=VERTEX_POINT('',#78557);
#24951=VERTEX_POINT('',#78561);
#24952=VERTEX_POINT('',#78563);
#24953=VERTEX_POINT('',#78574);
#24954=VERTEX_POINT('',#78578);
#24955=VERTEX_POINT('',#78589);
#24956=VERTEX_POINT('',#78593);
#24957=VERTEX_POINT('',#78604);
#24958=VERTEX_POINT('',#78608);
#24959=VERTEX_POINT('',#78619);
#24960=VERTEX_POINT('',#78623);
#24961=VERTEX_POINT('',#78634);
#24962=VERTEX_POINT('',#78638);
#24963=VERTEX_POINT('',#78649);
#24964=VERTEX_POINT('',#78653);
#24965=VERTEX_POINT('',#78664);
#24966=VERTEX_POINT('',#78668);
#24967=VERTEX_POINT('',#78679);
#24968=VERTEX_POINT('',#78683);
#24969=VERTEX_POINT('',#78694);
#24970=VERTEX_POINT('',#78698);
#24971=VERTEX_POINT('',#78709);
#24972=VERTEX_POINT('',#78713);
#24973=VERTEX_POINT('',#78724);
#24974=VERTEX_POINT('',#78728);
#24975=VERTEX_POINT('',#78739);
#24976=VERTEX_POINT('',#78743);
#24977=VERTEX_POINT('',#78754);
#24978=VERTEX_POINT('',#78758);
#24979=VERTEX_POINT('',#78769);
#24980=VERTEX_POINT('',#78773);
#24981=VERTEX_POINT('',#78784);
#24982=VERTEX_POINT('',#78788);
#24983=VERTEX_POINT('',#78799);
#24984=VERTEX_POINT('',#78803);
#24985=VERTEX_POINT('',#78809);
#24986=VERTEX_POINT('',#78811);
#24987=VERTEX_POINT('',#78835);
#24988=VERTEX_POINT('',#78836);
#24989=VERTEX_POINT('',#78840);
#24990=VERTEX_POINT('',#78842);
#24991=VERTEX_POINT('',#78853);
#24992=VERTEX_POINT('',#78857);
#24993=VERTEX_POINT('',#78868);
#24994=VERTEX_POINT('',#78872);
#24995=VERTEX_POINT('',#78883);
#24996=VERTEX_POINT('',#78887);
#24997=VERTEX_POINT('',#78898);
#24998=VERTEX_POINT('',#78902);
#24999=VERTEX_POINT('',#78913);
#25000=VERTEX_POINT('',#78917);
#25001=VERTEX_POINT('',#78928);
#25002=VERTEX_POINT('',#78932);
#25003=VERTEX_POINT('',#78955);
#25004=VERTEX_POINT('',#78956);
#25005=VERTEX_POINT('',#78960);
#25006=VERTEX_POINT('',#78962);
#25007=VERTEX_POINT('',#78973);
#25008=VERTEX_POINT('',#78977);
#25009=VERTEX_POINT('',#78988);
#25010=VERTEX_POINT('',#78992);
#25011=VERTEX_POINT('',#79003);
#25012=VERTEX_POINT('',#79007);
#25013=VERTEX_POINT('',#79018);
#25014=VERTEX_POINT('',#79022);
#25015=VERTEX_POINT('',#79033);
#25016=VERTEX_POINT('',#79037);
#25017=VERTEX_POINT('',#79048);
#25018=VERTEX_POINT('',#79052);
#25019=VERTEX_POINT('',#79063);
#25020=VERTEX_POINT('',#79067);
#25021=VERTEX_POINT('',#79078);
#25022=VERTEX_POINT('',#79082);
#25023=VERTEX_POINT('',#79093);
#25024=VERTEX_POINT('',#79097);
#25025=VERTEX_POINT('',#79108);
#25026=VERTEX_POINT('',#79112);
#25027=VERTEX_POINT('',#79136);
#25028=VERTEX_POINT('',#79137);
#25029=VERTEX_POINT('',#79141);
#25030=VERTEX_POINT('',#79143);
#25031=VERTEX_POINT('',#79154);
#25032=VERTEX_POINT('',#79158);
#25033=VERTEX_POINT('',#79169);
#25034=VERTEX_POINT('',#79173);
#25035=VERTEX_POINT('',#79184);
#25036=VERTEX_POINT('',#79188);
#25037=VERTEX_POINT('',#79199);
#25038=VERTEX_POINT('',#79203);
#25039=VERTEX_POINT('',#79214);
#25040=VERTEX_POINT('',#79218);
#25041=VERTEX_POINT('',#79224);
#25042=VERTEX_POINT('',#79226);
#25043=VERTEX_POINT('',#79230);
#25044=VERTEX_POINT('',#79232);
#25045=VERTEX_POINT('',#79236);
#25046=VERTEX_POINT('',#79238);
#25047=VERTEX_POINT('',#79242);
#25048=VERTEX_POINT('',#79244);
#25049=VERTEX_POINT('',#79248);
#25050=VERTEX_POINT('',#79250);
#25051=VERTEX_POINT('',#79254);
#25052=VERTEX_POINT('',#79256);
#25053=VERTEX_POINT('',#79265);
#25054=VERTEX_POINT('',#79269);
#25055=VERTEX_POINT('',#79280);
#25056=VERTEX_POINT('',#79284);
#25057=VERTEX_POINT('',#79295);
#25058=VERTEX_POINT('',#79299);
#25059=VERTEX_POINT('',#79310);
#25060=VERTEX_POINT('',#79314);
#25061=VERTEX_POINT('',#79325);
#25062=VERTEX_POINT('',#79329);
#25063=VERTEX_POINT('',#79340);
#25064=VERTEX_POINT('',#79344);
#25065=VERTEX_POINT('',#79355);
#25066=VERTEX_POINT('',#79359);
#25067=VERTEX_POINT('',#79370);
#25068=VERTEX_POINT('',#79374);
#25069=VERTEX_POINT('',#79380);
#25070=VERTEX_POINT('',#79382);
#25071=VERTEX_POINT('',#79405);
#25072=VERTEX_POINT('',#79406);
#25073=VERTEX_POINT('',#79410);
#25074=VERTEX_POINT('',#79412);
#25075=VERTEX_POINT('',#79423);
#25076=VERTEX_POINT('',#79427);
#25077=VERTEX_POINT('',#79438);
#25078=VERTEX_POINT('',#79442);
#25079=VERTEX_POINT('',#79453);
#25080=VERTEX_POINT('',#79457);
#25081=VERTEX_POINT('',#79468);
#25082=VERTEX_POINT('',#79472);
#25083=VERTEX_POINT('',#79483);
#25084=VERTEX_POINT('',#79487);
#25085=VERTEX_POINT('',#79498);
#25086=VERTEX_POINT('',#79502);
#25087=VERTEX_POINT('',#79525);
#25088=VERTEX_POINT('',#79526);
#25089=VERTEX_POINT('',#79530);
#25090=VERTEX_POINT('',#79532);
#25091=VERTEX_POINT('',#79543);
#25092=VERTEX_POINT('',#79547);
#25093=VERTEX_POINT('',#79558);
#25094=VERTEX_POINT('',#79562);
#25095=VERTEX_POINT('',#79573);
#25096=VERTEX_POINT('',#79577);
#25097=VERTEX_POINT('',#79588);
#25098=VERTEX_POINT('',#79592);
#25099=VERTEX_POINT('',#79603);
#25100=VERTEX_POINT('',#79607);
#25101=VERTEX_POINT('',#79618);
#25102=VERTEX_POINT('',#79622);
#25103=VERTEX_POINT('',#79633);
#25104=VERTEX_POINT('',#79637);
#25105=VERTEX_POINT('',#79648);
#25106=VERTEX_POINT('',#79652);
#25107=VERTEX_POINT('',#79663);
#25108=VERTEX_POINT('',#79667);
#25109=VERTEX_POINT('',#79678);
#25110=VERTEX_POINT('',#79682);
#25111=VERTEX_POINT('',#79701);
#25112=VERTEX_POINT('',#79702);
#25113=VERTEX_POINT('',#79704);
#25114=VERTEX_POINT('',#79706);
#25115=VERTEX_POINT('',#79710);
#25116=VERTEX_POINT('',#79712);
#25117=VERTEX_POINT('',#79719);
#25118=VERTEX_POINT('',#79720);
#25119=VERTEX_POINT('',#79722);
#25120=VERTEX_POINT('',#79724);
#25121=VERTEX_POINT('',#79728);
#25122=VERTEX_POINT('',#79730);
#25123=VERTEX_POINT('',#79734);
#25124=VERTEX_POINT('',#79736);
#25125=VERTEX_POINT('',#79740);
#25126=VERTEX_POINT('',#79742);
#25127=VERTEX_POINT('',#79746);
#25128=VERTEX_POINT('',#79748);
#25129=VERTEX_POINT('',#79752);
#25130=VERTEX_POINT('',#79754);
#25131=VERTEX_POINT('',#79758);
#25132=VERTEX_POINT('',#79760);
#25133=VERTEX_POINT('',#79764);
#25134=VERTEX_POINT('',#79766);
#25135=VERTEX_POINT('',#79770);
#25136=VERTEX_POINT('',#79772);
#25137=VERTEX_POINT('',#79776);
#25138=VERTEX_POINT('',#79778);
#25139=VERTEX_POINT('',#79793);
#25140=VERTEX_POINT('',#79794);
#25141=VERTEX_POINT('',#79798);
#25142=VERTEX_POINT('',#79800);
#25143=VERTEX_POINT('',#79811);
#25144=VERTEX_POINT('',#79815);
#25145=VERTEX_POINT('',#79826);
#25146=VERTEX_POINT('',#79830);
#25147=VERTEX_POINT('',#79841);
#25148=VERTEX_POINT('',#79845);
#25149=VERTEX_POINT('',#79856);
#25150=VERTEX_POINT('',#79860);
#25151=VERTEX_POINT('',#79871);
#25152=VERTEX_POINT('',#79875);
#25153=VERTEX_POINT('',#79886);
#25154=VERTEX_POINT('',#79890);
#25155=VERTEX_POINT('',#79913);
#25156=VERTEX_POINT('',#79914);
#25157=VERTEX_POINT('',#79918);
#25158=VERTEX_POINT('',#79920);
#25159=VERTEX_POINT('',#79931);
#25160=VERTEX_POINT('',#79935);
#25161=VERTEX_POINT('',#79946);
#25162=VERTEX_POINT('',#79950);
#25163=VERTEX_POINT('',#79961);
#25164=VERTEX_POINT('',#79965);
#25165=VERTEX_POINT('',#79976);
#25166=VERTEX_POINT('',#79980);
#25167=VERTEX_POINT('',#79991);
#25168=VERTEX_POINT('',#79995);
#25169=VERTEX_POINT('',#80006);
#25170=VERTEX_POINT('',#80010);
#25171=VERTEX_POINT('',#80021);
#25172=VERTEX_POINT('',#80025);
#25173=VERTEX_POINT('',#80036);
#25174=VERTEX_POINT('',#80040);
#25175=VERTEX_POINT('',#80051);
#25176=VERTEX_POINT('',#80055);
#25177=VERTEX_POINT('',#80066);
#25178=VERTEX_POINT('',#80070);
#25179=VERTEX_POINT('',#80094);
#25180=VERTEX_POINT('',#80095);
#25181=VERTEX_POINT('',#80099);
#25182=VERTEX_POINT('',#80101);
#25183=VERTEX_POINT('',#80112);
#25184=VERTEX_POINT('',#80116);
#25185=VERTEX_POINT('',#80127);
#25186=VERTEX_POINT('',#80131);
#25187=VERTEX_POINT('',#80142);
#25188=VERTEX_POINT('',#80146);
#25189=VERTEX_POINT('',#80157);
#25190=VERTEX_POINT('',#80161);
#25191=VERTEX_POINT('',#80172);
#25192=VERTEX_POINT('',#80176);
#25193=VERTEX_POINT('',#80187);
#25194=VERTEX_POINT('',#80191);
#25195=VERTEX_POINT('',#80202);
#25196=VERTEX_POINT('',#80206);
#25197=VERTEX_POINT('',#80217);
#25198=VERTEX_POINT('',#80221);
#25199=VERTEX_POINT('',#80232);
#25200=VERTEX_POINT('',#80236);
#25201=VERTEX_POINT('',#80247);
#25202=VERTEX_POINT('',#80251);
#25203=VERTEX_POINT('',#80262);
#25204=VERTEX_POINT('',#80266);
#25205=VERTEX_POINT('',#80272);
#25206=VERTEX_POINT('',#80274);
#25207=VERTEX_POINT('',#80283);
#25208=VERTEX_POINT('',#80287);
#25209=VERTEX_POINT('',#80298);
#25210=VERTEX_POINT('',#80302);
#25211=VERTEX_POINT('',#80313);
#25212=VERTEX_POINT('',#80317);
#25213=VERTEX_POINT('',#80328);
#25214=VERTEX_POINT('',#80332);
#25215=VERTEX_POINT('',#80343);
#25216=VERTEX_POINT('',#80347);
#25217=VERTEX_POINT('',#80358);
#25218=VERTEX_POINT('',#80362);
#25219=VERTEX_POINT('',#80373);
#25220=VERTEX_POINT('',#80377);
#25221=VERTEX_POINT('',#80383);
#25222=VERTEX_POINT('',#80385);
#25223=VERTEX_POINT('',#80394);
#25224=VERTEX_POINT('',#80398);
#25225=VERTEX_POINT('',#80409);
#25226=VERTEX_POINT('',#80413);
#25227=VERTEX_POINT('',#80424);
#25228=VERTEX_POINT('',#80428);
#25229=VERTEX_POINT('',#80439);
#25230=VERTEX_POINT('',#80443);
#25231=VERTEX_POINT('',#80454);
#25232=VERTEX_POINT('',#80458);
#25233=VERTEX_POINT('',#80469);
#25234=VERTEX_POINT('',#80473);
#25235=VERTEX_POINT('',#80484);
#25236=VERTEX_POINT('',#80488);
#25237=VERTEX_POINT('',#80494);
#25238=VERTEX_POINT('',#80496);
#25239=VERTEX_POINT('',#80519);
#25240=VERTEX_POINT('',#80520);
#25241=VERTEX_POINT('',#80524);
#25242=VERTEX_POINT('',#80526);
#25243=VERTEX_POINT('',#80537);
#25244=VERTEX_POINT('',#80541);
#25245=VERTEX_POINT('',#80552);
#25246=VERTEX_POINT('',#80556);
#25247=VERTEX_POINT('',#80567);
#25248=VERTEX_POINT('',#80571);
#25249=VERTEX_POINT('',#80582);
#25250=VERTEX_POINT('',#80586);
#25251=VERTEX_POINT('',#80597);
#25252=VERTEX_POINT('',#80601);
#25253=VERTEX_POINT('',#80612);
#25254=VERTEX_POINT('',#80616);
#25255=VERTEX_POINT('',#80639);
#25256=VERTEX_POINT('',#80640);
#25257=VERTEX_POINT('',#80644);
#25258=VERTEX_POINT('',#80646);
#25259=VERTEX_POINT('',#80657);
#25260=VERTEX_POINT('',#80661);
#25261=VERTEX_POINT('',#80672);
#25262=VERTEX_POINT('',#80676);
#25263=VERTEX_POINT('',#80687);
#25264=VERTEX_POINT('',#80691);
#25265=VERTEX_POINT('',#80702);
#25266=VERTEX_POINT('',#80706);
#25267=VERTEX_POINT('',#80717);
#25268=VERTEX_POINT('',#80721);
#25269=VERTEX_POINT('',#80732);
#25270=VERTEX_POINT('',#80736);
#25271=VERTEX_POINT('',#80747);
#25272=VERTEX_POINT('',#80751);
#25273=VERTEX_POINT('',#80762);
#25274=VERTEX_POINT('',#80766);
#25275=VERTEX_POINT('',#80777);
#25276=VERTEX_POINT('',#80781);
#25277=VERTEX_POINT('',#80792);
#25278=VERTEX_POINT('',#80796);
#25279=VERTEX_POINT('',#80820);
#25280=VERTEX_POINT('',#80821);
#25281=VERTEX_POINT('',#80825);
#25282=VERTEX_POINT('',#80827);
#25283=VERTEX_POINT('',#80838);
#25284=VERTEX_POINT('',#80842);
#25285=VERTEX_POINT('',#80853);
#25286=VERTEX_POINT('',#80857);
#25287=VERTEX_POINT('',#80868);
#25288=VERTEX_POINT('',#80872);
#25289=VERTEX_POINT('',#80883);
#25290=VERTEX_POINT('',#80887);
#25291=VERTEX_POINT('',#80898);
#25292=VERTEX_POINT('',#80902);
#25293=VERTEX_POINT('',#80913);
#25294=VERTEX_POINT('',#80917);
#25295=VERTEX_POINT('',#80928);
#25296=VERTEX_POINT('',#80932);
#25297=VERTEX_POINT('',#80943);
#25298=VERTEX_POINT('',#80947);
#25299=VERTEX_POINT('',#80953);
#25300=VERTEX_POINT('',#80955);
#25301=VERTEX_POINT('',#80964);
#25302=VERTEX_POINT('',#80968);
#25303=VERTEX_POINT('',#80979);
#25304=VERTEX_POINT('',#80983);
#25305=VERTEX_POINT('',#80994);
#25306=VERTEX_POINT('',#80998);
#25307=VERTEX_POINT('',#81009);
#25308=VERTEX_POINT('',#81013);
#25309=VERTEX_POINT('',#81024);
#25310=VERTEX_POINT('',#81028);
#25311=VERTEX_POINT('',#81039);
#25312=VERTEX_POINT('',#81043);
#25313=VERTEX_POINT('',#81054);
#25314=VERTEX_POINT('',#81058);
#25315=VERTEX_POINT('',#81069);
#25316=VERTEX_POINT('',#81073);
#25317=VERTEX_POINT('',#81084);
#25318=VERTEX_POINT('',#81088);
#25319=VERTEX_POINT('',#81094);
#25320=VERTEX_POINT('',#81096);
#25321=VERTEX_POINT('',#81100);
#25322=VERTEX_POINT('',#81102);
#25323=VERTEX_POINT('',#81116);
#25324=VERTEX_POINT('',#81117);
#25325=VERTEX_POINT('',#81121);
#25326=VERTEX_POINT('',#81123);
#25327=VERTEX_POINT('',#81134);
#25328=VERTEX_POINT('',#81138);
#25329=VERTEX_POINT('',#81149);
#25330=VERTEX_POINT('',#81153);
#25331=VERTEX_POINT('',#81164);
#25332=VERTEX_POINT('',#81168);
#25333=VERTEX_POINT('',#81179);
#25334=VERTEX_POINT('',#81183);
#25335=VERTEX_POINT('',#81194);
#25336=VERTEX_POINT('',#81198);
#25337=VERTEX_POINT('',#81209);
#25338=VERTEX_POINT('',#81213);
#25339=VERTEX_POINT('',#81236);
#25340=VERTEX_POINT('',#81237);
#25341=VERTEX_POINT('',#81241);
#25342=VERTEX_POINT('',#81243);
#25343=VERTEX_POINT('',#81254);
#25344=VERTEX_POINT('',#81258);
#25345=VERTEX_POINT('',#81269);
#25346=VERTEX_POINT('',#81273);
#25347=VERTEX_POINT('',#81284);
#25348=VERTEX_POINT('',#81288);
#25349=VERTEX_POINT('',#81299);
#25350=VERTEX_POINT('',#81303);
#25351=VERTEX_POINT('',#81314);
#25352=VERTEX_POINT('',#81318);
#25353=VERTEX_POINT('',#81329);
#25354=VERTEX_POINT('',#81333);
#25355=VERTEX_POINT('',#81344);
#25356=VERTEX_POINT('',#81348);
#25357=VERTEX_POINT('',#81359);
#25358=VERTEX_POINT('',#81363);
#25359=VERTEX_POINT('',#81374);
#25360=VERTEX_POINT('',#81378);
#25361=VERTEX_POINT('',#81389);
#25362=VERTEX_POINT('',#81393);
#25363=VERTEX_POINT('',#81412);
#25364=VERTEX_POINT('',#81413);
#25365=VERTEX_POINT('',#81415);
#25366=VERTEX_POINT('',#81417);
#25367=VERTEX_POINT('',#81426);
#25368=VERTEX_POINT('',#81430);
#25369=VERTEX_POINT('',#81441);
#25370=VERTEX_POINT('',#81445);
#25371=VERTEX_POINT('',#81451);
#25372=VERTEX_POINT('',#81453);
#25373=VERTEX_POINT('',#81462);
#25374=VERTEX_POINT('',#81466);
#25375=VERTEX_POINT('',#81477);
#25376=VERTEX_POINT('',#81481);
#25377=VERTEX_POINT('',#81487);
#25378=VERTEX_POINT('',#81489);
#25379=VERTEX_POINT('',#81493);
#25380=VERTEX_POINT('',#81495);
#25381=VERTEX_POINT('',#81509);
#25382=VERTEX_POINT('',#81510);
#25383=VERTEX_POINT('',#81514);
#25384=VERTEX_POINT('',#81516);
#25385=VERTEX_POINT('',#81527);
#25386=VERTEX_POINT('',#81531);
#25387=VERTEX_POINT('',#81542);
#25388=VERTEX_POINT('',#81546);
#25389=VERTEX_POINT('',#81557);
#25390=VERTEX_POINT('',#81561);
#25391=VERTEX_POINT('',#81572);
#25392=VERTEX_POINT('',#81576);
#25393=VERTEX_POINT('',#81587);
#25394=VERTEX_POINT('',#81591);
#25395=VERTEX_POINT('',#81602);
#25396=VERTEX_POINT('',#81606);
#25397=VERTEX_POINT('',#81629);
#25398=VERTEX_POINT('',#81630);
#25399=VERTEX_POINT('',#81634);
#25400=VERTEX_POINT('',#81636);
#25401=VERTEX_POINT('',#81647);
#25402=VERTEX_POINT('',#81651);
#25403=VERTEX_POINT('',#81662);
#25404=VERTEX_POINT('',#81666);
#25405=VERTEX_POINT('',#81677);
#25406=VERTEX_POINT('',#81681);
#25407=VERTEX_POINT('',#81692);
#25408=VERTEX_POINT('',#81696);
#25409=VERTEX_POINT('',#81707);
#25410=VERTEX_POINT('',#81711);
#25411=VERTEX_POINT('',#81722);
#25412=VERTEX_POINT('',#81726);
#25413=VERTEX_POINT('',#81737);
#25414=VERTEX_POINT('',#81741);
#25415=VERTEX_POINT('',#81752);
#25416=VERTEX_POINT('',#81756);
#25417=VERTEX_POINT('',#81767);
#25418=VERTEX_POINT('',#81771);
#25419=VERTEX_POINT('',#81782);
#25420=VERTEX_POINT('',#81786);
#25421=VERTEX_POINT('',#81811);
#25422=VERTEX_POINT('',#81812);
#25423=VERTEX_POINT('',#81816);
#25424=VERTEX_POINT('',#81818);
#25425=VERTEX_POINT('',#81829);
#25426=VERTEX_POINT('',#81833);
#25427=VERTEX_POINT('',#81844);
#25428=VERTEX_POINT('',#81848);
#25429=VERTEX_POINT('',#81859);
#25430=VERTEX_POINT('',#81863);
#25431=VERTEX_POINT('',#81874);
#25432=VERTEX_POINT('',#81878);
#25433=VERTEX_POINT('',#81889);
#25434=VERTEX_POINT('',#81893);
#25435=VERTEX_POINT('',#81904);
#25436=VERTEX_POINT('',#81908);
#25437=VERTEX_POINT('',#81931);
#25438=VERTEX_POINT('',#81932);
#25439=VERTEX_POINT('',#81936);
#25440=VERTEX_POINT('',#81938);
#25441=VERTEX_POINT('',#81949);
#25442=VERTEX_POINT('',#81953);
#25443=VERTEX_POINT('',#81964);
#25444=VERTEX_POINT('',#81968);
#25445=VERTEX_POINT('',#81979);
#25446=VERTEX_POINT('',#81983);
#25447=VERTEX_POINT('',#81994);
#25448=VERTEX_POINT('',#81998);
#25449=VERTEX_POINT('',#82009);
#25450=VERTEX_POINT('',#82013);
#25451=VERTEX_POINT('',#82024);
#25452=VERTEX_POINT('',#82028);
#25453=VERTEX_POINT('',#82039);
#25454=VERTEX_POINT('',#82043);
#25455=VERTEX_POINT('',#82054);
#25456=VERTEX_POINT('',#82058);
#25457=VERTEX_POINT('',#82069);
#25458=VERTEX_POINT('',#82073);
#25459=VERTEX_POINT('',#82084);
#25460=VERTEX_POINT('',#82088);
#25461=VERTEX_POINT('',#82107);
#25462=VERTEX_POINT('',#82108);
#25463=VERTEX_POINT('',#82110);
#25464=VERTEX_POINT('',#82112);
#25465=VERTEX_POINT('',#82121);
#25466=VERTEX_POINT('',#82125);
#25467=VERTEX_POINT('',#82136);
#25468=VERTEX_POINT('',#82140);
#25469=VERTEX_POINT('',#82146);
#25470=VERTEX_POINT('',#82148);
#25471=VERTEX_POINT('',#82157);
#25472=VERTEX_POINT('',#82161);
#25473=VERTEX_POINT('',#82172);
#25474=VERTEX_POINT('',#82176);
#25475=VERTEX_POINT('',#82182);
#25476=VERTEX_POINT('',#82184);
#25477=VERTEX_POINT('',#82188);
#25478=VERTEX_POINT('',#82190);
#25479=VERTEX_POINT('',#82204);
#25480=VERTEX_POINT('',#82205);
#25481=VERTEX_POINT('',#82209);
#25482=VERTEX_POINT('',#82211);
#25483=VERTEX_POINT('',#82222);
#25484=VERTEX_POINT('',#82226);
#25485=VERTEX_POINT('',#82237);
#25486=VERTEX_POINT('',#82241);
#25487=VERTEX_POINT('',#82252);
#25488=VERTEX_POINT('',#82256);
#25489=VERTEX_POINT('',#82267);
#25490=VERTEX_POINT('',#82271);
#25491=VERTEX_POINT('',#82282);
#25492=VERTEX_POINT('',#82286);
#25493=VERTEX_POINT('',#82297);
#25494=VERTEX_POINT('',#82301);
#25495=VERTEX_POINT('',#82324);
#25496=VERTEX_POINT('',#82325);
#25497=VERTEX_POINT('',#82329);
#25498=VERTEX_POINT('',#82331);
#25499=VERTEX_POINT('',#82342);
#25500=VERTEX_POINT('',#82346);
#25501=VERTEX_POINT('',#82357);
#25502=VERTEX_POINT('',#82361);
#25503=VERTEX_POINT('',#82372);
#25504=VERTEX_POINT('',#82376);
#25505=VERTEX_POINT('',#82387);
#25506=VERTEX_POINT('',#82391);
#25507=VERTEX_POINT('',#82402);
#25508=VERTEX_POINT('',#82406);
#25509=VERTEX_POINT('',#82417);
#25510=VERTEX_POINT('',#82421);
#25511=VERTEX_POINT('',#82432);
#25512=VERTEX_POINT('',#82436);
#25513=VERTEX_POINT('',#82447);
#25514=VERTEX_POINT('',#82451);
#25515=VERTEX_POINT('',#82462);
#25516=VERTEX_POINT('',#82466);
#25517=VERTEX_POINT('',#82477);
#25518=VERTEX_POINT('',#82481);
#25519=VERTEX_POINT('',#82505);
#25520=VERTEX_POINT('',#82506);
#25521=VERTEX_POINT('',#82510);
#25522=VERTEX_POINT('',#82512);
#25523=VERTEX_POINT('',#82523);
#25524=VERTEX_POINT('',#82527);
#25525=VERTEX_POINT('',#82538);
#25526=VERTEX_POINT('',#82542);
#25527=VERTEX_POINT('',#82553);
#25528=VERTEX_POINT('',#82557);
#25529=VERTEX_POINT('',#82568);
#25530=VERTEX_POINT('',#82572);
#25531=VERTEX_POINT('',#82583);
#25532=VERTEX_POINT('',#82587);
#25533=VERTEX_POINT('',#82598);
#25534=VERTEX_POINT('',#82602);
#25535=VERTEX_POINT('',#82613);
#25536=VERTEX_POINT('',#82617);
#25537=VERTEX_POINT('',#82628);
#25538=VERTEX_POINT('',#82632);
#25539=VERTEX_POINT('',#82638);
#25540=VERTEX_POINT('',#82640);
#25541=VERTEX_POINT('',#82649);
#25542=VERTEX_POINT('',#82653);
#25543=VERTEX_POINT('',#82664);
#25544=VERTEX_POINT('',#82668);
#25545=VERTEX_POINT('',#82679);
#25546=VERTEX_POINT('',#82683);
#25547=VERTEX_POINT('',#82694);
#25548=VERTEX_POINT('',#82698);
#25549=VERTEX_POINT('',#82709);
#25550=VERTEX_POINT('',#82713);
#25551=VERTEX_POINT('',#82724);
#25552=VERTEX_POINT('',#82728);
#25553=VERTEX_POINT('',#82739);
#25554=VERTEX_POINT('',#82743);
#25555=VERTEX_POINT('',#82754);
#25556=VERTEX_POINT('',#82758);
#25557=VERTEX_POINT('',#82769);
#25558=VERTEX_POINT('',#82773);
#25559=VERTEX_POINT('',#82779);
#25560=VERTEX_POINT('',#82781);
#25561=VERTEX_POINT('',#82785);
#25562=VERTEX_POINT('',#82787);
#25563=VERTEX_POINT('',#82801);
#25564=VERTEX_POINT('',#82802);
#25565=VERTEX_POINT('',#82806);
#25566=VERTEX_POINT('',#82808);
#25567=VERTEX_POINT('',#82819);
#25568=VERTEX_POINT('',#82823);
#25569=VERTEX_POINT('',#82834);
#25570=VERTEX_POINT('',#82838);
#25571=VERTEX_POINT('',#82849);
#25572=VERTEX_POINT('',#82853);
#25573=VERTEX_POINT('',#82864);
#25574=VERTEX_POINT('',#82868);
#25575=VERTEX_POINT('',#82879);
#25576=VERTEX_POINT('',#82883);
#25577=VERTEX_POINT('',#82894);
#25578=VERTEX_POINT('',#82898);
#25579=VERTEX_POINT('',#82921);
#25580=VERTEX_POINT('',#82922);
#25581=VERTEX_POINT('',#82926);
#25582=VERTEX_POINT('',#82928);
#25583=VERTEX_POINT('',#82939);
#25584=VERTEX_POINT('',#82943);
#25585=VERTEX_POINT('',#82954);
#25586=VERTEX_POINT('',#82958);
#25587=VERTEX_POINT('',#82969);
#25588=VERTEX_POINT('',#82973);
#25589=VERTEX_POINT('',#82984);
#25590=VERTEX_POINT('',#82988);
#25591=VERTEX_POINT('',#82999);
#25592=VERTEX_POINT('',#83003);
#25593=VERTEX_POINT('',#83014);
#25594=VERTEX_POINT('',#83018);
#25595=VERTEX_POINT('',#83029);
#25596=VERTEX_POINT('',#83033);
#25597=VERTEX_POINT('',#83044);
#25598=VERTEX_POINT('',#83048);
#25599=VERTEX_POINT('',#83059);
#25600=VERTEX_POINT('',#83063);
#25601=VERTEX_POINT('',#83074);
#25602=VERTEX_POINT('',#83078);
#25603=VERTEX_POINT('',#83102);
#25604=VERTEX_POINT('',#83103);
#25605=VERTEX_POINT('',#83107);
#25606=VERTEX_POINT('',#83109);
#25607=VERTEX_POINT('',#83120);
#25608=VERTEX_POINT('',#83124);
#25609=VERTEX_POINT('',#83135);
#25610=VERTEX_POINT('',#83139);
#25611=VERTEX_POINT('',#83150);
#25612=VERTEX_POINT('',#83154);
#25613=VERTEX_POINT('',#83165);
#25614=VERTEX_POINT('',#83169);
#25615=VERTEX_POINT('',#83180);
#25616=VERTEX_POINT('',#83184);
#25617=VERTEX_POINT('',#83195);
#25618=VERTEX_POINT('',#83199);
#25619=VERTEX_POINT('',#83210);
#25620=VERTEX_POINT('',#83214);
#25621=VERTEX_POINT('',#83225);
#25622=VERTEX_POINT('',#83229);
#25623=VERTEX_POINT('',#83240);
#25624=VERTEX_POINT('',#83244);
#25625=VERTEX_POINT('',#83255);
#25626=VERTEX_POINT('',#83259);
#25627=VERTEX_POINT('',#83270);
#25628=VERTEX_POINT('',#83274);
#25629=VERTEX_POINT('',#83280);
#25630=VERTEX_POINT('',#83282);
#25631=VERTEX_POINT('',#83291);
#25632=VERTEX_POINT('',#83295);
#25633=VERTEX_POINT('',#83306);
#25634=VERTEX_POINT('',#83310);
#25635=VERTEX_POINT('',#83321);
#25636=VERTEX_POINT('',#83325);
#25637=VERTEX_POINT('',#83336);
#25638=VERTEX_POINT('',#83340);
#25639=VERTEX_POINT('',#83351);
#25640=VERTEX_POINT('',#83355);
#25641=VERTEX_POINT('',#83366);
#25642=VERTEX_POINT('',#83370);
#25643=VERTEX_POINT('',#83381);
#25644=VERTEX_POINT('',#83385);
#25645=VERTEX_POINT('',#83391);
#25646=VERTEX_POINT('',#83393);
#25647=VERTEX_POINT('',#83402);
#25648=VERTEX_POINT('',#83406);
#25649=VERTEX_POINT('',#83417);
#25650=VERTEX_POINT('',#83421);
#25651=VERTEX_POINT('',#83432);
#25652=VERTEX_POINT('',#83436);
#25653=VERTEX_POINT('',#83447);
#25654=VERTEX_POINT('',#83451);
#25655=VERTEX_POINT('',#83462);
#25656=VERTEX_POINT('',#83466);
#25657=VERTEX_POINT('',#83477);
#25658=VERTEX_POINT('',#83481);
#25659=VERTEX_POINT('',#83492);
#25660=VERTEX_POINT('',#83496);
#25661=VERTEX_POINT('',#83502);
#25662=VERTEX_POINT('',#83504);
#25663=VERTEX_POINT('',#83527);
#25664=VERTEX_POINT('',#83528);
#25665=VERTEX_POINT('',#83532);
#25666=VERTEX_POINT('',#83534);
#25667=VERTEX_POINT('',#83545);
#25668=VERTEX_POINT('',#83549);
#25669=VERTEX_POINT('',#83560);
#25670=VERTEX_POINT('',#83564);
#25671=VERTEX_POINT('',#83575);
#25672=VERTEX_POINT('',#83579);
#25673=VERTEX_POINT('',#83590);
#25674=VERTEX_POINT('',#83594);
#25675=VERTEX_POINT('',#83605);
#25676=VERTEX_POINT('',#83609);
#25677=VERTEX_POINT('',#83620);
#25678=VERTEX_POINT('',#83624);
#25679=VERTEX_POINT('',#83647);
#25680=VERTEX_POINT('',#83648);
#25681=VERTEX_POINT('',#83652);
#25682=VERTEX_POINT('',#83654);
#25683=VERTEX_POINT('',#83665);
#25684=VERTEX_POINT('',#83669);
#25685=VERTEX_POINT('',#83680);
#25686=VERTEX_POINT('',#83684);
#25687=VERTEX_POINT('',#83695);
#25688=VERTEX_POINT('',#83699);
#25689=VERTEX_POINT('',#83710);
#25690=VERTEX_POINT('',#83714);
#25691=VERTEX_POINT('',#83725);
#25692=VERTEX_POINT('',#83729);
#25693=VERTEX_POINT('',#83740);
#25694=VERTEX_POINT('',#83744);
#25695=VERTEX_POINT('',#83755);
#25696=VERTEX_POINT('',#83759);
#25697=VERTEX_POINT('',#83770);
#25698=VERTEX_POINT('',#83774);
#25699=VERTEX_POINT('',#83785);
#25700=VERTEX_POINT('',#83789);
#25701=VERTEX_POINT('',#83800);
#25702=VERTEX_POINT('',#83804);
#25703=VERTEX_POINT('',#83823);
#25704=VERTEX_POINT('',#83824);
#25705=VERTEX_POINT('',#83826);
#25706=VERTEX_POINT('',#83828);
#25707=VERTEX_POINT('',#83832);
#25708=VERTEX_POINT('',#83834);
#25709=VERTEX_POINT('',#83841);
#25710=VERTEX_POINT('',#83842);
#25711=VERTEX_POINT('',#83844);
#25712=VERTEX_POINT('',#83846);
#25713=VERTEX_POINT('',#83850);
#25714=VERTEX_POINT('',#83852);
#25715=VERTEX_POINT('',#83856);
#25716=VERTEX_POINT('',#83858);
#25717=VERTEX_POINT('',#83862);
#25718=VERTEX_POINT('',#83864);
#25719=VERTEX_POINT('',#83868);
#25720=VERTEX_POINT('',#83870);
#25721=VERTEX_POINT('',#83874);
#25722=VERTEX_POINT('',#83876);
#25723=VERTEX_POINT('',#83880);
#25724=VERTEX_POINT('',#83882);
#25725=VERTEX_POINT('',#83886);
#25726=VERTEX_POINT('',#83888);
#25727=VERTEX_POINT('',#83892);
#25728=VERTEX_POINT('',#83894);
#25729=VERTEX_POINT('',#83898);
#25730=VERTEX_POINT('',#83900);
#25731=VERTEX_POINT('',#83915);
#25732=VERTEX_POINT('',#83916);
#25733=VERTEX_POINT('',#83920);
#25734=VERTEX_POINT('',#83922);
#25735=VERTEX_POINT('',#83933);
#25736=VERTEX_POINT('',#83937);
#25737=VERTEX_POINT('',#83948);
#25738=VERTEX_POINT('',#83952);
#25739=VERTEX_POINT('',#83963);
#25740=VERTEX_POINT('',#83967);
#25741=VERTEX_POINT('',#83978);
#25742=VERTEX_POINT('',#83982);
#25743=VERTEX_POINT('',#83993);
#25744=VERTEX_POINT('',#83997);
#25745=VERTEX_POINT('',#84008);
#25746=VERTEX_POINT('',#84012);
#25747=VERTEX_POINT('',#84035);
#25748=VERTEX_POINT('',#84036);
#25749=VERTEX_POINT('',#84040);
#25750=VERTEX_POINT('',#84042);
#25751=VERTEX_POINT('',#84053);
#25752=VERTEX_POINT('',#84057);
#25753=VERTEX_POINT('',#84068);
#25754=VERTEX_POINT('',#84072);
#25755=VERTEX_POINT('',#84083);
#25756=VERTEX_POINT('',#84087);
#25757=VERTEX_POINT('',#84098);
#25758=VERTEX_POINT('',#84102);
#25759=VERTEX_POINT('',#84113);
#25760=VERTEX_POINT('',#84117);
#25761=VERTEX_POINT('',#84128);
#25762=VERTEX_POINT('',#84132);
#25763=VERTEX_POINT('',#84143);
#25764=VERTEX_POINT('',#84147);
#25765=VERTEX_POINT('',#84158);
#25766=VERTEX_POINT('',#84162);
#25767=VERTEX_POINT('',#84173);
#25768=VERTEX_POINT('',#84177);
#25769=VERTEX_POINT('',#84188);
#25770=VERTEX_POINT('',#84192);
#25771=VERTEX_POINT('',#84216);
#25772=VERTEX_POINT('',#84217);
#25773=VERTEX_POINT('',#84221);
#25774=VERTEX_POINT('',#84223);
#25775=VERTEX_POINT('',#84234);
#25776=VERTEX_POINT('',#84238);
#25777=VERTEX_POINT('',#84249);
#25778=VERTEX_POINT('',#84253);
#25779=VERTEX_POINT('',#84264);
#25780=VERTEX_POINT('',#84268);
#25781=VERTEX_POINT('',#84279);
#25782=VERTEX_POINT('',#84283);
#25783=VERTEX_POINT('',#84294);
#25784=VERTEX_POINT('',#84298);
#25785=VERTEX_POINT('',#84304);
#25786=VERTEX_POINT('',#84306);
#25787=VERTEX_POINT('',#84310);
#25788=VERTEX_POINT('',#84312);
#25789=VERTEX_POINT('',#84316);
#25790=VERTEX_POINT('',#84318);
#25791=VERTEX_POINT('',#84322);
#25792=VERTEX_POINT('',#84324);
#25793=VERTEX_POINT('',#84328);
#25794=VERTEX_POINT('',#84330);
#25795=VERTEX_POINT('',#84334);
#25796=VERTEX_POINT('',#84336);
#25797=VERTEX_POINT('',#84345);
#25798=VERTEX_POINT('',#84349);
#25799=VERTEX_POINT('',#84360);
#25800=VERTEX_POINT('',#84364);
#25801=VERTEX_POINT('',#84375);
#25802=VERTEX_POINT('',#84379);
#25803=VERTEX_POINT('',#84390);
#25804=VERTEX_POINT('',#84394);
#25805=VERTEX_POINT('',#84405);
#25806=VERTEX_POINT('',#84409);
#25807=VERTEX_POINT('',#84420);
#25808=VERTEX_POINT('',#84424);
#25809=VERTEX_POINT('',#84435);
#25810=VERTEX_POINT('',#84439);
#25811=VERTEX_POINT('',#84450);
#25812=VERTEX_POINT('',#84454);
#25813=VERTEX_POINT('',#84460);
#25814=VERTEX_POINT('',#84462);
#25815=VERTEX_POINT('',#84485);
#25816=VERTEX_POINT('',#84486);
#25817=VERTEX_POINT('',#84490);
#25818=VERTEX_POINT('',#84492);
#25819=VERTEX_POINT('',#84503);
#25820=VERTEX_POINT('',#84507);
#25821=VERTEX_POINT('',#84518);
#25822=VERTEX_POINT('',#84522);
#25823=VERTEX_POINT('',#84533);
#25824=VERTEX_POINT('',#84537);
#25825=VERTEX_POINT('',#84548);
#25826=VERTEX_POINT('',#84552);
#25827=VERTEX_POINT('',#84563);
#25828=VERTEX_POINT('',#84567);
#25829=VERTEX_POINT('',#84578);
#25830=VERTEX_POINT('',#84582);
#25831=VERTEX_POINT('',#84605);
#25832=VERTEX_POINT('',#84606);
#25833=VERTEX_POINT('',#84610);
#25834=VERTEX_POINT('',#84612);
#25835=VERTEX_POINT('',#84623);
#25836=VERTEX_POINT('',#84627);
#25837=VERTEX_POINT('',#84638);
#25838=VERTEX_POINT('',#84642);
#25839=VERTEX_POINT('',#84653);
#25840=VERTEX_POINT('',#84657);
#25841=VERTEX_POINT('',#84668);
#25842=VERTEX_POINT('',#84672);
#25843=VERTEX_POINT('',#84683);
#25844=VERTEX_POINT('',#84687);
#25845=VERTEX_POINT('',#84698);
#25846=VERTEX_POINT('',#84702);
#25847=VERTEX_POINT('',#84713);
#25848=VERTEX_POINT('',#84717);
#25849=VERTEX_POINT('',#84728);
#25850=VERTEX_POINT('',#84732);
#25851=VERTEX_POINT('',#84743);
#25852=VERTEX_POINT('',#84747);
#25853=VERTEX_POINT('',#84758);
#25854=VERTEX_POINT('',#84762);
#25855=VERTEX_POINT('',#84786);
#25856=VERTEX_POINT('',#84787);
#25857=VERTEX_POINT('',#84791);
#25858=VERTEX_POINT('',#84793);
#25859=VERTEX_POINT('',#84804);
#25860=VERTEX_POINT('',#84808);
#25861=VERTEX_POINT('',#84819);
#25862=VERTEX_POINT('',#84823);
#25863=VERTEX_POINT('',#84834);
#25864=VERTEX_POINT('',#84838);
#25865=VERTEX_POINT('',#84849);
#25866=VERTEX_POINT('',#84853);
#25867=VERTEX_POINT('',#84864);
#25868=VERTEX_POINT('',#84868);
#25869=VERTEX_POINT('',#84879);
#25870=VERTEX_POINT('',#84883);
#25871=VERTEX_POINT('',#84894);
#25872=VERTEX_POINT('',#84898);
#25873=VERTEX_POINT('',#84921);
#25874=VERTEX_POINT('',#84922);
#25875=VERTEX_POINT('',#84926);
#25876=VERTEX_POINT('',#84928);
#25877=VERTEX_POINT('',#84939);
#25878=VERTEX_POINT('',#84943);
#25879=VERTEX_POINT('',#84954);
#25880=VERTEX_POINT('',#84958);
#25881=VERTEX_POINT('',#84969);
#25882=VERTEX_POINT('',#84973);
#25883=VERTEX_POINT('',#84984);
#25884=VERTEX_POINT('',#84988);
#25885=VERTEX_POINT('',#84999);
#25886=VERTEX_POINT('',#85003);
#25887=VERTEX_POINT('',#85014);
#25888=VERTEX_POINT('',#85018);
#25889=VERTEX_POINT('',#85029);
#25890=VERTEX_POINT('',#85033);
#25891=VERTEX_POINT('',#85044);
#25892=VERTEX_POINT('',#85048);
#25893=VERTEX_POINT('',#85059);
#25894=VERTEX_POINT('',#85063);
#25895=VERTEX_POINT('',#85074);
#25896=VERTEX_POINT('',#85078);
#25897=VERTEX_POINT('',#85089);
#25898=VERTEX_POINT('',#85093);
#25899=VERTEX_POINT('',#85104);
#25900=VERTEX_POINT('',#85108);
#25901=VERTEX_POINT('',#85119);
#25902=VERTEX_POINT('',#85123);
#25903=VERTEX_POINT('',#85134);
#25904=VERTEX_POINT('',#85138);
#25905=VERTEX_POINT('',#85149);
#25906=VERTEX_POINT('',#85153);
#25907=VERTEX_POINT('',#85164);
#25908=VERTEX_POINT('',#85168);
#25909=VERTEX_POINT('',#85174);
#25910=VERTEX_POINT('',#85176);
#25911=VERTEX_POINT('',#85200);
#25912=VERTEX_POINT('',#85201);
#25913=VERTEX_POINT('',#85205);
#25914=VERTEX_POINT('',#85207);
#25915=VERTEX_POINT('',#85218);
#25916=VERTEX_POINT('',#85222);
#25917=VERTEX_POINT('',#85233);
#25918=VERTEX_POINT('',#85237);
#25919=VERTEX_POINT('',#85248);
#25920=VERTEX_POINT('',#85252);
#25921=VERTEX_POINT('',#85263);
#25922=VERTEX_POINT('',#85267);
#25923=VERTEX_POINT('',#85278);
#25924=VERTEX_POINT('',#85282);
#25925=VERTEX_POINT('',#85293);
#25926=VERTEX_POINT('',#85297);
#25927=VERTEX_POINT('',#85320);
#25928=VERTEX_POINT('',#85321);
#25929=VERTEX_POINT('',#85325);
#25930=VERTEX_POINT('',#85327);
#25931=VERTEX_POINT('',#85338);
#25932=VERTEX_POINT('',#85342);
#25933=VERTEX_POINT('',#85353);
#25934=VERTEX_POINT('',#85357);
#25935=VERTEX_POINT('',#85368);
#25936=VERTEX_POINT('',#85372);
#25937=VERTEX_POINT('',#85383);
#25938=VERTEX_POINT('',#85387);
#25939=VERTEX_POINT('',#85398);
#25940=VERTEX_POINT('',#85402);
#25941=VERTEX_POINT('',#85413);
#25942=VERTEX_POINT('',#85417);
#25943=VERTEX_POINT('',#85428);
#25944=VERTEX_POINT('',#85432);
#25945=VERTEX_POINT('',#85443);
#25946=VERTEX_POINT('',#85447);
#25947=VERTEX_POINT('',#85458);
#25948=VERTEX_POINT('',#85462);
#25949=VERTEX_POINT('',#85473);
#25950=VERTEX_POINT('',#85477);
#25951=VERTEX_POINT('',#85501);
#25952=VERTEX_POINT('',#85502);
#25953=VERTEX_POINT('',#85506);
#25954=VERTEX_POINT('',#85508);
#25955=VERTEX_POINT('',#85519);
#25956=VERTEX_POINT('',#85523);
#25957=VERTEX_POINT('',#85534);
#25958=VERTEX_POINT('',#85538);
#25959=VERTEX_POINT('',#85544);
#25960=VERTEX_POINT('',#85546);
#25961=VERTEX_POINT('',#85555);
#25962=VERTEX_POINT('',#85559);
#25963=VERTEX_POINT('',#85570);
#25964=VERTEX_POINT('',#85574);
#25965=VERTEX_POINT('',#85585);
#25966=VERTEX_POINT('',#85589);
#25967=VERTEX_POINT('',#85595);
#25968=VERTEX_POINT('',#85597);
#25969=VERTEX_POINT('',#85601);
#25970=VERTEX_POINT('',#85603);
#25971=VERTEX_POINT('',#85607);
#25972=VERTEX_POINT('',#85609);
#25973=VERTEX_POINT('',#85623);
#25974=VERTEX_POINT('',#85624);
#25975=VERTEX_POINT('',#85628);
#25976=VERTEX_POINT('',#85630);
#25977=VERTEX_POINT('',#85641);
#25978=VERTEX_POINT('',#85645);
#25979=VERTEX_POINT('',#85656);
#25980=VERTEX_POINT('',#85660);
#25981=VERTEX_POINT('',#85671);
#25982=VERTEX_POINT('',#85675);
#25983=VERTEX_POINT('',#85686);
#25984=VERTEX_POINT('',#85690);
#25985=VERTEX_POINT('',#85701);
#25986=VERTEX_POINT('',#85705);
#25987=VERTEX_POINT('',#85716);
#25988=VERTEX_POINT('',#85720);
#25989=VERTEX_POINT('',#85743);
#25990=VERTEX_POINT('',#85744);
#25991=VERTEX_POINT('',#85748);
#25992=VERTEX_POINT('',#85750);
#25993=VERTEX_POINT('',#85761);
#25994=VERTEX_POINT('',#85765);
#25995=VERTEX_POINT('',#85776);
#25996=VERTEX_POINT('',#85780);
#25997=VERTEX_POINT('',#85791);
#25998=VERTEX_POINT('',#85795);
#25999=VERTEX_POINT('',#85806);
#26000=VERTEX_POINT('',#85810);
#26001=VERTEX_POINT('',#85821);
#26002=VERTEX_POINT('',#85825);
#26003=VERTEX_POINT('',#85836);
#26004=VERTEX_POINT('',#85840);
#26005=VERTEX_POINT('',#85851);
#26006=VERTEX_POINT('',#85855);
#26007=VERTEX_POINT('',#85866);
#26008=VERTEX_POINT('',#85870);
#26009=VERTEX_POINT('',#85881);
#26010=VERTEX_POINT('',#85885);
#26011=VERTEX_POINT('',#85896);
#26012=VERTEX_POINT('',#85900);
#26013=VERTEX_POINT('',#85924);
#26014=VERTEX_POINT('',#85925);
#26015=VERTEX_POINT('',#85929);
#26016=VERTEX_POINT('',#85931);
#26017=VERTEX_POINT('',#85942);
#26018=VERTEX_POINT('',#85946);
#26019=VERTEX_POINT('',#85957);
#26020=VERTEX_POINT('',#85961);
#26021=VERTEX_POINT('',#85972);
#26022=VERTEX_POINT('',#85976);
#26023=VERTEX_POINT('',#85987);
#26024=VERTEX_POINT('',#85991);
#26025=VERTEX_POINT('',#86002);
#26026=VERTEX_POINT('',#86006);
#26027=VERTEX_POINT('',#86017);
#26028=VERTEX_POINT('',#86021);
#26029=VERTEX_POINT('',#86044);
#26030=VERTEX_POINT('',#86045);
#26031=VERTEX_POINT('',#86049);
#26032=VERTEX_POINT('',#86051);
#26033=VERTEX_POINT('',#86062);
#26034=VERTEX_POINT('',#86066);
#26035=VERTEX_POINT('',#86077);
#26036=VERTEX_POINT('',#86081);
#26037=VERTEX_POINT('',#86092);
#26038=VERTEX_POINT('',#86096);
#26039=VERTEX_POINT('',#86107);
#26040=VERTEX_POINT('',#86111);
#26041=VERTEX_POINT('',#86122);
#26042=VERTEX_POINT('',#86126);
#26043=VERTEX_POINT('',#86137);
#26044=VERTEX_POINT('',#86141);
#26045=VERTEX_POINT('',#86152);
#26046=VERTEX_POINT('',#86156);
#26047=VERTEX_POINT('',#86179);
#26048=VERTEX_POINT('',#86180);
#26049=VERTEX_POINT('',#86184);
#26050=VERTEX_POINT('',#86186);
#26051=VERTEX_POINT('',#86197);
#26052=VERTEX_POINT('',#86201);
#26053=VERTEX_POINT('',#86212);
#26054=VERTEX_POINT('',#86216);
#26055=VERTEX_POINT('',#86227);
#26056=VERTEX_POINT('',#86231);
#26057=VERTEX_POINT('',#86242);
#26058=VERTEX_POINT('',#86246);
#26059=VERTEX_POINT('',#86257);
#26060=VERTEX_POINT('',#86261);
#26061=VERTEX_POINT('',#86272);
#26062=VERTEX_POINT('',#86276);
#26063=VERTEX_POINT('',#86287);
#26064=VERTEX_POINT('',#86291);
#26065=VERTEX_POINT('',#86302);
#26066=VERTEX_POINT('',#86306);
#26067=VERTEX_POINT('',#86317);
#26068=VERTEX_POINT('',#86321);
#26069=VERTEX_POINT('',#86332);
#26070=VERTEX_POINT('',#86336);
#26071=VERTEX_POINT('',#86347);
#26072=VERTEX_POINT('',#86351);
#26073=VERTEX_POINT('',#86362);
#26074=VERTEX_POINT('',#86366);
#26075=VERTEX_POINT('',#86377);
#26076=VERTEX_POINT('',#86381);
#26077=VERTEX_POINT('',#86392);
#26078=VERTEX_POINT('',#86396);
#26079=VERTEX_POINT('',#86423);
#26080=VERTEX_POINT('',#86424);
#26081=VERTEX_POINT('',#86428);
#26082=VERTEX_POINT('',#86430);
#26083=VERTEX_POINT('',#86441);
#26084=VERTEX_POINT('',#86445);
#26085=VERTEX_POINT('',#86456);
#26086=VERTEX_POINT('',#86460);
#26087=VERTEX_POINT('',#86471);
#26088=VERTEX_POINT('',#86475);
#26089=VERTEX_POINT('',#86486);
#26090=VERTEX_POINT('',#86490);
#26091=VERTEX_POINT('',#86501);
#26092=VERTEX_POINT('',#86505);
#26093=VERTEX_POINT('',#86516);
#26094=VERTEX_POINT('',#86520);
#26095=VERTEX_POINT('',#86543);
#26096=VERTEX_POINT('',#86544);
#26097=VERTEX_POINT('',#86548);
#26098=VERTEX_POINT('',#86550);
#26099=VERTEX_POINT('',#86561);
#26100=VERTEX_POINT('',#86565);
#26101=VERTEX_POINT('',#86576);
#26102=VERTEX_POINT('',#86580);
#26103=VERTEX_POINT('',#86591);
#26104=VERTEX_POINT('',#86595);
#26105=VERTEX_POINT('',#86606);
#26106=VERTEX_POINT('',#86610);
#26107=VERTEX_POINT('',#86621);
#26108=VERTEX_POINT('',#86625);
#26109=VERTEX_POINT('',#86636);
#26110=VERTEX_POINT('',#86640);
#26111=VERTEX_POINT('',#86651);
#26112=VERTEX_POINT('',#86655);
#26113=VERTEX_POINT('',#86666);
#26114=VERTEX_POINT('',#86670);
#26115=VERTEX_POINT('',#86681);
#26116=VERTEX_POINT('',#86685);
#26117=VERTEX_POINT('',#86696);
#26118=VERTEX_POINT('',#86700);
#26119=VERTEX_POINT('',#86724);
#26120=VERTEX_POINT('',#86725);
#26121=VERTEX_POINT('',#86729);
#26122=VERTEX_POINT('',#86731);
#26123=VERTEX_POINT('',#86742);
#26124=VERTEX_POINT('',#86746);
#26125=VERTEX_POINT('',#86757);
#26126=VERTEX_POINT('',#86761);
#26127=VERTEX_POINT('',#86772);
#26128=VERTEX_POINT('',#86776);
#26129=VERTEX_POINT('',#86787);
#26130=VERTEX_POINT('',#86791);
#26131=VERTEX_POINT('',#86802);
#26132=VERTEX_POINT('',#86806);
#26133=VERTEX_POINT('',#86817);
#26134=VERTEX_POINT('',#86821);
#26135=VERTEX_POINT('',#86844);
#26136=VERTEX_POINT('',#86845);
#26137=VERTEX_POINT('',#86849);
#26138=VERTEX_POINT('',#86851);
#26139=VERTEX_POINT('',#86862);
#26140=VERTEX_POINT('',#86866);
#26141=VERTEX_POINT('',#86877);
#26142=VERTEX_POINT('',#86881);
#26143=VERTEX_POINT('',#86892);
#26144=VERTEX_POINT('',#86896);
#26145=VERTEX_POINT('',#86907);
#26146=VERTEX_POINT('',#86911);
#26147=VERTEX_POINT('',#86922);
#26148=VERTEX_POINT('',#86926);
#26149=VERTEX_POINT('',#86937);
#26150=VERTEX_POINT('',#86941);
#26151=VERTEX_POINT('',#86952);
#26152=VERTEX_POINT('',#86956);
#26153=VERTEX_POINT('',#86967);
#26154=VERTEX_POINT('',#86971);
#26155=VERTEX_POINT('',#86982);
#26156=VERTEX_POINT('',#86986);
#26157=VERTEX_POINT('',#86997);
#26158=VERTEX_POINT('',#87001);
#26159=VERTEX_POINT('',#87012);
#26160=VERTEX_POINT('',#87016);
#26161=VERTEX_POINT('',#87027);
#26162=VERTEX_POINT('',#87031);
#26163=VERTEX_POINT('',#87042);
#26164=VERTEX_POINT('',#87046);
#26165=VERTEX_POINT('',#87057);
#26166=VERTEX_POINT('',#87061);
#26167=VERTEX_POINT('',#87072);
#26168=VERTEX_POINT('',#87076);
#26169=VERTEX_POINT('',#87087);
#26170=VERTEX_POINT('',#87091);
#26171=VERTEX_POINT('',#87102);
#26172=VERTEX_POINT('',#87106);
#26173=VERTEX_POINT('',#87117);
#26174=VERTEX_POINT('',#87121);
#26175=VERTEX_POINT('',#87132);
#26176=VERTEX_POINT('',#87136);
#26177=VERTEX_POINT('',#87142);
#26178=VERTEX_POINT('',#87144);
#26179=VERTEX_POINT('',#87163);
#26180=VERTEX_POINT('',#87164);
#26181=VERTEX_POINT('',#87166);
#26182=VERTEX_POINT('',#87168);
#26183=VERTEX_POINT('',#87172);
#26184=VERTEX_POINT('',#87174);
#26185=VERTEX_POINT('',#87178);
#26186=VERTEX_POINT('',#87180);
#26187=VERTEX_POINT('',#87188);
#26188=VERTEX_POINT('',#87189);
#26189=VERTEX_POINT('',#87191);
#26190=VERTEX_POINT('',#87193);
#26191=VERTEX_POINT('',#87197);
#26192=VERTEX_POINT('',#87199);
#26193=VERTEX_POINT('',#87203);
#26194=VERTEX_POINT('',#87205);
#26195=VERTEX_POINT('',#87213);
#26196=VERTEX_POINT('',#87214);
#26197=VERTEX_POINT('',#87216);
#26198=VERTEX_POINT('',#87218);
#26199=VERTEX_POINT('',#87222);
#26200=VERTEX_POINT('',#87224);
#26201=VERTEX_POINT('',#87228);
#26202=VERTEX_POINT('',#87230);
#26203=VERTEX_POINT('',#87238);
#26204=VERTEX_POINT('',#87239);
#26205=VERTEX_POINT('',#87241);
#26206=VERTEX_POINT('',#87243);
#26207=VERTEX_POINT('',#87247);
#26208=VERTEX_POINT('',#87249);
#26209=VERTEX_POINT('',#87253);
#26210=VERTEX_POINT('',#87255);
#26211=VERTEX_POINT('',#87263);
#26212=VERTEX_POINT('',#87264);
#26213=VERTEX_POINT('',#87266);
#26214=VERTEX_POINT('',#87268);
#26215=VERTEX_POINT('',#87272);
#26216=VERTEX_POINT('',#87274);
#26217=VERTEX_POINT('',#87278);
#26218=VERTEX_POINT('',#87280);
#26219=VERTEX_POINT('',#87288);
#26220=VERTEX_POINT('',#87289);
#26221=VERTEX_POINT('',#87291);
#26222=VERTEX_POINT('',#87293);
#26223=VERTEX_POINT('',#87297);
#26224=VERTEX_POINT('',#87299);
#26225=VERTEX_POINT('',#87303);
#26226=VERTEX_POINT('',#87305);
#26227=VERTEX_POINT('',#87313);
#26228=VERTEX_POINT('',#87314);
#26229=VERTEX_POINT('',#87316);
#26230=VERTEX_POINT('',#87318);
#26231=VERTEX_POINT('',#87322);
#26232=VERTEX_POINT('',#87324);
#26233=VERTEX_POINT('',#87328);
#26234=VERTEX_POINT('',#87330);
#26235=VERTEX_POINT('',#87338);
#26236=VERTEX_POINT('',#87339);
#26237=VERTEX_POINT('',#87341);
#26238=VERTEX_POINT('',#87343);
#26239=VERTEX_POINT('',#87347);
#26240=VERTEX_POINT('',#87349);
#26241=VERTEX_POINT('',#87353);
#26242=VERTEX_POINT('',#87355);
#26243=VERTEX_POINT('',#87363);
#26244=VERTEX_POINT('',#87364);
#26245=VERTEX_POINT('',#87366);
#26246=VERTEX_POINT('',#87368);
#26247=VERTEX_POINT('',#87372);
#26248=VERTEX_POINT('',#87374);
#26249=VERTEX_POINT('',#87378);
#26250=VERTEX_POINT('',#87380);
#26251=VERTEX_POINT('',#87388);
#26252=VERTEX_POINT('',#87389);
#26253=VERTEX_POINT('',#87391);
#26254=VERTEX_POINT('',#87393);
#26255=VERTEX_POINT('',#87397);
#26256=VERTEX_POINT('',#87399);
#26257=VERTEX_POINT('',#87403);
#26258=VERTEX_POINT('',#87405);
#26259=VERTEX_POINT('',#87413);
#26260=VERTEX_POINT('',#87414);
#26261=VERTEX_POINT('',#87416);
#26262=VERTEX_POINT('',#87418);
#26263=VERTEX_POINT('',#87422);
#26264=VERTEX_POINT('',#87424);
#26265=VERTEX_POINT('',#87428);
#26266=VERTEX_POINT('',#87430);
#26267=VERTEX_POINT('',#87438);
#26268=VERTEX_POINT('',#87439);
#26269=VERTEX_POINT('',#87441);
#26270=VERTEX_POINT('',#87443);
#26271=VERTEX_POINT('',#87447);
#26272=VERTEX_POINT('',#87449);
#26273=VERTEX_POINT('',#87453);
#26274=VERTEX_POINT('',#87455);
#26275=VERTEX_POINT('',#87463);
#26276=VERTEX_POINT('',#87464);
#26277=VERTEX_POINT('',#87466);
#26278=VERTEX_POINT('',#87468);
#26279=VERTEX_POINT('',#87472);
#26280=VERTEX_POINT('',#87474);
#26281=VERTEX_POINT('',#87478);
#26282=VERTEX_POINT('',#87480);
#26283=VERTEX_POINT('',#87488);
#26284=VERTEX_POINT('',#87489);
#26285=VERTEX_POINT('',#87491);
#26286=VERTEX_POINT('',#87493);
#26287=VERTEX_POINT('',#87497);
#26288=VERTEX_POINT('',#87499);
#26289=VERTEX_POINT('',#87503);
#26290=VERTEX_POINT('',#87505);
#26291=VERTEX_POINT('',#87513);
#26292=VERTEX_POINT('',#87514);
#26293=VERTEX_POINT('',#87516);
#26294=VERTEX_POINT('',#87518);
#26295=VERTEX_POINT('',#87522);
#26296=VERTEX_POINT('',#87524);
#26297=VERTEX_POINT('',#87528);
#26298=VERTEX_POINT('',#87530);
#26299=VERTEX_POINT('',#87538);
#26300=VERTEX_POINT('',#87539);
#26301=VERTEX_POINT('',#87541);
#26302=VERTEX_POINT('',#87543);
#26303=VERTEX_POINT('',#87547);
#26304=VERTEX_POINT('',#87549);
#26305=VERTEX_POINT('',#87553);
#26306=VERTEX_POINT('',#87555);
#26307=VERTEX_POINT('',#87563);
#26308=VERTEX_POINT('',#87564);
#26309=VERTEX_POINT('',#87566);
#26310=VERTEX_POINT('',#87568);
#26311=VERTEX_POINT('',#87572);
#26312=VERTEX_POINT('',#87574);
#26313=VERTEX_POINT('',#87578);
#26314=VERTEX_POINT('',#87580);
#26315=VERTEX_POINT('',#87588);
#26316=VERTEX_POINT('',#87589);
#26317=VERTEX_POINT('',#87591);
#26318=VERTEX_POINT('',#87593);
#26319=VERTEX_POINT('',#87597);
#26320=VERTEX_POINT('',#87599);
#26321=VERTEX_POINT('',#87603);
#26322=VERTEX_POINT('',#87605);
#26323=VERTEX_POINT('',#87613);
#26324=VERTEX_POINT('',#87614);
#26325=VERTEX_POINT('',#87616);
#26326=VERTEX_POINT('',#87618);
#26327=VERTEX_POINT('',#87622);
#26328=VERTEX_POINT('',#87624);
#26329=VERTEX_POINT('',#87628);
#26330=VERTEX_POINT('',#87630);
#26331=VERTEX_POINT('',#87638);
#26332=VERTEX_POINT('',#87639);
#26333=VERTEX_POINT('',#87641);
#26334=VERTEX_POINT('',#87643);
#26335=VERTEX_POINT('',#87647);
#26336=VERTEX_POINT('',#87649);
#26337=VERTEX_POINT('',#87653);
#26338=VERTEX_POINT('',#87655);
#26339=VERTEX_POINT('',#87663);
#26340=VERTEX_POINT('',#87664);
#26341=VERTEX_POINT('',#87666);
#26342=VERTEX_POINT('',#87668);
#26343=VERTEX_POINT('',#87672);
#26344=VERTEX_POINT('',#87674);
#26345=VERTEX_POINT('',#87678);
#26346=VERTEX_POINT('',#87680);
#26347=VERTEX_POINT('',#87688);
#26348=VERTEX_POINT('',#87689);
#26349=VERTEX_POINT('',#87691);
#26350=VERTEX_POINT('',#87693);
#26351=VERTEX_POINT('',#87697);
#26352=VERTEX_POINT('',#87699);
#26353=VERTEX_POINT('',#87703);
#26354=VERTEX_POINT('',#87705);
#26355=VERTEX_POINT('',#87713);
#26356=VERTEX_POINT('',#87714);
#26357=VERTEX_POINT('',#87716);
#26358=VERTEX_POINT('',#87718);
#26359=VERTEX_POINT('',#87722);
#26360=VERTEX_POINT('',#87724);
#26361=VERTEX_POINT('',#87728);
#26362=VERTEX_POINT('',#87730);
#26363=VERTEX_POINT('',#87738);
#26364=VERTEX_POINT('',#87739);
#26365=VERTEX_POINT('',#87741);
#26366=VERTEX_POINT('',#87743);
#26367=VERTEX_POINT('',#87747);
#26368=VERTEX_POINT('',#87749);
#26369=VERTEX_POINT('',#87753);
#26370=VERTEX_POINT('',#87755);
#26371=VERTEX_POINT('',#87763);
#26372=VERTEX_POINT('',#87764);
#26373=VERTEX_POINT('',#87766);
#26374=VERTEX_POINT('',#87768);
#26375=VERTEX_POINT('',#87772);
#26376=VERTEX_POINT('',#87774);
#26377=VERTEX_POINT('',#87778);
#26378=VERTEX_POINT('',#87780);
#26379=VERTEX_POINT('',#87788);
#26380=VERTEX_POINT('',#87789);
#26381=VERTEX_POINT('',#87791);
#26382=VERTEX_POINT('',#87793);
#26383=VERTEX_POINT('',#87797);
#26384=VERTEX_POINT('',#87799);
#26385=VERTEX_POINT('',#87803);
#26386=VERTEX_POINT('',#87805);
#26387=VERTEX_POINT('',#87813);
#26388=VERTEX_POINT('',#87814);
#26389=VERTEX_POINT('',#87816);
#26390=VERTEX_POINT('',#87818);
#26391=VERTEX_POINT('',#87822);
#26392=VERTEX_POINT('',#87824);
#26393=VERTEX_POINT('',#87828);
#26394=VERTEX_POINT('',#87830);
#26395=VERTEX_POINT('',#87838);
#26396=VERTEX_POINT('',#87839);
#26397=VERTEX_POINT('',#87841);
#26398=VERTEX_POINT('',#87843);
#26399=VERTEX_POINT('',#87847);
#26400=VERTEX_POINT('',#87849);
#26401=VERTEX_POINT('',#87853);
#26402=VERTEX_POINT('',#87855);
#26403=VERTEX_POINT('',#87863);
#26404=VERTEX_POINT('',#87864);
#26405=VERTEX_POINT('',#87866);
#26406=VERTEX_POINT('',#87868);
#26407=VERTEX_POINT('',#87872);
#26408=VERTEX_POINT('',#87874);
#26409=VERTEX_POINT('',#87878);
#26410=VERTEX_POINT('',#87880);
#26411=VERTEX_POINT('',#87888);
#26412=VERTEX_POINT('',#87889);
#26413=VERTEX_POINT('',#87891);
#26414=VERTEX_POINT('',#87893);
#26415=VERTEX_POINT('',#87897);
#26416=VERTEX_POINT('',#87899);
#26417=VERTEX_POINT('',#87903);
#26418=VERTEX_POINT('',#87905);
#26419=VERTEX_POINT('',#87913);
#26420=VERTEX_POINT('',#87914);
#26421=VERTEX_POINT('',#87916);
#26422=VERTEX_POINT('',#87918);
#26423=VERTEX_POINT('',#87922);
#26424=VERTEX_POINT('',#87924);
#26425=VERTEX_POINT('',#87928);
#26426=VERTEX_POINT('',#87930);
#26427=VERTEX_POINT('',#87938);
#26428=VERTEX_POINT('',#87939);
#26429=VERTEX_POINT('',#87941);
#26430=VERTEX_POINT('',#87943);
#26431=VERTEX_POINT('',#87947);
#26432=VERTEX_POINT('',#87949);
#26433=VERTEX_POINT('',#87953);
#26434=VERTEX_POINT('',#87955);
#26435=VERTEX_POINT('',#87963);
#26436=VERTEX_POINT('',#87964);
#26437=VERTEX_POINT('',#87966);
#26438=VERTEX_POINT('',#87968);
#26439=VERTEX_POINT('',#87972);
#26440=VERTEX_POINT('',#87974);
#26441=VERTEX_POINT('',#87978);
#26442=VERTEX_POINT('',#87980);
#26443=VERTEX_POINT('',#87988);
#26444=VERTEX_POINT('',#87989);
#26445=VERTEX_POINT('',#87991);
#26446=VERTEX_POINT('',#87993);
#26447=VERTEX_POINT('',#87997);
#26448=VERTEX_POINT('',#87999);
#26449=VERTEX_POINT('',#88003);
#26450=VERTEX_POINT('',#88005);
#26451=VERTEX_POINT('',#88013);
#26452=VERTEX_POINT('',#88014);
#26453=VERTEX_POINT('',#88016);
#26454=VERTEX_POINT('',#88018);
#26455=VERTEX_POINT('',#88022);
#26456=VERTEX_POINT('',#88024);
#26457=VERTEX_POINT('',#88028);
#26458=VERTEX_POINT('',#88030);
#26459=VERTEX_POINT('',#88038);
#26460=VERTEX_POINT('',#88039);
#26461=VERTEX_POINT('',#88041);
#26462=VERTEX_POINT('',#88043);
#26463=VERTEX_POINT('',#88047);
#26464=VERTEX_POINT('',#88049);
#26465=VERTEX_POINT('',#88053);
#26466=VERTEX_POINT('',#88055);
#26467=VERTEX_POINT('',#88063);
#26468=VERTEX_POINT('',#88064);
#26469=VERTEX_POINT('',#88066);
#26470=VERTEX_POINT('',#88068);
#26471=VERTEX_POINT('',#88072);
#26472=VERTEX_POINT('',#88074);
#26473=VERTEX_POINT('',#88078);
#26474=VERTEX_POINT('',#88080);
#26475=VERTEX_POINT('',#88088);
#26476=VERTEX_POINT('',#88089);
#26477=VERTEX_POINT('',#88091);
#26478=VERTEX_POINT('',#88093);
#26479=VERTEX_POINT('',#88097);
#26480=VERTEX_POINT('',#88099);
#26481=VERTEX_POINT('',#88103);
#26482=VERTEX_POINT('',#88105);
#26483=VERTEX_POINT('',#88113);
#26484=VERTEX_POINT('',#88114);
#26485=VERTEX_POINT('',#88116);
#26486=VERTEX_POINT('',#88118);
#26487=VERTEX_POINT('',#88122);
#26488=VERTEX_POINT('',#88124);
#26489=VERTEX_POINT('',#88128);
#26490=VERTEX_POINT('',#88130);
#26491=VERTEX_POINT('',#88138);
#26492=VERTEX_POINT('',#88139);
#26493=VERTEX_POINT('',#88141);
#26494=VERTEX_POINT('',#88143);
#26495=VERTEX_POINT('',#88147);
#26496=VERTEX_POINT('',#88149);
#26497=VERTEX_POINT('',#88153);
#26498=VERTEX_POINT('',#88155);
#26499=VERTEX_POINT('',#88163);
#26500=VERTEX_POINT('',#88164);
#26501=VERTEX_POINT('',#88166);
#26502=VERTEX_POINT('',#88168);
#26503=VERTEX_POINT('',#88172);
#26504=VERTEX_POINT('',#88174);
#26505=VERTEX_POINT('',#88178);
#26506=VERTEX_POINT('',#88180);
#26507=VERTEX_POINT('',#88188);
#26508=VERTEX_POINT('',#88189);
#26509=VERTEX_POINT('',#88191);
#26510=VERTEX_POINT('',#88193);
#26511=VERTEX_POINT('',#88197);
#26512=VERTEX_POINT('',#88199);
#26513=VERTEX_POINT('',#88203);
#26514=VERTEX_POINT('',#88205);
#26515=VERTEX_POINT('',#88213);
#26516=VERTEX_POINT('',#88214);
#26517=VERTEX_POINT('',#88216);
#26518=VERTEX_POINT('',#88218);
#26519=VERTEX_POINT('',#88222);
#26520=VERTEX_POINT('',#88224);
#26521=VERTEX_POINT('',#88228);
#26522=VERTEX_POINT('',#88230);
#26523=VERTEX_POINT('',#88238);
#26524=VERTEX_POINT('',#88239);
#26525=VERTEX_POINT('',#88241);
#26526=VERTEX_POINT('',#88243);
#26527=VERTEX_POINT('',#88247);
#26528=VERTEX_POINT('',#88249);
#26529=VERTEX_POINT('',#88253);
#26530=VERTEX_POINT('',#88255);
#26531=VERTEX_POINT('',#88263);
#26532=VERTEX_POINT('',#88264);
#26533=VERTEX_POINT('',#88266);
#26534=VERTEX_POINT('',#88268);
#26535=VERTEX_POINT('',#88272);
#26536=VERTEX_POINT('',#88274);
#26537=VERTEX_POINT('',#88278);
#26538=VERTEX_POINT('',#88280);
#26539=VERTEX_POINT('',#88288);
#26540=VERTEX_POINT('',#88289);
#26541=VERTEX_POINT('',#88291);
#26542=VERTEX_POINT('',#88293);
#26543=VERTEX_POINT('',#88297);
#26544=VERTEX_POINT('',#88299);
#26545=VERTEX_POINT('',#88303);
#26546=VERTEX_POINT('',#88305);
#26547=VERTEX_POINT('',#88313);
#26548=VERTEX_POINT('',#88314);
#26549=VERTEX_POINT('',#88316);
#26550=VERTEX_POINT('',#88318);
#26551=VERTEX_POINT('',#88322);
#26552=VERTEX_POINT('',#88324);
#26553=VERTEX_POINT('',#88328);
#26554=VERTEX_POINT('',#88330);
#26555=VERTEX_POINT('',#88338);
#26556=VERTEX_POINT('',#88339);
#26557=VERTEX_POINT('',#88341);
#26558=VERTEX_POINT('',#88343);
#26559=VERTEX_POINT('',#88347);
#26560=VERTEX_POINT('',#88349);
#26561=VERTEX_POINT('',#88353);
#26562=VERTEX_POINT('',#88355);
#26563=VERTEX_POINT('',#88363);
#26564=VERTEX_POINT('',#88364);
#26565=VERTEX_POINT('',#88366);
#26566=VERTEX_POINT('',#88368);
#26567=VERTEX_POINT('',#88372);
#26568=VERTEX_POINT('',#88374);
#26569=VERTEX_POINT('',#88378);
#26570=VERTEX_POINT('',#88380);
#26571=VERTEX_POINT('',#88388);
#26572=VERTEX_POINT('',#88389);
#26573=VERTEX_POINT('',#88391);
#26574=VERTEX_POINT('',#88393);
#26575=VERTEX_POINT('',#88397);
#26576=VERTEX_POINT('',#88399);
#26577=VERTEX_POINT('',#88403);
#26578=VERTEX_POINT('',#88405);
#26579=VERTEX_POINT('',#88413);
#26580=VERTEX_POINT('',#88414);
#26581=VERTEX_POINT('',#88416);
#26582=VERTEX_POINT('',#88418);
#26583=VERTEX_POINT('',#88422);
#26584=VERTEX_POINT('',#88424);
#26585=VERTEX_POINT('',#88428);
#26586=VERTEX_POINT('',#88430);
#26587=VERTEX_POINT('',#88438);
#26588=VERTEX_POINT('',#88439);
#26589=VERTEX_POINT('',#88441);
#26590=VERTEX_POINT('',#88443);
#26591=VERTEX_POINT('',#88447);
#26592=VERTEX_POINT('',#88449);
#26593=VERTEX_POINT('',#88453);
#26594=VERTEX_POINT('',#88455);
#26595=VERTEX_POINT('',#88463);
#26596=VERTEX_POINT('',#88464);
#26597=VERTEX_POINT('',#88466);
#26598=VERTEX_POINT('',#88468);
#26599=VERTEX_POINT('',#88472);
#26600=VERTEX_POINT('',#88474);
#26601=VERTEX_POINT('',#88478);
#26602=VERTEX_POINT('',#88480);
#26603=VERTEX_POINT('',#88488);
#26604=VERTEX_POINT('',#88489);
#26605=VERTEX_POINT('',#88491);
#26606=VERTEX_POINT('',#88493);
#26607=VERTEX_POINT('',#88497);
#26608=VERTEX_POINT('',#88499);
#26609=VERTEX_POINT('',#88503);
#26610=VERTEX_POINT('',#88505);
#26611=VERTEX_POINT('',#88513);
#26612=VERTEX_POINT('',#88514);
#26613=VERTEX_POINT('',#88516);
#26614=VERTEX_POINT('',#88518);
#26615=VERTEX_POINT('',#88522);
#26616=VERTEX_POINT('',#88524);
#26617=VERTEX_POINT('',#88528);
#26618=VERTEX_POINT('',#88530);
#26619=VERTEX_POINT('',#88538);
#26620=VERTEX_POINT('',#88539);
#26621=VERTEX_POINT('',#88541);
#26622=VERTEX_POINT('',#88543);
#26623=VERTEX_POINT('',#88547);
#26624=VERTEX_POINT('',#88549);
#26625=VERTEX_POINT('',#88553);
#26626=VERTEX_POINT('',#88555);
#26627=VERTEX_POINT('',#88563);
#26628=VERTEX_POINT('',#88564);
#26629=VERTEX_POINT('',#88566);
#26630=VERTEX_POINT('',#88568);
#26631=VERTEX_POINT('',#88572);
#26632=VERTEX_POINT('',#88574);
#26633=VERTEX_POINT('',#88578);
#26634=VERTEX_POINT('',#88580);
#26635=VERTEX_POINT('',#88588);
#26636=VERTEX_POINT('',#88589);
#26637=VERTEX_POINT('',#88591);
#26638=VERTEX_POINT('',#88593);
#26639=VERTEX_POINT('',#88597);
#26640=VERTEX_POINT('',#88599);
#26641=VERTEX_POINT('',#88603);
#26642=VERTEX_POINT('',#88605);
#26643=VERTEX_POINT('',#88613);
#26644=VERTEX_POINT('',#88614);
#26645=VERTEX_POINT('',#88616);
#26646=VERTEX_POINT('',#88618);
#26647=VERTEX_POINT('',#88622);
#26648=VERTEX_POINT('',#88624);
#26649=VERTEX_POINT('',#88628);
#26650=VERTEX_POINT('',#88630);
#26651=VERTEX_POINT('',#88638);
#26652=VERTEX_POINT('',#88639);
#26653=VERTEX_POINT('',#88641);
#26654=VERTEX_POINT('',#88643);
#26655=VERTEX_POINT('',#88647);
#26656=VERTEX_POINT('',#88649);
#26657=VERTEX_POINT('',#88653);
#26658=VERTEX_POINT('',#88655);
#26659=VERTEX_POINT('',#88663);
#26660=VERTEX_POINT('',#88664);
#26661=VERTEX_POINT('',#88666);
#26662=VERTEX_POINT('',#88668);
#26663=VERTEX_POINT('',#88672);
#26664=VERTEX_POINT('',#88674);
#26665=VERTEX_POINT('',#88678);
#26666=VERTEX_POINT('',#88680);
#26667=VERTEX_POINT('',#88688);
#26668=VERTEX_POINT('',#88689);
#26669=VERTEX_POINT('',#88691);
#26670=VERTEX_POINT('',#88693);
#26671=VERTEX_POINT('',#88697);
#26672=VERTEX_POINT('',#88699);
#26673=VERTEX_POINT('',#88703);
#26674=VERTEX_POINT('',#88705);
#26675=VERTEX_POINT('',#88713);
#26676=VERTEX_POINT('',#88714);
#26677=VERTEX_POINT('',#88716);
#26678=VERTEX_POINT('',#88718);
#26679=VERTEX_POINT('',#88722);
#26680=VERTEX_POINT('',#88724);
#26681=VERTEX_POINT('',#88728);
#26682=VERTEX_POINT('',#88730);
#26683=VERTEX_POINT('',#88738);
#26684=VERTEX_POINT('',#88739);
#26685=VERTEX_POINT('',#88741);
#26686=VERTEX_POINT('',#88743);
#26687=VERTEX_POINT('',#88747);
#26688=VERTEX_POINT('',#88749);
#26689=VERTEX_POINT('',#88753);
#26690=VERTEX_POINT('',#88755);
#26691=VERTEX_POINT('',#88763);
#26692=VERTEX_POINT('',#88764);
#26693=VERTEX_POINT('',#88766);
#26694=VERTEX_POINT('',#88768);
#26695=VERTEX_POINT('',#88772);
#26696=VERTEX_POINT('',#88774);
#26697=VERTEX_POINT('',#88778);
#26698=VERTEX_POINT('',#88780);
#26699=VERTEX_POINT('',#88788);
#26700=VERTEX_POINT('',#88789);
#26701=VERTEX_POINT('',#88791);
#26702=VERTEX_POINT('',#88793);
#26703=VERTEX_POINT('',#88797);
#26704=VERTEX_POINT('',#88799);
#26705=VERTEX_POINT('',#88803);
#26706=VERTEX_POINT('',#88805);
#26707=VERTEX_POINT('',#88813);
#26708=VERTEX_POINT('',#88814);
#26709=VERTEX_POINT('',#88816);
#26710=VERTEX_POINT('',#88818);
#26711=VERTEX_POINT('',#88822);
#26712=VERTEX_POINT('',#88824);
#26713=VERTEX_POINT('',#88828);
#26714=VERTEX_POINT('',#88830);
#26715=VERTEX_POINT('',#88838);
#26716=VERTEX_POINT('',#88839);
#26717=VERTEX_POINT('',#88841);
#26718=VERTEX_POINT('',#88843);
#26719=VERTEX_POINT('',#88847);
#26720=VERTEX_POINT('',#88849);
#26721=VERTEX_POINT('',#88853);
#26722=VERTEX_POINT('',#88855);
#26723=VERTEX_POINT('',#88863);
#26724=VERTEX_POINT('',#88864);
#26725=VERTEX_POINT('',#88866);
#26726=VERTEX_POINT('',#88868);
#26727=VERTEX_POINT('',#88872);
#26728=VERTEX_POINT('',#88874);
#26729=VERTEX_POINT('',#88878);
#26730=VERTEX_POINT('',#88880);
#26731=VERTEX_POINT('',#88888);
#26732=VERTEX_POINT('',#88889);
#26733=VERTEX_POINT('',#88891);
#26734=VERTEX_POINT('',#88893);
#26735=VERTEX_POINT('',#88897);
#26736=VERTEX_POINT('',#88899);
#26737=VERTEX_POINT('',#88903);
#26738=VERTEX_POINT('',#88905);
#26739=VERTEX_POINT('',#88913);
#26740=VERTEX_POINT('',#88914);
#26741=VERTEX_POINT('',#88916);
#26742=VERTEX_POINT('',#88918);
#26743=VERTEX_POINT('',#88922);
#26744=VERTEX_POINT('',#88924);
#26745=VERTEX_POINT('',#88928);
#26746=VERTEX_POINT('',#88930);
#26747=VERTEX_POINT('',#88938);
#26748=VERTEX_POINT('',#88939);
#26749=VERTEX_POINT('',#88941);
#26750=VERTEX_POINT('',#88943);
#26751=VERTEX_POINT('',#88947);
#26752=VERTEX_POINT('',#88949);
#26753=VERTEX_POINT('',#88953);
#26754=VERTEX_POINT('',#88955);
#26755=VERTEX_POINT('',#88963);
#26756=VERTEX_POINT('',#88964);
#26757=VERTEX_POINT('',#88966);
#26758=VERTEX_POINT('',#88968);
#26759=VERTEX_POINT('',#88972);
#26760=VERTEX_POINT('',#88974);
#26761=VERTEX_POINT('',#88978);
#26762=VERTEX_POINT('',#88980);
#26763=VERTEX_POINT('',#88988);
#26764=VERTEX_POINT('',#88989);
#26765=VERTEX_POINT('',#88991);
#26766=VERTEX_POINT('',#88993);
#26767=VERTEX_POINT('',#88997);
#26768=VERTEX_POINT('',#88999);
#26769=VERTEX_POINT('',#89003);
#26770=VERTEX_POINT('',#89005);
#26771=VERTEX_POINT('',#89013);
#26772=VERTEX_POINT('',#89014);
#26773=VERTEX_POINT('',#89016);
#26774=VERTEX_POINT('',#89018);
#26775=VERTEX_POINT('',#89022);
#26776=VERTEX_POINT('',#89024);
#26777=VERTEX_POINT('',#89028);
#26778=VERTEX_POINT('',#89030);
#26779=VERTEX_POINT('',#89038);
#26780=VERTEX_POINT('',#89039);
#26781=VERTEX_POINT('',#89041);
#26782=VERTEX_POINT('',#89043);
#26783=VERTEX_POINT('',#89047);
#26784=VERTEX_POINT('',#89049);
#26785=VERTEX_POINT('',#89053);
#26786=VERTEX_POINT('',#89055);
#26787=VERTEX_POINT('',#89063);
#26788=VERTEX_POINT('',#89064);
#26789=VERTEX_POINT('',#89066);
#26790=VERTEX_POINT('',#89068);
#26791=VERTEX_POINT('',#89072);
#26792=VERTEX_POINT('',#89074);
#26793=VERTEX_POINT('',#89078);
#26794=VERTEX_POINT('',#89080);
#26795=VERTEX_POINT('',#89088);
#26796=VERTEX_POINT('',#89089);
#26797=VERTEX_POINT('',#89091);
#26798=VERTEX_POINT('',#89093);
#26799=VERTEX_POINT('',#89097);
#26800=VERTEX_POINT('',#89099);
#26801=VERTEX_POINT('',#89103);
#26802=VERTEX_POINT('',#89105);
#26803=VERTEX_POINT('',#89113);
#26804=VERTEX_POINT('',#89114);
#26805=VERTEX_POINT('',#89116);
#26806=VERTEX_POINT('',#89118);
#26807=VERTEX_POINT('',#89122);
#26808=VERTEX_POINT('',#89124);
#26809=VERTEX_POINT('',#89128);
#26810=VERTEX_POINT('',#89130);
#26811=VERTEX_POINT('',#89138);
#26812=VERTEX_POINT('',#89139);
#26813=VERTEX_POINT('',#89141);
#26814=VERTEX_POINT('',#89143);
#26815=VERTEX_POINT('',#89147);
#26816=VERTEX_POINT('',#89149);
#26817=VERTEX_POINT('',#89153);
#26818=VERTEX_POINT('',#89155);
#26819=VERTEX_POINT('',#89163);
#26820=VERTEX_POINT('',#89164);
#26821=VERTEX_POINT('',#89166);
#26822=VERTEX_POINT('',#89168);
#26823=VERTEX_POINT('',#89172);
#26824=VERTEX_POINT('',#89174);
#26825=VERTEX_POINT('',#89178);
#26826=VERTEX_POINT('',#89180);
#26827=VERTEX_POINT('',#89188);
#26828=VERTEX_POINT('',#89189);
#26829=VERTEX_POINT('',#89191);
#26830=VERTEX_POINT('',#89193);
#26831=VERTEX_POINT('',#89197);
#26832=VERTEX_POINT('',#89199);
#26833=VERTEX_POINT('',#89203);
#26834=VERTEX_POINT('',#89205);
#26835=VERTEX_POINT('',#89213);
#26836=VERTEX_POINT('',#89214);
#26837=VERTEX_POINT('',#89216);
#26838=VERTEX_POINT('',#89218);
#26839=VERTEX_POINT('',#89222);
#26840=VERTEX_POINT('',#89224);
#26841=VERTEX_POINT('',#89228);
#26842=VERTEX_POINT('',#89230);
#26843=VERTEX_POINT('',#89238);
#26844=VERTEX_POINT('',#89239);
#26845=VERTEX_POINT('',#89241);
#26846=VERTEX_POINT('',#89243);
#26847=VERTEX_POINT('',#89247);
#26848=VERTEX_POINT('',#89249);
#26849=VERTEX_POINT('',#89253);
#26850=VERTEX_POINT('',#89255);
#26851=VERTEX_POINT('',#89263);
#26852=VERTEX_POINT('',#89264);
#26853=VERTEX_POINT('',#89266);
#26854=VERTEX_POINT('',#89268);
#26855=VERTEX_POINT('',#89272);
#26856=VERTEX_POINT('',#89274);
#26857=VERTEX_POINT('',#89278);
#26858=VERTEX_POINT('',#89280);
#26859=VERTEX_POINT('',#89288);
#26860=VERTEX_POINT('',#89289);
#26861=VERTEX_POINT('',#89291);
#26862=VERTEX_POINT('',#89293);
#26863=VERTEX_POINT('',#89297);
#26864=VERTEX_POINT('',#89299);
#26865=VERTEX_POINT('',#89303);
#26866=VERTEX_POINT('',#89305);
#26867=VERTEX_POINT('',#89313);
#26868=VERTEX_POINT('',#89314);
#26869=VERTEX_POINT('',#89316);
#26870=VERTEX_POINT('',#89318);
#26871=VERTEX_POINT('',#89322);
#26872=VERTEX_POINT('',#89324);
#26873=VERTEX_POINT('',#89328);
#26874=VERTEX_POINT('',#89330);
#26875=VERTEX_POINT('',#89338);
#26876=VERTEX_POINT('',#89339);
#26877=VERTEX_POINT('',#89341);
#26878=VERTEX_POINT('',#89343);
#26879=VERTEX_POINT('',#89347);
#26880=VERTEX_POINT('',#89349);
#26881=VERTEX_POINT('',#89353);
#26882=VERTEX_POINT('',#89355);
#26883=VERTEX_POINT('',#89363);
#26884=VERTEX_POINT('',#89364);
#26885=VERTEX_POINT('',#89366);
#26886=VERTEX_POINT('',#89368);
#26887=VERTEX_POINT('',#89372);
#26888=VERTEX_POINT('',#89374);
#26889=VERTEX_POINT('',#89378);
#26890=VERTEX_POINT('',#89380);
#26891=VERTEX_POINT('',#89388);
#26892=VERTEX_POINT('',#89389);
#26893=VERTEX_POINT('',#89391);
#26894=VERTEX_POINT('',#89393);
#26895=VERTEX_POINT('',#89397);
#26896=VERTEX_POINT('',#89399);
#26897=VERTEX_POINT('',#89403);
#26898=VERTEX_POINT('',#89405);
#26899=VERTEX_POINT('',#89413);
#26900=VERTEX_POINT('',#89414);
#26901=VERTEX_POINT('',#89416);
#26902=VERTEX_POINT('',#89418);
#26903=VERTEX_POINT('',#89422);
#26904=VERTEX_POINT('',#89424);
#26905=VERTEX_POINT('',#89428);
#26906=VERTEX_POINT('',#89430);
#26907=VERTEX_POINT('',#89438);
#26908=VERTEX_POINT('',#89439);
#26909=VERTEX_POINT('',#89441);
#26910=VERTEX_POINT('',#89443);
#26911=VERTEX_POINT('',#89447);
#26912=VERTEX_POINT('',#89449);
#26913=VERTEX_POINT('',#89453);
#26914=VERTEX_POINT('',#89455);
#26915=VERTEX_POINT('',#89463);
#26916=VERTEX_POINT('',#89464);
#26917=VERTEX_POINT('',#89466);
#26918=VERTEX_POINT('',#89468);
#26919=VERTEX_POINT('',#89472);
#26920=VERTEX_POINT('',#89474);
#26921=VERTEX_POINT('',#89478);
#26922=VERTEX_POINT('',#89480);
#26923=VERTEX_POINT('',#89488);
#26924=VERTEX_POINT('',#89489);
#26925=VERTEX_POINT('',#89491);
#26926=VERTEX_POINT('',#89493);
#26927=VERTEX_POINT('',#89497);
#26928=VERTEX_POINT('',#89499);
#26929=VERTEX_POINT('',#89503);
#26930=VERTEX_POINT('',#89505);
#26931=VERTEX_POINT('',#89513);
#26932=VERTEX_POINT('',#89514);
#26933=VERTEX_POINT('',#89516);
#26934=VERTEX_POINT('',#89518);
#26935=VERTEX_POINT('',#89522);
#26936=VERTEX_POINT('',#89524);
#26937=VERTEX_POINT('',#89528);
#26938=VERTEX_POINT('',#89530);
#26939=VERTEX_POINT('',#89538);
#26940=VERTEX_POINT('',#89539);
#26941=VERTEX_POINT('',#89541);
#26942=VERTEX_POINT('',#89543);
#26943=VERTEX_POINT('',#89547);
#26944=VERTEX_POINT('',#89549);
#26945=VERTEX_POINT('',#89553);
#26946=VERTEX_POINT('',#89555);
#26947=VERTEX_POINT('',#89563);
#26948=VERTEX_POINT('',#89564);
#26949=VERTEX_POINT('',#89566);
#26950=VERTEX_POINT('',#89568);
#26951=VERTEX_POINT('',#89572);
#26952=VERTEX_POINT('',#89574);
#26953=VERTEX_POINT('',#89578);
#26954=VERTEX_POINT('',#89580);
#26955=VERTEX_POINT('',#89588);
#26956=VERTEX_POINT('',#89589);
#26957=VERTEX_POINT('',#89591);
#26958=VERTEX_POINT('',#89593);
#26959=VERTEX_POINT('',#89597);
#26960=VERTEX_POINT('',#89599);
#26961=VERTEX_POINT('',#89603);
#26962=VERTEX_POINT('',#89605);
#26963=VERTEX_POINT('',#89613);
#26964=VERTEX_POINT('',#89614);
#26965=VERTEX_POINT('',#89616);
#26966=VERTEX_POINT('',#89618);
#26967=VERTEX_POINT('',#89622);
#26968=VERTEX_POINT('',#89624);
#26969=VERTEX_POINT('',#89628);
#26970=VERTEX_POINT('',#89630);
#26971=VERTEX_POINT('',#89638);
#26972=VERTEX_POINT('',#89639);
#26973=VERTEX_POINT('',#89641);
#26974=VERTEX_POINT('',#89643);
#26975=VERTEX_POINT('',#89647);
#26976=VERTEX_POINT('',#89649);
#26977=VERTEX_POINT('',#89653);
#26978=VERTEX_POINT('',#89655);
#26979=VERTEX_POINT('',#89663);
#26980=VERTEX_POINT('',#89664);
#26981=VERTEX_POINT('',#89666);
#26982=VERTEX_POINT('',#89668);
#26983=VERTEX_POINT('',#89672);
#26984=VERTEX_POINT('',#89674);
#26985=VERTEX_POINT('',#89678);
#26986=VERTEX_POINT('',#89680);
#26987=VERTEX_POINT('',#89688);
#26988=VERTEX_POINT('',#89689);
#26989=VERTEX_POINT('',#89691);
#26990=VERTEX_POINT('',#89693);
#26991=VERTEX_POINT('',#89697);
#26992=VERTEX_POINT('',#89699);
#26993=VERTEX_POINT('',#89703);
#26994=VERTEX_POINT('',#89705);
#26995=VERTEX_POINT('',#89713);
#26996=VERTEX_POINT('',#89714);
#26997=VERTEX_POINT('',#89716);
#26998=VERTEX_POINT('',#89718);
#26999=VERTEX_POINT('',#89722);
#27000=VERTEX_POINT('',#89724);
#27001=VERTEX_POINT('',#89728);
#27002=VERTEX_POINT('',#89730);
#27003=VERTEX_POINT('',#89738);
#27004=VERTEX_POINT('',#89739);
#27005=VERTEX_POINT('',#89741);
#27006=VERTEX_POINT('',#89743);
#27007=VERTEX_POINT('',#89747);
#27008=VERTEX_POINT('',#89749);
#27009=VERTEX_POINT('',#89753);
#27010=VERTEX_POINT('',#89755);
#27011=VERTEX_POINT('',#89763);
#27012=VERTEX_POINT('',#89764);
#27013=VERTEX_POINT('',#89766);
#27014=VERTEX_POINT('',#89768);
#27015=VERTEX_POINT('',#89772);
#27016=VERTEX_POINT('',#89774);
#27017=VERTEX_POINT('',#89778);
#27018=VERTEX_POINT('',#89780);
#27019=VERTEX_POINT('',#89788);
#27020=VERTEX_POINT('',#89789);
#27021=VERTEX_POINT('',#89791);
#27022=VERTEX_POINT('',#89793);
#27023=VERTEX_POINT('',#89797);
#27024=VERTEX_POINT('',#89799);
#27025=VERTEX_POINT('',#89803);
#27026=VERTEX_POINT('',#89805);
#27027=VERTEX_POINT('',#89813);
#27028=VERTEX_POINT('',#89814);
#27029=VERTEX_POINT('',#89816);
#27030=VERTEX_POINT('',#89818);
#27031=VERTEX_POINT('',#89822);
#27032=VERTEX_POINT('',#89824);
#27033=VERTEX_POINT('',#89828);
#27034=VERTEX_POINT('',#89830);
#27035=VERTEX_POINT('',#89838);
#27036=VERTEX_POINT('',#89839);
#27037=VERTEX_POINT('',#89841);
#27038=VERTEX_POINT('',#89843);
#27039=VERTEX_POINT('',#89847);
#27040=VERTEX_POINT('',#89849);
#27041=VERTEX_POINT('',#89853);
#27042=VERTEX_POINT('',#89855);
#27043=VERTEX_POINT('',#89863);
#27044=VERTEX_POINT('',#89864);
#27045=VERTEX_POINT('',#89866);
#27046=VERTEX_POINT('',#89868);
#27047=VERTEX_POINT('',#89872);
#27048=VERTEX_POINT('',#89874);
#27049=VERTEX_POINT('',#89878);
#27050=VERTEX_POINT('',#89880);
#27051=VERTEX_POINT('',#89888);
#27052=VERTEX_POINT('',#89889);
#27053=VERTEX_POINT('',#89891);
#27054=VERTEX_POINT('',#89893);
#27055=VERTEX_POINT('',#89897);
#27056=VERTEX_POINT('',#89899);
#27057=VERTEX_POINT('',#89903);
#27058=VERTEX_POINT('',#89905);
#27059=VERTEX_POINT('',#89913);
#27060=VERTEX_POINT('',#89914);
#27061=VERTEX_POINT('',#89916);
#27062=VERTEX_POINT('',#89918);
#27063=VERTEX_POINT('',#89922);
#27064=VERTEX_POINT('',#89924);
#27065=VERTEX_POINT('',#89928);
#27066=VERTEX_POINT('',#89930);
#27067=VERTEX_POINT('',#89938);
#27068=VERTEX_POINT('',#89939);
#27069=VERTEX_POINT('',#89941);
#27070=VERTEX_POINT('',#89943);
#27071=VERTEX_POINT('',#89947);
#27072=VERTEX_POINT('',#89949);
#27073=VERTEX_POINT('',#89953);
#27074=VERTEX_POINT('',#89955);
#27075=VERTEX_POINT('',#89963);
#27076=VERTEX_POINT('',#89964);
#27077=VERTEX_POINT('',#89966);
#27078=VERTEX_POINT('',#89968);
#27079=VERTEX_POINT('',#89972);
#27080=VERTEX_POINT('',#89974);
#27081=VERTEX_POINT('',#89978);
#27082=VERTEX_POINT('',#89980);
#27083=VERTEX_POINT('',#89988);
#27084=VERTEX_POINT('',#89989);
#27085=VERTEX_POINT('',#89991);
#27086=VERTEX_POINT('',#89993);
#27087=VERTEX_POINT('',#89997);
#27088=VERTEX_POINT('',#89999);
#27089=VERTEX_POINT('',#90003);
#27090=VERTEX_POINT('',#90005);
#27091=VERTEX_POINT('',#90013);
#27092=VERTEX_POINT('',#90014);
#27093=VERTEX_POINT('',#90016);
#27094=VERTEX_POINT('',#90018);
#27095=VERTEX_POINT('',#90022);
#27096=VERTEX_POINT('',#90024);
#27097=VERTEX_POINT('',#90028);
#27098=VERTEX_POINT('',#90030);
#27099=VERTEX_POINT('',#90038);
#27100=VERTEX_POINT('',#90039);
#27101=VERTEX_POINT('',#90041);
#27102=VERTEX_POINT('',#90043);
#27103=VERTEX_POINT('',#90047);
#27104=VERTEX_POINT('',#90049);
#27105=VERTEX_POINT('',#90053);
#27106=VERTEX_POINT('',#90055);
#27107=VERTEX_POINT('',#90063);
#27108=VERTEX_POINT('',#90064);
#27109=VERTEX_POINT('',#90066);
#27110=VERTEX_POINT('',#90068);
#27111=VERTEX_POINT('',#90072);
#27112=VERTEX_POINT('',#90074);
#27113=VERTEX_POINT('',#90078);
#27114=VERTEX_POINT('',#90080);
#27115=VERTEX_POINT('',#90088);
#27116=VERTEX_POINT('',#90089);
#27117=VERTEX_POINT('',#90091);
#27118=VERTEX_POINT('',#90093);
#27119=VERTEX_POINT('',#90097);
#27120=VERTEX_POINT('',#90099);
#27121=VERTEX_POINT('',#90103);
#27122=VERTEX_POINT('',#90105);
#27123=VERTEX_POINT('',#90113);
#27124=VERTEX_POINT('',#90114);
#27125=VERTEX_POINT('',#90116);
#27126=VERTEX_POINT('',#90118);
#27127=VERTEX_POINT('',#90122);
#27128=VERTEX_POINT('',#90124);
#27129=VERTEX_POINT('',#90128);
#27130=VERTEX_POINT('',#90130);
#27131=VERTEX_POINT('',#90138);
#27132=VERTEX_POINT('',#90139);
#27133=VERTEX_POINT('',#90141);
#27134=VERTEX_POINT('',#90143);
#27135=VERTEX_POINT('',#90147);
#27136=VERTEX_POINT('',#90149);
#27137=VERTEX_POINT('',#90153);
#27138=VERTEX_POINT('',#90155);
#27139=VERTEX_POINT('',#90163);
#27140=VERTEX_POINT('',#90164);
#27141=VERTEX_POINT('',#90166);
#27142=VERTEX_POINT('',#90168);
#27143=VERTEX_POINT('',#90172);
#27144=VERTEX_POINT('',#90174);
#27145=VERTEX_POINT('',#90178);
#27146=VERTEX_POINT('',#90180);
#27147=VERTEX_POINT('',#90188);
#27148=VERTEX_POINT('',#90189);
#27149=VERTEX_POINT('',#90191);
#27150=VERTEX_POINT('',#90193);
#27151=VERTEX_POINT('',#90197);
#27152=VERTEX_POINT('',#90199);
#27153=VERTEX_POINT('',#90203);
#27154=VERTEX_POINT('',#90205);
#27155=VERTEX_POINT('',#90213);
#27156=VERTEX_POINT('',#90214);
#27157=VERTEX_POINT('',#90216);
#27158=VERTEX_POINT('',#90218);
#27159=VERTEX_POINT('',#90222);
#27160=VERTEX_POINT('',#90224);
#27161=VERTEX_POINT('',#90228);
#27162=VERTEX_POINT('',#90230);
#27163=VERTEX_POINT('',#90238);
#27164=VERTEX_POINT('',#90239);
#27165=VERTEX_POINT('',#90241);
#27166=VERTEX_POINT('',#90243);
#27167=VERTEX_POINT('',#90247);
#27168=VERTEX_POINT('',#90249);
#27169=VERTEX_POINT('',#90253);
#27170=VERTEX_POINT('',#90255);
#27171=VERTEX_POINT('',#90263);
#27172=VERTEX_POINT('',#90264);
#27173=VERTEX_POINT('',#90266);
#27174=VERTEX_POINT('',#90268);
#27175=VERTEX_POINT('',#90272);
#27176=VERTEX_POINT('',#90274);
#27177=VERTEX_POINT('',#90278);
#27178=VERTEX_POINT('',#90280);
#27179=VERTEX_POINT('',#90288);
#27180=VERTEX_POINT('',#90289);
#27181=VERTEX_POINT('',#90291);
#27182=VERTEX_POINT('',#90293);
#27183=VERTEX_POINT('',#90297);
#27184=VERTEX_POINT('',#90299);
#27185=VERTEX_POINT('',#90303);
#27186=VERTEX_POINT('',#90305);
#27187=VERTEX_POINT('',#90313);
#27188=VERTEX_POINT('',#90314);
#27189=VERTEX_POINT('',#90316);
#27190=VERTEX_POINT('',#90318);
#27191=VERTEX_POINT('',#90322);
#27192=VERTEX_POINT('',#90324);
#27193=VERTEX_POINT('',#90328);
#27194=VERTEX_POINT('',#90330);
#27195=VERTEX_POINT('',#90338);
#27196=VERTEX_POINT('',#90339);
#27197=VERTEX_POINT('',#90341);
#27198=VERTEX_POINT('',#90343);
#27199=VERTEX_POINT('',#90347);
#27200=VERTEX_POINT('',#90349);
#27201=VERTEX_POINT('',#90353);
#27202=VERTEX_POINT('',#90355);
#27203=VERTEX_POINT('',#90363);
#27204=VERTEX_POINT('',#90364);
#27205=VERTEX_POINT('',#90366);
#27206=VERTEX_POINT('',#90368);
#27207=VERTEX_POINT('',#90372);
#27208=VERTEX_POINT('',#90374);
#27209=VERTEX_POINT('',#90378);
#27210=VERTEX_POINT('',#90380);
#27211=VERTEX_POINT('',#90388);
#27212=VERTEX_POINT('',#90389);
#27213=VERTEX_POINT('',#90391);
#27214=VERTEX_POINT('',#90393);
#27215=VERTEX_POINT('',#90397);
#27216=VERTEX_POINT('',#90399);
#27217=VERTEX_POINT('',#90403);
#27218=VERTEX_POINT('',#90405);
#27219=VERTEX_POINT('',#90413);
#27220=VERTEX_POINT('',#90414);
#27221=VERTEX_POINT('',#90416);
#27222=VERTEX_POINT('',#90418);
#27223=VERTEX_POINT('',#90422);
#27224=VERTEX_POINT('',#90424);
#27225=VERTEX_POINT('',#90428);
#27226=VERTEX_POINT('',#90430);
#27227=VERTEX_POINT('',#90438);
#27228=VERTEX_POINT('',#90439);
#27229=VERTEX_POINT('',#90441);
#27230=VERTEX_POINT('',#90443);
#27231=VERTEX_POINT('',#90447);
#27232=VERTEX_POINT('',#90449);
#27233=VERTEX_POINT('',#90453);
#27234=VERTEX_POINT('',#90455);
#27235=VERTEX_POINT('',#90463);
#27236=VERTEX_POINT('',#90464);
#27237=VERTEX_POINT('',#90466);
#27238=VERTEX_POINT('',#90468);
#27239=VERTEX_POINT('',#90472);
#27240=VERTEX_POINT('',#90474);
#27241=VERTEX_POINT('',#90478);
#27242=VERTEX_POINT('',#90480);
#27243=VERTEX_POINT('',#90488);
#27244=VERTEX_POINT('',#90489);
#27245=VERTEX_POINT('',#90491);
#27246=VERTEX_POINT('',#90493);
#27247=VERTEX_POINT('',#90497);
#27248=VERTEX_POINT('',#90499);
#27249=VERTEX_POINT('',#90503);
#27250=VERTEX_POINT('',#90505);
#27251=VERTEX_POINT('',#90513);
#27252=VERTEX_POINT('',#90514);
#27253=VERTEX_POINT('',#90516);
#27254=VERTEX_POINT('',#90518);
#27255=VERTEX_POINT('',#90522);
#27256=VERTEX_POINT('',#90524);
#27257=VERTEX_POINT('',#90528);
#27258=VERTEX_POINT('',#90530);
#27259=VERTEX_POINT('',#90538);
#27260=VERTEX_POINT('',#90539);
#27261=VERTEX_POINT('',#90541);
#27262=VERTEX_POINT('',#90543);
#27263=VERTEX_POINT('',#90547);
#27264=VERTEX_POINT('',#90549);
#27265=VERTEX_POINT('',#90553);
#27266=VERTEX_POINT('',#90555);
#27267=VERTEX_POINT('',#90563);
#27268=VERTEX_POINT('',#90564);
#27269=VERTEX_POINT('',#90566);
#27270=VERTEX_POINT('',#90568);
#27271=VERTEX_POINT('',#90572);
#27272=VERTEX_POINT('',#90574);
#27273=VERTEX_POINT('',#90578);
#27274=VERTEX_POINT('',#90580);
#27275=VERTEX_POINT('',#90588);
#27276=VERTEX_POINT('',#90589);
#27277=VERTEX_POINT('',#90591);
#27278=VERTEX_POINT('',#90593);
#27279=VERTEX_POINT('',#90597);
#27280=VERTEX_POINT('',#90599);
#27281=VERTEX_POINT('',#90603);
#27282=VERTEX_POINT('',#90605);
#27283=VERTEX_POINT('',#90613);
#27284=VERTEX_POINT('',#90614);
#27285=VERTEX_POINT('',#90616);
#27286=VERTEX_POINT('',#90618);
#27287=VERTEX_POINT('',#90622);
#27288=VERTEX_POINT('',#90624);
#27289=VERTEX_POINT('',#90628);
#27290=VERTEX_POINT('',#90630);
#27291=VERTEX_POINT('',#90638);
#27292=VERTEX_POINT('',#90639);
#27293=VERTEX_POINT('',#90641);
#27294=VERTEX_POINT('',#90643);
#27295=VERTEX_POINT('',#90647);
#27296=VERTEX_POINT('',#90649);
#27297=VERTEX_POINT('',#90653);
#27298=VERTEX_POINT('',#90655);
#27299=VERTEX_POINT('',#90663);
#27300=VERTEX_POINT('',#90664);
#27301=VERTEX_POINT('',#90666);
#27302=VERTEX_POINT('',#90668);
#27303=VERTEX_POINT('',#90672);
#27304=VERTEX_POINT('',#90674);
#27305=VERTEX_POINT('',#90678);
#27306=VERTEX_POINT('',#90680);
#27307=VERTEX_POINT('',#90688);
#27308=VERTEX_POINT('',#90689);
#27309=VERTEX_POINT('',#90691);
#27310=VERTEX_POINT('',#90693);
#27311=VERTEX_POINT('',#90697);
#27312=VERTEX_POINT('',#90699);
#27313=VERTEX_POINT('',#90703);
#27314=VERTEX_POINT('',#90705);
#27315=VERTEX_POINT('',#90713);
#27316=VERTEX_POINT('',#90714);
#27317=VERTEX_POINT('',#90716);
#27318=VERTEX_POINT('',#90718);
#27319=VERTEX_POINT('',#90722);
#27320=VERTEX_POINT('',#90724);
#27321=VERTEX_POINT('',#90728);
#27322=VERTEX_POINT('',#90730);
#27323=VERTEX_POINT('',#90738);
#27324=VERTEX_POINT('',#90739);
#27325=VERTEX_POINT('',#90741);
#27326=VERTEX_POINT('',#90743);
#27327=VERTEX_POINT('',#90747);
#27328=VERTEX_POINT('',#90749);
#27329=VERTEX_POINT('',#90753);
#27330=VERTEX_POINT('',#90755);
#27331=VERTEX_POINT('',#90763);
#27332=VERTEX_POINT('',#90764);
#27333=VERTEX_POINT('',#90766);
#27334=VERTEX_POINT('',#90768);
#27335=VERTEX_POINT('',#90772);
#27336=VERTEX_POINT('',#90774);
#27337=VERTEX_POINT('',#90778);
#27338=VERTEX_POINT('',#90780);
#27339=VERTEX_POINT('',#90788);
#27340=VERTEX_POINT('',#90789);
#27341=VERTEX_POINT('',#90791);
#27342=VERTEX_POINT('',#90793);
#27343=VERTEX_POINT('',#90797);
#27344=VERTEX_POINT('',#90799);
#27345=VERTEX_POINT('',#90803);
#27346=VERTEX_POINT('',#90805);
#27347=VERTEX_POINT('',#90813);
#27348=VERTEX_POINT('',#90814);
#27349=VERTEX_POINT('',#90816);
#27350=VERTEX_POINT('',#90818);
#27351=VERTEX_POINT('',#90822);
#27352=VERTEX_POINT('',#90824);
#27353=VERTEX_POINT('',#90828);
#27354=VERTEX_POINT('',#90830);
#27355=VERTEX_POINT('',#90838);
#27356=VERTEX_POINT('',#90839);
#27357=VERTEX_POINT('',#90841);
#27358=VERTEX_POINT('',#90843);
#27359=VERTEX_POINT('',#90847);
#27360=VERTEX_POINT('',#90849);
#27361=VERTEX_POINT('',#90853);
#27362=VERTEX_POINT('',#90855);
#27363=VERTEX_POINT('',#90863);
#27364=VERTEX_POINT('',#90864);
#27365=VERTEX_POINT('',#90866);
#27366=VERTEX_POINT('',#90868);
#27367=VERTEX_POINT('',#90872);
#27368=VERTEX_POINT('',#90874);
#27369=VERTEX_POINT('',#90878);
#27370=VERTEX_POINT('',#90880);
#27371=VERTEX_POINT('',#90888);
#27372=VERTEX_POINT('',#90889);
#27373=VERTEX_POINT('',#90891);
#27374=VERTEX_POINT('',#90893);
#27375=VERTEX_POINT('',#90897);
#27376=VERTEX_POINT('',#90899);
#27377=VERTEX_POINT('',#90903);
#27378=VERTEX_POINT('',#90905);
#27379=VERTEX_POINT('',#90913);
#27380=VERTEX_POINT('',#90914);
#27381=VERTEX_POINT('',#90916);
#27382=VERTEX_POINT('',#90918);
#27383=VERTEX_POINT('',#90922);
#27384=VERTEX_POINT('',#90924);
#27385=VERTEX_POINT('',#90928);
#27386=VERTEX_POINT('',#90930);
#27387=VERTEX_POINT('',#90938);
#27388=VERTEX_POINT('',#90939);
#27389=VERTEX_POINT('',#90941);
#27390=VERTEX_POINT('',#90943);
#27391=VERTEX_POINT('',#90947);
#27392=VERTEX_POINT('',#90949);
#27393=VERTEX_POINT('',#90953);
#27394=VERTEX_POINT('',#90955);
#27395=VERTEX_POINT('',#90963);
#27396=VERTEX_POINT('',#90964);
#27397=VERTEX_POINT('',#90966);
#27398=VERTEX_POINT('',#90968);
#27399=VERTEX_POINT('',#90972);
#27400=VERTEX_POINT('',#90974);
#27401=VERTEX_POINT('',#90978);
#27402=VERTEX_POINT('',#90980);
#27403=VERTEX_POINT('',#90988);
#27404=VERTEX_POINT('',#90989);
#27405=VERTEX_POINT('',#90991);
#27406=VERTEX_POINT('',#90993);
#27407=VERTEX_POINT('',#90997);
#27408=VERTEX_POINT('',#90999);
#27409=VERTEX_POINT('',#91003);
#27410=VERTEX_POINT('',#91005);
#27411=VERTEX_POINT('',#91013);
#27412=VERTEX_POINT('',#91014);
#27413=VERTEX_POINT('',#91016);
#27414=VERTEX_POINT('',#91018);
#27415=VERTEX_POINT('',#91022);
#27416=VERTEX_POINT('',#91024);
#27417=VERTEX_POINT('',#91028);
#27418=VERTEX_POINT('',#91030);
#27419=VERTEX_POINT('',#91038);
#27420=VERTEX_POINT('',#91039);
#27421=VERTEX_POINT('',#91041);
#27422=VERTEX_POINT('',#91043);
#27423=VERTEX_POINT('',#91047);
#27424=VERTEX_POINT('',#91049);
#27425=VERTEX_POINT('',#91053);
#27426=VERTEX_POINT('',#91055);
#27427=VERTEX_POINT('',#91063);
#27428=VERTEX_POINT('',#91064);
#27429=VERTEX_POINT('',#91066);
#27430=VERTEX_POINT('',#91068);
#27431=VERTEX_POINT('',#91072);
#27432=VERTEX_POINT('',#91074);
#27433=VERTEX_POINT('',#91078);
#27434=VERTEX_POINT('',#91080);
#27435=VERTEX_POINT('',#91088);
#27436=VERTEX_POINT('',#91089);
#27437=VERTEX_POINT('',#91091);
#27438=VERTEX_POINT('',#91093);
#27439=VERTEX_POINT('',#91097);
#27440=VERTEX_POINT('',#91099);
#27441=VERTEX_POINT('',#91103);
#27442=VERTEX_POINT('',#91105);
#27443=VERTEX_POINT('',#91113);
#27444=VERTEX_POINT('',#91114);
#27445=VERTEX_POINT('',#91116);
#27446=VERTEX_POINT('',#91118);
#27447=VERTEX_POINT('',#91122);
#27448=VERTEX_POINT('',#91124);
#27449=VERTEX_POINT('',#91128);
#27450=VERTEX_POINT('',#91130);
#27451=VERTEX_POINT('',#91138);
#27452=VERTEX_POINT('',#91139);
#27453=VERTEX_POINT('',#91141);
#27454=VERTEX_POINT('',#91143);
#27455=VERTEX_POINT('',#91147);
#27456=VERTEX_POINT('',#91149);
#27457=VERTEX_POINT('',#91153);
#27458=VERTEX_POINT('',#91155);
#27459=VERTEX_POINT('',#91163);
#27460=VERTEX_POINT('',#91164);
#27461=VERTEX_POINT('',#91166);
#27462=VERTEX_POINT('',#91168);
#27463=VERTEX_POINT('',#91172);
#27464=VERTEX_POINT('',#91174);
#27465=VERTEX_POINT('',#91178);
#27466=VERTEX_POINT('',#91180);
#27467=VERTEX_POINT('',#91188);
#27468=VERTEX_POINT('',#91189);
#27469=VERTEX_POINT('',#91191);
#27470=VERTEX_POINT('',#91193);
#27471=VERTEX_POINT('',#91197);
#27472=VERTEX_POINT('',#91199);
#27473=VERTEX_POINT('',#91203);
#27474=VERTEX_POINT('',#91205);
#27475=VERTEX_POINT('',#91213);
#27476=VERTEX_POINT('',#91214);
#27477=VERTEX_POINT('',#91216);
#27478=VERTEX_POINT('',#91218);
#27479=VERTEX_POINT('',#91222);
#27480=VERTEX_POINT('',#91224);
#27481=VERTEX_POINT('',#91228);
#27482=VERTEX_POINT('',#91230);
#27483=VERTEX_POINT('',#91238);
#27484=VERTEX_POINT('',#91239);
#27485=VERTEX_POINT('',#91241);
#27486=VERTEX_POINT('',#91243);
#27487=VERTEX_POINT('',#91247);
#27488=VERTEX_POINT('',#91249);
#27489=VERTEX_POINT('',#91253);
#27490=VERTEX_POINT('',#91255);
#27491=VERTEX_POINT('',#91263);
#27492=VERTEX_POINT('',#91264);
#27493=VERTEX_POINT('',#91266);
#27494=VERTEX_POINT('',#91268);
#27495=VERTEX_POINT('',#91272);
#27496=VERTEX_POINT('',#91274);
#27497=VERTEX_POINT('',#91278);
#27498=VERTEX_POINT('',#91280);
#27499=VERTEX_POINT('',#91288);
#27500=VERTEX_POINT('',#91289);
#27501=VERTEX_POINT('',#91291);
#27502=VERTEX_POINT('',#91293);
#27503=VERTEX_POINT('',#91297);
#27504=VERTEX_POINT('',#91299);
#27505=VERTEX_POINT('',#91303);
#27506=VERTEX_POINT('',#91305);
#27507=VERTEX_POINT('',#91313);
#27508=VERTEX_POINT('',#91314);
#27509=VERTEX_POINT('',#91316);
#27510=VERTEX_POINT('',#91318);
#27511=VERTEX_POINT('',#91322);
#27512=VERTEX_POINT('',#91324);
#27513=VERTEX_POINT('',#91328);
#27514=VERTEX_POINT('',#91330);
#27515=VERTEX_POINT('',#91338);
#27516=VERTEX_POINT('',#91339);
#27517=VERTEX_POINT('',#91341);
#27518=VERTEX_POINT('',#91343);
#27519=VERTEX_POINT('',#91347);
#27520=VERTEX_POINT('',#91349);
#27521=VERTEX_POINT('',#91353);
#27522=VERTEX_POINT('',#91355);
#27523=VERTEX_POINT('',#91363);
#27524=VERTEX_POINT('',#91364);
#27525=VERTEX_POINT('',#91366);
#27526=VERTEX_POINT('',#91368);
#27527=VERTEX_POINT('',#91372);
#27528=VERTEX_POINT('',#91374);
#27529=VERTEX_POINT('',#91378);
#27530=VERTEX_POINT('',#91380);
#27531=VERTEX_POINT('',#91388);
#27532=VERTEX_POINT('',#91389);
#27533=VERTEX_POINT('',#91391);
#27534=VERTEX_POINT('',#91393);
#27535=VERTEX_POINT('',#91397);
#27536=VERTEX_POINT('',#91399);
#27537=VERTEX_POINT('',#91403);
#27538=VERTEX_POINT('',#91405);
#27539=VERTEX_POINT('',#91413);
#27540=VERTEX_POINT('',#91414);
#27541=VERTEX_POINT('',#91416);
#27542=VERTEX_POINT('',#91418);
#27543=VERTEX_POINT('',#91422);
#27544=VERTEX_POINT('',#91424);
#27545=VERTEX_POINT('',#91428);
#27546=VERTEX_POINT('',#91430);
#27547=VERTEX_POINT('',#91438);
#27548=VERTEX_POINT('',#91439);
#27549=VERTEX_POINT('',#91441);
#27550=VERTEX_POINT('',#91443);
#27551=VERTEX_POINT('',#91447);
#27552=VERTEX_POINT('',#91449);
#27553=VERTEX_POINT('',#91453);
#27554=VERTEX_POINT('',#91455);
#27555=VERTEX_POINT('',#91463);
#27556=VERTEX_POINT('',#91464);
#27557=VERTEX_POINT('',#91466);
#27558=VERTEX_POINT('',#91468);
#27559=VERTEX_POINT('',#91472);
#27560=VERTEX_POINT('',#91474);
#27561=VERTEX_POINT('',#91478);
#27562=VERTEX_POINT('',#91480);
#27563=VERTEX_POINT('',#91488);
#27564=VERTEX_POINT('',#91489);
#27565=VERTEX_POINT('',#91491);
#27566=VERTEX_POINT('',#91493);
#27567=VERTEX_POINT('',#91497);
#27568=VERTEX_POINT('',#91499);
#27569=VERTEX_POINT('',#91503);
#27570=VERTEX_POINT('',#91505);
#27571=VERTEX_POINT('',#91513);
#27572=VERTEX_POINT('',#91514);
#27573=VERTEX_POINT('',#91516);
#27574=VERTEX_POINT('',#91518);
#27575=VERTEX_POINT('',#91522);
#27576=VERTEX_POINT('',#91524);
#27577=VERTEX_POINT('',#91528);
#27578=VERTEX_POINT('',#91530);
#27579=VERTEX_POINT('',#91538);
#27580=VERTEX_POINT('',#91539);
#27581=VERTEX_POINT('',#91541);
#27582=VERTEX_POINT('',#91543);
#27583=VERTEX_POINT('',#91547);
#27584=VERTEX_POINT('',#91549);
#27585=VERTEX_POINT('',#91553);
#27586=VERTEX_POINT('',#91555);
#27587=VERTEX_POINT('',#91563);
#27588=VERTEX_POINT('',#91564);
#27589=VERTEX_POINT('',#91566);
#27590=VERTEX_POINT('',#91568);
#27591=VERTEX_POINT('',#91572);
#27592=VERTEX_POINT('',#91574);
#27593=VERTEX_POINT('',#91578);
#27594=VERTEX_POINT('',#91580);
#27595=VERTEX_POINT('',#91588);
#27596=VERTEX_POINT('',#91589);
#27597=VERTEX_POINT('',#91591);
#27598=VERTEX_POINT('',#91593);
#27599=VERTEX_POINT('',#91597);
#27600=VERTEX_POINT('',#91599);
#27601=VERTEX_POINT('',#91603);
#27602=VERTEX_POINT('',#91605);
#27603=VERTEX_POINT('',#91613);
#27604=VERTEX_POINT('',#91614);
#27605=VERTEX_POINT('',#91616);
#27606=VERTEX_POINT('',#91618);
#27607=VERTEX_POINT('',#91622);
#27608=VERTEX_POINT('',#91624);
#27609=VERTEX_POINT('',#91628);
#27610=VERTEX_POINT('',#91630);
#27611=VERTEX_POINT('',#91638);
#27612=VERTEX_POINT('',#91639);
#27613=VERTEX_POINT('',#91641);
#27614=VERTEX_POINT('',#91643);
#27615=VERTEX_POINT('',#91647);
#27616=VERTEX_POINT('',#91649);
#27617=VERTEX_POINT('',#91653);
#27618=VERTEX_POINT('',#91655);
#27619=VERTEX_POINT('',#91663);
#27620=VERTEX_POINT('',#91664);
#27621=VERTEX_POINT('',#91666);
#27622=VERTEX_POINT('',#91668);
#27623=VERTEX_POINT('',#91672);
#27624=VERTEX_POINT('',#91674);
#27625=VERTEX_POINT('',#91678);
#27626=VERTEX_POINT('',#91680);
#27627=VERTEX_POINT('',#91688);
#27628=VERTEX_POINT('',#91689);
#27629=VERTEX_POINT('',#91691);
#27630=VERTEX_POINT('',#91693);
#27631=VERTEX_POINT('',#91695);
#27632=VERTEX_POINT('',#91697);
#27633=VERTEX_POINT('',#91701);
#27634=VERTEX_POINT('',#91702);
#27635=VERTEX_POINT('',#91704);
#27636=VERTEX_POINT('',#91706);
#27637=VERTEX_POINT('',#91708);
#27638=VERTEX_POINT('',#91710);
#27639=VERTEX_POINT('',#91717);
#27640=VERTEX_POINT('',#91719);
#27641=VERTEX_POINT('',#91721);
#27642=VERTEX_POINT('',#91723);
#27643=VERTEX_POINT('',#91725);
#27644=VERTEX_POINT('',#91727);
#27645=VERTEX_POINT('',#91729);
#27646=VERTEX_POINT('',#91731);
#27647=VERTEX_POINT('',#91733);
#27648=VERTEX_POINT('',#91735);
#27649=VERTEX_POINT('',#91737);
#27650=VERTEX_POINT('',#91739);
#27651=VERTEX_POINT('',#91741);
#27652=VERTEX_POINT('',#91743);
#27653=VERTEX_POINT('',#91745);
#27654=VERTEX_POINT('',#91747);
#27655=VERTEX_POINT('',#91749);
#27656=VERTEX_POINT('',#91751);
#27657=VERTEX_POINT('',#91753);
#27658=VERTEX_POINT('',#91755);
#27659=VERTEX_POINT('',#91759);
#27660=VERTEX_POINT('',#91761);
#27661=VERTEX_POINT('',#91765);
#27662=VERTEX_POINT('',#91767);
#27663=VERTEX_POINT('',#91771);
#27664=VERTEX_POINT('',#91776);
#27665=VERTEX_POINT('',#91778);
#27666=VERTEX_POINT('',#91780);
#27667=VERTEX_POINT('',#91783);
#27668=VERTEX_POINT('',#91785);
#27669=VERTEX_POINT('',#91788);
#27670=VERTEX_POINT('',#91790);
#27671=VERTEX_POINT('',#91793);
#27672=VERTEX_POINT('',#91797);
#27673=VERTEX_POINT('',#91801);
#27674=VERTEX_POINT('',#91803);
#27675=VERTEX_POINT('',#91807);
#27676=VERTEX_POINT('',#91811);
#27677=VERTEX_POINT('',#91812);
#27678=VERTEX_POINT('',#91814);
#27679=VERTEX_POINT('',#91816);
#27680=VERTEX_POINT('',#91819);
#27681=VERTEX_POINT('',#91822);
#27682=VERTEX_POINT('',#91825);
#27683=VERTEX_POINT('',#91829);
#27684=VERTEX_POINT('',#91833);
#27685=VERTEX_POINT('',#91836);
#27686=VERTEX_POINT('',#91838);
#27687=VERTEX_POINT('',#91842);
#27688=VERTEX_POINT('',#91845);
#27689=VERTEX_POINT('',#91847);
#27690=VERTEX_POINT('',#91851);
#27691=VERTEX_POINT('',#91854);
#27692=VERTEX_POINT('',#91856);
#27693=VERTEX_POINT('',#91860);
#27694=VERTEX_POINT('',#91863);
#27695=VERTEX_POINT('',#91865);
#27696=VERTEX_POINT('',#91869);
#27697=VERTEX_POINT('',#91872);
#27698=VERTEX_POINT('',#91874);
#27699=VERTEX_POINT('',#91878);
#27700=VERTEX_POINT('',#91881);
#27701=VERTEX_POINT('',#91883);
#27702=VERTEX_POINT('',#91887);
#27703=VERTEX_POINT('',#91890);
#27704=VERTEX_POINT('',#91894);
#27705=VERTEX_POINT('',#91897);
#27706=VERTEX_POINT('',#91899);
#27707=VERTEX_POINT('',#91901);
#27708=VERTEX_POINT('',#91906);
#27709=VERTEX_POINT('',#91912);
#27710=VERTEX_POINT('',#91918);
#27711=VERTEX_POINT('',#91924);
#27712=VERTEX_POINT('',#91930);
#27713=VERTEX_POINT('',#91936);
#27714=VERTEX_POINT('',#91937);
#27715=VERTEX_POINT('',#91939);
#27716=VERTEX_POINT('',#91941);
#27717=VERTEX_POINT('',#91945);
#27718=VERTEX_POINT('',#91947);
#27719=VERTEX_POINT('',#91951);
#27720=VERTEX_POINT('',#91953);
#27721=VERTEX_POINT('',#91957);
#27722=VERTEX_POINT('',#91958);
#27723=VERTEX_POINT('',#91960);
#27724=VERTEX_POINT('',#91965);
#27725=VERTEX_POINT('',#91967);
#27726=VERTEX_POINT('',#91971);
#27727=VERTEX_POINT('',#91973);
#27728=VERTEX_POINT('',#91977);
#27729=VERTEX_POINT('',#91979);
#27730=VERTEX_POINT('',#91983);
#27731=VERTEX_POINT('',#91990);
#27732=VERTEX_POINT('',#91993);
#27733=VERTEX_POINT('',#91995);
#27734=VERTEX_POINT('',#91997);
#27735=VERTEX_POINT('',#92001);
#27736=VERTEX_POINT('',#92005);
#27737=VERTEX_POINT('',#92009);
#27738=VERTEX_POINT('',#92015);
#27739=VERTEX_POINT('',#92019);
#27740=VERTEX_POINT('',#92020);
#27741=VERTEX_POINT('',#92022);
#27742=VERTEX_POINT('',#92024);
#27743=VERTEX_POINT('',#92028);
#27744=VERTEX_POINT('',#92030);
#27745=VERTEX_POINT('',#92034);
#27746=VERTEX_POINT('',#92036);
#27747=VERTEX_POINT('',#92043);
#27748=VERTEX_POINT('',#92045);
#27749=VERTEX_POINT('',#92049);
#27750=VERTEX_POINT('',#92051);
#27751=VERTEX_POINT('',#92055);
#27752=VERTEX_POINT('',#92057);
#27753=VERTEX_POINT('',#92064);
#27754=VERTEX_POINT('',#92066);
#27755=VERTEX_POINT('',#92070);
#27756=VERTEX_POINT('',#92074);
#27757=VERTEX_POINT('',#92080);
#27758=VERTEX_POINT('',#92084);
#27759=VERTEX_POINT('',#92088);
#27760=VERTEX_POINT('',#92094);
#27761=VERTEX_POINT('',#92095);
#27762=VERTEX_POINT('',#92100);
#27763=VERTEX_POINT('',#92145);
#27764=VERTEX_POINT('',#92146);
#27765=VERTEX_POINT('',#92148);
#27766=VERTEX_POINT('',#92150);
#27767=VERTEX_POINT('',#92156);
#27768=VERTEX_POINT('',#92157);
#27769=VERTEX_POINT('',#92159);
#27770=VERTEX_POINT('',#92164);
#27771=VERTEX_POINT('',#92165);
#27772=VERTEX_POINT('',#92167);
#27773=VERTEX_POINT('',#92169);
#27774=VERTEX_POINT('',#92173);
#27775=VERTEX_POINT('',#92175);
#27776=VERTEX_POINT('',#92178);
#27777=VERTEX_POINT('',#92181);
#27778=VERTEX_POINT('',#92185);
#27779=VERTEX_POINT('',#92189);
#27780=VERTEX_POINT('',#92193);
#27781=VERTEX_POINT('',#92196);
#27782=VERTEX_POINT('',#92199);
#27783=VERTEX_POINT('',#92200);
#27784=VERTEX_POINT('',#92204);
#27785=VERTEX_POINT('',#92206);
#27786=VERTEX_POINT('',#92211);
#27787=VERTEX_POINT('',#92213);
#27788=VERTEX_POINT('',#92215);
#27789=VERTEX_POINT('',#92217);
#27790=VERTEX_POINT('',#92219);
#27791=VERTEX_POINT('',#92221);
#27792=VERTEX_POINT('',#92225);
#27793=VERTEX_POINT('',#92232);
#27794=VERTEX_POINT('',#92236);
#27795=VERTEX_POINT('',#92238);
#27796=VERTEX_POINT('',#92243);
#27797=VERTEX_POINT('',#92250);
#27798=VERTEX_POINT('',#92254);
#27799=VERTEX_POINT('',#92256);
#27800=VERTEX_POINT('',#92260);
#27801=VERTEX_POINT('',#92261);
#27802=VERTEX_POINT('',#92265);
#27803=VERTEX_POINT('',#92267);
#27804=VERTEX_POINT('',#92272);
#27805=VERTEX_POINT('',#92275);
#27806=VERTEX_POINT('',#92279);
#27807=VERTEX_POINT('',#92281);
#27808=VERTEX_POINT('',#92283);
#27809=VERTEX_POINT('',#92287);
#27810=VERTEX_POINT('',#92289);
#27811=VERTEX_POINT('',#92293);
#27812=VERTEX_POINT('',#92295);
#27813=VERTEX_POINT('',#92298);
#27814=VERTEX_POINT('',#92300);
#27815=VERTEX_POINT('',#92302);
#27816=VERTEX_POINT('',#92304);
#27817=VERTEX_POINT('',#92306);
#27818=VERTEX_POINT('',#92309);
#27819=VERTEX_POINT('',#92311);
#27820=VERTEX_POINT('',#92313);
#27821=VERTEX_POINT('',#92317);
#27822=VERTEX_POINT('',#92321);
#27823=VERTEX_POINT('',#92323);
#27824=VERTEX_POINT('',#92325);
#27825=VERTEX_POINT('',#92341);
#27826=VERTEX_POINT('',#92345);
#27827=VERTEX_POINT('',#92349);
#27828=VERTEX_POINT('',#92353);
#27829=VERTEX_POINT('',#92357);
#27830=VERTEX_POINT('',#92361);
#27831=VERTEX_POINT('',#92365);
#27832=VERTEX_POINT('',#92369);
#27833=VERTEX_POINT('',#92373);
#27834=VERTEX_POINT('',#92376);
#27835=VERTEX_POINT('',#92379);
#27836=VERTEX_POINT('',#92382);
#27837=VERTEX_POINT('',#92385);
#27838=VERTEX_POINT('',#92387);
#27839=VERTEX_POINT('',#92394);
#27840=VERTEX_POINT('',#92396);
#27841=VERTEX_POINT('',#92398);
#27842=VERTEX_POINT('',#92400);
#27843=VERTEX_POINT('',#92402);
#27844=VERTEX_POINT('',#92406);
#27845=VERTEX_POINT('',#92407);
#27846=VERTEX_POINT('',#92411);
#27847=VERTEX_POINT('',#92417);
#27848=VERTEX_POINT('',#92419);
#27849=VERTEX_POINT('',#92421);
#27850=VERTEX_POINT('',#92423);
#27851=VERTEX_POINT('',#92427);
#27852=VERTEX_POINT('',#92428);
#27853=VERTEX_POINT('',#92433);
#27854=VERTEX_POINT('',#92435);
#27855=VERTEX_POINT('',#92439);
#27856=VERTEX_POINT('',#92441);
#27857=VERTEX_POINT('',#92443);
#27858=VERTEX_POINT('',#92445);
#27859=VERTEX_POINT('',#92447);
#27860=VERTEX_POINT('',#92449);
#27861=VERTEX_POINT('',#92451);
#27862=VERTEX_POINT('',#92453);
#27863=VERTEX_POINT('',#92457);
#27864=VERTEX_POINT('',#92461);
#27865=VERTEX_POINT('',#92463);
#27866=VERTEX_POINT('',#92465);
#27867=VERTEX_POINT('',#92469);
#27868=VERTEX_POINT('',#92471);
#27869=VERTEX_POINT('',#92473);
#27870=VERTEX_POINT('',#92475);
#27871=VERTEX_POINT('',#92481);
#27872=VERTEX_POINT('',#92488);
#27873=VERTEX_POINT('',#92492);
#27874=VERTEX_POINT('',#92499);
#27875=VERTEX_POINT('',#92506);
#27876=VERTEX_POINT('',#92513);
#27877=VERTEX_POINT('',#92541);
#27878=VERTEX_POINT('',#92543);
#27879=VERTEX_POINT('',#92546);
#27880=VERTEX_POINT('',#92548);
#27881=VERTEX_POINT('',#92551);
#27882=VERTEX_POINT('',#92553);
#27883=VERTEX_POINT('',#92556);
#27884=VERTEX_POINT('',#92557);
#27885=VERTEX_POINT('',#92559);
#27886=VERTEX_POINT('',#92561);
#27887=VERTEX_POINT('',#92565);
#27888=VERTEX_POINT('',#92567);
#27889=VERTEX_POINT('',#92571);
#27890=VERTEX_POINT('',#92573);
#27891=VERTEX_POINT('',#92580);
#27892=VERTEX_POINT('',#92582);
#27893=VERTEX_POINT('',#92586);
#27894=VERTEX_POINT('',#92591);
#27895=VERTEX_POINT('',#92592);
#27896=VERTEX_POINT('',#92597);
#27897=VERTEX_POINT('',#92601);
#27898=VERTEX_POINT('',#92603);
#27899=VERTEX_POINT('',#92615);
#27900=VERTEX_POINT('',#92616);
#27901=VERTEX_POINT('',#92620);
#27902=VERTEX_POINT('',#92621);
#27903=VERTEX_POINT('',#92628);
#27904=VERTEX_POINT('',#92629);
#27905=VERTEX_POINT('',#92633);
#27906=VERTEX_POINT('',#92634);
#27907=VERTEX_POINT('',#92641);
#27908=VERTEX_POINT('',#92644);
#27909=VERTEX_POINT('',#92648);
#27910=VERTEX_POINT('',#92652);
#27911=VERTEX_POINT('',#92658);
#27912=VERTEX_POINT('',#92659);
#27913=VERTEX_POINT('',#92663);
#27914=VERTEX_POINT('',#92664);
#27915=VERTEX_POINT('',#92675);
#27916=VERTEX_POINT('',#92705);
#27917=VERTEX_POINT('',#92707);
#27918=VERTEX_POINT('',#92719);
#27919=VERTEX_POINT('',#92734);
#27920=VERTEX_POINT('',#92735);
#27921=VERTEX_POINT('',#92737);
#27922=VERTEX_POINT('',#92739);
#27923=VERTEX_POINT('',#92743);
#27924=VERTEX_POINT('',#92744);
#27925=VERTEX_POINT('',#92746);
#27926=VERTEX_POINT('',#92748);
#27927=VERTEX_POINT('',#92821);
#27928=VERTEX_POINT('',#92857);
#27929=VERTEX_POINT('',#92895);
#27930=VERTEX_POINT('',#92897);
#27931=VERTEX_POINT('',#93043);
#27932=VERTEX_POINT('',#93045);
#27933=VERTEX_POINT('',#93047);
#27934=VERTEX_POINT('',#93049);
#27935=VERTEX_POINT('',#93051);
#27936=VERTEX_POINT('',#93053);
#27937=VERTEX_POINT('',#93055);
#27938=VERTEX_POINT('',#93057);
#27939=VERTEX_POINT('',#93059);
#27940=VERTEX_POINT('',#93061);
#27941=VERTEX_POINT('',#93063);
#27942=VERTEX_POINT('',#93065);
#27943=VERTEX_POINT('',#93068);
#27944=VERTEX_POINT('',#93070);
#27945=VERTEX_POINT('',#93072);
#27946=VERTEX_POINT('',#93074);
#27947=VERTEX_POINT('',#93076);
#27948=VERTEX_POINT('',#93078);
#27949=VERTEX_POINT('',#93080);
#27950=VERTEX_POINT('',#93082);
#27951=VERTEX_POINT('',#93084);
#27952=VERTEX_POINT('',#93086);
#27953=VERTEX_POINT('',#93088);
#27954=VERTEX_POINT('',#93090);
#27955=VERTEX_POINT('',#93092);
#27956=VERTEX_POINT('',#93094);
#27957=VERTEX_POINT('',#93096);
#27958=VERTEX_POINT('',#93098);
#27959=VERTEX_POINT('',#93100);
#27960=VERTEX_POINT('',#93102);
#27961=VERTEX_POINT('',#93104);
#27962=VERTEX_POINT('',#93106);
#27963=VERTEX_POINT('',#93108);
#27964=VERTEX_POINT('',#93110);
#27965=VERTEX_POINT('',#93112);
#27966=VERTEX_POINT('',#93114);
#27967=VERTEX_POINT('',#93116);
#27968=VERTEX_POINT('',#93118);
#27969=VERTEX_POINT('',#93120);
#27970=VERTEX_POINT('',#93122);
#27971=VERTEX_POINT('',#93124);
#27972=VERTEX_POINT('',#93126);
#27973=VERTEX_POINT('',#93128);
#27974=VERTEX_POINT('',#93130);
#27975=VERTEX_POINT('',#93132);
#27976=VERTEX_POINT('',#93134);
#27977=VERTEX_POINT('',#93136);
#27978=VERTEX_POINT('',#93138);
#27979=VERTEX_POINT('',#93140);
#27980=VERTEX_POINT('',#93142);
#27981=VERTEX_POINT('',#93144);
#27982=VERTEX_POINT('',#93146);
#27983=VERTEX_POINT('',#93148);
#27984=VERTEX_POINT('',#93150);
#27985=VERTEX_POINT('',#93152);
#27986=VERTEX_POINT('',#93154);
#27987=VERTEX_POINT('',#93156);
#27988=VERTEX_POINT('',#93158);
#27989=VERTEX_POINT('',#93160);
#27990=VERTEX_POINT('',#93162);
#27991=VERTEX_POINT('',#93164);
#27992=VERTEX_POINT('',#93166);
#27993=VERTEX_POINT('',#93170);
#27994=VERTEX_POINT('',#93172);
#27995=VERTEX_POINT('',#93176);
#27996=VERTEX_POINT('',#93178);
#27997=VERTEX_POINT('',#93251);
#27998=VERTEX_POINT('',#93287);
#27999=VERTEX_POINT('',#93325);
#28000=VERTEX_POINT('',#93327);
#28001=VERTEX_POINT('',#93472);
#28002=VERTEX_POINT('',#93474);
#28003=VERTEX_POINT('',#93478);
#28004=VERTEX_POINT('',#93480);
#28005=VERTEX_POINT('',#93553);
#28006=VERTEX_POINT('',#93589);
#28007=VERTEX_POINT('',#93627);
#28008=VERTEX_POINT('',#93629);
#28009=VERTEX_POINT('',#93774);
#28010=VERTEX_POINT('',#93776);
#28011=VERTEX_POINT('',#93780);
#28012=VERTEX_POINT('',#93782);
#28013=VERTEX_POINT('',#93855);
#28014=VERTEX_POINT('',#93891);
#28015=VERTEX_POINT('',#93929);
#28016=VERTEX_POINT('',#93931);
#28017=VERTEX_POINT('',#94076);
#28018=VERTEX_POINT('',#94078);
#28019=VERTEX_POINT('',#94082);
#28020=VERTEX_POINT('',#94084);
#28021=VERTEX_POINT('',#94157);
#28022=VERTEX_POINT('',#94193);
#28023=VERTEX_POINT('',#94231);
#28024=VERTEX_POINT('',#94233);
#28025=VERTEX_POINT('',#94378);
#28026=VERTEX_POINT('',#94380);
#28027=VERTEX_POINT('',#94384);
#28028=VERTEX_POINT('',#94386);
#28029=VERTEX_POINT('',#94459);
#28030=VERTEX_POINT('',#94495);
#28031=VERTEX_POINT('',#94533);
#28032=VERTEX_POINT('',#94535);
#28033=VERTEX_POINT('',#94680);
#28034=VERTEX_POINT('',#94682);
#28035=VERTEX_POINT('',#94686);
#28036=VERTEX_POINT('',#94688);
#28037=VERTEX_POINT('',#94761);
#28038=VERTEX_POINT('',#94797);
#28039=VERTEX_POINT('',#94835);
#28040=VERTEX_POINT('',#94837);
#28041=VERTEX_POINT('',#94982);
#28042=VERTEX_POINT('',#94984);
#28043=VERTEX_POINT('',#94988);
#28044=VERTEX_POINT('',#94990);
#28045=VERTEX_POINT('',#95063);
#28046=VERTEX_POINT('',#95099);
#28047=VERTEX_POINT('',#95137);
#28048=VERTEX_POINT('',#95139);
#28049=VERTEX_POINT('',#95284);
#28050=VERTEX_POINT('',#95286);
#28051=VERTEX_POINT('',#95290);
#28052=VERTEX_POINT('',#95292);
#28053=VERTEX_POINT('',#95365);
#28054=VERTEX_POINT('',#95401);
#28055=VERTEX_POINT('',#95439);
#28056=VERTEX_POINT('',#95441);
#28057=VERTEX_POINT('',#95586);
#28058=VERTEX_POINT('',#95588);
#28059=VERTEX_POINT('',#95592);
#28060=VERTEX_POINT('',#95594);
#28061=VERTEX_POINT('',#95667);
#28062=VERTEX_POINT('',#95703);
#28063=VERTEX_POINT('',#95741);
#28064=VERTEX_POINT('',#95743);
#28065=VERTEX_POINT('',#95888);
#28066=VERTEX_POINT('',#95890);
#28067=VERTEX_POINT('',#95894);
#28068=VERTEX_POINT('',#95896);
#28069=VERTEX_POINT('',#95969);
#28070=VERTEX_POINT('',#96005);
#28071=VERTEX_POINT('',#96043);
#28072=VERTEX_POINT('',#96045);
#28073=VERTEX_POINT('',#96190);
#28074=VERTEX_POINT('',#96192);
#28075=VERTEX_POINT('',#96196);
#28076=VERTEX_POINT('',#96198);
#28077=VERTEX_POINT('',#96271);
#28078=VERTEX_POINT('',#96307);
#28079=VERTEX_POINT('',#96345);
#28080=VERTEX_POINT('',#96347);
#28081=VERTEX_POINT('',#96492);
#28082=VERTEX_POINT('',#96494);
#28083=VERTEX_POINT('',#96498);
#28084=VERTEX_POINT('',#96500);
#28085=VERTEX_POINT('',#96573);
#28086=VERTEX_POINT('',#96609);
#28087=VERTEX_POINT('',#96647);
#28088=VERTEX_POINT('',#96649);
#28089=VERTEX_POINT('',#96794);
#28090=VERTEX_POINT('',#96796);
#28091=VERTEX_POINT('',#96800);
#28092=VERTEX_POINT('',#96802);
#28093=VERTEX_POINT('',#96875);
#28094=VERTEX_POINT('',#96911);
#28095=VERTEX_POINT('',#96949);
#28096=VERTEX_POINT('',#96951);
#28097=VERTEX_POINT('',#97096);
#28098=VERTEX_POINT('',#97098);
#28099=VERTEX_POINT('',#97102);
#28100=VERTEX_POINT('',#97104);
#28101=VERTEX_POINT('',#97177);
#28102=VERTEX_POINT('',#97213);
#28103=VERTEX_POINT('',#97251);
#28104=VERTEX_POINT('',#97253);
#28105=VERTEX_POINT('',#97398);
#28106=VERTEX_POINT('',#97400);
#28107=VERTEX_POINT('',#97473);
#28108=VERTEX_POINT('',#97509);
#28109=VERTEX_POINT('',#97547);
#28110=VERTEX_POINT('',#97549);
#28111=VERTEX_POINT('',#97622);
#28112=VERTEX_POINT('',#97658);
#28113=VERTEX_POINT('',#97700);
#28114=VERTEX_POINT('',#97702);
#28115=VERTEX_POINT('',#97707);
#28116=VERTEX_POINT('',#97710);
#28117=VERTEX_POINT('',#97714);
#28118=VERTEX_POINT('',#97720);
#28119=VERTEX_POINT('',#97721);
#28120=VERTEX_POINT('',#97723);
#28121=VERTEX_POINT('',#97727);
#28122=VERTEX_POINT('',#97728);
#28123=VERTEX_POINT('',#97739);
#28124=VERTEX_POINT('',#97770);
#28125=VERTEX_POINT('',#97789);
#28126=VERTEX_POINT('',#97812);
#28127=VERTEX_POINT('',#97813);
#28128=VERTEX_POINT('',#97817);
#28129=VERTEX_POINT('',#97819);
#28130=VERTEX_POINT('',#97825);
#28131=VERTEX_POINT('',#97829);
#28132=VERTEX_POINT('',#97835);
#28133=VERTEX_POINT('',#97837);
#28134=VERTEX_POINT('',#97841);
#28135=VERTEX_POINT('',#97845);
#28136=VERTEX_POINT('',#97847);
#28137=VERTEX_POINT('',#97851);
#28138=VERTEX_POINT('',#97855);
#28139=VERTEX_POINT('',#97857);
#28140=VERTEX_POINT('',#97861);
#28141=VERTEX_POINT('',#97865);
#28142=VERTEX_POINT('',#97867);
#28143=VERTEX_POINT('',#97871);
#28144=VERTEX_POINT('',#97875);
#28145=VERTEX_POINT('',#97877);
#28146=VERTEX_POINT('',#97881);
#28147=VERTEX_POINT('',#97885);
#28148=VERTEX_POINT('',#97887);
#28149=VERTEX_POINT('',#97891);
#28150=VERTEX_POINT('',#97895);
#28151=VERTEX_POINT('',#97897);
#28152=VERTEX_POINT('',#97901);
#28153=VERTEX_POINT('',#97905);
#28154=VERTEX_POINT('',#97907);
#28155=VERTEX_POINT('',#97911);
#28156=VERTEX_POINT('',#97915);
#28157=VERTEX_POINT('',#97917);
#28158=VERTEX_POINT('',#97921);
#28159=VERTEX_POINT('',#97925);
#28160=VERTEX_POINT('',#97927);
#28161=VERTEX_POINT('',#97931);
#28162=VERTEX_POINT('',#97935);
#28163=VERTEX_POINT('',#97937);
#28164=VERTEX_POINT('',#97941);
#28165=VERTEX_POINT('',#97945);
#28166=VERTEX_POINT('',#97947);
#28167=VERTEX_POINT('',#97951);
#28168=VERTEX_POINT('',#97955);
#28169=VERTEX_POINT('',#97957);
#28170=VERTEX_POINT('',#97961);
#28171=VERTEX_POINT('',#97965);
#28172=VERTEX_POINT('',#97967);
#28173=VERTEX_POINT('',#97971);
#28174=VERTEX_POINT('',#97975);
#28175=VERTEX_POINT('',#97977);
#28176=VERTEX_POINT('',#97981);
#28177=VERTEX_POINT('',#97985);
#28178=VERTEX_POINT('',#97987);
#28179=VERTEX_POINT('',#97991);
#28180=VERTEX_POINT('',#97995);
#28181=VERTEX_POINT('',#97997);
#28182=VERTEX_POINT('',#98001);
#28183=VERTEX_POINT('',#98005);
#28184=VERTEX_POINT('',#98007);
#28185=VERTEX_POINT('',#98011);
#28186=VERTEX_POINT('',#98015);
#28187=VERTEX_POINT('',#98017);
#28188=VERTEX_POINT('',#98021);
#28189=VERTEX_POINT('',#98024);
#28190=VERTEX_POINT('',#98028);
#28191=VERTEX_POINT('',#98030);
#28192=VERTEX_POINT('',#98034);
#28193=VERTEX_POINT('',#98038);
#28194=VERTEX_POINT('',#98040);
#28195=VERTEX_POINT('',#98044);
#28196=VERTEX_POINT('',#98048);
#28197=VERTEX_POINT('',#98050);
#28198=VERTEX_POINT('',#98054);
#28199=VERTEX_POINT('',#98058);
#28200=VERTEX_POINT('',#98060);
#28201=VERTEX_POINT('',#98064);
#28202=VERTEX_POINT('',#98068);
#28203=VERTEX_POINT('',#98070);
#28204=VERTEX_POINT('',#98074);
#28205=VERTEX_POINT('',#98078);
#28206=VERTEX_POINT('',#98080);
#28207=VERTEX_POINT('',#98084);
#28208=VERTEX_POINT('',#98088);
#28209=VERTEX_POINT('',#98090);
#28210=VERTEX_POINT('',#98094);
#28211=VERTEX_POINT('',#98098);
#28212=VERTEX_POINT('',#98100);
#28213=VERTEX_POINT('',#98104);
#28214=VERTEX_POINT('',#98108);
#28215=VERTEX_POINT('',#98110);
#28216=VERTEX_POINT('',#98114);
#28217=VERTEX_POINT('',#98118);
#28218=VERTEX_POINT('',#98120);
#28219=VERTEX_POINT('',#98124);
#28220=VERTEX_POINT('',#98128);
#28221=VERTEX_POINT('',#98130);
#28222=VERTEX_POINT('',#98134);
#28223=VERTEX_POINT('',#98138);
#28224=VERTEX_POINT('',#98140);
#28225=VERTEX_POINT('',#98144);
#28226=VERTEX_POINT('',#98148);
#28227=VERTEX_POINT('',#98150);
#28228=VERTEX_POINT('',#98154);
#28229=VERTEX_POINT('',#98158);
#28230=VERTEX_POINT('',#98160);
#28231=VERTEX_POINT('',#98164);
#28232=VERTEX_POINT('',#98168);
#28233=VERTEX_POINT('',#98170);
#28234=VERTEX_POINT('',#98174);
#28235=VERTEX_POINT('',#98178);
#28236=VERTEX_POINT('',#98180);
#28237=VERTEX_POINT('',#98184);
#28238=VERTEX_POINT('',#98188);
#28239=VERTEX_POINT('',#98190);
#28240=VERTEX_POINT('',#98194);
#28241=VERTEX_POINT('',#98198);
#28242=VERTEX_POINT('',#98200);
#28243=VERTEX_POINT('',#98204);
#28244=VERTEX_POINT('',#98208);
#28245=VERTEX_POINT('',#98210);
#28246=VERTEX_POINT('',#98214);
#28247=VERTEX_POINT('',#98218);
#28248=VERTEX_POINT('',#98220);
#28249=VERTEX_POINT('',#98224);
#28250=VERTEX_POINT('',#98230);
#28251=VERTEX_POINT('',#98234);
#28252=VERTEX_POINT('',#98238);
#28253=VERTEX_POINT('',#98240);
#28254=VERTEX_POINT('',#98250);
#28255=VERTEX_POINT('',#98254);
#28256=VERTEX_POINT('',#98256);
#28257=VERTEX_POINT('',#98258);
#28258=VERTEX_POINT('',#98262);
#28259=VERTEX_POINT('',#98264);
#28260=VERTEX_POINT('',#98268);
#28261=VERTEX_POINT('',#98272);
#28262=VERTEX_POINT('',#98274);
#28263=VERTEX_POINT('',#98278);
#28264=VERTEX_POINT('',#98282);
#28265=VERTEX_POINT('',#98284);
#28266=VERTEX_POINT('',#98288);
#28267=VERTEX_POINT('',#98292);
#28268=VERTEX_POINT('',#98294);
#28269=VERTEX_POINT('',#98298);
#28270=VERTEX_POINT('',#98302);
#28271=VERTEX_POINT('',#98304);
#28272=VERTEX_POINT('',#98308);
#28273=VERTEX_POINT('',#98312);
#28274=VERTEX_POINT('',#98314);
#28275=VERTEX_POINT('',#98318);
#28276=VERTEX_POINT('',#98322);
#28277=VERTEX_POINT('',#98324);
#28278=VERTEX_POINT('',#98328);
#28279=VERTEX_POINT('',#98332);
#28280=VERTEX_POINT('',#98334);
#28281=VERTEX_POINT('',#98338);
#28282=VERTEX_POINT('',#98342);
#28283=VERTEX_POINT('',#98344);
#28284=VERTEX_POINT('',#98348);
#28285=VERTEX_POINT('',#98352);
#28286=VERTEX_POINT('',#98354);
#28287=VERTEX_POINT('',#98358);
#28288=VERTEX_POINT('',#98362);
#28289=VERTEX_POINT('',#98364);
#28290=VERTEX_POINT('',#98368);
#28291=VERTEX_POINT('',#98372);
#28292=VERTEX_POINT('',#98374);
#28293=VERTEX_POINT('',#98378);
#28294=VERTEX_POINT('',#98382);
#28295=VERTEX_POINT('',#98384);
#28296=VERTEX_POINT('',#98388);
#28297=VERTEX_POINT('',#98392);
#28298=VERTEX_POINT('',#98394);
#28299=VERTEX_POINT('',#98398);
#28300=VERTEX_POINT('',#98402);
#28301=VERTEX_POINT('',#98404);
#28302=VERTEX_POINT('',#98408);
#28303=VERTEX_POINT('',#98412);
#28304=VERTEX_POINT('',#98414);
#28305=VERTEX_POINT('',#98418);
#28306=VERTEX_POINT('',#98422);
#28307=VERTEX_POINT('',#98424);
#28308=VERTEX_POINT('',#98431);
#28309=VERTEX_POINT('',#98435);
#28310=VERTEX_POINT('',#98439);
#28311=VERTEX_POINT('',#98441);
#28312=VERTEX_POINT('',#98445);
#28313=VERTEX_POINT('',#98449);
#28314=VERTEX_POINT('',#98451);
#28315=VERTEX_POINT('',#98455);
#28316=VERTEX_POINT('',#98459);
#28317=VERTEX_POINT('',#98461);
#28318=VERTEX_POINT('',#98465);
#28319=VERTEX_POINT('',#98469);
#28320=VERTEX_POINT('',#98471);
#28321=VERTEX_POINT('',#98475);
#28322=VERTEX_POINT('',#98479);
#28323=VERTEX_POINT('',#98481);
#28324=VERTEX_POINT('',#98485);
#28325=VERTEX_POINT('',#98489);
#28326=VERTEX_POINT('',#98491);
#28327=VERTEX_POINT('',#98495);
#28328=VERTEX_POINT('',#98499);
#28329=VERTEX_POINT('',#98501);
#28330=VERTEX_POINT('',#98505);
#28331=VERTEX_POINT('',#98509);
#28332=VERTEX_POINT('',#98511);
#28333=VERTEX_POINT('',#98515);
#28334=VERTEX_POINT('',#98519);
#28335=VERTEX_POINT('',#98521);
#28336=VERTEX_POINT('',#98525);
#28337=VERTEX_POINT('',#98529);
#28338=VERTEX_POINT('',#98531);
#28339=VERTEX_POINT('',#98535);
#28340=VERTEX_POINT('',#98539);
#28341=VERTEX_POINT('',#98541);
#28342=VERTEX_POINT('',#98545);
#28343=VERTEX_POINT('',#98549);
#28344=VERTEX_POINT('',#98551);
#28345=VERTEX_POINT('',#98555);
#28346=VERTEX_POINT('',#98559);
#28347=VERTEX_POINT('',#98561);
#28348=VERTEX_POINT('',#98565);
#28349=VERTEX_POINT('',#98569);
#28350=VERTEX_POINT('',#98571);
#28351=VERTEX_POINT('',#98575);
#28352=VERTEX_POINT('',#98579);
#28353=VERTEX_POINT('',#98581);
#28354=VERTEX_POINT('',#98585);
#28355=VERTEX_POINT('',#98589);
#28356=VERTEX_POINT('',#98591);
#28357=VERTEX_POINT('',#98595);
#28358=VERTEX_POINT('',#98599);
#28359=VERTEX_POINT('',#98601);
#28360=VERTEX_POINT('',#98605);
#28361=VERTEX_POINT('',#98609);
#28362=VERTEX_POINT('',#98611);
#28363=VERTEX_POINT('',#98615);
#28364=VERTEX_POINT('',#98619);
#28365=VERTEX_POINT('',#98621);
#28366=VERTEX_POINT('',#98625);
#28367=VERTEX_POINT('',#98629);
#28368=VERTEX_POINT('',#98859);
#28369=VERTEX_POINT('',#98861);
#28370=VERTEX_POINT('',#98865);
#28371=VERTEX_POINT('',#98868);
#28372=VERTEX_POINT('',#98872);
#28373=VERTEX_POINT('',#98876);
#28374=VERTEX_POINT('',#98880);
#28375=VERTEX_POINT('',#98883);
#28376=VERTEX_POINT('',#98887);
#28377=VERTEX_POINT('',#98893);
#28378=VERTEX_POINT('',#98896);
#28379=VERTEX_POINT('',#98901);
#28380=VERTEX_POINT('',#98902);
#28381=VERTEX_POINT('',#98909);
#28382=VERTEX_POINT('',#98911);
#28383=VERTEX_POINT('',#98915);
#28384=VERTEX_POINT('',#98918);
#28385=VERTEX_POINT('',#98922);
#28386=VERTEX_POINT('',#98926);
#28387=VERTEX_POINT('',#98929);
#28388=VERTEX_POINT('',#98933);
#28389=VERTEX_POINT('',#98937);
#28390=VERTEX_POINT('',#98940);
#28391=VERTEX_POINT('',#98947);
#28392=VERTEX_POINT('',#98949);
#28393=VERTEX_POINT('',#98953);
#28394=VERTEX_POINT('',#98957);
#28395=VERTEX_POINT('',#98958);
#28396=VERTEX_POINT('',#98960);
#28397=VERTEX_POINT('',#98962);
#28398=VERTEX_POINT('',#98966);
#28399=VERTEX_POINT('',#98968);
#28400=VERTEX_POINT('',#98972);
#28401=VERTEX_POINT('',#98976);
#28402=VERTEX_POINT('',#98977);
#28403=VERTEX_POINT('',#98979);
#28404=VERTEX_POINT('',#98981);
#28405=VERTEX_POINT('',#98985);
#28406=VERTEX_POINT('',#98988);
#28407=VERTEX_POINT('',#98991);
#28408=VERTEX_POINT('',#98995);
#28409=VERTEX_POINT('',#98999);
#28410=VERTEX_POINT('',#99000);
#28411=VERTEX_POINT('',#99002);
#28412=VERTEX_POINT('',#99004);
#28413=VERTEX_POINT('',#99008);
#28414=VERTEX_POINT('',#99010);
#28415=VERTEX_POINT('',#99015);
#28416=VERTEX_POINT('',#99019);
#28417=VERTEX_POINT('',#99023);
#28418=VERTEX_POINT('',#99025);
#28419=VERTEX_POINT('',#99029);
#28420=VERTEX_POINT('',#99031);
#28421=VERTEX_POINT('',#99035);
#28422=VERTEX_POINT('',#99037);
#28423=VERTEX_POINT('',#99041);
#28424=VERTEX_POINT('',#99043);
#28425=VERTEX_POINT('',#99047);
#28426=VERTEX_POINT('',#99049);
#28427=VERTEX_POINT('',#99053);
#28428=VERTEX_POINT('',#99055);
#28429=VERTEX_POINT('',#99059);
#28430=VERTEX_POINT('',#99061);
#28431=VERTEX_POINT('',#99065);
#28432=VERTEX_POINT('',#99067);
#28433=VERTEX_POINT('',#99071);
#28434=VERTEX_POINT('',#99073);
#28435=VERTEX_POINT('',#99077);
#28436=VERTEX_POINT('',#99079);
#28437=VERTEX_POINT('',#99083);
#28438=VERTEX_POINT('',#99085);
#28439=VERTEX_POINT('',#99089);
#28440=VERTEX_POINT('',#99091);
#28441=VERTEX_POINT('',#99095);
#28442=VERTEX_POINT('',#99097);
#28443=VERTEX_POINT('',#99101);
#28444=VERTEX_POINT('',#99103);
#28445=VERTEX_POINT('',#99107);
#28446=VERTEX_POINT('',#99109);
#28447=VERTEX_POINT('',#99113);
#28448=VERTEX_POINT('',#99115);
#28449=VERTEX_POINT('',#99119);
#28450=VERTEX_POINT('',#99121);
#28451=VERTEX_POINT('',#99125);
#28452=VERTEX_POINT('',#99127);
#28453=VERTEX_POINT('',#99131);
#28454=VERTEX_POINT('',#99133);
#28455=VERTEX_POINT('',#99137);
#28456=VERTEX_POINT('',#99139);
#28457=VERTEX_POINT('',#99143);
#28458=VERTEX_POINT('',#99145);
#28459=VERTEX_POINT('',#99149);
#28460=VERTEX_POINT('',#99151);
#28461=VERTEX_POINT('',#99155);
#28462=VERTEX_POINT('',#99157);
#28463=VERTEX_POINT('',#99161);
#28464=VERTEX_POINT('',#99163);
#28465=VERTEX_POINT('',#99167);
#28466=VERTEX_POINT('',#99169);
#28467=VERTEX_POINT('',#99173);
#28468=VERTEX_POINT('',#99175);
#28469=VERTEX_POINT('',#99179);
#28470=VERTEX_POINT('',#99181);
#28471=VERTEX_POINT('',#99185);
#28472=VERTEX_POINT('',#99187);
#28473=VERTEX_POINT('',#99191);
#28474=VERTEX_POINT('',#99193);
#28475=VERTEX_POINT('',#99197);
#28476=VERTEX_POINT('',#99199);
#28477=VERTEX_POINT('',#99203);
#28478=VERTEX_POINT('',#99205);
#28479=VERTEX_POINT('',#99209);
#28480=VERTEX_POINT('',#99211);
#28481=VERTEX_POINT('',#99215);
#28482=VERTEX_POINT('',#99217);
#28483=VERTEX_POINT('',#99221);
#28484=VERTEX_POINT('',#99223);
#28485=VERTEX_POINT('',#99227);
#28486=VERTEX_POINT('',#99229);
#28487=VERTEX_POINT('',#99233);
#28488=VERTEX_POINT('',#99235);
#28489=VERTEX_POINT('',#99239);
#28490=VERTEX_POINT('',#99241);
#28491=VERTEX_POINT('',#99245);
#28492=VERTEX_POINT('',#99247);
#28493=VERTEX_POINT('',#99251);
#28494=VERTEX_POINT('',#99253);
#28495=VERTEX_POINT('',#99257);
#28496=VERTEX_POINT('',#99259);
#28497=VERTEX_POINT('',#99263);
#28498=VERTEX_POINT('',#99265);
#28499=VERTEX_POINT('',#99269);
#28500=VERTEX_POINT('',#99271);
#28501=VERTEX_POINT('',#99275);
#28502=VERTEX_POINT('',#99277);
#28503=VERTEX_POINT('',#99281);
#28504=VERTEX_POINT('',#99283);
#28505=VERTEX_POINT('',#99287);
#28506=VERTEX_POINT('',#99289);
#28507=VERTEX_POINT('',#99293);
#28508=VERTEX_POINT('',#99295);
#28509=VERTEX_POINT('',#99299);
#28510=VERTEX_POINT('',#99301);
#28511=VERTEX_POINT('',#99305);
#28512=VERTEX_POINT('',#99307);
#28513=VERTEX_POINT('',#99311);
#28514=VERTEX_POINT('',#99313);
#28515=VERTEX_POINT('',#99317);
#28516=VERTEX_POINT('',#99319);
#28517=VERTEX_POINT('',#99323);
#28518=VERTEX_POINT('',#99325);
#28519=VERTEX_POINT('',#99329);
#28520=VERTEX_POINT('',#99331);
#28521=VERTEX_POINT('',#99335);
#28522=VERTEX_POINT('',#99337);
#28523=VERTEX_POINT('',#99341);
#28524=VERTEX_POINT('',#99343);
#28525=VERTEX_POINT('',#99347);
#28526=VERTEX_POINT('',#99349);
#28527=VERTEX_POINT('',#99353);
#28528=VERTEX_POINT('',#99355);
#28529=VERTEX_POINT('',#99359);
#28530=VERTEX_POINT('',#99361);
#28531=VERTEX_POINT('',#99365);
#28532=VERTEX_POINT('',#99367);
#28533=VERTEX_POINT('',#99371);
#28534=VERTEX_POINT('',#99373);
#28535=VERTEX_POINT('',#99377);
#28536=VERTEX_POINT('',#99379);
#28537=VERTEX_POINT('',#99383);
#28538=VERTEX_POINT('',#99385);
#28539=VERTEX_POINT('',#99389);
#28540=VERTEX_POINT('',#99391);
#28541=VERTEX_POINT('',#99395);
#28542=VERTEX_POINT('',#99397);
#28543=VERTEX_POINT('',#99401);
#28544=VERTEX_POINT('',#99403);
#28545=VERTEX_POINT('',#99407);
#28546=VERTEX_POINT('',#99409);
#28547=VERTEX_POINT('',#99413);
#28548=VERTEX_POINT('',#99415);
#28549=VERTEX_POINT('',#99419);
#28550=VERTEX_POINT('',#99421);
#28551=VERTEX_POINT('',#99425);
#28552=VERTEX_POINT('',#99427);
#28553=VERTEX_POINT('',#99431);
#28554=VERTEX_POINT('',#99433);
#28555=VERTEX_POINT('',#99437);
#28556=VERTEX_POINT('',#99439);
#28557=VERTEX_POINT('',#99443);
#28558=VERTEX_POINT('',#99445);
#28559=VERTEX_POINT('',#99449);
#28560=VERTEX_POINT('',#99451);
#28561=VERTEX_POINT('',#99455);
#28562=VERTEX_POINT('',#99457);
#28563=VERTEX_POINT('',#99461);
#28564=VERTEX_POINT('',#99463);
#28565=VERTEX_POINT('',#99467);
#28566=VERTEX_POINT('',#99469);
#28567=VERTEX_POINT('',#99473);
#28568=VERTEX_POINT('',#99475);
#28569=VERTEX_POINT('',#99479);
#28570=VERTEX_POINT('',#99481);
#28571=VERTEX_POINT('',#99485);
#28572=VERTEX_POINT('',#99487);
#28573=VERTEX_POINT('',#99491);
#28574=VERTEX_POINT('',#99493);
#28575=VERTEX_POINT('',#99497);
#28576=VERTEX_POINT('',#99499);
#28577=VERTEX_POINT('',#99503);
#28578=VERTEX_POINT('',#99505);
#28579=VERTEX_POINT('',#99509);
#28580=VERTEX_POINT('',#99511);
#28581=VERTEX_POINT('',#99515);
#28582=VERTEX_POINT('',#99517);
#28583=VERTEX_POINT('',#99521);
#28584=VERTEX_POINT('',#99523);
#28585=VERTEX_POINT('',#99527);
#28586=VERTEX_POINT('',#99529);
#28587=VERTEX_POINT('',#99533);
#28588=VERTEX_POINT('',#99535);
#28589=VERTEX_POINT('',#99539);
#28590=VERTEX_POINT('',#99541);
#28591=VERTEX_POINT('',#99545);
#28592=VERTEX_POINT('',#99547);
#28593=VERTEX_POINT('',#99551);
#28594=VERTEX_POINT('',#99553);
#28595=VERTEX_POINT('',#99557);
#28596=VERTEX_POINT('',#99559);
#28597=VERTEX_POINT('',#99563);
#28598=VERTEX_POINT('',#99565);
#28599=VERTEX_POINT('',#99569);
#28600=VERTEX_POINT('',#99571);
#28601=VERTEX_POINT('',#99575);
#28602=VERTEX_POINT('',#99577);
#28603=VERTEX_POINT('',#99581);
#28604=VERTEX_POINT('',#99583);
#28605=VERTEX_POINT('',#99587);
#28606=VERTEX_POINT('',#99589);
#28607=VERTEX_POINT('',#99593);
#28608=VERTEX_POINT('',#99595);
#28609=VERTEX_POINT('',#99599);
#28610=VERTEX_POINT('',#99601);
#28611=VERTEX_POINT('',#99605);
#28612=VERTEX_POINT('',#99607);
#28613=VERTEX_POINT('',#99611);
#28614=VERTEX_POINT('',#99613);
#28615=VERTEX_POINT('',#99617);
#28616=VERTEX_POINT('',#99619);
#28617=VERTEX_POINT('',#99623);
#28618=VERTEX_POINT('',#99625);
#28619=VERTEX_POINT('',#99629);
#28620=VERTEX_POINT('',#99631);
#28621=VERTEX_POINT('',#99635);
#28622=VERTEX_POINT('',#99637);
#28623=VERTEX_POINT('',#99641);
#28624=VERTEX_POINT('',#99643);
#28625=VERTEX_POINT('',#99647);
#28626=VERTEX_POINT('',#99649);
#28627=VERTEX_POINT('',#99653);
#28628=VERTEX_POINT('',#99655);
#28629=VERTEX_POINT('',#99659);
#28630=VERTEX_POINT('',#99661);
#28631=VERTEX_POINT('',#99665);
#28632=VERTEX_POINT('',#99667);
#28633=VERTEX_POINT('',#99671);
#28634=VERTEX_POINT('',#99673);
#28635=VERTEX_POINT('',#99677);
#28636=VERTEX_POINT('',#99679);
#28637=VERTEX_POINT('',#99683);
#28638=VERTEX_POINT('',#99685);
#28639=VERTEX_POINT('',#99689);
#28640=VERTEX_POINT('',#99691);
#28641=VERTEX_POINT('',#99695);
#28642=VERTEX_POINT('',#99697);
#28643=VERTEX_POINT('',#99701);
#28644=VERTEX_POINT('',#99703);
#28645=VERTEX_POINT('',#99707);
#28646=VERTEX_POINT('',#99709);
#28647=VERTEX_POINT('',#99713);
#28648=VERTEX_POINT('',#99715);
#28649=VERTEX_POINT('',#99719);
#28650=VERTEX_POINT('',#99721);
#28651=VERTEX_POINT('',#99725);
#28652=VERTEX_POINT('',#99727);
#28653=VERTEX_POINT('',#99731);
#28654=VERTEX_POINT('',#99733);
#28655=VERTEX_POINT('',#99737);
#28656=VERTEX_POINT('',#99739);
#28657=VERTEX_POINT('',#99743);
#28658=VERTEX_POINT('',#99745);
#28659=VERTEX_POINT('',#99749);
#28660=VERTEX_POINT('',#99751);
#28661=VERTEX_POINT('',#99755);
#28662=VERTEX_POINT('',#99757);
#28663=VERTEX_POINT('',#99761);
#28664=VERTEX_POINT('',#99763);
#28665=VERTEX_POINT('',#99767);
#28666=VERTEX_POINT('',#99769);
#28667=VERTEX_POINT('',#99773);
#28668=VERTEX_POINT('',#99775);
#28669=VERTEX_POINT('',#99779);
#28670=VERTEX_POINT('',#99781);
#28671=VERTEX_POINT('',#99785);
#28672=VERTEX_POINT('',#99787);
#28673=VERTEX_POINT('',#99791);
#28674=VERTEX_POINT('',#99793);
#28675=VERTEX_POINT('',#99797);
#28676=VERTEX_POINT('',#99799);
#28677=VERTEX_POINT('',#99803);
#28678=VERTEX_POINT('',#99805);
#28679=VERTEX_POINT('',#99809);
#28680=VERTEX_POINT('',#99811);
#28681=VERTEX_POINT('',#99815);
#28682=VERTEX_POINT('',#99817);
#28683=VERTEX_POINT('',#99821);
#28684=VERTEX_POINT('',#99823);
#28685=VERTEX_POINT('',#99827);
#28686=VERTEX_POINT('',#99829);
#28687=VERTEX_POINT('',#99833);
#28688=VERTEX_POINT('',#99835);
#28689=VERTEX_POINT('',#99839);
#28690=VERTEX_POINT('',#99841);
#28691=VERTEX_POINT('',#99845);
#28692=VERTEX_POINT('',#99847);
#28693=VERTEX_POINT('',#99851);
#28694=VERTEX_POINT('',#99853);
#28695=VERTEX_POINT('',#99857);
#28696=VERTEX_POINT('',#99859);
#28697=VERTEX_POINT('',#99863);
#28698=VERTEX_POINT('',#99865);
#28699=VERTEX_POINT('',#99869);
#28700=VERTEX_POINT('',#99871);
#28701=VERTEX_POINT('',#99875);
#28702=VERTEX_POINT('',#99877);
#28703=VERTEX_POINT('',#99881);
#28704=VERTEX_POINT('',#99883);
#28705=VERTEX_POINT('',#99887);
#28706=VERTEX_POINT('',#99889);
#28707=VERTEX_POINT('',#99893);
#28708=VERTEX_POINT('',#99895);
#28709=VERTEX_POINT('',#99899);
#28710=VERTEX_POINT('',#99901);
#28711=VERTEX_POINT('',#99905);
#28712=VERTEX_POINT('',#99907);
#28713=VERTEX_POINT('',#99911);
#28714=VERTEX_POINT('',#99913);
#28715=VERTEX_POINT('',#99917);
#28716=VERTEX_POINT('',#99919);
#28717=VERTEX_POINT('',#99923);
#28718=VERTEX_POINT('',#99925);
#28719=VERTEX_POINT('',#99929);
#28720=VERTEX_POINT('',#99931);
#28721=VERTEX_POINT('',#99935);
#28722=VERTEX_POINT('',#99937);
#28723=VERTEX_POINT('',#99941);
#28724=VERTEX_POINT('',#99943);
#28725=VERTEX_POINT('',#99947);
#28726=VERTEX_POINT('',#99949);
#28727=VERTEX_POINT('',#99953);
#28728=VERTEX_POINT('',#99955);
#28729=VERTEX_POINT('',#99959);
#28730=VERTEX_POINT('',#99961);
#28731=VERTEX_POINT('',#99965);
#28732=VERTEX_POINT('',#99967);
#28733=VERTEX_POINT('',#99971);
#28734=VERTEX_POINT('',#99973);
#28735=VERTEX_POINT('',#99977);
#28736=VERTEX_POINT('',#99979);
#28737=VERTEX_POINT('',#99983);
#28738=VERTEX_POINT('',#99985);
#28739=VERTEX_POINT('',#99989);
#28740=VERTEX_POINT('',#99991);
#28741=VERTEX_POINT('',#99995);
#28742=VERTEX_POINT('',#99997);
#28743=VERTEX_POINT('',#100001);
#28744=VERTEX_POINT('',#100003);
#28745=VERTEX_POINT('',#100007);
#28746=VERTEX_POINT('',#100009);
#28747=VERTEX_POINT('',#100013);
#28748=VERTEX_POINT('',#100015);
#28749=VERTEX_POINT('',#100019);
#28750=VERTEX_POINT('',#100021);
#28751=VERTEX_POINT('',#100025);
#28752=VERTEX_POINT('',#100027);
#28753=VERTEX_POINT('',#100031);
#28754=VERTEX_POINT('',#100033);
#28755=VERTEX_POINT('',#100037);
#28756=VERTEX_POINT('',#100039);
#28757=VERTEX_POINT('',#100043);
#28758=VERTEX_POINT('',#100045);
#28759=VERTEX_POINT('',#100049);
#28760=VERTEX_POINT('',#100051);
#28761=VERTEX_POINT('',#100055);
#28762=VERTEX_POINT('',#100057);
#28763=VERTEX_POINT('',#100061);
#28764=VERTEX_POINT('',#100063);
#28765=VERTEX_POINT('',#100067);
#28766=VERTEX_POINT('',#100069);
#28767=VERTEX_POINT('',#100073);
#28768=VERTEX_POINT('',#100075);
#28769=VERTEX_POINT('',#100079);
#28770=VERTEX_POINT('',#100081);
#28771=VERTEX_POINT('',#100085);
#28772=VERTEX_POINT('',#100087);
#28773=VERTEX_POINT('',#100091);
#28774=VERTEX_POINT('',#100093);
#28775=VERTEX_POINT('',#100097);
#28776=VERTEX_POINT('',#100099);
#28777=VERTEX_POINT('',#100103);
#28778=VERTEX_POINT('',#100105);
#28779=VERTEX_POINT('',#100109);
#28780=VERTEX_POINT('',#100111);
#28781=VERTEX_POINT('',#100115);
#28782=VERTEX_POINT('',#100117);
#28783=VERTEX_POINT('',#100121);
#28784=VERTEX_POINT('',#100123);
#28785=VERTEX_POINT('',#100127);
#28786=VERTEX_POINT('',#100129);
#28787=VERTEX_POINT('',#100133);
#28788=VERTEX_POINT('',#100135);
#28789=VERTEX_POINT('',#100139);
#28790=VERTEX_POINT('',#100141);
#28791=VERTEX_POINT('',#100145);
#28792=VERTEX_POINT('',#100147);
#28793=VERTEX_POINT('',#100151);
#28794=VERTEX_POINT('',#100153);
#28795=VERTEX_POINT('',#100157);
#28796=VERTEX_POINT('',#100159);
#28797=VERTEX_POINT('',#100163);
#28798=VERTEX_POINT('',#100165);
#28799=VERTEX_POINT('',#100169);
#28800=VERTEX_POINT('',#100171);
#28801=VERTEX_POINT('',#100175);
#28802=VERTEX_POINT('',#100177);
#28803=VERTEX_POINT('',#100181);
#28804=VERTEX_POINT('',#100183);
#28805=VERTEX_POINT('',#100187);
#28806=VERTEX_POINT('',#100189);
#28807=VERTEX_POINT('',#100193);
#28808=VERTEX_POINT('',#100195);
#28809=VERTEX_POINT('',#100199);
#28810=VERTEX_POINT('',#100201);
#28811=VERTEX_POINT('',#100205);
#28812=VERTEX_POINT('',#100207);
#28813=VERTEX_POINT('',#100211);
#28814=VERTEX_POINT('',#100213);
#28815=VERTEX_POINT('',#100217);
#28816=VERTEX_POINT('',#100219);
#28817=VERTEX_POINT('',#100223);
#28818=VERTEX_POINT('',#100225);
#28819=VERTEX_POINT('',#100229);
#28820=VERTEX_POINT('',#100231);
#28821=VERTEX_POINT('',#100235);
#28822=VERTEX_POINT('',#100237);
#28823=VERTEX_POINT('',#100241);
#28824=VERTEX_POINT('',#100243);
#28825=VERTEX_POINT('',#100247);
#28826=VERTEX_POINT('',#100249);
#28827=VERTEX_POINT('',#100253);
#28828=VERTEX_POINT('',#100255);
#28829=VERTEX_POINT('',#100259);
#28830=VERTEX_POINT('',#100261);
#28831=VERTEX_POINT('',#100265);
#28832=VERTEX_POINT('',#100267);
#28833=VERTEX_POINT('',#100271);
#28834=VERTEX_POINT('',#100273);
#28835=VERTEX_POINT('',#100277);
#28836=VERTEX_POINT('',#100279);
#28837=VERTEX_POINT('',#100283);
#28838=VERTEX_POINT('',#100285);
#28839=VERTEX_POINT('',#100289);
#28840=VERTEX_POINT('',#100291);
#28841=VERTEX_POINT('',#100295);
#28842=VERTEX_POINT('',#100297);
#28843=VERTEX_POINT('',#100301);
#28844=VERTEX_POINT('',#100303);
#28845=VERTEX_POINT('',#100307);
#28846=VERTEX_POINT('',#100309);
#28847=VERTEX_POINT('',#100313);
#28848=VERTEX_POINT('',#100315);
#28849=VERTEX_POINT('',#100319);
#28850=VERTEX_POINT('',#100321);
#28851=VERTEX_POINT('',#100325);
#28852=VERTEX_POINT('',#100327);
#28853=VERTEX_POINT('',#100331);
#28854=VERTEX_POINT('',#100333);
#28855=VERTEX_POINT('',#100337);
#28856=VERTEX_POINT('',#100339);
#28857=VERTEX_POINT('',#100343);
#28858=VERTEX_POINT('',#100345);
#28859=VERTEX_POINT('',#100349);
#28860=VERTEX_POINT('',#100351);
#28861=VERTEX_POINT('',#100355);
#28862=VERTEX_POINT('',#100357);
#28863=VERTEX_POINT('',#100361);
#28864=VERTEX_POINT('',#100363);
#28865=VERTEX_POINT('',#100367);
#28866=VERTEX_POINT('',#100369);
#28867=VERTEX_POINT('',#100373);
#28868=VERTEX_POINT('',#100375);
#28869=VERTEX_POINT('',#100379);
#28870=VERTEX_POINT('',#100381);
#28871=VERTEX_POINT('',#100385);
#28872=VERTEX_POINT('',#100387);
#28873=VERTEX_POINT('',#100391);
#28874=VERTEX_POINT('',#100393);
#28875=VERTEX_POINT('',#100397);
#28876=VERTEX_POINT('',#100399);
#28877=VERTEX_POINT('',#100403);
#28878=VERTEX_POINT('',#100405);
#28879=VERTEX_POINT('',#100409);
#28880=VERTEX_POINT('',#100411);
#28881=VERTEX_POINT('',#100415);
#28882=VERTEX_POINT('',#100417);
#28883=VERTEX_POINT('',#100421);
#28884=VERTEX_POINT('',#100423);
#28885=VERTEX_POINT('',#100427);
#28886=VERTEX_POINT('',#100429);
#28887=VERTEX_POINT('',#100433);
#28888=VERTEX_POINT('',#100435);
#28889=VERTEX_POINT('',#100439);
#28890=VERTEX_POINT('',#100441);
#28891=VERTEX_POINT('',#100445);
#28892=VERTEX_POINT('',#100447);
#28893=VERTEX_POINT('',#100451);
#28894=VERTEX_POINT('',#100453);
#28895=VERTEX_POINT('',#100457);
#28896=VERTEX_POINT('',#100459);
#28897=VERTEX_POINT('',#100463);
#28898=VERTEX_POINT('',#100465);
#28899=VERTEX_POINT('',#100469);
#28900=VERTEX_POINT('',#100471);
#28901=VERTEX_POINT('',#100475);
#28902=VERTEX_POINT('',#100477);
#28903=VERTEX_POINT('',#100481);
#28904=VERTEX_POINT('',#100483);
#28905=VERTEX_POINT('',#100487);
#28906=VERTEX_POINT('',#100489);
#28907=VERTEX_POINT('',#100493);
#28908=VERTEX_POINT('',#100495);
#28909=VERTEX_POINT('',#100499);
#28910=VERTEX_POINT('',#100501);
#28911=VERTEX_POINT('',#100505);
#28912=VERTEX_POINT('',#100507);
#28913=VERTEX_POINT('',#100511);
#28914=VERTEX_POINT('',#100513);
#28915=VERTEX_POINT('',#100517);
#28916=VERTEX_POINT('',#100519);
#28917=VERTEX_POINT('',#100523);
#28918=VERTEX_POINT('',#100525);
#28919=VERTEX_POINT('',#100529);
#28920=VERTEX_POINT('',#100531);
#28921=VERTEX_POINT('',#100535);
#28922=VERTEX_POINT('',#100537);
#28923=VERTEX_POINT('',#100541);
#28924=VERTEX_POINT('',#100543);
#28925=VERTEX_POINT('',#100547);
#28926=VERTEX_POINT('',#100549);
#28927=VERTEX_POINT('',#100553);
#28928=VERTEX_POINT('',#100555);
#28929=VERTEX_POINT('',#100559);
#28930=VERTEX_POINT('',#100561);
#28931=VERTEX_POINT('',#100565);
#28932=VERTEX_POINT('',#100567);
#28933=VERTEX_POINT('',#100571);
#28934=VERTEX_POINT('',#100573);
#28935=VERTEX_POINT('',#100577);
#28936=VERTEX_POINT('',#100579);
#28937=VERTEX_POINT('',#100583);
#28938=VERTEX_POINT('',#100585);
#28939=VERTEX_POINT('',#100589);
#28940=VERTEX_POINT('',#100591);
#28941=VERTEX_POINT('',#100595);
#28942=VERTEX_POINT('',#100597);
#28943=VERTEX_POINT('',#100601);
#28944=VERTEX_POINT('',#100603);
#28945=VERTEX_POINT('',#100607);
#28946=VERTEX_POINT('',#100609);
#28947=VERTEX_POINT('',#100613);
#28948=VERTEX_POINT('',#100615);
#28949=VERTEX_POINT('',#100619);
#28950=VERTEX_POINT('',#100621);
#28951=VERTEX_POINT('',#100625);
#28952=VERTEX_POINT('',#100627);
#28953=VERTEX_POINT('',#100631);
#28954=VERTEX_POINT('',#100633);
#28955=VERTEX_POINT('',#100637);
#28956=VERTEX_POINT('',#100639);
#28957=VERTEX_POINT('',#100643);
#28958=VERTEX_POINT('',#100645);
#28959=VERTEX_POINT('',#100649);
#28960=VERTEX_POINT('',#100651);
#28961=VERTEX_POINT('',#100655);
#28962=VERTEX_POINT('',#100657);
#28963=VERTEX_POINT('',#100661);
#28964=VERTEX_POINT('',#100663);
#28965=VERTEX_POINT('',#100667);
#28966=VERTEX_POINT('',#100669);
#28967=VERTEX_POINT('',#100673);
#28968=VERTEX_POINT('',#100675);
#28969=VERTEX_POINT('',#100679);
#28970=VERTEX_POINT('',#100681);
#28971=VERTEX_POINT('',#100685);
#28972=VERTEX_POINT('',#100687);
#28973=VERTEX_POINT('',#100691);
#28974=VERTEX_POINT('',#100693);
#28975=VERTEX_POINT('',#100697);
#28976=VERTEX_POINT('',#100699);
#28977=VERTEX_POINT('',#100703);
#28978=VERTEX_POINT('',#100705);
#28979=VERTEX_POINT('',#100709);
#28980=VERTEX_POINT('',#100711);
#28981=VERTEX_POINT('',#100715);
#28982=VERTEX_POINT('',#100717);
#28983=VERTEX_POINT('',#100721);
#28984=VERTEX_POINT('',#100723);
#28985=VERTEX_POINT('',#100727);
#28986=VERTEX_POINT('',#100729);
#28987=VERTEX_POINT('',#100733);
#28988=VERTEX_POINT('',#100735);
#28989=VERTEX_POINT('',#100739);
#28990=VERTEX_POINT('',#100741);
#28991=VERTEX_POINT('',#100745);
#28992=VERTEX_POINT('',#100747);
#28993=VERTEX_POINT('',#100751);
#28994=VERTEX_POINT('',#100753);
#28995=VERTEX_POINT('',#100757);
#28996=VERTEX_POINT('',#100759);
#28997=VERTEX_POINT('',#100763);
#28998=VERTEX_POINT('',#100765);
#28999=VERTEX_POINT('',#100769);
#29000=VERTEX_POINT('',#100771);
#29001=VERTEX_POINT('',#100775);
#29002=VERTEX_POINT('',#100777);
#29003=VERTEX_POINT('',#100781);
#29004=VERTEX_POINT('',#100783);
#29005=VERTEX_POINT('',#100787);
#29006=VERTEX_POINT('',#100789);
#29007=VERTEX_POINT('',#100793);
#29008=VERTEX_POINT('',#100795);
#29009=VERTEX_POINT('',#100799);
#29010=VERTEX_POINT('',#100801);
#29011=VERTEX_POINT('',#100805);
#29012=VERTEX_POINT('',#100807);
#29013=VERTEX_POINT('',#100811);
#29014=VERTEX_POINT('',#100813);
#29015=VERTEX_POINT('',#100817);
#29016=VERTEX_POINT('',#100819);
#29017=VERTEX_POINT('',#100823);
#29018=VERTEX_POINT('',#100825);
#29019=VERTEX_POINT('',#100829);
#29020=VERTEX_POINT('',#100831);
#29021=VERTEX_POINT('',#100835);
#29022=VERTEX_POINT('',#100837);
#29023=VERTEX_POINT('',#100841);
#29024=VERTEX_POINT('',#100843);
#29025=VERTEX_POINT('',#100847);
#29026=VERTEX_POINT('',#100849);
#29027=VERTEX_POINT('',#100853);
#29028=VERTEX_POINT('',#100855);
#29029=VERTEX_POINT('',#100859);
#29030=VERTEX_POINT('',#100861);
#29031=VERTEX_POINT('',#100865);
#29032=VERTEX_POINT('',#100867);
#29033=VERTEX_POINT('',#100871);
#29034=VERTEX_POINT('',#100873);
#29035=VERTEX_POINT('',#100877);
#29036=VERTEX_POINT('',#100879);
#29037=VERTEX_POINT('',#100883);
#29038=VERTEX_POINT('',#100885);
#29039=VERTEX_POINT('',#100889);
#29040=VERTEX_POINT('',#100891);
#29041=VERTEX_POINT('',#100895);
#29042=VERTEX_POINT('',#100897);
#29043=VERTEX_POINT('',#100901);
#29044=VERTEX_POINT('',#100903);
#29045=VERTEX_POINT('',#100907);
#29046=VERTEX_POINT('',#100909);
#29047=VERTEX_POINT('',#100913);
#29048=VERTEX_POINT('',#100915);
#29049=VERTEX_POINT('',#100919);
#29050=VERTEX_POINT('',#100921);
#29051=VERTEX_POINT('',#100925);
#29052=VERTEX_POINT('',#100927);
#29053=VERTEX_POINT('',#100931);
#29054=VERTEX_POINT('',#100933);
#29055=VERTEX_POINT('',#100937);
#29056=VERTEX_POINT('',#100939);
#29057=VERTEX_POINT('',#100943);
#29058=VERTEX_POINT('',#100945);
#29059=VERTEX_POINT('',#100949);
#29060=VERTEX_POINT('',#100951);
#29061=VERTEX_POINT('',#100955);
#29062=VERTEX_POINT('',#100957);
#29063=VERTEX_POINT('',#100961);
#29064=VERTEX_POINT('',#100963);
#29065=VERTEX_POINT('',#100967);
#29066=VERTEX_POINT('',#100969);
#29067=VERTEX_POINT('',#100973);
#29068=VERTEX_POINT('',#100975);
#29069=VERTEX_POINT('',#100979);
#29070=VERTEX_POINT('',#100981);
#29071=VERTEX_POINT('',#100985);
#29072=VERTEX_POINT('',#100987);
#29073=VERTEX_POINT('',#100991);
#29074=VERTEX_POINT('',#100993);
#29075=VERTEX_POINT('',#100997);
#29076=VERTEX_POINT('',#100999);
#29077=VERTEX_POINT('',#101003);
#29078=VERTEX_POINT('',#101005);
#29079=VERTEX_POINT('',#101009);
#29080=VERTEX_POINT('',#101011);
#29081=VERTEX_POINT('',#101015);
#29082=VERTEX_POINT('',#101017);
#29083=VERTEX_POINT('',#101021);
#29084=VERTEX_POINT('',#101023);
#29085=VERTEX_POINT('',#101027);
#29086=VERTEX_POINT('',#101029);
#29087=VERTEX_POINT('',#101033);
#29088=VERTEX_POINT('',#101035);
#29089=VERTEX_POINT('',#101039);
#29090=VERTEX_POINT('',#101041);
#29091=VERTEX_POINT('',#101045);
#29092=VERTEX_POINT('',#101047);
#29093=VERTEX_POINT('',#101051);
#29094=VERTEX_POINT('',#101053);
#29095=VERTEX_POINT('',#101057);
#29096=VERTEX_POINT('',#101059);
#29097=VERTEX_POINT('',#101063);
#29098=VERTEX_POINT('',#101065);
#29099=VERTEX_POINT('',#101069);
#29100=VERTEX_POINT('',#101071);
#29101=VERTEX_POINT('',#101075);
#29102=VERTEX_POINT('',#101077);
#29103=VERTEX_POINT('',#101081);
#29104=VERTEX_POINT('',#101083);
#29105=VERTEX_POINT('',#101087);
#29106=VERTEX_POINT('',#101089);
#29107=VERTEX_POINT('',#101093);
#29108=VERTEX_POINT('',#101095);
#29109=VERTEX_POINT('',#101099);
#29110=VERTEX_POINT('',#101101);
#29111=VERTEX_POINT('',#101105);
#29112=VERTEX_POINT('',#101107);
#29113=VERTEX_POINT('',#101111);
#29114=VERTEX_POINT('',#101113);
#29115=VERTEX_POINT('',#101117);
#29116=VERTEX_POINT('',#101119);
#29117=VERTEX_POINT('',#101123);
#29118=VERTEX_POINT('',#101125);
#29119=VERTEX_POINT('',#101129);
#29120=VERTEX_POINT('',#101131);
#29121=VERTEX_POINT('',#101135);
#29122=VERTEX_POINT('',#101137);
#29123=VERTEX_POINT('',#101141);
#29124=VERTEX_POINT('',#101143);
#29125=VERTEX_POINT('',#101147);
#29126=VERTEX_POINT('',#101149);
#29127=VERTEX_POINT('',#101153);
#29128=VERTEX_POINT('',#101155);
#29129=VERTEX_POINT('',#101159);
#29130=VERTEX_POINT('',#101161);
#29131=VERTEX_POINT('',#101165);
#29132=VERTEX_POINT('',#101167);
#29133=VERTEX_POINT('',#101171);
#29134=VERTEX_POINT('',#101173);
#29135=VERTEX_POINT('',#101177);
#29136=VERTEX_POINT('',#101179);
#29137=VERTEX_POINT('',#101183);
#29138=VERTEX_POINT('',#101185);
#29139=VERTEX_POINT('',#101189);
#29140=VERTEX_POINT('',#101191);
#29141=VERTEX_POINT('',#101195);
#29142=VERTEX_POINT('',#101197);
#29143=VERTEX_POINT('',#101201);
#29144=VERTEX_POINT('',#101203);
#29145=VERTEX_POINT('',#101207);
#29146=VERTEX_POINT('',#101209);
#29147=VERTEX_POINT('',#101213);
#29148=VERTEX_POINT('',#101215);
#29149=VERTEX_POINT('',#101219);
#29150=VERTEX_POINT('',#101221);
#29151=VERTEX_POINT('',#101225);
#29152=VERTEX_POINT('',#101227);
#29153=VERTEX_POINT('',#101231);
#29154=VERTEX_POINT('',#101233);
#29155=VERTEX_POINT('',#101237);
#29156=VERTEX_POINT('',#101239);
#29157=VERTEX_POINT('',#101243);
#29158=VERTEX_POINT('',#101245);
#29159=VERTEX_POINT('',#101249);
#29160=VERTEX_POINT('',#101251);
#29161=VERTEX_POINT('',#101255);
#29162=VERTEX_POINT('',#101257);
#29163=VERTEX_POINT('',#101261);
#29164=VERTEX_POINT('',#101263);
#29165=VERTEX_POINT('',#101267);
#29166=VERTEX_POINT('',#101269);
#29167=VERTEX_POINT('',#101273);
#29168=VERTEX_POINT('',#101275);
#29169=VERTEX_POINT('',#101279);
#29170=VERTEX_POINT('',#101281);
#29171=VERTEX_POINT('',#101285);
#29172=VERTEX_POINT('',#101287);
#29173=VERTEX_POINT('',#101291);
#29174=VERTEX_POINT('',#101293);
#29175=VERTEX_POINT('',#101297);
#29176=VERTEX_POINT('',#101299);
#29177=VERTEX_POINT('',#101303);
#29178=VERTEX_POINT('',#101305);
#29179=VERTEX_POINT('',#101309);
#29180=VERTEX_POINT('',#101311);
#29181=VERTEX_POINT('',#101315);
#29182=VERTEX_POINT('',#101317);
#29183=VERTEX_POINT('',#101321);
#29184=VERTEX_POINT('',#101323);
#29185=VERTEX_POINT('',#101327);
#29186=VERTEX_POINT('',#101329);
#29187=VERTEX_POINT('',#101333);
#29188=VERTEX_POINT('',#101335);
#29189=VERTEX_POINT('',#101339);
#29190=VERTEX_POINT('',#101341);
#29191=VERTEX_POINT('',#101345);
#29192=VERTEX_POINT('',#101347);
#29193=VERTEX_POINT('',#101351);
#29194=VERTEX_POINT('',#101353);
#29195=VERTEX_POINT('',#101357);
#29196=VERTEX_POINT('',#101359);
#29197=VERTEX_POINT('',#101363);
#29198=VERTEX_POINT('',#101365);
#29199=VERTEX_POINT('',#101369);
#29200=VERTEX_POINT('',#101371);
#29201=VERTEX_POINT('',#101375);
#29202=VERTEX_POINT('',#101377);
#29203=VERTEX_POINT('',#101381);
#29204=VERTEX_POINT('',#101383);
#29205=VERTEX_POINT('',#101387);
#29206=VERTEX_POINT('',#101389);
#29207=VERTEX_POINT('',#101393);
#29208=VERTEX_POINT('',#101395);
#29209=VERTEX_POINT('',#101399);
#29210=VERTEX_POINT('',#101401);
#29211=VERTEX_POINT('',#101405);
#29212=VERTEX_POINT('',#101407);
#29213=VERTEX_POINT('',#101411);
#29214=VERTEX_POINT('',#101413);
#29215=VERTEX_POINT('',#101417);
#29216=VERTEX_POINT('',#101419);
#29217=VERTEX_POINT('',#101423);
#29218=VERTEX_POINT('',#101425);
#29219=VERTEX_POINT('',#101429);
#29220=VERTEX_POINT('',#101431);
#29221=VERTEX_POINT('',#101435);
#29222=VERTEX_POINT('',#101437);
#29223=VERTEX_POINT('',#101441);
#29224=VERTEX_POINT('',#101443);
#29225=VERTEX_POINT('',#101447);
#29226=VERTEX_POINT('',#101449);
#29227=VERTEX_POINT('',#101453);
#29228=VERTEX_POINT('',#101455);
#29229=VERTEX_POINT('',#101459);
#29230=VERTEX_POINT('',#101461);
#29231=VERTEX_POINT('',#101465);
#29232=VERTEX_POINT('',#101467);
#29233=VERTEX_POINT('',#101471);
#29234=VERTEX_POINT('',#101473);
#29235=VERTEX_POINT('',#101477);
#29236=VERTEX_POINT('',#101479);
#29237=VERTEX_POINT('',#101483);
#29238=VERTEX_POINT('',#101485);
#29239=VERTEX_POINT('',#101489);
#29240=VERTEX_POINT('',#101491);
#29241=VERTEX_POINT('',#101495);
#29242=VERTEX_POINT('',#101497);
#29243=VERTEX_POINT('',#101501);
#29244=VERTEX_POINT('',#101503);
#29245=VERTEX_POINT('',#101507);
#29246=VERTEX_POINT('',#101509);
#29247=VERTEX_POINT('',#101513);
#29248=VERTEX_POINT('',#101515);
#29249=VERTEX_POINT('',#101519);
#29250=VERTEX_POINT('',#101521);
#29251=VERTEX_POINT('',#101525);
#29252=VERTEX_POINT('',#101527);
#29253=VERTEX_POINT('',#101531);
#29254=VERTEX_POINT('',#101533);
#29255=VERTEX_POINT('',#101537);
#29256=VERTEX_POINT('',#101539);
#29257=VERTEX_POINT('',#101543);
#29258=VERTEX_POINT('',#101545);
#29259=VERTEX_POINT('',#101549);
#29260=VERTEX_POINT('',#101551);
#29261=VERTEX_POINT('',#101555);
#29262=VERTEX_POINT('',#101557);
#29263=VERTEX_POINT('',#101561);
#29264=VERTEX_POINT('',#101563);
#29265=VERTEX_POINT('',#101567);
#29266=VERTEX_POINT('',#101569);
#29267=VERTEX_POINT('',#101573);
#29268=VERTEX_POINT('',#101575);
#29269=VERTEX_POINT('',#101579);
#29270=VERTEX_POINT('',#101581);
#29271=VERTEX_POINT('',#101585);
#29272=VERTEX_POINT('',#101587);
#29273=VERTEX_POINT('',#101591);
#29274=VERTEX_POINT('',#101593);
#29275=VERTEX_POINT('',#101597);
#29276=VERTEX_POINT('',#101599);
#29277=VERTEX_POINT('',#101603);
#29278=VERTEX_POINT('',#101605);
#29279=VERTEX_POINT('',#101609);
#29280=VERTEX_POINT('',#101611);
#29281=VERTEX_POINT('',#101615);
#29282=VERTEX_POINT('',#101617);
#29283=VERTEX_POINT('',#101621);
#29284=VERTEX_POINT('',#101623);
#29285=VERTEX_POINT('',#101627);
#29286=VERTEX_POINT('',#101629);
#29287=VERTEX_POINT('',#101633);
#29288=VERTEX_POINT('',#101635);
#29289=VERTEX_POINT('',#101639);
#29290=VERTEX_POINT('',#101641);
#29291=VERTEX_POINT('',#101645);
#29292=VERTEX_POINT('',#101647);
#29293=VERTEX_POINT('',#101651);
#29294=VERTEX_POINT('',#101653);
#29295=VERTEX_POINT('',#101657);
#29296=VERTEX_POINT('',#101659);
#29297=VERTEX_POINT('',#101663);
#29298=VERTEX_POINT('',#101665);
#29299=VERTEX_POINT('',#101669);
#29300=VERTEX_POINT('',#101671);
#29301=VERTEX_POINT('',#101675);
#29302=VERTEX_POINT('',#101677);
#29303=VERTEX_POINT('',#101681);
#29304=VERTEX_POINT('',#101683);
#29305=VERTEX_POINT('',#101687);
#29306=VERTEX_POINT('',#101689);
#29307=VERTEX_POINT('',#101693);
#29308=VERTEX_POINT('',#101695);
#29309=VERTEX_POINT('',#101699);
#29310=VERTEX_POINT('',#101701);
#29311=VERTEX_POINT('',#101705);
#29312=VERTEX_POINT('',#101707);
#29313=VERTEX_POINT('',#101711);
#29314=VERTEX_POINT('',#101713);
#29315=VERTEX_POINT('',#101717);
#29316=VERTEX_POINT('',#101719);
#29317=VERTEX_POINT('',#101723);
#29318=VERTEX_POINT('',#101725);
#29319=VERTEX_POINT('',#101729);
#29320=VERTEX_POINT('',#101731);
#29321=VERTEX_POINT('',#101735);
#29322=VERTEX_POINT('',#101737);
#29323=VERTEX_POINT('',#101741);
#29324=VERTEX_POINT('',#101743);
#29325=VERTEX_POINT('',#101747);
#29326=VERTEX_POINT('',#101749);
#29327=VERTEX_POINT('',#101753);
#29328=VERTEX_POINT('',#101755);
#29329=VERTEX_POINT('',#101759);
#29330=VERTEX_POINT('',#101761);
#29331=VERTEX_POINT('',#101765);
#29332=VERTEX_POINT('',#101767);
#29333=VERTEX_POINT('',#101771);
#29334=VERTEX_POINT('',#101773);
#29335=VERTEX_POINT('',#101777);
#29336=VERTEX_POINT('',#101779);
#29337=VERTEX_POINT('',#101783);
#29338=VERTEX_POINT('',#101785);
#29339=VERTEX_POINT('',#101789);
#29340=VERTEX_POINT('',#101791);
#29341=VERTEX_POINT('',#101795);
#29342=VERTEX_POINT('',#101797);
#29343=VERTEX_POINT('',#101801);
#29344=VERTEX_POINT('',#101803);
#29345=VERTEX_POINT('',#101807);
#29346=VERTEX_POINT('',#101809);
#29347=VERTEX_POINT('',#101813);
#29348=VERTEX_POINT('',#101815);
#29349=VERTEX_POINT('',#101819);
#29350=VERTEX_POINT('',#101821);
#29351=VERTEX_POINT('',#101825);
#29352=VERTEX_POINT('',#101827);
#29353=VERTEX_POINT('',#101831);
#29354=VERTEX_POINT('',#101833);
#29355=VERTEX_POINT('',#101837);
#29356=VERTEX_POINT('',#101839);
#29357=VERTEX_POINT('',#101843);
#29358=VERTEX_POINT('',#101845);
#29359=VERTEX_POINT('',#101849);
#29360=VERTEX_POINT('',#101851);
#29361=VERTEX_POINT('',#101855);
#29362=VERTEX_POINT('',#101857);
#29363=VERTEX_POINT('',#101861);
#29364=VERTEX_POINT('',#101863);
#29365=VERTEX_POINT('',#101867);
#29366=VERTEX_POINT('',#101869);
#29367=VERTEX_POINT('',#101873);
#29368=VERTEX_POINT('',#101875);
#29369=VERTEX_POINT('',#101879);
#29370=VERTEX_POINT('',#101881);
#29371=VERTEX_POINT('',#101885);
#29372=VERTEX_POINT('',#101887);
#29373=VERTEX_POINT('',#101891);
#29374=VERTEX_POINT('',#101893);
#29375=VERTEX_POINT('',#101897);
#29376=VERTEX_POINT('',#101899);
#29377=VERTEX_POINT('',#101903);
#29378=VERTEX_POINT('',#101905);
#29379=VERTEX_POINT('',#101909);
#29380=VERTEX_POINT('',#101911);
#29381=VERTEX_POINT('',#101915);
#29382=VERTEX_POINT('',#101917);
#29383=VERTEX_POINT('',#101921);
#29384=VERTEX_POINT('',#101923);
#29385=VERTEX_POINT('',#101927);
#29386=VERTEX_POINT('',#101929);
#29387=VERTEX_POINT('',#101933);
#29388=VERTEX_POINT('',#101935);
#29389=VERTEX_POINT('',#101939);
#29390=VERTEX_POINT('',#101941);
#29391=VERTEX_POINT('',#101945);
#29392=VERTEX_POINT('',#101947);
#29393=VERTEX_POINT('',#101951);
#29394=VERTEX_POINT('',#101953);
#29395=VERTEX_POINT('',#101957);
#29396=VERTEX_POINT('',#101959);
#29397=VERTEX_POINT('',#101963);
#29398=VERTEX_POINT('',#101965);
#29399=VERTEX_POINT('',#101969);
#29400=VERTEX_POINT('',#101971);
#29401=VERTEX_POINT('',#101975);
#29402=VERTEX_POINT('',#101977);
#29403=VERTEX_POINT('',#101981);
#29404=VERTEX_POINT('',#101983);
#29405=VERTEX_POINT('',#101987);
#29406=VERTEX_POINT('',#101989);
#29407=VERTEX_POINT('',#101993);
#29408=VERTEX_POINT('',#101995);
#29409=VERTEX_POINT('',#101999);
#29410=VERTEX_POINT('',#102001);
#29411=VERTEX_POINT('',#102005);
#29412=VERTEX_POINT('',#102007);
#29413=VERTEX_POINT('',#102020);
#29414=VERTEX_POINT('',#102021);
#29415=VERTEX_POINT('',#102023);
#29416=VERTEX_POINT('',#102025);
#29417=VERTEX_POINT('',#102029);
#29418=VERTEX_POINT('',#102031);
#29419=VERTEX_POINT('',#102035);
#29420=VERTEX_POINT('',#102037);
#29421=VERTEX_POINT('',#102041);
#29422=VERTEX_POINT('',#102043);
#29423=VERTEX_POINT('',#102045);
#29424=VERTEX_POINT('',#102047);
#29425=VERTEX_POINT('',#102051);
#29426=VERTEX_POINT('',#102053);
#29427=VERTEX_POINT('',#102057);
#29428=VERTEX_POINT('',#102059);
#29429=VERTEX_POINT('',#102063);
#29430=VERTEX_POINT('',#102065);
#29431=VERTEX_POINT('',#102067);
#29432=VERTEX_POINT('',#102069);
#29433=VERTEX_POINT('',#102071);
#29434=VERTEX_POINT('',#102075);
#29435=VERTEX_POINT('',#102077);
#29436=VERTEX_POINT('',#102081);
#29437=VERTEX_POINT('',#102083);
#29438=VERTEX_POINT('',#102087);
#29439=VERTEX_POINT('',#102090);
#29440=VERTEX_POINT('',#102094);
#29441=VERTEX_POINT('',#102096);
#29442=VERTEX_POINT('',#102098);
#29443=VERTEX_POINT('',#102102);
#29444=VERTEX_POINT('',#102106);
#29445=VERTEX_POINT('',#102108);
#29446=VERTEX_POINT('',#102117);
#29447=VERTEX_POINT('',#102125);
#29448=VERTEX_POINT('',#102126);
#29449=VERTEX_POINT('',#102128);
#29450=VERTEX_POINT('',#102130);
#29451=VERTEX_POINT('',#102134);
#29452=VERTEX_POINT('',#102136);
#29453=VERTEX_POINT('',#102140);
#29454=VERTEX_POINT('',#102144);
#29455=VERTEX_POINT('',#102148);
#29456=VERTEX_POINT('',#102149);
#29457=VERTEX_POINT('',#102151);
#29458=VERTEX_POINT('',#102153);
#29459=VERTEX_POINT('',#102157);
#29460=VERTEX_POINT('',#102159);
#29461=VERTEX_POINT('',#102163);
#29462=VERTEX_POINT('',#102167);
#29463=VERTEX_POINT('',#102171);
#29464=VERTEX_POINT('',#102172);
#29465=VERTEX_POINT('',#102174);
#29466=VERTEX_POINT('',#102176);
#29467=VERTEX_POINT('',#102180);
#29468=VERTEX_POINT('',#102182);
#29469=VERTEX_POINT('',#102186);
#29470=VERTEX_POINT('',#102190);
#29471=VERTEX_POINT('',#102194);
#29472=VERTEX_POINT('',#102195);
#29473=VERTEX_POINT('',#102197);
#29474=VERTEX_POINT('',#102199);
#29475=VERTEX_POINT('',#102203);
#29476=VERTEX_POINT('',#102205);
#29477=VERTEX_POINT('',#102209);
#29478=VERTEX_POINT('',#102213);
#29479=VERTEX_POINT('',#102217);
#29480=VERTEX_POINT('',#102218);
#29481=VERTEX_POINT('',#102220);
#29482=VERTEX_POINT('',#102222);
#29483=VERTEX_POINT('',#102226);
#29484=VERTEX_POINT('',#102228);
#29485=VERTEX_POINT('',#102232);
#29486=VERTEX_POINT('',#102236);
#29487=VERTEX_POINT('',#102240);
#29488=VERTEX_POINT('',#102241);
#29489=VERTEX_POINT('',#102243);
#29490=VERTEX_POINT('',#102245);
#29491=VERTEX_POINT('',#102249);
#29492=VERTEX_POINT('',#102251);
#29493=VERTEX_POINT('',#102255);
#29494=VERTEX_POINT('',#102259);
#29495=VERTEX_POINT('',#102263);
#29496=VERTEX_POINT('',#102264);
#29497=VERTEX_POINT('',#102266);
#29498=VERTEX_POINT('',#102268);
#29499=VERTEX_POINT('',#102272);
#29500=VERTEX_POINT('',#102274);
#29501=VERTEX_POINT('',#102278);
#29502=VERTEX_POINT('',#102282);
#29503=VERTEX_POINT('',#102286);
#29504=VERTEX_POINT('',#102287);
#29505=VERTEX_POINT('',#102289);
#29506=VERTEX_POINT('',#102291);
#29507=VERTEX_POINT('',#102295);
#29508=VERTEX_POINT('',#102297);
#29509=VERTEX_POINT('',#102301);
#29510=VERTEX_POINT('',#102305);
#29511=VERTEX_POINT('',#102309);
#29512=VERTEX_POINT('',#102310);
#29513=VERTEX_POINT('',#102314);
#29514=VERTEX_POINT('',#102316);
#29515=VERTEX_POINT('',#102320);
#29516=VERTEX_POINT('',#102321);
#29517=VERTEX_POINT('',#102325);
#29518=VERTEX_POINT('',#102327);
#29519=VERTEX_POINT('',#102334);
#29520=VERTEX_POINT('',#102335);
#29521=VERTEX_POINT('',#102337);
#29522=VERTEX_POINT('',#102339);
#29523=VERTEX_POINT('',#102343);
#29524=VERTEX_POINT('',#102345);
#29525=VERTEX_POINT('',#102349);
#29526=VERTEX_POINT('',#102353);
#29527=VERTEX_POINT('',#102357);
#29528=VERTEX_POINT('',#102358);
#29529=VERTEX_POINT('',#102360);
#29530=VERTEX_POINT('',#102362);
#29531=VERTEX_POINT('',#102366);
#29532=VERTEX_POINT('',#102368);
#29533=VERTEX_POINT('',#102372);
#29534=VERTEX_POINT('',#102376);
#29535=VERTEX_POINT('',#102380);
#29536=VERTEX_POINT('',#102381);
#29537=VERTEX_POINT('',#102383);
#29538=VERTEX_POINT('',#102385);
#29539=VERTEX_POINT('',#102389);
#29540=VERTEX_POINT('',#102391);
#29541=VERTEX_POINT('',#102395);
#29542=VERTEX_POINT('',#102399);
#29543=VERTEX_POINT('',#102403);
#29544=VERTEX_POINT('',#102404);
#29545=VERTEX_POINT('',#102406);
#29546=VERTEX_POINT('',#102408);
#29547=VERTEX_POINT('',#102412);
#29548=VERTEX_POINT('',#102414);
#29549=VERTEX_POINT('',#102418);
#29550=VERTEX_POINT('',#102422);
#29551=VERTEX_POINT('',#102426);
#29552=VERTEX_POINT('',#102427);
#29553=VERTEX_POINT('',#102429);
#29554=VERTEX_POINT('',#102431);
#29555=VERTEX_POINT('',#102435);
#29556=VERTEX_POINT('',#102437);
#29557=VERTEX_POINT('',#102441);
#29558=VERTEX_POINT('',#102445);
#29559=VERTEX_POINT('',#102449);
#29560=VERTEX_POINT('',#102450);
#29561=VERTEX_POINT('',#102452);
#29562=VERTEX_POINT('',#102454);
#29563=VERTEX_POINT('',#102458);
#29564=VERTEX_POINT('',#102460);
#29565=VERTEX_POINT('',#102464);
#29566=VERTEX_POINT('',#102468);
#29567=VERTEX_POINT('',#102472);
#29568=VERTEX_POINT('',#102473);
#29569=VERTEX_POINT('',#102475);
#29570=VERTEX_POINT('',#102477);
#29571=VERTEX_POINT('',#102481);
#29572=VERTEX_POINT('',#102483);
#29573=VERTEX_POINT('',#102487);
#29574=VERTEX_POINT('',#102491);
#29575=VERTEX_POINT('',#102495);
#29576=VERTEX_POINT('',#102496);
#29577=VERTEX_POINT('',#102500);
#29578=VERTEX_POINT('',#102502);
#29579=VERTEX_POINT('',#102506);
#29580=VERTEX_POINT('',#102507);
#29581=VERTEX_POINT('',#102511);
#29582=VERTEX_POINT('',#102513);
#29583=VERTEX_POINT('',#102520);
#29584=VERTEX_POINT('',#102524);
#29585=VERTEX_POINT('',#102543);
#29586=VERTEX_POINT('',#102547);
#29587=VERTEX_POINT('',#102549);
#29588=VERTEX_POINT('',#102551);
#29589=VERTEX_POINT('',#102553);
#29590=VERTEX_POINT('',#102555);
#29591=VERTEX_POINT('',#102562);
#29592=VERTEX_POINT('',#102564);
#29593=VERTEX_POINT('',#102568);
#29594=VERTEX_POINT('',#102571);
#29595=VERTEX_POINT('',#102573);
#29596=VERTEX_POINT('',#102579);
#29597=VERTEX_POINT('',#102583);
#29598=VERTEX_POINT('',#102585);
#29599=VERTEX_POINT('',#102589);
#29600=VERTEX_POINT('',#102591);
#29601=VERTEX_POINT('',#102595);
#29602=VERTEX_POINT('',#102598);
#29603=VERTEX_POINT('',#102604);
#29604=VERTEX_POINT('',#102606);
#29605=VERTEX_POINT('',#102610);
#29606=VERTEX_POINT('',#102611);
#29607=VERTEX_POINT('',#102616);
#29608=VERTEX_POINT('',#102620);
#29609=VERTEX_POINT('',#102630);
#29610=VERTEX_POINT('',#102631);
#29611=VERTEX_POINT('',#102633);
#29612=VERTEX_POINT('',#102644);
#29613=VERTEX_POINT('',#102654);
#29614=VERTEX_POINT('',#102655);
#29615=VERTEX_POINT('',#102702);
#29616=VERTEX_POINT('',#102703);
#29617=VERTEX_POINT('',#102750);
#29618=VERTEX_POINT('',#102751);
#29619=VERTEX_POINT('',#102804);
#29620=VERTEX_POINT('',#102805);
#29621=VERTEX_POINT('',#102852);
#29622=VERTEX_POINT('',#102853);
#29623=VERTEX_POINT('',#102906);
#29624=VERTEX_POINT('',#102907);
#29625=VERTEX_POINT('',#102954);
#29626=VERTEX_POINT('',#102955);
#29627=VERTEX_POINT('',#103002);
#29628=VERTEX_POINT('',#103003);
#29629=VERTEX_POINT('',#103056);
#29630=VERTEX_POINT('',#103057);
#29631=VERTEX_POINT('',#103104);
#29632=VERTEX_POINT('',#103105);
#29633=VERTEX_POINT('',#103152);
#29634=VERTEX_POINT('',#103153);
#29635=VERTEX_POINT('',#103155);
#29636=VERTEX_POINT('',#103165);
#29637=VERTEX_POINT('',#103176);
#29638=VERTEX_POINT('',#103177);
#29639=VERTEX_POINT('',#103200);
#29640=VERTEX_POINT('',#103201);
#29641=VERTEX_POINT('',#103225);
#29642=VERTEX_POINT('',#103226);
#29643=VERTEX_POINT('',#103250);
#29644=VERTEX_POINT('',#103251);
#29645=VERTEX_POINT('',#103274);
#29646=VERTEX_POINT('',#103275);
#29647=VERTEX_POINT('',#103299);
#29648=VERTEX_POINT('',#103300);
#29649=VERTEX_POINT('',#103324);
#29650=VERTEX_POINT('',#103325);
#29651=VERTEX_POINT('',#103349);
#29652=VERTEX_POINT('',#103350);
#29653=VERTEX_POINT('',#103374);
#29654=VERTEX_POINT('',#103375);
#29655=VERTEX_POINT('',#103398);
#29656=VERTEX_POINT('',#103484);
#29657=VERTEX_POINT('',#103486);
#29658=VERTEX_POINT('',#103871);
#29659=VERTEX_POINT('',#103967);
#29660=VERTEX_POINT('',#103969);
#29661=VERTEX_POINT('',#104362);
#29662=VERTEX_POINT('',#104366);
#29663=VERTEX_POINT('',#104371);
#29664=VERTEX_POINT('',#104372);
#29665=VERTEX_POINT('',#104374);
#29666=VERTEX_POINT('',#104376);
#29667=VERTEX_POINT('',#104378);
#29668=VERTEX_POINT('',#104382);
#29669=VERTEX_POINT('',#104388);
#29670=VERTEX_POINT('',#104389);
#29671=VERTEX_POINT('',#104391);
#29672=VERTEX_POINT('',#104395);
#29673=VERTEX_POINT('',#104397);
#29674=VERTEX_POINT('',#104401);
#29675=VERTEX_POINT('',#104406);
#29676=VERTEX_POINT('',#104420);
#29677=VERTEX_POINT('',#104426);
#29678=VERTEX_POINT('',#104427);
#29679=VERTEX_POINT('',#104429);
#29680=VERTEX_POINT('',#104440);
#29681=VERTEX_POINT('',#104450);
#29682=VERTEX_POINT('',#104451);
#29683=VERTEX_POINT('',#104498);
#29684=VERTEX_POINT('',#104499);
#29685=VERTEX_POINT('',#104546);
#29686=VERTEX_POINT('',#104547);
#29687=VERTEX_POINT('',#104600);
#29688=VERTEX_POINT('',#104601);
#29689=VERTEX_POINT('',#104648);
#29690=VERTEX_POINT('',#104649);
#29691=VERTEX_POINT('',#104651);
#29692=VERTEX_POINT('',#104661);
#29693=VERTEX_POINT('',#104672);
#29694=VERTEX_POINT('',#104673);
#29695=VERTEX_POINT('',#104697);
#29696=VERTEX_POINT('',#104698);
#29697=VERTEX_POINT('',#104722);
#29698=VERTEX_POINT('',#104723);
#29699=VERTEX_POINT('',#104746);
#29700=VERTEX_POINT('',#104832);
#29701=VERTEX_POINT('',#104834);
#29702=VERTEX_POINT('',#105064);
#29703=VERTEX_POINT('',#105160);
#29704=VERTEX_POINT('',#105163);
#29705=VERTEX_POINT('',#105400);
#29706=VERTEX_POINT('',#105402);
#29707=VERTEX_POINT('',#105404);
#29708=VERTEX_POINT('',#105408);
#29709=VERTEX_POINT('',#105410);
#29710=VERTEX_POINT('',#105414);
#29711=VERTEX_POINT('',#105418);
#29712=VERTEX_POINT('',#105420);
#29713=VERTEX_POINT('',#105424);
#29714=VERTEX_POINT('',#105428);
#29715=VERTEX_POINT('',#105430);
#29716=VERTEX_POINT('',#105434);
#29717=VERTEX_POINT('',#105438);
#29718=VERTEX_POINT('',#105440);
#29719=VERTEX_POINT('',#105444);
#29720=VERTEX_POINT('',#105448);
#29721=VERTEX_POINT('',#105450);
#29722=VERTEX_POINT('',#105454);
#29723=VERTEX_POINT('',#105458);
#29724=VERTEX_POINT('',#105464);
#29725=VERTEX_POINT('',#105466);
#29726=VERTEX_POINT('',#105470);
#29727=VERTEX_POINT('',#105472);
#29728=VERTEX_POINT('',#105476);
#29729=VERTEX_POINT('',#105478);
#29730=VERTEX_POINT('',#105482);
#29731=VERTEX_POINT('',#105484);
#29732=VERTEX_POINT('',#105488);
#29733=VERTEX_POINT('',#105490);
#29734=VERTEX_POINT('',#105494);
#29735=VERTEX_POINT('',#105496);
#29736=VERTEX_POINT('',#105501);
#29737=VERTEX_POINT('',#105503);
#29738=VERTEX_POINT('',#105508);
#29739=VERTEX_POINT('',#105513);
#29740=VERTEX_POINT('',#105526);
#29741=VERTEX_POINT('',#105536);
#29742=VERTEX_POINT('',#105543);
#29743=VERTEX_POINT('',#105551);
#29744=VERTEX_POINT('',#105558);
#29745=VERTEX_POINT('',#105564);
#29746=VERTEX_POINT('',#105565);
#29747=VERTEX_POINT('',#105567);
#29748=VERTEX_POINT('',#105578);
#29749=VERTEX_POINT('',#105588);
#29750=VERTEX_POINT('',#105589);
#29751=VERTEX_POINT('',#105636);
#29752=VERTEX_POINT('',#105637);
#29753=VERTEX_POINT('',#105684);
#29754=VERTEX_POINT('',#105685);
#29755=VERTEX_POINT('',#105687);
#29756=VERTEX_POINT('',#105737);
#29757=VERTEX_POINT('',#105738);
#29758=VERTEX_POINT('',#105740);
#29759=VERTEX_POINT('',#105749);
#29760=VERTEX_POINT('',#105758);
#29761=VERTEX_POINT('',#105759);
#29762=VERTEX_POINT('',#105783);
#29763=VERTEX_POINT('',#105784);
#29764=VERTEX_POINT('',#105880);
#29765=VERTEX_POINT('',#106066);
#29766=VERTEX_POINT('',#106150);
#29767=VERTEX_POINT('',#106153);
#29768=VERTEX_POINT('',#106345);
#29769=VERTEX_POINT('',#106347);
#29770=VERTEX_POINT('',#106349);
#29771=VERTEX_POINT('',#106353);
#29772=VERTEX_POINT('',#106355);
#29773=VERTEX_POINT('',#106359);
#29774=VERTEX_POINT('',#106363);
#29775=VERTEX_POINT('',#106365);
#29776=VERTEX_POINT('',#106369);
#29777=VERTEX_POINT('',#106373);
#29778=VERTEX_POINT('',#106375);
#29779=VERTEX_POINT('',#106379);
#29780=VERTEX_POINT('',#106383);
#29781=VERTEX_POINT('',#106385);
#29782=VERTEX_POINT('',#106389);
#29783=VERTEX_POINT('',#106393);
#29784=VERTEX_POINT('',#106395);
#29785=VERTEX_POINT('',#106399);
#29786=VERTEX_POINT('',#106403);
#29787=VERTEX_POINT('',#106409);
#29788=VERTEX_POINT('',#106411);
#29789=VERTEX_POINT('',#106415);
#29790=VERTEX_POINT('',#106417);
#29791=VERTEX_POINT('',#106421);
#29792=VERTEX_POINT('',#106423);
#29793=VERTEX_POINT('',#106427);
#29794=VERTEX_POINT('',#106429);
#29795=VERTEX_POINT('',#106433);
#29796=VERTEX_POINT('',#106435);
#29797=VERTEX_POINT('',#106439);
#29798=VERTEX_POINT('',#106441);
#29799=VERTEX_POINT('',#106446);
#29800=VERTEX_POINT('',#106448);
#29801=VERTEX_POINT('',#106453);
#29802=VERTEX_POINT('',#106458);
#29803=VERTEX_POINT('',#106471);
#29804=VERTEX_POINT('',#106481);
#29805=VERTEX_POINT('',#106488);
#29806=VERTEX_POINT('',#106496);
#29807=VERTEX_POINT('',#106503);
#29808=VERTEX_POINT('',#106509);
#29809=VERTEX_POINT('',#106510);
#29810=VERTEX_POINT('',#106512);
#29811=VERTEX_POINT('',#106523);
#29812=VERTEX_POINT('',#106533);
#29813=VERTEX_POINT('',#106534);
#29814=VERTEX_POINT('',#106581);
#29815=VERTEX_POINT('',#106582);
#29816=VERTEX_POINT('',#106629);
#29817=VERTEX_POINT('',#106630);
#29818=VERTEX_POINT('',#106683);
#29819=VERTEX_POINT('',#106684);
#29820=VERTEX_POINT('',#106731);
#29821=VERTEX_POINT('',#106732);
#29822=VERTEX_POINT('',#106779);
#29823=VERTEX_POINT('',#106780);
#29824=VERTEX_POINT('',#106833);
#29825=VERTEX_POINT('',#106834);
#29826=VERTEX_POINT('',#106881);
#29827=VERTEX_POINT('',#106882);
#29828=VERTEX_POINT('',#106929);
#29829=VERTEX_POINT('',#106930);
#29830=VERTEX_POINT('',#106983);
#29831=VERTEX_POINT('',#106984);
#29832=VERTEX_POINT('',#107031);
#29833=VERTEX_POINT('',#107032);
#29834=VERTEX_POINT('',#107034);
#29835=VERTEX_POINT('',#107044);
#29836=VERTEX_POINT('',#107055);
#29837=VERTEX_POINT('',#107056);
#29838=VERTEX_POINT('',#107080);
#29839=VERTEX_POINT('',#107081);
#29840=VERTEX_POINT('',#107105);
#29841=VERTEX_POINT('',#107106);
#29842=VERTEX_POINT('',#107129);
#29843=VERTEX_POINT('',#107130);
#29844=VERTEX_POINT('',#107154);
#29845=VERTEX_POINT('',#107155);
#29846=VERTEX_POINT('',#107179);
#29847=VERTEX_POINT('',#107180);
#29848=VERTEX_POINT('',#107203);
#29849=VERTEX_POINT('',#107204);
#29850=VERTEX_POINT('',#107228);
#29851=VERTEX_POINT('',#107229);
#29852=VERTEX_POINT('',#107253);
#29853=VERTEX_POINT('',#107254);
#29854=VERTEX_POINT('',#107277);
#29855=VERTEX_POINT('',#107363);
#29856=VERTEX_POINT('',#107365);
#29857=VERTEX_POINT('',#107747);
#29858=VERTEX_POINT('',#107843);
#29859=VERTEX_POINT('',#107846);
#29860=VERTEX_POINT('',#108235);
#29861=VERTEX_POINT('',#108237);
#29862=VERTEX_POINT('',#108239);
#29863=VERTEX_POINT('',#108243);
#29864=VERTEX_POINT('',#108245);
#29865=VERTEX_POINT('',#108249);
#29866=VERTEX_POINT('',#108253);
#29867=VERTEX_POINT('',#108255);
#29868=VERTEX_POINT('',#108259);
#29869=VERTEX_POINT('',#108263);
#29870=VERTEX_POINT('',#108265);
#29871=VERTEX_POINT('',#108269);
#29872=VERTEX_POINT('',#108273);
#29873=VERTEX_POINT('',#108275);
#29874=VERTEX_POINT('',#108279);
#29875=VERTEX_POINT('',#108283);
#29876=VERTEX_POINT('',#108285);
#29877=VERTEX_POINT('',#108289);
#29878=VERTEX_POINT('',#108293);
#29879=VERTEX_POINT('',#108299);
#29880=VERTEX_POINT('',#108301);
#29881=VERTEX_POINT('',#108305);
#29882=VERTEX_POINT('',#108307);
#29883=VERTEX_POINT('',#108311);
#29884=VERTEX_POINT('',#108313);
#29885=VERTEX_POINT('',#108317);
#29886=VERTEX_POINT('',#108319);
#29887=VERTEX_POINT('',#108323);
#29888=VERTEX_POINT('',#108325);
#29889=VERTEX_POINT('',#108329);
#29890=VERTEX_POINT('',#108331);
#29891=VERTEX_POINT('',#108336);
#29892=VERTEX_POINT('',#108338);
#29893=VERTEX_POINT('',#108343);
#29894=VERTEX_POINT('',#108348);
#29895=VERTEX_POINT('',#108361);
#29896=VERTEX_POINT('',#108371);
#29897=VERTEX_POINT('',#108378);
#29898=VERTEX_POINT('',#108386);
#29899=VERTEX_POINT('',#108393);
#29900=VERTEX_POINT('',#108399);
#29901=VERTEX_POINT('',#108400);
#29902=VERTEX_POINT('',#108402);
#29903=VERTEX_POINT('',#108413);
#29904=VERTEX_POINT('',#108423);
#29905=VERTEX_POINT('',#108424);
#29906=VERTEX_POINT('',#108471);
#29907=VERTEX_POINT('',#108472);
#29908=VERTEX_POINT('',#108519);
#29909=VERTEX_POINT('',#108520);
#29910=VERTEX_POINT('',#108573);
#29911=VERTEX_POINT('',#108574);
#29912=VERTEX_POINT('',#108621);
#29913=VERTEX_POINT('',#108622);
#29914=VERTEX_POINT('',#108669);
#29915=VERTEX_POINT('',#108670);
#29916=VERTEX_POINT('',#108672);
#29917=VERTEX_POINT('',#108680);
#29918=VERTEX_POINT('',#108681);
#29919=VERTEX_POINT('',#108693);
#29920=VERTEX_POINT('',#108706);
#29921=VERTEX_POINT('',#108707);
#29922=VERTEX_POINT('',#108730);
#29923=VERTEX_POINT('',#108731);
#29924=VERTEX_POINT('',#108755);
#29925=VERTEX_POINT('',#108756);
#29926=VERTEX_POINT('',#108780);
#29927=VERTEX_POINT('',#108781);
#29928=VERTEX_POINT('',#108804);
#29929=VERTEX_POINT('',#108878);
#29930=VERTEX_POINT('',#108880);
#29931=VERTEX_POINT('',#109142);
#29932=VERTEX_POINT('',#109226);
#29933=VERTEX_POINT('',#109229);
#29934=VERTEX_POINT('',#109498);
#29935=VERTEX_POINT('',#109500);
#29936=VERTEX_POINT('',#109502);
#29937=VERTEX_POINT('',#109506);
#29938=VERTEX_POINT('',#109508);
#29939=VERTEX_POINT('',#109512);
#29940=VERTEX_POINT('',#109516);
#29941=VERTEX_POINT('',#109518);
#29942=VERTEX_POINT('',#109522);
#29943=VERTEX_POINT('',#109526);
#29944=VERTEX_POINT('',#109528);
#29945=VERTEX_POINT('',#109532);
#29946=VERTEX_POINT('',#109536);
#29947=VERTEX_POINT('',#109538);
#29948=VERTEX_POINT('',#109542);
#29949=VERTEX_POINT('',#109546);
#29950=VERTEX_POINT('',#109548);
#29951=VERTEX_POINT('',#109552);
#29952=VERTEX_POINT('',#109556);
#29953=VERTEX_POINT('',#109562);
#29954=VERTEX_POINT('',#109564);
#29955=VERTEX_POINT('',#109568);
#29956=VERTEX_POINT('',#109570);
#29957=VERTEX_POINT('',#109574);
#29958=VERTEX_POINT('',#109576);
#29959=VERTEX_POINT('',#109580);
#29960=VERTEX_POINT('',#109582);
#29961=VERTEX_POINT('',#109586);
#29962=VERTEX_POINT('',#109588);
#29963=VERTEX_POINT('',#109592);
#29964=VERTEX_POINT('',#109594);
#29965=VERTEX_POINT('',#109599);
#29966=VERTEX_POINT('',#109601);
#29967=VERTEX_POINT('',#109606);
#29968=VERTEX_POINT('',#109611);
#29969=VERTEX_POINT('',#109624);
#29970=VERTEX_POINT('',#109634);
#29971=VERTEX_POINT('',#109641);
#29972=VERTEX_POINT('',#109649);
#29973=VERTEX_POINT('',#109656);
#29974=VERTEX_POINT('',#109662);
#29975=VERTEX_POINT('',#109663);
#29976=VERTEX_POINT('',#109665);
#29977=VERTEX_POINT('',#109676);
#29978=VERTEX_POINT('',#109686);
#29979=VERTEX_POINT('',#109687);
#29980=VERTEX_POINT('',#109734);
#29981=VERTEX_POINT('',#109735);
#29982=VERTEX_POINT('',#109782);
#29983=VERTEX_POINT('',#109783);
#29984=VERTEX_POINT('',#109836);
#29985=VERTEX_POINT('',#109837);
#29986=VERTEX_POINT('',#109884);
#29987=VERTEX_POINT('',#109885);
#29988=VERTEX_POINT('',#109932);
#29989=VERTEX_POINT('',#109933);
#29990=VERTEX_POINT('',#109986);
#29991=VERTEX_POINT('',#109987);
#29992=VERTEX_POINT('',#109989);
#29993=VERTEX_POINT('',#110033);
#29994=VERTEX_POINT('',#110034);
#29995=VERTEX_POINT('',#110036);
#29996=VERTEX_POINT('',#110044);
#29997=VERTEX_POINT('',#110053);
#29998=VERTEX_POINT('',#110054);
#29999=VERTEX_POINT('',#110078);
#30000=VERTEX_POINT('',#110079);
#30001=VERTEX_POINT('',#110103);
#30002=VERTEX_POINT('',#110104);
#30003=VERTEX_POINT('',#110127);
#30004=VERTEX_POINT('',#110128);
#30005=VERTEX_POINT('',#110152);
#30006=VERTEX_POINT('',#110153);
#30007=VERTEX_POINT('',#110177);
#30008=VERTEX_POINT('',#110178);
#30009=VERTEX_POINT('',#110274);
#30010=VERTEX_POINT('',#110560);
#30011=VERTEX_POINT('',#110644);
#30012=VERTEX_POINT('',#110647);
#30013=VERTEX_POINT('',#110939);
#30014=VERTEX_POINT('',#110940);
#30015=VERTEX_POINT('',#110942);
#30016=VERTEX_POINT('',#110944);
#30017=VERTEX_POINT('',#110948);
#30018=VERTEX_POINT('',#110950);
#30019=VERTEX_POINT('',#110954);
#30020=VERTEX_POINT('',#110956);
#30021=VERTEX_POINT('',#110960);
#30022=VERTEX_POINT('',#110962);
#30023=VERTEX_POINT('',#110966);
#30024=VERTEX_POINT('',#110968);
#30025=VERTEX_POINT('',#110976);
#30026=VERTEX_POINT('',#110983);
#30027=VERTEX_POINT('',#110989);
#30028=VERTEX_POINT('',#110990);
#30029=VERTEX_POINT('',#110992);
#30030=VERTEX_POINT('',#111003);
#30031=VERTEX_POINT('',#111013);
#30032=VERTEX_POINT('',#111014);
#30033=VERTEX_POINT('',#111061);
#30034=VERTEX_POINT('',#111062);
#30035=VERTEX_POINT('',#111109);
#30036=VERTEX_POINT('',#111110);
#30037=VERTEX_POINT('',#111163);
#30038=VERTEX_POINT('',#111164);
#30039=VERTEX_POINT('',#111211);
#30040=VERTEX_POINT('',#111212);
#30041=VERTEX_POINT('',#111259);
#30042=VERTEX_POINT('',#111260);
#30043=VERTEX_POINT('',#111313);
#30044=VERTEX_POINT('',#111314);
#30045=VERTEX_POINT('',#111361);
#30046=VERTEX_POINT('',#111362);
#30047=VERTEX_POINT('',#111409);
#30048=VERTEX_POINT('',#111410);
#30049=VERTEX_POINT('',#111457);
#30050=VERTEX_POINT('',#111458);
#30051=VERTEX_POINT('',#111511);
#30052=VERTEX_POINT('',#111512);
#30053=VERTEX_POINT('',#111559);
#30054=VERTEX_POINT('',#111560);
#30055=VERTEX_POINT('',#111607);
#30056=VERTEX_POINT('',#111608);
#30057=VERTEX_POINT('',#111610);
#30058=VERTEX_POINT('',#111619);
#30059=VERTEX_POINT('',#111629);
#30060=VERTEX_POINT('',#111630);
#30061=VERTEX_POINT('',#111653);
#30062=VERTEX_POINT('',#111654);
#30063=VERTEX_POINT('',#111678);
#30064=VERTEX_POINT('',#111679);
#30065=VERTEX_POINT('',#111703);
#30066=VERTEX_POINT('',#111704);
#30067=VERTEX_POINT('',#111727);
#30068=VERTEX_POINT('',#111728);
#30069=VERTEX_POINT('',#111751);
#30070=VERTEX_POINT('',#111752);
#30071=VERTEX_POINT('',#111776);
#30072=VERTEX_POINT('',#111777);
#30073=VERTEX_POINT('',#111801);
#30074=VERTEX_POINT('',#111802);
#30075=VERTEX_POINT('',#111825);
#30076=VERTEX_POINT('',#111826);
#30077=VERTEX_POINT('',#111850);
#30078=VERTEX_POINT('',#111851);
#30079=VERTEX_POINT('',#111875);
#30080=VERTEX_POINT('',#111876);
#30081=VERTEX_POINT('',#111899);
#30082=VERTEX_POINT('',#111982);
#30083=VERTEX_POINT('',#111984);
#30084=VERTEX_POINT('',#112407);
#30085=VERTEX_POINT('',#112500);
#30086=VERTEX_POINT('',#112502);
#30087=VERTEX_POINT('',#112933);
#30088=VERTEX_POINT('',#112939);
#30089=VERTEX_POINT('',#112942);
#30090=VERTEX_POINT('',#112947);
#30091=VERTEX_POINT('',#112948);
#30092=VERTEX_POINT('',#112952);
#30093=VERTEX_POINT('',#112954);
#30094=VERTEX_POINT('',#112958);
#30095=VERTEX_POINT('',#112962);
#30096=VERTEX_POINT('',#112968);
#30097=VERTEX_POINT('',#112970);
#30098=VERTEX_POINT('',#112972);
#30099=VERTEX_POINT('',#112974);
#30100=VERTEX_POINT('',#112976);
#30101=VERTEX_POINT('',#112978);
#30102=VERTEX_POINT('',#112980);
#30103=VERTEX_POINT('',#112982);
#30104=VERTEX_POINT('',#112984);
#30105=VERTEX_POINT('',#112986);
#30106=VERTEX_POINT('',#112988);
#30107=VERTEX_POINT('',#112990);
#30108=VERTEX_POINT('',#112992);
#30109=VERTEX_POINT('',#112994);
#30110=VERTEX_POINT('',#112996);
#30111=VERTEX_POINT('',#112998);
#30112=VERTEX_POINT('',#113000);
#30113=VERTEX_POINT('',#113002);
#30114=VERTEX_POINT('',#113004);
#30115=VERTEX_POINT('',#113006);
#30116=VERTEX_POINT('',#113008);
#30117=VERTEX_POINT('',#113010);
#30118=VERTEX_POINT('',#113012);
#30119=VERTEX_POINT('',#113014);
#30120=VERTEX_POINT('',#113016);
#30121=VERTEX_POINT('',#113018);
#30122=VERTEX_POINT('',#113020);
#30123=VERTEX_POINT('',#113022);
#30124=VERTEX_POINT('',#113024);
#30125=VERTEX_POINT('',#113026);
#30126=VERTEX_POINT('',#113028);
#30127=VERTEX_POINT('',#113030);
#30128=VERTEX_POINT('',#113032);
#30129=VERTEX_POINT('',#113034);
#30130=VERTEX_POINT('',#113036);
#30131=VERTEX_POINT('',#113038);
#30132=VERTEX_POINT('',#113040);
#30133=VERTEX_POINT('',#113042);
#30134=VERTEX_POINT('',#113044);
#30135=VERTEX_POINT('',#113046);
#30136=VERTEX_POINT('',#113048);
#30137=VERTEX_POINT('',#113050);
#30138=VERTEX_POINT('',#113052);
#30139=VERTEX_POINT('',#113054);
#30140=VERTEX_POINT('',#113056);
#30141=VERTEX_POINT('',#113058);
#30142=VERTEX_POINT('',#113060);
#30143=VERTEX_POINT('',#113062);
#30144=VERTEX_POINT('',#113064);
#30145=VERTEX_POINT('',#113066);
#30146=VERTEX_POINT('',#113068);
#30147=VERTEX_POINT('',#113070);
#30148=VERTEX_POINT('',#113072);
#30149=VERTEX_POINT('',#113074);
#30150=VERTEX_POINT('',#113076);
#30151=VERTEX_POINT('',#113078);
#30152=VERTEX_POINT('',#113080);
#30153=VERTEX_POINT('',#113082);
#30154=VERTEX_POINT('',#113084);
#30155=VERTEX_POINT('',#113086);
#30156=VERTEX_POINT('',#113088);
#30157=VERTEX_POINT('',#113090);
#30158=VERTEX_POINT('',#113092);
#30159=VERTEX_POINT('',#113094);
#30160=VERTEX_POINT('',#113096);
#30161=VERTEX_POINT('',#113098);
#30162=VERTEX_POINT('',#113100);
#30163=VERTEX_POINT('',#113102);
#30164=VERTEX_POINT('',#113104);
#30165=VERTEX_POINT('',#113106);
#30166=VERTEX_POINT('',#113108);
#30167=VERTEX_POINT('',#113110);
#30168=VERTEX_POINT('',#113112);
#30169=VERTEX_POINT('',#113114);
#30170=VERTEX_POINT('',#113116);
#30171=VERTEX_POINT('',#113118);
#30172=VERTEX_POINT('',#113120);
#30173=VERTEX_POINT('',#113123);
#30174=VERTEX_POINT('',#113125);
#30175=VERTEX_POINT('',#113127);
#30176=VERTEX_POINT('',#113129);
#30177=VERTEX_POINT('',#113131);
#30178=VERTEX_POINT('',#113133);
#30179=VERTEX_POINT('',#113135);
#30180=VERTEX_POINT('',#113137);
#30181=VERTEX_POINT('',#113139);
#30182=VERTEX_POINT('',#113141);
#30183=VERTEX_POINT('',#113143);
#30184=VERTEX_POINT('',#113145);
#30185=VERTEX_POINT('',#113147);
#30186=VERTEX_POINT('',#113149);
#30187=VERTEX_POINT('',#113151);
#30188=VERTEX_POINT('',#113153);
#30189=VERTEX_POINT('',#113155);
#30190=VERTEX_POINT('',#113157);
#30191=VERTEX_POINT('',#113159);
#30192=VERTEX_POINT('',#113161);
#30193=VERTEX_POINT('',#113163);
#30194=VERTEX_POINT('',#113165);
#30195=VERTEX_POINT('',#113167);
#30196=VERTEX_POINT('',#113169);
#30197=VERTEX_POINT('',#113171);
#30198=VERTEX_POINT('',#113173);
#30199=VERTEX_POINT('',#113175);
#30200=VERTEX_POINT('',#113177);
#30201=VERTEX_POINT('',#113179);
#30202=VERTEX_POINT('',#113181);
#30203=VERTEX_POINT('',#113183);
#30204=VERTEX_POINT('',#113185);
#30205=VERTEX_POINT('',#113187);
#30206=VERTEX_POINT('',#113189);
#30207=VERTEX_POINT('',#113191);
#30208=VERTEX_POINT('',#113193);
#30209=VERTEX_POINT('',#113195);
#30210=VERTEX_POINT('',#113197);
#30211=VERTEX_POINT('',#113199);
#30212=VERTEX_POINT('',#113201);
#30213=VERTEX_POINT('',#113203);
#30214=VERTEX_POINT('',#113205);
#30215=VERTEX_POINT('',#113207);
#30216=VERTEX_POINT('',#113209);
#30217=VERTEX_POINT('',#113211);
#30218=VERTEX_POINT('',#113213);
#30219=VERTEX_POINT('',#113215);
#30220=VERTEX_POINT('',#113217);
#30221=VERTEX_POINT('',#113219);
#30222=VERTEX_POINT('',#113221);
#30223=VERTEX_POINT('',#113223);
#30224=VERTEX_POINT('',#113225);
#30225=VERTEX_POINT('',#113227);
#30226=VERTEX_POINT('',#113229);
#30227=VERTEX_POINT('',#113231);
#30228=VERTEX_POINT('',#113233);
#30229=VERTEX_POINT('',#113235);
#30230=VERTEX_POINT('',#113237);
#30231=VERTEX_POINT('',#113239);
#30232=VERTEX_POINT('',#113241);
#30233=VERTEX_POINT('',#113243);
#30234=VERTEX_POINT('',#113245);
#30235=VERTEX_POINT('',#113247);
#30236=VERTEX_POINT('',#113249);
#30237=VERTEX_POINT('',#113251);
#30238=VERTEX_POINT('',#113253);
#30239=VERTEX_POINT('',#113257);
#30240=VERTEX_POINT('',#113261);
#30241=VERTEX_POINT('',#113271);
#30242=VERTEX_POINT('',#113275);
#30243=VERTEX_POINT('',#113285);
#30244=VERTEX_POINT('',#113289);
#30245=VERTEX_POINT('',#113299);
#30246=VERTEX_POINT('',#113303);
#30247=VERTEX_POINT('',#113313);
#30248=VERTEX_POINT('',#113317);
#30249=VERTEX_POINT('',#113327);
#30250=VERTEX_POINT('',#113331);
#30251=VERTEX_POINT('',#113341);
#30252=VERTEX_POINT('',#113345);
#30253=VERTEX_POINT('',#113355);
#30254=VERTEX_POINT('',#113359);
#30255=VERTEX_POINT('',#113369);
#30256=VERTEX_POINT('',#113373);
#30257=VERTEX_POINT('',#113383);
#30258=VERTEX_POINT('',#113387);
#30259=VERTEX_POINT('',#113397);
#30260=VERTEX_POINT('',#113401);
#30261=VERTEX_POINT('',#113411);
#30262=VERTEX_POINT('',#113415);
#30263=VERTEX_POINT('',#113425);
#30264=VERTEX_POINT('',#113429);
#30265=VERTEX_POINT('',#113439);
#30266=VERTEX_POINT('',#113443);
#30267=VERTEX_POINT('',#113453);
#30268=VERTEX_POINT('',#113457);
#30269=VERTEX_POINT('',#113467);
#30270=VERTEX_POINT('',#113471);
#30271=VERTEX_POINT('',#113481);
#30272=VERTEX_POINT('',#113485);
#30273=VERTEX_POINT('',#113495);
#30274=VERTEX_POINT('',#113499);
#30275=VERTEX_POINT('',#113509);
#30276=VERTEX_POINT('',#113513);
#30277=VERTEX_POINT('',#113523);
#30278=VERTEX_POINT('',#113527);
#30279=VERTEX_POINT('',#113537);
#30280=VERTEX_POINT('',#113541);
#30281=VERTEX_POINT('',#113551);
#30282=VERTEX_POINT('',#113555);
#30283=VERTEX_POINT('',#113565);
#30284=VERTEX_POINT('',#113569);
#30285=VERTEX_POINT('',#113579);
#30286=VERTEX_POINT('',#113583);
#30287=VERTEX_POINT('',#113593);
#30288=VERTEX_POINT('',#113597);
#30289=VERTEX_POINT('',#113607);
#30290=VERTEX_POINT('',#113611);
#30291=VERTEX_POINT('',#113621);
#30292=VERTEX_POINT('',#113625);
#30293=VERTEX_POINT('',#113635);
#30294=VERTEX_POINT('',#113639);
#30295=VERTEX_POINT('',#113649);
#30296=VERTEX_POINT('',#113653);
#30297=VERTEX_POINT('',#113663);
#30298=VERTEX_POINT('',#113667);
#30299=VERTEX_POINT('',#113677);
#30300=VERTEX_POINT('',#113681);
#30301=VERTEX_POINT('',#113691);
#30302=VERTEX_POINT('',#113695);
#30303=VERTEX_POINT('',#113705);
#30304=VERTEX_POINT('',#113709);
#30305=VERTEX_POINT('',#113719);
#30306=VERTEX_POINT('',#113723);
#30307=VERTEX_POINT('',#113733);
#30308=VERTEX_POINT('',#113737);
#30309=VERTEX_POINT('',#113749);
#30310=VERTEX_POINT('',#113753);
#30311=VERTEX_POINT('',#113756);
#30312=VERTEX_POINT('',#113758);
#30313=VERTEX_POINT('',#113762);
#30314=VERTEX_POINT('',#113764);
#30315=VERTEX_POINT('',#113768);
#30316=VERTEX_POINT('',#113772);
#30317=VERTEX_POINT('',#113774);
#30318=VERTEX_POINT('',#113778);
#30319=VERTEX_POINT('',#113782);
#30320=VERTEX_POINT('',#113784);
#30321=VERTEX_POINT('',#113788);
#30322=VERTEX_POINT('',#113792);
#30323=VERTEX_POINT('',#113794);
#30324=VERTEX_POINT('',#113798);
#30325=VERTEX_POINT('',#113802);
#30326=VERTEX_POINT('',#113804);
#30327=VERTEX_POINT('',#113808);
#30328=VERTEX_POINT('',#113812);
#30329=VERTEX_POINT('',#113818);
#30330=VERTEX_POINT('',#113820);
#30331=VERTEX_POINT('',#113824);
#30332=VERTEX_POINT('',#113826);
#30333=VERTEX_POINT('',#113830);
#30334=VERTEX_POINT('',#113832);
#30335=VERTEX_POINT('',#113836);
#30336=VERTEX_POINT('',#113838);
#30337=VERTEX_POINT('',#113842);
#30338=VERTEX_POINT('',#113844);
#30339=VERTEX_POINT('',#113848);
#30340=VERTEX_POINT('',#113850);
#30341=VERTEX_POINT('',#113855);
#30342=VERTEX_POINT('',#113857);
#30343=VERTEX_POINT('',#113862);
#30344=VERTEX_POINT('',#113867);
#30345=VERTEX_POINT('',#113880);
#30346=VERTEX_POINT('',#113890);
#30347=VERTEX_POINT('',#113897);
#30348=VERTEX_POINT('',#113906);
#30349=VERTEX_POINT('',#113909);
#30350=VERTEX_POINT('',#113913);
#30351=VERTEX_POINT('',#113917);
#30352=EDGE_CURVE('',#24623,#24624,#22944,.T.);
#30353=EDGE_CURVE('',#24623,#24625,#10876,.T.);
#30354=EDGE_CURVE('',#24625,#24626,#22945,.T.);
#30355=EDGE_CURVE('',#24624,#24626,#10877,.T.);
#30356=EDGE_CURVE('',#24627,#24623,#22946,.T.);
#30357=EDGE_CURVE('',#24627,#24628,#10878,.T.);
#30358=EDGE_CURVE('',#24628,#24625,#22947,.T.);
#30359=EDGE_CURVE('',#24629,#24627,#22948,.T.);
#30360=EDGE_CURVE('',#24629,#24630,#10879,.T.);
#30361=EDGE_CURVE('',#24630,#24628,#22949,.T.);
#30362=EDGE_CURVE('',#24631,#24629,#22950,.T.);
#30363=EDGE_CURVE('',#24631,#24632,#10880,.T.);
#30364=EDGE_CURVE('',#24632,#24630,#22951,.T.);
#30365=EDGE_CURVE('',#24633,#24631,#22952,.T.);
#30366=EDGE_CURVE('',#24633,#24634,#10881,.T.);
#30367=EDGE_CURVE('',#24634,#24632,#22953,.T.);
#30368=EDGE_CURVE('',#24635,#24633,#22954,.T.);
#30369=EDGE_CURVE('',#24635,#24636,#10882,.T.);
#30370=EDGE_CURVE('',#24636,#24634,#22955,.T.);
#30371=EDGE_CURVE('',#24637,#24635,#22956,.T.);
#30372=EDGE_CURVE('',#24637,#24638,#10883,.T.);
#30373=EDGE_CURVE('',#24638,#24636,#22957,.T.);
#30374=EDGE_CURVE('',#24624,#24637,#22958,.T.);
#30375=EDGE_CURVE('',#24626,#24638,#22959,.T.);
#30376=EDGE_CURVE('',#24639,#24640,#22960,.T.);
#30377=EDGE_CURVE('',#24639,#24641,#10884,.T.);
#30378=EDGE_CURVE('',#24641,#24642,#22961,.T.);
#30379=EDGE_CURVE('',#24640,#24642,#10885,.T.);
#30380=EDGE_CURVE('',#24643,#24639,#22962,.T.);
#30381=EDGE_CURVE('',#24643,#24644,#10886,.T.);
#30382=EDGE_CURVE('',#24644,#24641,#22963,.T.);
#30383=EDGE_CURVE('',#24645,#24643,#22964,.T.);
#30384=EDGE_CURVE('',#24645,#24646,#10887,.T.);
#30385=EDGE_CURVE('',#24646,#24644,#22965,.T.);
#30386=EDGE_CURVE('',#24647,#24645,#22966,.T.);
#30387=EDGE_CURVE('',#24647,#24648,#10888,.T.);
#30388=EDGE_CURVE('',#24648,#24646,#22967,.T.);
#30389=EDGE_CURVE('',#24649,#24647,#22968,.T.);
#30390=EDGE_CURVE('',#24649,#24650,#10889,.T.);
#30391=EDGE_CURVE('',#24650,#24648,#22969,.T.);
#30392=EDGE_CURVE('',#24651,#24649,#22970,.T.);
#30393=EDGE_CURVE('',#24651,#24652,#10890,.T.);
#30394=EDGE_CURVE('',#24652,#24650,#22971,.T.);
#30395=EDGE_CURVE('',#24653,#24651,#22972,.T.);
#30396=EDGE_CURVE('',#24653,#24654,#10891,.T.);
#30397=EDGE_CURVE('',#24654,#24652,#22973,.T.);
#30398=EDGE_CURVE('',#24655,#24653,#22974,.T.);
#30399=EDGE_CURVE('',#24655,#24656,#10892,.T.);
#30400=EDGE_CURVE('',#24656,#24654,#22975,.T.);
#30401=EDGE_CURVE('',#24657,#24655,#22976,.T.);
#30402=EDGE_CURVE('',#24657,#24658,#10893,.T.);
#30403=EDGE_CURVE('',#24658,#24656,#22977,.T.);
#30404=EDGE_CURVE('',#24659,#24657,#22978,.T.);
#30405=EDGE_CURVE('',#24659,#24660,#10894,.T.);
#30406=EDGE_CURVE('',#24660,#24658,#22979,.T.);
#30407=EDGE_CURVE('',#24661,#24659,#22980,.T.);
#30408=EDGE_CURVE('',#24661,#24662,#10895,.T.);
#30409=EDGE_CURVE('',#24662,#24660,#22981,.T.);
#30410=EDGE_CURVE('',#24640,#24661,#22982,.T.);
#30411=EDGE_CURVE('',#24642,#24662,#22983,.T.);
#30412=EDGE_CURVE('',#24663,#24664,#22984,.T.);
#30413=EDGE_CURVE('',#24663,#24665,#10896,.T.);
#30414=EDGE_CURVE('',#24665,#24666,#22985,.T.);
#30415=EDGE_CURVE('',#24664,#24666,#10897,.T.);
#30416=EDGE_CURVE('',#24667,#24663,#22986,.T.);
#30417=EDGE_CURVE('',#24667,#24668,#10898,.T.);
#30418=EDGE_CURVE('',#24668,#24665,#22987,.T.);
#30419=EDGE_CURVE('',#24669,#24667,#22988,.T.);
#30420=EDGE_CURVE('',#24669,#24670,#10899,.T.);
#30421=EDGE_CURVE('',#24670,#24668,#22989,.T.);
#30422=EDGE_CURVE('',#24671,#24669,#22990,.T.);
#30423=EDGE_CURVE('',#24671,#24672,#10900,.T.);
#30424=EDGE_CURVE('',#24672,#24670,#22991,.T.);
#30425=EDGE_CURVE('',#24673,#24671,#22992,.T.);
#30426=EDGE_CURVE('',#24673,#24674,#10901,.T.);
#30427=EDGE_CURVE('',#24674,#24672,#22993,.T.);
#30428=EDGE_CURVE('',#24675,#24673,#22994,.T.);
#30429=EDGE_CURVE('',#24675,#24676,#10902,.T.);
#30430=EDGE_CURVE('',#24676,#24674,#22995,.T.);
#30431=EDGE_CURVE('',#24677,#24675,#22996,.T.);
#30432=EDGE_CURVE('',#24677,#24678,#10903,.T.);
#30433=EDGE_CURVE('',#24678,#24676,#22997,.T.);
#30434=EDGE_CURVE('',#24664,#24677,#22998,.T.);
#30435=EDGE_CURVE('',#24666,#24678,#22999,.T.);
#30436=EDGE_CURVE('',#24679,#24680,#23000,.T.);
#30437=EDGE_CURVE('',#24679,#24681,#10904,.T.);
#30438=EDGE_CURVE('',#24681,#24682,#23001,.T.);
#30439=EDGE_CURVE('',#24680,#24682,#10905,.T.);
#30440=EDGE_CURVE('',#24683,#24679,#23002,.T.);
#30441=EDGE_CURVE('',#24683,#24684,#10906,.T.);
#30442=EDGE_CURVE('',#24684,#24681,#23003,.T.);
#30443=EDGE_CURVE('',#24685,#24683,#23004,.T.);
#30444=EDGE_CURVE('',#24685,#24686,#10907,.T.);
#30445=EDGE_CURVE('',#24686,#24684,#23005,.T.);
#30446=EDGE_CURVE('',#24687,#24685,#23006,.T.);
#30447=EDGE_CURVE('',#24687,#24688,#10908,.T.);
#30448=EDGE_CURVE('',#24688,#24686,#23007,.T.);
#30449=EDGE_CURVE('',#24689,#24687,#23008,.T.);
#30450=EDGE_CURVE('',#24689,#24690,#10909,.T.);
#30451=EDGE_CURVE('',#24690,#24688,#23009,.T.);
#30452=EDGE_CURVE('',#24691,#24689,#23010,.T.);
#30453=EDGE_CURVE('',#24691,#24692,#10910,.T.);
#30454=EDGE_CURVE('',#24692,#24690,#23011,.T.);
#30455=EDGE_CURVE('',#24693,#24691,#23012,.T.);
#30456=EDGE_CURVE('',#24693,#24694,#10911,.T.);
#30457=EDGE_CURVE('',#24694,#24692,#23013,.T.);
#30458=EDGE_CURVE('',#24695,#24693,#23014,.T.);
#30459=EDGE_CURVE('',#24695,#24696,#10912,.T.);
#30460=EDGE_CURVE('',#24696,#24694,#23015,.T.);
#30461=EDGE_CURVE('',#24697,#24695,#23016,.T.);
#30462=EDGE_CURVE('',#24697,#24698,#10913,.T.);
#30463=EDGE_CURVE('',#24698,#24696,#23017,.T.);
#30464=EDGE_CURVE('',#24699,#24697,#23018,.T.);
#30465=EDGE_CURVE('',#24699,#24700,#10914,.T.);
#30466=EDGE_CURVE('',#24700,#24698,#23019,.T.);
#30467=EDGE_CURVE('',#24701,#24699,#23020,.T.);
#30468=EDGE_CURVE('',#24701,#24702,#10915,.T.);
#30469=EDGE_CURVE('',#24702,#24700,#23021,.T.);
#30470=EDGE_CURVE('',#24703,#24701,#23022,.T.);
#30471=EDGE_CURVE('',#24703,#24704,#10916,.T.);
#30472=EDGE_CURVE('',#24704,#24702,#23023,.T.);
#30473=EDGE_CURVE('',#24705,#24703,#23024,.T.);
#30474=EDGE_CURVE('',#24705,#24706,#10917,.T.);
#30475=EDGE_CURVE('',#24706,#24704,#23025,.T.);
#30476=EDGE_CURVE('',#24707,#24705,#23026,.T.);
#30477=EDGE_CURVE('',#24707,#24708,#10918,.T.);
#30478=EDGE_CURVE('',#24708,#24706,#23027,.T.);
#30479=EDGE_CURVE('',#24709,#24707,#23028,.T.);
#30480=EDGE_CURVE('',#24709,#24710,#10919,.T.);
#30481=EDGE_CURVE('',#24710,#24708,#23029,.T.);
#30482=EDGE_CURVE('',#24711,#24709,#23030,.T.);
#30483=EDGE_CURVE('',#24711,#24712,#10920,.T.);
#30484=EDGE_CURVE('',#24712,#24710,#23031,.T.);
#30485=EDGE_CURVE('',#24713,#24711,#23032,.T.);
#30486=EDGE_CURVE('',#24713,#24714,#10921,.T.);
#30487=EDGE_CURVE('',#24714,#24712,#23033,.T.);
#30488=EDGE_CURVE('',#24715,#24713,#23034,.T.);
#30489=EDGE_CURVE('',#24715,#24716,#10922,.T.);
#30490=EDGE_CURVE('',#24716,#24714,#23035,.T.);
#30491=EDGE_CURVE('',#24717,#24715,#23036,.T.);
#30492=EDGE_CURVE('',#24717,#24718,#10923,.T.);
#30493=EDGE_CURVE('',#24718,#24716,#23037,.T.);
#30494=EDGE_CURVE('',#24719,#24717,#23038,.T.);
#30495=EDGE_CURVE('',#24719,#24720,#10924,.T.);
#30496=EDGE_CURVE('',#24720,#24718,#23039,.T.);
#30497=EDGE_CURVE('',#24721,#24719,#10925,.T.);
#30498=EDGE_CURVE('',#24721,#24722,#10926,.T.);
#30499=EDGE_CURVE('',#24722,#24720,#10927,.T.);
#30500=EDGE_CURVE('',#24680,#24721,#23040,.T.);
#30501=EDGE_CURVE('',#24682,#24722,#23041,.T.);
#30502=EDGE_CURVE('',#24723,#24724,#23042,.T.);
#30503=EDGE_CURVE('',#24723,#24725,#10928,.T.);
#30504=EDGE_CURVE('',#24725,#24726,#23043,.T.);
#30505=EDGE_CURVE('',#24724,#24726,#10929,.T.);
#30506=EDGE_CURVE('',#24727,#24723,#23044,.T.);
#30507=EDGE_CURVE('',#24727,#24728,#10930,.T.);
#30508=EDGE_CURVE('',#24728,#24725,#23045,.T.);
#30509=EDGE_CURVE('',#24729,#24727,#23046,.T.);
#30510=EDGE_CURVE('',#24729,#24730,#10931,.T.);
#30511=EDGE_CURVE('',#24730,#24728,#23047,.T.);
#30512=EDGE_CURVE('',#24731,#24729,#23048,.T.);
#30513=EDGE_CURVE('',#24731,#24732,#10932,.T.);
#30514=EDGE_CURVE('',#24732,#24730,#23049,.T.);
#30515=EDGE_CURVE('',#24733,#24731,#23050,.T.);
#30516=EDGE_CURVE('',#24733,#24734,#10933,.T.);
#30517=EDGE_CURVE('',#24734,#24732,#23051,.T.);
#30518=EDGE_CURVE('',#24735,#24733,#23052,.T.);
#30519=EDGE_CURVE('',#24735,#24736,#10934,.T.);
#30520=EDGE_CURVE('',#24736,#24734,#23053,.T.);
#30521=EDGE_CURVE('',#24737,#24735,#23054,.T.);
#30522=EDGE_CURVE('',#24737,#24738,#10935,.T.);
#30523=EDGE_CURVE('',#24738,#24736,#23055,.T.);
#30524=EDGE_CURVE('',#24724,#24737,#23056,.T.);
#30525=EDGE_CURVE('',#24726,#24738,#23057,.T.);
#30526=EDGE_CURVE('',#24739,#24740,#23058,.T.);
#30527=EDGE_CURVE('',#24739,#24741,#10936,.T.);
#30528=EDGE_CURVE('',#24741,#24742,#23059,.T.);
#30529=EDGE_CURVE('',#24740,#24742,#10937,.T.);
#30530=EDGE_CURVE('',#24743,#24739,#23060,.T.);
#30531=EDGE_CURVE('',#24743,#24744,#10938,.T.);
#30532=EDGE_CURVE('',#24744,#24741,#23061,.T.);
#30533=EDGE_CURVE('',#24745,#24743,#23062,.T.);
#30534=EDGE_CURVE('',#24745,#24746,#10939,.T.);
#30535=EDGE_CURVE('',#24746,#24744,#23063,.T.);
#30536=EDGE_CURVE('',#24747,#24745,#23064,.T.);
#30537=EDGE_CURVE('',#24747,#24748,#10940,.T.);
#30538=EDGE_CURVE('',#24748,#24746,#23065,.T.);
#30539=EDGE_CURVE('',#24749,#24747,#23066,.T.);
#30540=EDGE_CURVE('',#24749,#24750,#10941,.T.);
#30541=EDGE_CURVE('',#24750,#24748,#23067,.T.);
#30542=EDGE_CURVE('',#24751,#24749,#23068,.T.);
#30543=EDGE_CURVE('',#24751,#24752,#10942,.T.);
#30544=EDGE_CURVE('',#24752,#24750,#23069,.T.);
#30545=EDGE_CURVE('',#24753,#24751,#23070,.T.);
#30546=EDGE_CURVE('',#24753,#24754,#10943,.T.);
#30547=EDGE_CURVE('',#24754,#24752,#23071,.T.);
#30548=EDGE_CURVE('',#24755,#24753,#23072,.T.);
#30549=EDGE_CURVE('',#24755,#24756,#10944,.T.);
#30550=EDGE_CURVE('',#24756,#24754,#23073,.T.);
#30551=EDGE_CURVE('',#24757,#24755,#23074,.T.);
#30552=EDGE_CURVE('',#24757,#24758,#10945,.T.);
#30553=EDGE_CURVE('',#24758,#24756,#23075,.T.);
#30554=EDGE_CURVE('',#24759,#24757,#23076,.T.);
#30555=EDGE_CURVE('',#24759,#24760,#10946,.T.);
#30556=EDGE_CURVE('',#24760,#24758,#23077,.T.);
#30557=EDGE_CURVE('',#24761,#24759,#23078,.T.);
#30558=EDGE_CURVE('',#24761,#24762,#10947,.T.);
#30559=EDGE_CURVE('',#24762,#24760,#23079,.T.);
#30560=EDGE_CURVE('',#24740,#24761,#23080,.T.);
#30561=EDGE_CURVE('',#24742,#24762,#23081,.T.);
#30562=EDGE_CURVE('',#24763,#24764,#23082,.T.);
#30563=EDGE_CURVE('',#24763,#24765,#10948,.T.);
#30564=EDGE_CURVE('',#24765,#24766,#23083,.T.);
#30565=EDGE_CURVE('',#24764,#24766,#10949,.T.);
#30566=EDGE_CURVE('',#24767,#24763,#23084,.T.);
#30567=EDGE_CURVE('',#24767,#24768,#10950,.T.);
#30568=EDGE_CURVE('',#24768,#24765,#23085,.T.);
#30569=EDGE_CURVE('',#24769,#24767,#23086,.T.);
#30570=EDGE_CURVE('',#24769,#24770,#10951,.T.);
#30571=EDGE_CURVE('',#24770,#24768,#23087,.T.);
#30572=EDGE_CURVE('',#24771,#24769,#23088,.T.);
#30573=EDGE_CURVE('',#24771,#24772,#10952,.T.);
#30574=EDGE_CURVE('',#24772,#24770,#23089,.T.);
#30575=EDGE_CURVE('',#24773,#24771,#23090,.T.);
#30576=EDGE_CURVE('',#24773,#24774,#10953,.T.);
#30577=EDGE_CURVE('',#24774,#24772,#23091,.T.);
#30578=EDGE_CURVE('',#24775,#24773,#23092,.T.);
#30579=EDGE_CURVE('',#24775,#24776,#10954,.T.);
#30580=EDGE_CURVE('',#24776,#24774,#23093,.T.);
#30581=EDGE_CURVE('',#24777,#24775,#23094,.T.);
#30582=EDGE_CURVE('',#24777,#24778,#10955,.T.);
#30583=EDGE_CURVE('',#24778,#24776,#23095,.T.);
#30584=EDGE_CURVE('',#24764,#24777,#23096,.T.);
#30585=EDGE_CURVE('',#24766,#24778,#23097,.T.);
#30586=EDGE_CURVE('',#24779,#24780,#23098,.T.);
#30587=EDGE_CURVE('',#24779,#24781,#10956,.T.);
#30588=EDGE_CURVE('',#24781,#24782,#23099,.T.);
#30589=EDGE_CURVE('',#24780,#24782,#10957,.T.);
#30590=EDGE_CURVE('',#24783,#24779,#23100,.T.);
#30591=EDGE_CURVE('',#24783,#24784,#10958,.T.);
#30592=EDGE_CURVE('',#24784,#24781,#23101,.T.);
#30593=EDGE_CURVE('',#24785,#24783,#23102,.T.);
#30594=EDGE_CURVE('',#24785,#24786,#10959,.T.);
#30595=EDGE_CURVE('',#24786,#24784,#23103,.T.);
#30596=EDGE_CURVE('',#24787,#24785,#23104,.T.);
#30597=EDGE_CURVE('',#24787,#24788,#10960,.T.);
#30598=EDGE_CURVE('',#24788,#24786,#23105,.T.);
#30599=EDGE_CURVE('',#24789,#24787,#23106,.T.);
#30600=EDGE_CURVE('',#24789,#24790,#10961,.T.);
#30601=EDGE_CURVE('',#24790,#24788,#23107,.T.);
#30602=EDGE_CURVE('',#24791,#24789,#23108,.T.);
#30603=EDGE_CURVE('',#24791,#24792,#10962,.T.);
#30604=EDGE_CURVE('',#24792,#24790,#23109,.T.);
#30605=EDGE_CURVE('',#24793,#24791,#23110,.T.);
#30606=EDGE_CURVE('',#24793,#24794,#10963,.T.);
#30607=EDGE_CURVE('',#24794,#24792,#23111,.T.);
#30608=EDGE_CURVE('',#24795,#24793,#23112,.T.);
#30609=EDGE_CURVE('',#24795,#24796,#10964,.T.);
#30610=EDGE_CURVE('',#24796,#24794,#23113,.T.);
#30611=EDGE_CURVE('',#24780,#24795,#23114,.T.);
#30612=EDGE_CURVE('',#24782,#24796,#23115,.T.);
#30613=EDGE_CURVE('',#24797,#24798,#23116,.T.);
#30614=EDGE_CURVE('',#24797,#24799,#10965,.T.);
#30615=EDGE_CURVE('',#24799,#24800,#23117,.T.);
#30616=EDGE_CURVE('',#24798,#24800,#10966,.T.);
#30617=EDGE_CURVE('',#24801,#24797,#23118,.T.);
#30618=EDGE_CURVE('',#24801,#24802,#10967,.T.);
#30619=EDGE_CURVE('',#24802,#24799,#23119,.T.);
#30620=EDGE_CURVE('',#24803,#24801,#23120,.T.);
#30621=EDGE_CURVE('',#24803,#24804,#10968,.T.);
#30622=EDGE_CURVE('',#24804,#24802,#23121,.T.);
#30623=EDGE_CURVE('',#24805,#24803,#23122,.T.);
#30624=EDGE_CURVE('',#24805,#24806,#10969,.T.);
#30625=EDGE_CURVE('',#24806,#24804,#23123,.T.);
#30626=EDGE_CURVE('',#24807,#24805,#23124,.T.);
#30627=EDGE_CURVE('',#24807,#24808,#10970,.T.);
#30628=EDGE_CURVE('',#24808,#24806,#23125,.T.);
#30629=EDGE_CURVE('',#24809,#24807,#23126,.T.);
#30630=EDGE_CURVE('',#24809,#24810,#10971,.T.);
#30631=EDGE_CURVE('',#24810,#24808,#23127,.T.);
#30632=EDGE_CURVE('',#24811,#24809,#23128,.T.);
#30633=EDGE_CURVE('',#24811,#24812,#10972,.T.);
#30634=EDGE_CURVE('',#24812,#24810,#23129,.T.);
#30635=EDGE_CURVE('',#24813,#24811,#23130,.T.);
#30636=EDGE_CURVE('',#24813,#24814,#10973,.T.);
#30637=EDGE_CURVE('',#24814,#24812,#23131,.T.);
#30638=EDGE_CURVE('',#24815,#24813,#23132,.T.);
#30639=EDGE_CURVE('',#24815,#24816,#10974,.T.);
#30640=EDGE_CURVE('',#24816,#24814,#23133,.T.);
#30641=EDGE_CURVE('',#24817,#24815,#23134,.T.);
#30642=EDGE_CURVE('',#24817,#24818,#10975,.T.);
#30643=EDGE_CURVE('',#24818,#24816,#23135,.T.);
#30644=EDGE_CURVE('',#24819,#24817,#23136,.T.);
#30645=EDGE_CURVE('',#24819,#24820,#10976,.T.);
#30646=EDGE_CURVE('',#24820,#24818,#23137,.T.);
#30647=EDGE_CURVE('',#24821,#24819,#23138,.T.);
#30648=EDGE_CURVE('',#24821,#24822,#10977,.T.);
#30649=EDGE_CURVE('',#24822,#24820,#23139,.T.);
#30650=EDGE_CURVE('',#24823,#24821,#23140,.T.);
#30651=EDGE_CURVE('',#24823,#24824,#10978,.T.);
#30652=EDGE_CURVE('',#24824,#24822,#23141,.T.);
#30653=EDGE_CURVE('',#24825,#24823,#23142,.T.);
#30654=EDGE_CURVE('',#24825,#24826,#10979,.T.);
#30655=EDGE_CURVE('',#24826,#24824,#23143,.T.);
#30656=EDGE_CURVE('',#24827,#24825,#23144,.T.);
#30657=EDGE_CURVE('',#24827,#24828,#10980,.T.);
#30658=EDGE_CURVE('',#24828,#24826,#23145,.T.);
#30659=EDGE_CURVE('',#24798,#24827,#23146,.T.);
#30660=EDGE_CURVE('',#24800,#24828,#23147,.T.);
#30661=EDGE_CURVE('',#24829,#24830,#23148,.T.);
#30662=EDGE_CURVE('',#24829,#24831,#10981,.T.);
#30663=EDGE_CURVE('',#24831,#24832,#23149,.T.);
#30664=EDGE_CURVE('',#24830,#24832,#10982,.T.);
#30665=EDGE_CURVE('',#24833,#24829,#23150,.T.);
#30666=EDGE_CURVE('',#24833,#24834,#10983,.T.);
#30667=EDGE_CURVE('',#24834,#24831,#23151,.T.);
#30668=EDGE_CURVE('',#24835,#24833,#23152,.T.);
#30669=EDGE_CURVE('',#24835,#24836,#10984,.T.);
#30670=EDGE_CURVE('',#24836,#24834,#23153,.T.);
#30671=EDGE_CURVE('',#24837,#24835,#23154,.T.);
#30672=EDGE_CURVE('',#24837,#24838,#10985,.T.);
#30673=EDGE_CURVE('',#24838,#24836,#23155,.T.);
#30674=EDGE_CURVE('',#24839,#24837,#23156,.T.);
#30675=EDGE_CURVE('',#24839,#24840,#10986,.T.);
#30676=EDGE_CURVE('',#24840,#24838,#23157,.T.);
#30677=EDGE_CURVE('',#24841,#24839,#23158,.T.);
#30678=EDGE_CURVE('',#24841,#24842,#10987,.T.);
#30679=EDGE_CURVE('',#24842,#24840,#23159,.T.);
#30680=EDGE_CURVE('',#24843,#24841,#23160,.T.);
#30681=EDGE_CURVE('',#24843,#24844,#10988,.T.);
#30682=EDGE_CURVE('',#24844,#24842,#23161,.T.);
#30683=EDGE_CURVE('',#24830,#24843,#23162,.T.);
#30684=EDGE_CURVE('',#24832,#24844,#23163,.T.);
#30685=EDGE_CURVE('',#24845,#24846,#23164,.T.);
#30686=EDGE_CURVE('',#24845,#24847,#10989,.T.);
#30687=EDGE_CURVE('',#24847,#24848,#23165,.T.);
#30688=EDGE_CURVE('',#24846,#24848,#10990,.T.);
#30689=EDGE_CURVE('',#24849,#24845,#23166,.T.);
#30690=EDGE_CURVE('',#24849,#24850,#10991,.T.);
#30691=EDGE_CURVE('',#24850,#24847,#23167,.T.);
#30692=EDGE_CURVE('',#24851,#24849,#23168,.T.);
#30693=EDGE_CURVE('',#24851,#24852,#10992,.T.);
#30694=EDGE_CURVE('',#24852,#24850,#23169,.T.);
#30695=EDGE_CURVE('',#24853,#24851,#23170,.T.);
#30696=EDGE_CURVE('',#24853,#24854,#10993,.T.);
#30697=EDGE_CURVE('',#24854,#24852,#23171,.T.);
#30698=EDGE_CURVE('',#24855,#24853,#23172,.T.);
#30699=EDGE_CURVE('',#24855,#24856,#10994,.T.);
#30700=EDGE_CURVE('',#24856,#24854,#23173,.T.);
#30701=EDGE_CURVE('',#24857,#24855,#23174,.T.);
#30702=EDGE_CURVE('',#24857,#24858,#10995,.T.);
#30703=EDGE_CURVE('',#24858,#24856,#23175,.T.);
#30704=EDGE_CURVE('',#24859,#24857,#23176,.T.);
#30705=EDGE_CURVE('',#24859,#24860,#10996,.T.);
#30706=EDGE_CURVE('',#24860,#24858,#23177,.T.);
#30707=EDGE_CURVE('',#24861,#24859,#23178,.T.);
#30708=EDGE_CURVE('',#24861,#24862,#10997,.T.);
#30709=EDGE_CURVE('',#24862,#24860,#23179,.T.);
#30710=EDGE_CURVE('',#24863,#24861,#23180,.T.);
#30711=EDGE_CURVE('',#24863,#24864,#10998,.T.);
#30712=EDGE_CURVE('',#24864,#24862,#23181,.T.);
#30713=EDGE_CURVE('',#24865,#24863,#23182,.T.);
#30714=EDGE_CURVE('',#24865,#24866,#10999,.T.);
#30715=EDGE_CURVE('',#24866,#24864,#23183,.T.);
#30716=EDGE_CURVE('',#24867,#24865,#23184,.T.);
#30717=EDGE_CURVE('',#24867,#24868,#11000,.T.);
#30718=EDGE_CURVE('',#24868,#24866,#23185,.T.);
#30719=EDGE_CURVE('',#24846,#24867,#23186,.T.);
#30720=EDGE_CURVE('',#24848,#24868,#23187,.T.);
#30721=EDGE_CURVE('',#24869,#24870,#23188,.T.);
#30722=EDGE_CURVE('',#24869,#24871,#11001,.T.);
#30723=EDGE_CURVE('',#24871,#24872,#23189,.T.);
#30724=EDGE_CURVE('',#24870,#24872,#11002,.T.);
#30725=EDGE_CURVE('',#24873,#24869,#23190,.T.);
#30726=EDGE_CURVE('',#24873,#24874,#11003,.T.);
#30727=EDGE_CURVE('',#24874,#24871,#23191,.T.);
#30728=EDGE_CURVE('',#24875,#24873,#23192,.T.);
#30729=EDGE_CURVE('',#24875,#24876,#11004,.T.);
#30730=EDGE_CURVE('',#24876,#24874,#23193,.T.);
#30731=EDGE_CURVE('',#24877,#24875,#11005,.T.);
#30732=EDGE_CURVE('',#24877,#24878,#11006,.T.);
#30733=EDGE_CURVE('',#24878,#24876,#11007,.T.);
#30734=EDGE_CURVE('',#24879,#24877,#23194,.T.);
#30735=EDGE_CURVE('',#24879,#24880,#11008,.T.);
#30736=EDGE_CURVE('',#24880,#24878,#23195,.T.);
#30737=EDGE_CURVE('',#24881,#24879,#23196,.T.);
#30738=EDGE_CURVE('',#24881,#24882,#11009,.T.);
#30739=EDGE_CURVE('',#24882,#24880,#23197,.T.);
#30740=EDGE_CURVE('',#24883,#24881,#23198,.T.);
#30741=EDGE_CURVE('',#24883,#24884,#11010,.T.);
#30742=EDGE_CURVE('',#24884,#24882,#23199,.T.);
#30743=EDGE_CURVE('',#24885,#24883,#11011,.T.);
#30744=EDGE_CURVE('',#24885,#24886,#11012,.T.);
#30745=EDGE_CURVE('',#24886,#24884,#11013,.T.);
#30746=EDGE_CURVE('',#24887,#24885,#11014,.T.);
#30747=EDGE_CURVE('',#24887,#24888,#11015,.T.);
#30748=EDGE_CURVE('',#24888,#24886,#11016,.T.);
#30749=EDGE_CURVE('',#24889,#24887,#11017,.T.);
#30750=EDGE_CURVE('',#24889,#24890,#11018,.T.);
#30751=EDGE_CURVE('',#24890,#24888,#11019,.T.);
#30752=EDGE_CURVE('',#24870,#24889,#11020,.T.);
#30753=EDGE_CURVE('',#24872,#24890,#11021,.T.);
#30754=EDGE_CURVE('',#24891,#24892,#23200,.T.);
#30755=EDGE_CURVE('',#24891,#24893,#11022,.T.);
#30756=EDGE_CURVE('',#24893,#24894,#23201,.T.);
#30757=EDGE_CURVE('',#24892,#24894,#11023,.T.);
#30758=EDGE_CURVE('',#24895,#24891,#23202,.T.);
#30759=EDGE_CURVE('',#24895,#24896,#11024,.T.);
#30760=EDGE_CURVE('',#24896,#24893,#23203,.T.);
#30761=EDGE_CURVE('',#24897,#24895,#23204,.T.);
#30762=EDGE_CURVE('',#24897,#24898,#11025,.T.);
#30763=EDGE_CURVE('',#24898,#24896,#23205,.T.);
#30764=EDGE_CURVE('',#24899,#24897,#23206,.T.);
#30765=EDGE_CURVE('',#24899,#24900,#11026,.T.);
#30766=EDGE_CURVE('',#24900,#24898,#23207,.T.);
#30767=EDGE_CURVE('',#24901,#24899,#23208,.T.);
#30768=EDGE_CURVE('',#24901,#24902,#11027,.T.);
#30769=EDGE_CURVE('',#24902,#24900,#23209,.T.);
#30770=EDGE_CURVE('',#24903,#24901,#23210,.T.);
#30771=EDGE_CURVE('',#24903,#24904,#11028,.T.);
#30772=EDGE_CURVE('',#24904,#24902,#23211,.T.);
#30773=EDGE_CURVE('',#24905,#24903,#23212,.T.);
#30774=EDGE_CURVE('',#24905,#24906,#11029,.T.);
#30775=EDGE_CURVE('',#24906,#24904,#23213,.T.);
#30776=EDGE_CURVE('',#24892,#24905,#23214,.T.);
#30777=EDGE_CURVE('',#24894,#24906,#23215,.T.);
#30778=EDGE_CURVE('',#24907,#24908,#23216,.T.);
#30779=EDGE_CURVE('',#24907,#24909,#11030,.T.);
#30780=EDGE_CURVE('',#24909,#24910,#23217,.T.);
#30781=EDGE_CURVE('',#24908,#24910,#11031,.T.);
#30782=EDGE_CURVE('',#24911,#24907,#23218,.T.);
#30783=EDGE_CURVE('',#24911,#24912,#11032,.T.);
#30784=EDGE_CURVE('',#24912,#24909,#23219,.T.);
#30785=EDGE_CURVE('',#24913,#24911,#23220,.T.);
#30786=EDGE_CURVE('',#24913,#24914,#11033,.T.);
#30787=EDGE_CURVE('',#24914,#24912,#23221,.T.);
#30788=EDGE_CURVE('',#24915,#24913,#23222,.T.);
#30789=EDGE_CURVE('',#24915,#24916,#11034,.T.);
#30790=EDGE_CURVE('',#24916,#24914,#23223,.T.);
#30791=EDGE_CURVE('',#24917,#24915,#23224,.T.);
#30792=EDGE_CURVE('',#24917,#24918,#11035,.T.);
#30793=EDGE_CURVE('',#24918,#24916,#23225,.T.);
#30794=EDGE_CURVE('',#24919,#24917,#23226,.T.);
#30795=EDGE_CURVE('',#24919,#24920,#11036,.T.);
#30796=EDGE_CURVE('',#24920,#24918,#23227,.T.);
#30797=EDGE_CURVE('',#24921,#24919,#23228,.T.);
#30798=EDGE_CURVE('',#24921,#24922,#11037,.T.);
#30799=EDGE_CURVE('',#24922,#24920,#23229,.T.);
#30800=EDGE_CURVE('',#24923,#24921,#23230,.T.);
#30801=EDGE_CURVE('',#24923,#24924,#11038,.T.);
#30802=EDGE_CURVE('',#24924,#24922,#23231,.T.);
#30803=EDGE_CURVE('',#24925,#24923,#23232,.T.);
#30804=EDGE_CURVE('',#24925,#24926,#11039,.T.);
#30805=EDGE_CURVE('',#24926,#24924,#23233,.T.);
#30806=EDGE_CURVE('',#24927,#24925,#23234,.T.);
#30807=EDGE_CURVE('',#24927,#24928,#11040,.T.);
#30808=EDGE_CURVE('',#24928,#24926,#23235,.T.);
#30809=EDGE_CURVE('',#24929,#24927,#23236,.T.);
#30810=EDGE_CURVE('',#24929,#24930,#11041,.T.);
#30811=EDGE_CURVE('',#24930,#24928,#23237,.T.);
#30812=EDGE_CURVE('',#24908,#24929,#23238,.T.);
#30813=EDGE_CURVE('',#24910,#24930,#23239,.T.);
#30814=EDGE_CURVE('',#24931,#24932,#23240,.T.);
#30815=EDGE_CURVE('',#24931,#24933,#11042,.T.);
#30816=EDGE_CURVE('',#24933,#24934,#23241,.T.);
#30817=EDGE_CURVE('',#24932,#24934,#11043,.T.);
#30818=EDGE_CURVE('',#24935,#24931,#23242,.T.);
#30819=EDGE_CURVE('',#24935,#24936,#11044,.T.);
#30820=EDGE_CURVE('',#24936,#24933,#23243,.T.);
#30821=EDGE_CURVE('',#24937,#24935,#23244,.T.);
#30822=EDGE_CURVE('',#24937,#24938,#11045,.T.);
#30823=EDGE_CURVE('',#24938,#24936,#23245,.T.);
#30824=EDGE_CURVE('',#24939,#24937,#23246,.T.);
#30825=EDGE_CURVE('',#24939,#24940,#11046,.T.);
#30826=EDGE_CURVE('',#24940,#24938,#23247,.T.);
#30827=EDGE_CURVE('',#24941,#24939,#23248,.T.);
#30828=EDGE_CURVE('',#24941,#24942,#11047,.T.);
#30829=EDGE_CURVE('',#24942,#24940,#23249,.T.);
#30830=EDGE_CURVE('',#24943,#24941,#23250,.T.);
#30831=EDGE_CURVE('',#24943,#24944,#11048,.T.);
#30832=EDGE_CURVE('',#24944,#24942,#23251,.T.);
#30833=EDGE_CURVE('',#24945,#24943,#23252,.T.);
#30834=EDGE_CURVE('',#24945,#24946,#11049,.T.);
#30835=EDGE_CURVE('',#24946,#24944,#23253,.T.);
#30836=EDGE_CURVE('',#24947,#24945,#23254,.T.);
#30837=EDGE_CURVE('',#24947,#24948,#11050,.T.);
#30838=EDGE_CURVE('',#24948,#24946,#23255,.T.);
#30839=EDGE_CURVE('',#24932,#24947,#23256,.T.);
#30840=EDGE_CURVE('',#24934,#24948,#23257,.T.);
#30841=EDGE_CURVE('',#24949,#24950,#23258,.T.);
#30842=EDGE_CURVE('',#24949,#24951,#11051,.T.);
#30843=EDGE_CURVE('',#24951,#24952,#23259,.T.);
#30844=EDGE_CURVE('',#24950,#24952,#11052,.T.);
#30845=EDGE_CURVE('',#24953,#24949,#23260,.T.);
#30846=EDGE_CURVE('',#24953,#24954,#11053,.T.);
#30847=EDGE_CURVE('',#24954,#24951,#23261,.T.);
#30848=EDGE_CURVE('',#24955,#24953,#23262,.T.);
#30849=EDGE_CURVE('',#24955,#24956,#11054,.T.);
#30850=EDGE_CURVE('',#24956,#24954,#23263,.T.);
#30851=EDGE_CURVE('',#24957,#24955,#23264,.T.);
#30852=EDGE_CURVE('',#24957,#24958,#11055,.T.);
#30853=EDGE_CURVE('',#24958,#24956,#23265,.T.);
#30854=EDGE_CURVE('',#24959,#24957,#23266,.T.);
#30855=EDGE_CURVE('',#24959,#24960,#11056,.T.);
#30856=EDGE_CURVE('',#24960,#24958,#23267,.T.);
#30857=EDGE_CURVE('',#24961,#24959,#23268,.T.);
#30858=EDGE_CURVE('',#24961,#24962,#11057,.T.);
#30859=EDGE_CURVE('',#24962,#24960,#23269,.T.);
#30860=EDGE_CURVE('',#24963,#24961,#23270,.T.);
#30861=EDGE_CURVE('',#24963,#24964,#11058,.T.);
#30862=EDGE_CURVE('',#24964,#24962,#23271,.T.);
#30863=EDGE_CURVE('',#24965,#24963,#23272,.T.);
#30864=EDGE_CURVE('',#24965,#24966,#11059,.T.);
#30865=EDGE_CURVE('',#24966,#24964,#23273,.T.);
#30866=EDGE_CURVE('',#24967,#24965,#23274,.T.);
#30867=EDGE_CURVE('',#24967,#24968,#11060,.T.);
#30868=EDGE_CURVE('',#24968,#24966,#23275,.T.);
#30869=EDGE_CURVE('',#24969,#24967,#23276,.T.);
#30870=EDGE_CURVE('',#24969,#24970,#11061,.T.);
#30871=EDGE_CURVE('',#24970,#24968,#23277,.T.);
#30872=EDGE_CURVE('',#24971,#24969,#23278,.T.);
#30873=EDGE_CURVE('',#24971,#24972,#11062,.T.);
#30874=EDGE_CURVE('',#24972,#24970,#23279,.T.);
#30875=EDGE_CURVE('',#24973,#24971,#23280,.T.);
#30876=EDGE_CURVE('',#24973,#24974,#11063,.T.);
#30877=EDGE_CURVE('',#24974,#24972,#23281,.T.);
#30878=EDGE_CURVE('',#24975,#24973,#23282,.T.);
#30879=EDGE_CURVE('',#24975,#24976,#11064,.T.);
#30880=EDGE_CURVE('',#24976,#24974,#23283,.T.);
#30881=EDGE_CURVE('',#24977,#24975,#23284,.T.);
#30882=EDGE_CURVE('',#24977,#24978,#11065,.T.);
#30883=EDGE_CURVE('',#24978,#24976,#23285,.T.);
#30884=EDGE_CURVE('',#24979,#24977,#23286,.T.);
#30885=EDGE_CURVE('',#24979,#24980,#11066,.T.);
#30886=EDGE_CURVE('',#24980,#24978,#23287,.T.);
#30887=EDGE_CURVE('',#24981,#24979,#23288,.T.);
#30888=EDGE_CURVE('',#24981,#24982,#11067,.T.);
#30889=EDGE_CURVE('',#24982,#24980,#23289,.T.);
#30890=EDGE_CURVE('',#24983,#24981,#23290,.T.);
#30891=EDGE_CURVE('',#24983,#24984,#11068,.T.);
#30892=EDGE_CURVE('',#24984,#24982,#23291,.T.);
#30893=EDGE_CURVE('',#24985,#24983,#11069,.T.);
#30894=EDGE_CURVE('',#24985,#24986,#11070,.T.);
#30895=EDGE_CURVE('',#24986,#24984,#11071,.T.);
#30896=EDGE_CURVE('',#24950,#24985,#23292,.T.);
#30897=EDGE_CURVE('',#24952,#24986,#23293,.T.);
#30898=EDGE_CURVE('',#24987,#24988,#23294,.T.);
#30899=EDGE_CURVE('',#24987,#24989,#11072,.T.);
#30900=EDGE_CURVE('',#24989,#24990,#23295,.T.);
#30901=EDGE_CURVE('',#24988,#24990,#11073,.T.);
#30902=EDGE_CURVE('',#24991,#24987,#23296,.T.);
#30903=EDGE_CURVE('',#24991,#24992,#11074,.T.);
#30904=EDGE_CURVE('',#24992,#24989,#23297,.T.);
#30905=EDGE_CURVE('',#24993,#24991,#23298,.T.);
#30906=EDGE_CURVE('',#24993,#24994,#11075,.T.);
#30907=EDGE_CURVE('',#24994,#24992,#23299,.T.);
#30908=EDGE_CURVE('',#24995,#24993,#23300,.T.);
#30909=EDGE_CURVE('',#24995,#24996,#11076,.T.);
#30910=EDGE_CURVE('',#24996,#24994,#23301,.T.);
#30911=EDGE_CURVE('',#24997,#24995,#23302,.T.);
#30912=EDGE_CURVE('',#24997,#24998,#11077,.T.);
#30913=EDGE_CURVE('',#24998,#24996,#23303,.T.);
#30914=EDGE_CURVE('',#24999,#24997,#23304,.T.);
#30915=EDGE_CURVE('',#24999,#25000,#11078,.T.);
#30916=EDGE_CURVE('',#25000,#24998,#23305,.T.);
#30917=EDGE_CURVE('',#25001,#24999,#23306,.T.);
#30918=EDGE_CURVE('',#25001,#25002,#11079,.T.);
#30919=EDGE_CURVE('',#25002,#25000,#23307,.T.);
#30920=EDGE_CURVE('',#24988,#25001,#23308,.T.);
#30921=EDGE_CURVE('',#24990,#25002,#23309,.T.);
#30922=EDGE_CURVE('',#25003,#25004,#23310,.T.);
#30923=EDGE_CURVE('',#25003,#25005,#11080,.T.);
#30924=EDGE_CURVE('',#25005,#25006,#23311,.T.);
#30925=EDGE_CURVE('',#25004,#25006,#11081,.T.);
#30926=EDGE_CURVE('',#25007,#25003,#23312,.T.);
#30927=EDGE_CURVE('',#25007,#25008,#11082,.T.);
#30928=EDGE_CURVE('',#25008,#25005,#23313,.T.);
#30929=EDGE_CURVE('',#25009,#25007,#23314,.T.);
#30930=EDGE_CURVE('',#25009,#25010,#11083,.T.);
#30931=EDGE_CURVE('',#25010,#25008,#23315,.T.);
#30932=EDGE_CURVE('',#25011,#25009,#23316,.T.);
#30933=EDGE_CURVE('',#25011,#25012,#11084,.T.);
#30934=EDGE_CURVE('',#25012,#25010,#23317,.T.);
#30935=EDGE_CURVE('',#25013,#25011,#23318,.T.);
#30936=EDGE_CURVE('',#25013,#25014,#11085,.T.);
#30937=EDGE_CURVE('',#25014,#25012,#23319,.T.);
#30938=EDGE_CURVE('',#25015,#25013,#23320,.T.);
#30939=EDGE_CURVE('',#25015,#25016,#11086,.T.);
#30940=EDGE_CURVE('',#25016,#25014,#23321,.T.);
#30941=EDGE_CURVE('',#25017,#25015,#23322,.T.);
#30942=EDGE_CURVE('',#25017,#25018,#11087,.T.);
#30943=EDGE_CURVE('',#25018,#25016,#23323,.T.);
#30944=EDGE_CURVE('',#25019,#25017,#23324,.T.);
#30945=EDGE_CURVE('',#25019,#25020,#11088,.T.);
#30946=EDGE_CURVE('',#25020,#25018,#23325,.T.);
#30947=EDGE_CURVE('',#25021,#25019,#23326,.T.);
#30948=EDGE_CURVE('',#25021,#25022,#11089,.T.);
#30949=EDGE_CURVE('',#25022,#25020,#23327,.T.);
#30950=EDGE_CURVE('',#25023,#25021,#23328,.T.);
#30951=EDGE_CURVE('',#25023,#25024,#11090,.T.);
#30952=EDGE_CURVE('',#25024,#25022,#23329,.T.);
#30953=EDGE_CURVE('',#25025,#25023,#23330,.T.);
#30954=EDGE_CURVE('',#25025,#25026,#11091,.T.);
#30955=EDGE_CURVE('',#25026,#25024,#23331,.T.);
#30956=EDGE_CURVE('',#25004,#25025,#23332,.T.);
#30957=EDGE_CURVE('',#25006,#25026,#23333,.T.);
#30958=EDGE_CURVE('',#25027,#25028,#23334,.T.);
#30959=EDGE_CURVE('',#25027,#25029,#11092,.T.);
#30960=EDGE_CURVE('',#25029,#25030,#23335,.T.);
#30961=EDGE_CURVE('',#25028,#25030,#11093,.T.);
#30962=EDGE_CURVE('',#25031,#25027,#23336,.T.);
#30963=EDGE_CURVE('',#25031,#25032,#11094,.T.);
#30964=EDGE_CURVE('',#25032,#25029,#23337,.T.);
#30965=EDGE_CURVE('',#25033,#25031,#23338,.T.);
#30966=EDGE_CURVE('',#25033,#25034,#11095,.T.);
#30967=EDGE_CURVE('',#25034,#25032,#23339,.T.);
#30968=EDGE_CURVE('',#25035,#25033,#23340,.T.);
#30969=EDGE_CURVE('',#25035,#25036,#11096,.T.);
#30970=EDGE_CURVE('',#25036,#25034,#23341,.T.);
#30971=EDGE_CURVE('',#25037,#25035,#23342,.T.);
#30972=EDGE_CURVE('',#25037,#25038,#11097,.T.);
#30973=EDGE_CURVE('',#25038,#25036,#23343,.T.);
#30974=EDGE_CURVE('',#25039,#25037,#23344,.T.);
#30975=EDGE_CURVE('',#25039,#25040,#11098,.T.);
#30976=EDGE_CURVE('',#25040,#25038,#23345,.T.);
#30977=EDGE_CURVE('',#25041,#25039,#11099,.T.);
#30978=EDGE_CURVE('',#25041,#25042,#11100,.T.);
#30979=EDGE_CURVE('',#25042,#25040,#11101,.T.);
#30980=EDGE_CURVE('',#25043,#25041,#11102,.T.);
#30981=EDGE_CURVE('',#25043,#25044,#11103,.T.);
#30982=EDGE_CURVE('',#25044,#25042,#11104,.T.);
#30983=EDGE_CURVE('',#25045,#25043,#11105,.T.);
#30984=EDGE_CURVE('',#25045,#25046,#11106,.T.);
#30985=EDGE_CURVE('',#25046,#25044,#11107,.T.);
#30986=EDGE_CURVE('',#25047,#25045,#11108,.T.);
#30987=EDGE_CURVE('',#25047,#25048,#11109,.T.);
#30988=EDGE_CURVE('',#25048,#25046,#11110,.T.);
#30989=EDGE_CURVE('',#25049,#25047,#11111,.T.);
#30990=EDGE_CURVE('',#25049,#25050,#11112,.T.);
#30991=EDGE_CURVE('',#25050,#25048,#11113,.T.);
#30992=EDGE_CURVE('',#25051,#25049,#11114,.T.);
#30993=EDGE_CURVE('',#25051,#25052,#11115,.T.);
#30994=EDGE_CURVE('',#25052,#25050,#11116,.T.);
#30995=EDGE_CURVE('',#25053,#25051,#23346,.T.);
#30996=EDGE_CURVE('',#25053,#25054,#11117,.T.);
#30997=EDGE_CURVE('',#25054,#25052,#23347,.T.);
#30998=EDGE_CURVE('',#25055,#25053,#23348,.T.);
#30999=EDGE_CURVE('',#25055,#25056,#11118,.T.);
#31000=EDGE_CURVE('',#25056,#25054,#23349,.T.);
#31001=EDGE_CURVE('',#25057,#25055,#23350,.T.);
#31002=EDGE_CURVE('',#25057,#25058,#11119,.T.);
#31003=EDGE_CURVE('',#25058,#25056,#23351,.T.);
#31004=EDGE_CURVE('',#25059,#25057,#23352,.T.);
#31005=EDGE_CURVE('',#25059,#25060,#11120,.T.);
#31006=EDGE_CURVE('',#25060,#25058,#23353,.T.);
#31007=EDGE_CURVE('',#25061,#25059,#23354,.T.);
#31008=EDGE_CURVE('',#25061,#25062,#11121,.T.);
#31009=EDGE_CURVE('',#25062,#25060,#23355,.T.);
#31010=EDGE_CURVE('',#25063,#25061,#23356,.T.);
#31011=EDGE_CURVE('',#25063,#25064,#11122,.T.);
#31012=EDGE_CURVE('',#25064,#25062,#23357,.T.);
#31013=EDGE_CURVE('',#25065,#25063,#23358,.T.);
#31014=EDGE_CURVE('',#25065,#25066,#11123,.T.);
#31015=EDGE_CURVE('',#25066,#25064,#23359,.T.);
#31016=EDGE_CURVE('',#25067,#25065,#23360,.T.);
#31017=EDGE_CURVE('',#25067,#25068,#11124,.T.);
#31018=EDGE_CURVE('',#25068,#25066,#23361,.T.);
#31019=EDGE_CURVE('',#25069,#25067,#11125,.T.);
#31020=EDGE_CURVE('',#25069,#25070,#11126,.T.);
#31021=EDGE_CURVE('',#25070,#25068,#11127,.T.);
#31022=EDGE_CURVE('',#25028,#25069,#23362,.T.);
#31023=EDGE_CURVE('',#25030,#25070,#23363,.T.);
#31024=EDGE_CURVE('',#25071,#25072,#23364,.T.);
#31025=EDGE_CURVE('',#25071,#25073,#11128,.T.);
#31026=EDGE_CURVE('',#25073,#25074,#23365,.T.);
#31027=EDGE_CURVE('',#25072,#25074,#11129,.T.);
#31028=EDGE_CURVE('',#25075,#25071,#23366,.T.);
#31029=EDGE_CURVE('',#25075,#25076,#11130,.T.);
#31030=EDGE_CURVE('',#25076,#25073,#23367,.T.);
#31031=EDGE_CURVE('',#25077,#25075,#23368,.T.);
#31032=EDGE_CURVE('',#25077,#25078,#11131,.T.);
#31033=EDGE_CURVE('',#25078,#25076,#23369,.T.);
#31034=EDGE_CURVE('',#25079,#25077,#23370,.T.);
#31035=EDGE_CURVE('',#25079,#25080,#11132,.T.);
#31036=EDGE_CURVE('',#25080,#25078,#23371,.T.);
#31037=EDGE_CURVE('',#25081,#25079,#23372,.T.);
#31038=EDGE_CURVE('',#25081,#25082,#11133,.T.);
#31039=EDGE_CURVE('',#25082,#25080,#23373,.T.);
#31040=EDGE_CURVE('',#25083,#25081,#23374,.T.);
#31041=EDGE_CURVE('',#25083,#25084,#11134,.T.);
#31042=EDGE_CURVE('',#25084,#25082,#23375,.T.);
#31043=EDGE_CURVE('',#25085,#25083,#23376,.T.);
#31044=EDGE_CURVE('',#25085,#25086,#11135,.T.);
#31045=EDGE_CURVE('',#25086,#25084,#23377,.T.);
#31046=EDGE_CURVE('',#25072,#25085,#23378,.T.);
#31047=EDGE_CURVE('',#25074,#25086,#23379,.T.);
#31048=EDGE_CURVE('',#25087,#25088,#23380,.T.);
#31049=EDGE_CURVE('',#25087,#25089,#11136,.T.);
#31050=EDGE_CURVE('',#25089,#25090,#23381,.T.);
#31051=EDGE_CURVE('',#25088,#25090,#11137,.T.);
#31052=EDGE_CURVE('',#25091,#25087,#23382,.T.);
#31053=EDGE_CURVE('',#25091,#25092,#11138,.T.);
#31054=EDGE_CURVE('',#25092,#25089,#23383,.T.);
#31055=EDGE_CURVE('',#25093,#25091,#23384,.T.);
#31056=EDGE_CURVE('',#25093,#25094,#11139,.T.);
#31057=EDGE_CURVE('',#25094,#25092,#23385,.T.);
#31058=EDGE_CURVE('',#25095,#25093,#23386,.T.);
#31059=EDGE_CURVE('',#25095,#25096,#11140,.T.);
#31060=EDGE_CURVE('',#25096,#25094,#23387,.T.);
#31061=EDGE_CURVE('',#25097,#25095,#23388,.T.);
#31062=EDGE_CURVE('',#25097,#25098,#11141,.T.);
#31063=EDGE_CURVE('',#25098,#25096,#23389,.T.);
#31064=EDGE_CURVE('',#25099,#25097,#23390,.T.);
#31065=EDGE_CURVE('',#25099,#25100,#11142,.T.);
#31066=EDGE_CURVE('',#25100,#25098,#23391,.T.);
#31067=EDGE_CURVE('',#25101,#25099,#23392,.T.);
#31068=EDGE_CURVE('',#25101,#25102,#11143,.T.);
#31069=EDGE_CURVE('',#25102,#25100,#23393,.T.);
#31070=EDGE_CURVE('',#25103,#25101,#23394,.T.);
#31071=EDGE_CURVE('',#25103,#25104,#11144,.T.);
#31072=EDGE_CURVE('',#25104,#25102,#23395,.T.);
#31073=EDGE_CURVE('',#25105,#25103,#23396,.T.);
#31074=EDGE_CURVE('',#25105,#25106,#11145,.T.);
#31075=EDGE_CURVE('',#25106,#25104,#23397,.T.);
#31076=EDGE_CURVE('',#25107,#25105,#23398,.T.);
#31077=EDGE_CURVE('',#25107,#25108,#11146,.T.);
#31078=EDGE_CURVE('',#25108,#25106,#23399,.T.);
#31079=EDGE_CURVE('',#25109,#25107,#23400,.T.);
#31080=EDGE_CURVE('',#25109,#25110,#11147,.T.);
#31081=EDGE_CURVE('',#25110,#25108,#23401,.T.);
#31082=EDGE_CURVE('',#25088,#25109,#23402,.T.);
#31083=EDGE_CURVE('',#25090,#25110,#23403,.T.);
#31084=EDGE_CURVE('',#25111,#25112,#11148,.T.);
#31085=EDGE_CURVE('',#25111,#25113,#11149,.T.);
#31086=EDGE_CURVE('',#25113,#25114,#11150,.T.);
#31087=EDGE_CURVE('',#25112,#25114,#11151,.T.);
#31088=EDGE_CURVE('',#25115,#25111,#11152,.T.);
#31089=EDGE_CURVE('',#25115,#25116,#11153,.T.);
#31090=EDGE_CURVE('',#25116,#25113,#11154,.T.);
#31091=EDGE_CURVE('',#25112,#25115,#11155,.T.);
#31092=EDGE_CURVE('',#25114,#25116,#11156,.T.);
#31093=EDGE_CURVE('',#25117,#25118,#11157,.T.);
#31094=EDGE_CURVE('',#25117,#25119,#11158,.T.);
#31095=EDGE_CURVE('',#25119,#25120,#11159,.T.);
#31096=EDGE_CURVE('',#25118,#25120,#11160,.T.);
#31097=EDGE_CURVE('',#25121,#25117,#11161,.T.);
#31098=EDGE_CURVE('',#25121,#25122,#11162,.T.);
#31099=EDGE_CURVE('',#25122,#25119,#11163,.T.);
#31100=EDGE_CURVE('',#25123,#25121,#11164,.T.);
#31101=EDGE_CURVE('',#25123,#25124,#11165,.T.);
#31102=EDGE_CURVE('',#25124,#25122,#11166,.T.);
#31103=EDGE_CURVE('',#25125,#25123,#11167,.T.);
#31104=EDGE_CURVE('',#25125,#25126,#11168,.T.);
#31105=EDGE_CURVE('',#25126,#25124,#11169,.T.);
#31106=EDGE_CURVE('',#25127,#25125,#11170,.T.);
#31107=EDGE_CURVE('',#25127,#25128,#11171,.T.);
#31108=EDGE_CURVE('',#25128,#25126,#11172,.T.);
#31109=EDGE_CURVE('',#25129,#25127,#11173,.T.);
#31110=EDGE_CURVE('',#25129,#25130,#11174,.T.);
#31111=EDGE_CURVE('',#25130,#25128,#11175,.T.);
#31112=EDGE_CURVE('',#25131,#25129,#11176,.T.);
#31113=EDGE_CURVE('',#25131,#25132,#11177,.T.);
#31114=EDGE_CURVE('',#25132,#25130,#11178,.T.);
#31115=EDGE_CURVE('',#25133,#25131,#11179,.T.);
#31116=EDGE_CURVE('',#25133,#25134,#11180,.T.);
#31117=EDGE_CURVE('',#25134,#25132,#11181,.T.);
#31118=EDGE_CURVE('',#25135,#25133,#11182,.T.);
#31119=EDGE_CURVE('',#25135,#25136,#11183,.T.);
#31120=EDGE_CURVE('',#25136,#25134,#11184,.T.);
#31121=EDGE_CURVE('',#25137,#25135,#11185,.T.);
#31122=EDGE_CURVE('',#25137,#25138,#11186,.T.);
#31123=EDGE_CURVE('',#25138,#25136,#11187,.T.);
#31124=EDGE_CURVE('',#25118,#25137,#11188,.T.);
#31125=EDGE_CURVE('',#25120,#25138,#11189,.T.);
#31126=EDGE_CURVE('',#25139,#25140,#23404,.T.);
#31127=EDGE_CURVE('',#25139,#25141,#11190,.T.);
#31128=EDGE_CURVE('',#25141,#25142,#23405,.T.);
#31129=EDGE_CURVE('',#25140,#25142,#11191,.T.);
#31130=EDGE_CURVE('',#25143,#25139,#23406,.T.);
#31131=EDGE_CURVE('',#25143,#25144,#11192,.T.);
#31132=EDGE_CURVE('',#25144,#25141,#23407,.T.);
#31133=EDGE_CURVE('',#25145,#25143,#23408,.T.);
#31134=EDGE_CURVE('',#25145,#25146,#11193,.T.);
#31135=EDGE_CURVE('',#25146,#25144,#23409,.T.);
#31136=EDGE_CURVE('',#25147,#25145,#23410,.T.);
#31137=EDGE_CURVE('',#25147,#25148,#11194,.T.);
#31138=EDGE_CURVE('',#25148,#25146,#23411,.T.);
#31139=EDGE_CURVE('',#25149,#25147,#23412,.T.);
#31140=EDGE_CURVE('',#25149,#25150,#11195,.T.);
#31141=EDGE_CURVE('',#25150,#25148,#23413,.T.);
#31142=EDGE_CURVE('',#25151,#25149,#23414,.T.);
#31143=EDGE_CURVE('',#25151,#25152,#11196,.T.);
#31144=EDGE_CURVE('',#25152,#25150,#23415,.T.);
#31145=EDGE_CURVE('',#25153,#25151,#23416,.T.);
#31146=EDGE_CURVE('',#25153,#25154,#11197,.T.);
#31147=EDGE_CURVE('',#25154,#25152,#23417,.T.);
#31148=EDGE_CURVE('',#25140,#25153,#23418,.T.);
#31149=EDGE_CURVE('',#25142,#25154,#23419,.T.);
#31150=EDGE_CURVE('',#25155,#25156,#23420,.T.);
#31151=EDGE_CURVE('',#25155,#25157,#11198,.T.);
#31152=EDGE_CURVE('',#25157,#25158,#23421,.T.);
#31153=EDGE_CURVE('',#25156,#25158,#11199,.T.);
#31154=EDGE_CURVE('',#25159,#25155,#23422,.T.);
#31155=EDGE_CURVE('',#25159,#25160,#11200,.T.);
#31156=EDGE_CURVE('',#25160,#25157,#23423,.T.);
#31157=EDGE_CURVE('',#25161,#25159,#23424,.T.);
#31158=EDGE_CURVE('',#25161,#25162,#11201,.T.);
#31159=EDGE_CURVE('',#25162,#25160,#23425,.T.);
#31160=EDGE_CURVE('',#25163,#25161,#23426,.T.);
#31161=EDGE_CURVE('',#25163,#25164,#11202,.T.);
#31162=EDGE_CURVE('',#25164,#25162,#23427,.T.);
#31163=EDGE_CURVE('',#25165,#25163,#23428,.T.);
#31164=EDGE_CURVE('',#25165,#25166,#11203,.T.);
#31165=EDGE_CURVE('',#25166,#25164,#23429,.T.);
#31166=EDGE_CURVE('',#25167,#25165,#23430,.T.);
#31167=EDGE_CURVE('',#25167,#25168,#11204,.T.);
#31168=EDGE_CURVE('',#25168,#25166,#23431,.T.);
#31169=EDGE_CURVE('',#25169,#25167,#23432,.T.);
#31170=EDGE_CURVE('',#25169,#25170,#11205,.T.);
#31171=EDGE_CURVE('',#25170,#25168,#23433,.T.);
#31172=EDGE_CURVE('',#25171,#25169,#23434,.T.);
#31173=EDGE_CURVE('',#25171,#25172,#11206,.T.);
#31174=EDGE_CURVE('',#25172,#25170,#23435,.T.);
#31175=EDGE_CURVE('',#25173,#25171,#23436,.T.);
#31176=EDGE_CURVE('',#25173,#25174,#11207,.T.);
#31177=EDGE_CURVE('',#25174,#25172,#23437,.T.);
#31178=EDGE_CURVE('',#25175,#25173,#23438,.T.);
#31179=EDGE_CURVE('',#25175,#25176,#11208,.T.);
#31180=EDGE_CURVE('',#25176,#25174,#23439,.T.);
#31181=EDGE_CURVE('',#25177,#25175,#23440,.T.);
#31182=EDGE_CURVE('',#25177,#25178,#11209,.T.);
#31183=EDGE_CURVE('',#25178,#25176,#23441,.T.);
#31184=EDGE_CURVE('',#25156,#25177,#23442,.T.);
#31185=EDGE_CURVE('',#25158,#25178,#23443,.T.);
#31186=EDGE_CURVE('',#25179,#25180,#23444,.T.);
#31187=EDGE_CURVE('',#25179,#25181,#11210,.T.);
#31188=EDGE_CURVE('',#25181,#25182,#23445,.T.);
#31189=EDGE_CURVE('',#25180,#25182,#11211,.T.);
#31190=EDGE_CURVE('',#25183,#25179,#23446,.T.);
#31191=EDGE_CURVE('',#25183,#25184,#11212,.T.);
#31192=EDGE_CURVE('',#25184,#25181,#23447,.T.);
#31193=EDGE_CURVE('',#25185,#25183,#23448,.T.);
#31194=EDGE_CURVE('',#25185,#25186,#11213,.T.);
#31195=EDGE_CURVE('',#25186,#25184,#23449,.T.);
#31196=EDGE_CURVE('',#25187,#25185,#23450,.T.);
#31197=EDGE_CURVE('',#25187,#25188,#11214,.T.);
#31198=EDGE_CURVE('',#25188,#25186,#23451,.T.);
#31199=EDGE_CURVE('',#25189,#25187,#23452,.T.);
#31200=EDGE_CURVE('',#25189,#25190,#11215,.T.);
#31201=EDGE_CURVE('',#25190,#25188,#23453,.T.);
#31202=EDGE_CURVE('',#25191,#25189,#23454,.T.);
#31203=EDGE_CURVE('',#25191,#25192,#11216,.T.);
#31204=EDGE_CURVE('',#25192,#25190,#23455,.T.);
#31205=EDGE_CURVE('',#25193,#25191,#23456,.T.);
#31206=EDGE_CURVE('',#25193,#25194,#11217,.T.);
#31207=EDGE_CURVE('',#25194,#25192,#23457,.T.);
#31208=EDGE_CURVE('',#25195,#25193,#23458,.T.);
#31209=EDGE_CURVE('',#25195,#25196,#11218,.T.);
#31210=EDGE_CURVE('',#25196,#25194,#23459,.T.);
#31211=EDGE_CURVE('',#25197,#25195,#23460,.T.);
#31212=EDGE_CURVE('',#25197,#25198,#11219,.T.);
#31213=EDGE_CURVE('',#25198,#25196,#23461,.T.);
#31214=EDGE_CURVE('',#25199,#25197,#23462,.T.);
#31215=EDGE_CURVE('',#25199,#25200,#11220,.T.);
#31216=EDGE_CURVE('',#25200,#25198,#23463,.T.);
#31217=EDGE_CURVE('',#25201,#25199,#23464,.T.);
#31218=EDGE_CURVE('',#25201,#25202,#11221,.T.);
#31219=EDGE_CURVE('',#25202,#25200,#23465,.T.);
#31220=EDGE_CURVE('',#25203,#25201,#23466,.T.);
#31221=EDGE_CURVE('',#25203,#25204,#11222,.T.);
#31222=EDGE_CURVE('',#25204,#25202,#23467,.T.);
#31223=EDGE_CURVE('',#25205,#25203,#11223,.T.);
#31224=EDGE_CURVE('',#25205,#25206,#11224,.T.);
#31225=EDGE_CURVE('',#25206,#25204,#11225,.T.);
#31226=EDGE_CURVE('',#25207,#25205,#23468,.T.);
#31227=EDGE_CURVE('',#25207,#25208,#11226,.T.);
#31228=EDGE_CURVE('',#25208,#25206,#23469,.T.);
#31229=EDGE_CURVE('',#25209,#25207,#23470,.T.);
#31230=EDGE_CURVE('',#25209,#25210,#11227,.T.);
#31231=EDGE_CURVE('',#25210,#25208,#23471,.T.);
#31232=EDGE_CURVE('',#25211,#25209,#23472,.T.);
#31233=EDGE_CURVE('',#25211,#25212,#11228,.T.);
#31234=EDGE_CURVE('',#25212,#25210,#23473,.T.);
#31235=EDGE_CURVE('',#25213,#25211,#23474,.T.);
#31236=EDGE_CURVE('',#25213,#25214,#11229,.T.);
#31237=EDGE_CURVE('',#25214,#25212,#23475,.T.);
#31238=EDGE_CURVE('',#25215,#25213,#23476,.T.);
#31239=EDGE_CURVE('',#25215,#25216,#11230,.T.);
#31240=EDGE_CURVE('',#25216,#25214,#23477,.T.);
#31241=EDGE_CURVE('',#25217,#25215,#23478,.T.);
#31242=EDGE_CURVE('',#25217,#25218,#11231,.T.);
#31243=EDGE_CURVE('',#25218,#25216,#23479,.T.);
#31244=EDGE_CURVE('',#25219,#25217,#23480,.T.);
#31245=EDGE_CURVE('',#25219,#25220,#11232,.T.);
#31246=EDGE_CURVE('',#25220,#25218,#23481,.T.);
#31247=EDGE_CURVE('',#25221,#25219,#11233,.T.);
#31248=EDGE_CURVE('',#25221,#25222,#11234,.T.);
#31249=EDGE_CURVE('',#25222,#25220,#11235,.T.);
#31250=EDGE_CURVE('',#25223,#25221,#23482,.T.);
#31251=EDGE_CURVE('',#25223,#25224,#11236,.T.);
#31252=EDGE_CURVE('',#25224,#25222,#23483,.T.);
#31253=EDGE_CURVE('',#25225,#25223,#23484,.T.);
#31254=EDGE_CURVE('',#25225,#25226,#11237,.T.);
#31255=EDGE_CURVE('',#25226,#25224,#23485,.T.);
#31256=EDGE_CURVE('',#25227,#25225,#23486,.T.);
#31257=EDGE_CURVE('',#25227,#25228,#11238,.T.);
#31258=EDGE_CURVE('',#25228,#25226,#23487,.T.);
#31259=EDGE_CURVE('',#25229,#25227,#23488,.T.);
#31260=EDGE_CURVE('',#25229,#25230,#11239,.T.);
#31261=EDGE_CURVE('',#25230,#25228,#23489,.T.);
#31262=EDGE_CURVE('',#25231,#25229,#23490,.T.);
#31263=EDGE_CURVE('',#25231,#25232,#11240,.T.);
#31264=EDGE_CURVE('',#25232,#25230,#23491,.T.);
#31265=EDGE_CURVE('',#25233,#25231,#23492,.T.);
#31266=EDGE_CURVE('',#25233,#25234,#11241,.T.);
#31267=EDGE_CURVE('',#25234,#25232,#23493,.T.);
#31268=EDGE_CURVE('',#25235,#25233,#23494,.T.);
#31269=EDGE_CURVE('',#25235,#25236,#11242,.T.);
#31270=EDGE_CURVE('',#25236,#25234,#23495,.T.);
#31271=EDGE_CURVE('',#25237,#25235,#11243,.T.);
#31272=EDGE_CURVE('',#25237,#25238,#11244,.T.);
#31273=EDGE_CURVE('',#25238,#25236,#11245,.T.);
#31274=EDGE_CURVE('',#25180,#25237,#23496,.T.);
#31275=EDGE_CURVE('',#25182,#25238,#23497,.T.);
#31276=EDGE_CURVE('',#25239,#25240,#23498,.T.);
#31277=EDGE_CURVE('',#25239,#25241,#11246,.T.);
#31278=EDGE_CURVE('',#25241,#25242,#23499,.T.);
#31279=EDGE_CURVE('',#25240,#25242,#11247,.T.);
#31280=EDGE_CURVE('',#25243,#25239,#23500,.T.);
#31281=EDGE_CURVE('',#25243,#25244,#11248,.T.);
#31282=EDGE_CURVE('',#25244,#25241,#23501,.T.);
#31283=EDGE_CURVE('',#25245,#25243,#23502,.T.);
#31284=EDGE_CURVE('',#25245,#25246,#11249,.T.);
#31285=EDGE_CURVE('',#25246,#25244,#23503,.T.);
#31286=EDGE_CURVE('',#25247,#25245,#23504,.T.);
#31287=EDGE_CURVE('',#25247,#25248,#11250,.T.);
#31288=EDGE_CURVE('',#25248,#25246,#23505,.T.);
#31289=EDGE_CURVE('',#25249,#25247,#23506,.T.);
#31290=EDGE_CURVE('',#25249,#25250,#11251,.T.);
#31291=EDGE_CURVE('',#25250,#25248,#23507,.T.);
#31292=EDGE_CURVE('',#25251,#25249,#23508,.T.);
#31293=EDGE_CURVE('',#25251,#25252,#11252,.T.);
#31294=EDGE_CURVE('',#25252,#25250,#23509,.T.);
#31295=EDGE_CURVE('',#25253,#25251,#23510,.T.);
#31296=EDGE_CURVE('',#25253,#25254,#11253,.T.);
#31297=EDGE_CURVE('',#25254,#25252,#23511,.T.);
#31298=EDGE_CURVE('',#25240,#25253,#23512,.T.);
#31299=EDGE_CURVE('',#25242,#25254,#23513,.T.);
#31300=EDGE_CURVE('',#25255,#25256,#23514,.T.);
#31301=EDGE_CURVE('',#25255,#25257,#11254,.T.);
#31302=EDGE_CURVE('',#25257,#25258,#23515,.T.);
#31303=EDGE_CURVE('',#25256,#25258,#11255,.T.);
#31304=EDGE_CURVE('',#25259,#25255,#23516,.T.);
#31305=EDGE_CURVE('',#25259,#25260,#11256,.T.);
#31306=EDGE_CURVE('',#25260,#25257,#23517,.T.);
#31307=EDGE_CURVE('',#25261,#25259,#23518,.T.);
#31308=EDGE_CURVE('',#25261,#25262,#11257,.T.);
#31309=EDGE_CURVE('',#25262,#25260,#23519,.T.);
#31310=EDGE_CURVE('',#25263,#25261,#23520,.T.);
#31311=EDGE_CURVE('',#25263,#25264,#11258,.T.);
#31312=EDGE_CURVE('',#25264,#25262,#23521,.T.);
#31313=EDGE_CURVE('',#25265,#25263,#23522,.T.);
#31314=EDGE_CURVE('',#25265,#25266,#11259,.T.);
#31315=EDGE_CURVE('',#25266,#25264,#23523,.T.);
#31316=EDGE_CURVE('',#25267,#25265,#23524,.T.);
#31317=EDGE_CURVE('',#25267,#25268,#11260,.T.);
#31318=EDGE_CURVE('',#25268,#25266,#23525,.T.);
#31319=EDGE_CURVE('',#25269,#25267,#23526,.T.);
#31320=EDGE_CURVE('',#25269,#25270,#11261,.T.);
#31321=EDGE_CURVE('',#25270,#25268,#23527,.T.);
#31322=EDGE_CURVE('',#25271,#25269,#23528,.T.);
#31323=EDGE_CURVE('',#25271,#25272,#11262,.T.);
#31324=EDGE_CURVE('',#25272,#25270,#23529,.T.);
#31325=EDGE_CURVE('',#25273,#25271,#23530,.T.);
#31326=EDGE_CURVE('',#25273,#25274,#11263,.T.);
#31327=EDGE_CURVE('',#25274,#25272,#23531,.T.);
#31328=EDGE_CURVE('',#25275,#25273,#23532,.T.);
#31329=EDGE_CURVE('',#25275,#25276,#11264,.T.);
#31330=EDGE_CURVE('',#25276,#25274,#23533,.T.);
#31331=EDGE_CURVE('',#25277,#25275,#23534,.T.);
#31332=EDGE_CURVE('',#25277,#25278,#11265,.T.);
#31333=EDGE_CURVE('',#25278,#25276,#23535,.T.);
#31334=EDGE_CURVE('',#25256,#25277,#23536,.T.);
#31335=EDGE_CURVE('',#25258,#25278,#23537,.T.);
#31336=EDGE_CURVE('',#25279,#25280,#23538,.T.);
#31337=EDGE_CURVE('',#25279,#25281,#11266,.T.);
#31338=EDGE_CURVE('',#25281,#25282,#23539,.T.);
#31339=EDGE_CURVE('',#25280,#25282,#11267,.T.);
#31340=EDGE_CURVE('',#25283,#25279,#23540,.T.);
#31341=EDGE_CURVE('',#25283,#25284,#11268,.T.);
#31342=EDGE_CURVE('',#25284,#25281,#23541,.T.);
#31343=EDGE_CURVE('',#25285,#25283,#23542,.T.);
#31344=EDGE_CURVE('',#25285,#25286,#11269,.T.);
#31345=EDGE_CURVE('',#25286,#25284,#23543,.T.);
#31346=EDGE_CURVE('',#25287,#25285,#23544,.T.);
#31347=EDGE_CURVE('',#25287,#25288,#11270,.T.);
#31348=EDGE_CURVE('',#25288,#25286,#23545,.T.);
#31349=EDGE_CURVE('',#25289,#25287,#23546,.T.);
#31350=EDGE_CURVE('',#25289,#25290,#11271,.T.);
#31351=EDGE_CURVE('',#25290,#25288,#23547,.T.);
#31352=EDGE_CURVE('',#25291,#25289,#23548,.T.);
#31353=EDGE_CURVE('',#25291,#25292,#11272,.T.);
#31354=EDGE_CURVE('',#25292,#25290,#23549,.T.);
#31355=EDGE_CURVE('',#25293,#25291,#23550,.T.);
#31356=EDGE_CURVE('',#25293,#25294,#11273,.T.);
#31357=EDGE_CURVE('',#25294,#25292,#23551,.T.);
#31358=EDGE_CURVE('',#25295,#25293,#23552,.T.);
#31359=EDGE_CURVE('',#25295,#25296,#11274,.T.);
#31360=EDGE_CURVE('',#25296,#25294,#23553,.T.);
#31361=EDGE_CURVE('',#25297,#25295,#23554,.T.);
#31362=EDGE_CURVE('',#25297,#25298,#11275,.T.);
#31363=EDGE_CURVE('',#25298,#25296,#23555,.T.);
#31364=EDGE_CURVE('',#25299,#25297,#11276,.T.);
#31365=EDGE_CURVE('',#25299,#25300,#11277,.T.);
#31366=EDGE_CURVE('',#25300,#25298,#11278,.T.);
#31367=EDGE_CURVE('',#25301,#25299,#23556,.T.);
#31368=EDGE_CURVE('',#25301,#25302,#11279,.T.);
#31369=EDGE_CURVE('',#25302,#25300,#23557,.T.);
#31370=EDGE_CURVE('',#25303,#25301,#23558,.T.);
#31371=EDGE_CURVE('',#25303,#25304,#11280,.T.);
#31372=EDGE_CURVE('',#25304,#25302,#23559,.T.);
#31373=EDGE_CURVE('',#25305,#25303,#23560,.T.);
#31374=EDGE_CURVE('',#25305,#25306,#11281,.T.);
#31375=EDGE_CURVE('',#25306,#25304,#23561,.T.);
#31376=EDGE_CURVE('',#25307,#25305,#23562,.T.);
#31377=EDGE_CURVE('',#25307,#25308,#11282,.T.);
#31378=EDGE_CURVE('',#25308,#25306,#23563,.T.);
#31379=EDGE_CURVE('',#25309,#25307,#23564,.T.);
#31380=EDGE_CURVE('',#25309,#25310,#11283,.T.);
#31381=EDGE_CURVE('',#25310,#25308,#23565,.T.);
#31382=EDGE_CURVE('',#25311,#25309,#23566,.T.);
#31383=EDGE_CURVE('',#25311,#25312,#11284,.T.);
#31384=EDGE_CURVE('',#25312,#25310,#23567,.T.);
#31385=EDGE_CURVE('',#25313,#25311,#23568,.T.);
#31386=EDGE_CURVE('',#25313,#25314,#11285,.T.);
#31387=EDGE_CURVE('',#25314,#25312,#23569,.T.);
#31388=EDGE_CURVE('',#25315,#25313,#23570,.T.);
#31389=EDGE_CURVE('',#25315,#25316,#11286,.T.);
#31390=EDGE_CURVE('',#25316,#25314,#23571,.T.);
#31391=EDGE_CURVE('',#25317,#25315,#23572,.T.);
#31392=EDGE_CURVE('',#25317,#25318,#11287,.T.);
#31393=EDGE_CURVE('',#25318,#25316,#23573,.T.);
#31394=EDGE_CURVE('',#25319,#25317,#11288,.T.);
#31395=EDGE_CURVE('',#25319,#25320,#11289,.T.);
#31396=EDGE_CURVE('',#25320,#25318,#11290,.T.);
#31397=EDGE_CURVE('',#25321,#25319,#11291,.T.);
#31398=EDGE_CURVE('',#25321,#25322,#11292,.T.);
#31399=EDGE_CURVE('',#25322,#25320,#11293,.T.);
#31400=EDGE_CURVE('',#25280,#25321,#11294,.T.);
#31401=EDGE_CURVE('',#25282,#25322,#11295,.T.);
#31402=EDGE_CURVE('',#25323,#25324,#23574,.T.);
#31403=EDGE_CURVE('',#25323,#25325,#11296,.T.);
#31404=EDGE_CURVE('',#25325,#25326,#23575,.T.);
#31405=EDGE_CURVE('',#25324,#25326,#11297,.T.);
#31406=EDGE_CURVE('',#25327,#25323,#23576,.T.);
#31407=EDGE_CURVE('',#25327,#25328,#11298,.T.);
#31408=EDGE_CURVE('',#25328,#25325,#23577,.T.);
#31409=EDGE_CURVE('',#25329,#25327,#23578,.T.);
#31410=EDGE_CURVE('',#25329,#25330,#11299,.T.);
#31411=EDGE_CURVE('',#25330,#25328,#23579,.T.);
#31412=EDGE_CURVE('',#25331,#25329,#23580,.T.);
#31413=EDGE_CURVE('',#25331,#25332,#11300,.T.);
#31414=EDGE_CURVE('',#25332,#25330,#23581,.T.);
#31415=EDGE_CURVE('',#25333,#25331,#23582,.T.);
#31416=EDGE_CURVE('',#25333,#25334,#11301,.T.);
#31417=EDGE_CURVE('',#25334,#25332,#23583,.T.);
#31418=EDGE_CURVE('',#25335,#25333,#23584,.T.);
#31419=EDGE_CURVE('',#25335,#25336,#11302,.T.);
#31420=EDGE_CURVE('',#25336,#25334,#23585,.T.);
#31421=EDGE_CURVE('',#25337,#25335,#23586,.T.);
#31422=EDGE_CURVE('',#25337,#25338,#11303,.T.);
#31423=EDGE_CURVE('',#25338,#25336,#23587,.T.);
#31424=EDGE_CURVE('',#25324,#25337,#23588,.T.);
#31425=EDGE_CURVE('',#25326,#25338,#23589,.T.);
#31426=EDGE_CURVE('',#25339,#25340,#23590,.T.);
#31427=EDGE_CURVE('',#25339,#25341,#11304,.T.);
#31428=EDGE_CURVE('',#25341,#25342,#23591,.T.);
#31429=EDGE_CURVE('',#25340,#25342,#11305,.T.);
#31430=EDGE_CURVE('',#25343,#25339,#23592,.T.);
#31431=EDGE_CURVE('',#25343,#25344,#11306,.T.);
#31432=EDGE_CURVE('',#25344,#25341,#23593,.T.);
#31433=EDGE_CURVE('',#25345,#25343,#23594,.T.);
#31434=EDGE_CURVE('',#25345,#25346,#11307,.T.);
#31435=EDGE_CURVE('',#25346,#25344,#23595,.T.);
#31436=EDGE_CURVE('',#25347,#25345,#23596,.T.);
#31437=EDGE_CURVE('',#25347,#25348,#11308,.T.);
#31438=EDGE_CURVE('',#25348,#25346,#23597,.T.);
#31439=EDGE_CURVE('',#25349,#25347,#23598,.T.);
#31440=EDGE_CURVE('',#25349,#25350,#11309,.T.);
#31441=EDGE_CURVE('',#25350,#25348,#23599,.T.);
#31442=EDGE_CURVE('',#25351,#25349,#23600,.T.);
#31443=EDGE_CURVE('',#25351,#25352,#11310,.T.);
#31444=EDGE_CURVE('',#25352,#25350,#23601,.T.);
#31445=EDGE_CURVE('',#25353,#25351,#23602,.T.);
#31446=EDGE_CURVE('',#25353,#25354,#11311,.T.);
#31447=EDGE_CURVE('',#25354,#25352,#23603,.T.);
#31448=EDGE_CURVE('',#25355,#25353,#23604,.T.);
#31449=EDGE_CURVE('',#25355,#25356,#11312,.T.);
#31450=EDGE_CURVE('',#25356,#25354,#23605,.T.);
#31451=EDGE_CURVE('',#25357,#25355,#23606,.T.);
#31452=EDGE_CURVE('',#25357,#25358,#11313,.T.);
#31453=EDGE_CURVE('',#25358,#25356,#23607,.T.);
#31454=EDGE_CURVE('',#25359,#25357,#23608,.T.);
#31455=EDGE_CURVE('',#25359,#25360,#11314,.T.);
#31456=EDGE_CURVE('',#25360,#25358,#23609,.T.);
#31457=EDGE_CURVE('',#25361,#25359,#23610,.T.);
#31458=EDGE_CURVE('',#25361,#25362,#11315,.T.);
#31459=EDGE_CURVE('',#25362,#25360,#23611,.T.);
#31460=EDGE_CURVE('',#25340,#25361,#23612,.T.);
#31461=EDGE_CURVE('',#25342,#25362,#23613,.T.);
#31462=EDGE_CURVE('',#25363,#25364,#11316,.T.);
#31463=EDGE_CURVE('',#25363,#25365,#11317,.T.);
#31464=EDGE_CURVE('',#25365,#25366,#11318,.T.);
#31465=EDGE_CURVE('',#25364,#25366,#11319,.T.);
#31466=EDGE_CURVE('',#25367,#25363,#23614,.T.);
#31467=EDGE_CURVE('',#25367,#25368,#11320,.T.);
#31468=EDGE_CURVE('',#25368,#25365,#23615,.T.);
#31469=EDGE_CURVE('',#25369,#25367,#23616,.T.);
#31470=EDGE_CURVE('',#25369,#25370,#11321,.T.);
#31471=EDGE_CURVE('',#25370,#25368,#23617,.T.);
#31472=EDGE_CURVE('',#25371,#25369,#11322,.T.);
#31473=EDGE_CURVE('',#25371,#25372,#11323,.T.);
#31474=EDGE_CURVE('',#25372,#25370,#11324,.T.);
#31475=EDGE_CURVE('',#25373,#25371,#23618,.T.);
#31476=EDGE_CURVE('',#25373,#25374,#11325,.T.);
#31477=EDGE_CURVE('',#25374,#25372,#23619,.T.);
#31478=EDGE_CURVE('',#25375,#25373,#23620,.T.);
#31479=EDGE_CURVE('',#25375,#25376,#11326,.T.);
#31480=EDGE_CURVE('',#25376,#25374,#23621,.T.);
#31481=EDGE_CURVE('',#25377,#25375,#11327,.T.);
#31482=EDGE_CURVE('',#25377,#25378,#11328,.T.);
#31483=EDGE_CURVE('',#25378,#25376,#11329,.T.);
#31484=EDGE_CURVE('',#25379,#25377,#11330,.T.);
#31485=EDGE_CURVE('',#25379,#25380,#11331,.T.);
#31486=EDGE_CURVE('',#25380,#25378,#11332,.T.);
#31487=EDGE_CURVE('',#25364,#25379,#11333,.T.);
#31488=EDGE_CURVE('',#25366,#25380,#11334,.T.);
#31489=EDGE_CURVE('',#25381,#25382,#23622,.T.);
#31490=EDGE_CURVE('',#25381,#25383,#11335,.T.);
#31491=EDGE_CURVE('',#25383,#25384,#23623,.T.);
#31492=EDGE_CURVE('',#25382,#25384,#11336,.T.);
#31493=EDGE_CURVE('',#25385,#25381,#23624,.T.);
#31494=EDGE_CURVE('',#25385,#25386,#11337,.T.);
#31495=EDGE_CURVE('',#25386,#25383,#23625,.T.);
#31496=EDGE_CURVE('',#25387,#25385,#23626,.T.);
#31497=EDGE_CURVE('',#25387,#25388,#11338,.T.);
#31498=EDGE_CURVE('',#25388,#25386,#23627,.T.);
#31499=EDGE_CURVE('',#25389,#25387,#23628,.T.);
#31500=EDGE_CURVE('',#25389,#25390,#11339,.T.);
#31501=EDGE_CURVE('',#25390,#25388,#23629,.T.);
#31502=EDGE_CURVE('',#25391,#25389,#23630,.T.);
#31503=EDGE_CURVE('',#25391,#25392,#11340,.T.);
#31504=EDGE_CURVE('',#25392,#25390,#23631,.T.);
#31505=EDGE_CURVE('',#25393,#25391,#23632,.T.);
#31506=EDGE_CURVE('',#25393,#25394,#11341,.T.);
#31507=EDGE_CURVE('',#25394,#25392,#23633,.T.);
#31508=EDGE_CURVE('',#25395,#25393,#23634,.T.);
#31509=EDGE_CURVE('',#25395,#25396,#11342,.T.);
#31510=EDGE_CURVE('',#25396,#25394,#23635,.T.);
#31511=EDGE_CURVE('',#25382,#25395,#23636,.T.);
#31512=EDGE_CURVE('',#25384,#25396,#23637,.T.);
#31513=EDGE_CURVE('',#25397,#25398,#23638,.T.);
#31514=EDGE_CURVE('',#25397,#25399,#11343,.T.);
#31515=EDGE_CURVE('',#25399,#25400,#23639,.T.);
#31516=EDGE_CURVE('',#25398,#25400,#11344,.T.);
#31517=EDGE_CURVE('',#25401,#25397,#23640,.T.);
#31518=EDGE_CURVE('',#25401,#25402,#11345,.T.);
#31519=EDGE_CURVE('',#25402,#25399,#23641,.T.);
#31520=EDGE_CURVE('',#25403,#25401,#23642,.T.);
#31521=EDGE_CURVE('',#25403,#25404,#11346,.T.);
#31522=EDGE_CURVE('',#25404,#25402,#23643,.T.);
#31523=EDGE_CURVE('',#25405,#25403,#23644,.T.);
#31524=EDGE_CURVE('',#25405,#25406,#11347,.T.);
#31525=EDGE_CURVE('',#25406,#25404,#23645,.T.);
#31526=EDGE_CURVE('',#25407,#25405,#23646,.T.);
#31527=EDGE_CURVE('',#25407,#25408,#11348,.T.);
#31528=EDGE_CURVE('',#25408,#25406,#23647,.T.);
#31529=EDGE_CURVE('',#25409,#25407,#23648,.T.);
#31530=EDGE_CURVE('',#25409,#25410,#11349,.T.);
#31531=EDGE_CURVE('',#25410,#25408,#23649,.T.);
#31532=EDGE_CURVE('',#25411,#25409,#23650,.T.);
#31533=EDGE_CURVE('',#25411,#25412,#11350,.T.);
#31534=EDGE_CURVE('',#25412,#25410,#23651,.T.);
#31535=EDGE_CURVE('',#25413,#25411,#23652,.T.);
#31536=EDGE_CURVE('',#25413,#25414,#11351,.T.);
#31537=EDGE_CURVE('',#25414,#25412,#23653,.T.);
#31538=EDGE_CURVE('',#25415,#25413,#23654,.T.);
#31539=EDGE_CURVE('',#25415,#25416,#11352,.T.);
#31540=EDGE_CURVE('',#25416,#25414,#23655,.T.);
#31541=EDGE_CURVE('',#25417,#25415,#23656,.T.);
#31542=EDGE_CURVE('',#25417,#25418,#11353,.T.);
#31543=EDGE_CURVE('',#25418,#25416,#23657,.T.);
#31544=EDGE_CURVE('',#25419,#25417,#23658,.T.);
#31545=EDGE_CURVE('',#25419,#25420,#11354,.T.);
#31546=EDGE_CURVE('',#25420,#25418,#23659,.T.);
#31547=EDGE_CURVE('',#25398,#25419,#23660,.T.);
#31548=EDGE_CURVE('',#25400,#25420,#23661,.T.);
#31549=EDGE_CURVE('',#25421,#25422,#23662,.T.);
#31550=EDGE_CURVE('',#25421,#25423,#11355,.T.);
#31551=EDGE_CURVE('',#25423,#25424,#23663,.T.);
#31552=EDGE_CURVE('',#25422,#25424,#11356,.T.);
#31553=EDGE_CURVE('',#25425,#25421,#23664,.T.);
#31554=EDGE_CURVE('',#25425,#25426,#11357,.T.);
#31555=EDGE_CURVE('',#25426,#25423,#23665,.T.);
#31556=EDGE_CURVE('',#25427,#25425,#23666,.T.);
#31557=EDGE_CURVE('',#25427,#25428,#11358,.T.);
#31558=EDGE_CURVE('',#25428,#25426,#23667,.T.);
#31559=EDGE_CURVE('',#25429,#25427,#23668,.T.);
#31560=EDGE_CURVE('',#25429,#25430,#11359,.T.);
#31561=EDGE_CURVE('',#25430,#25428,#23669,.T.);
#31562=EDGE_CURVE('',#25431,#25429,#23670,.T.);
#31563=EDGE_CURVE('',#25431,#25432,#11360,.T.);
#31564=EDGE_CURVE('',#25432,#25430,#23671,.T.);
#31565=EDGE_CURVE('',#25433,#25431,#23672,.T.);
#31566=EDGE_CURVE('',#25433,#25434,#11361,.T.);
#31567=EDGE_CURVE('',#25434,#25432,#23673,.T.);
#31568=EDGE_CURVE('',#25435,#25433,#23674,.T.);
#31569=EDGE_CURVE('',#25435,#25436,#11362,.T.);
#31570=EDGE_CURVE('',#25436,#25434,#23675,.T.);
#31571=EDGE_CURVE('',#25422,#25435,#23676,.T.);
#31572=EDGE_CURVE('',#25424,#25436,#23677,.T.);
#31573=EDGE_CURVE('',#25437,#25438,#23678,.T.);
#31574=EDGE_CURVE('',#25437,#25439,#11363,.T.);
#31575=EDGE_CURVE('',#25439,#25440,#23679,.T.);
#31576=EDGE_CURVE('',#25438,#25440,#11364,.T.);
#31577=EDGE_CURVE('',#25441,#25437,#23680,.T.);
#31578=EDGE_CURVE('',#25441,#25442,#11365,.T.);
#31579=EDGE_CURVE('',#25442,#25439,#23681,.T.);
#31580=EDGE_CURVE('',#25443,#25441,#23682,.T.);
#31581=EDGE_CURVE('',#25443,#25444,#11366,.T.);
#31582=EDGE_CURVE('',#25444,#25442,#23683,.T.);
#31583=EDGE_CURVE('',#25445,#25443,#23684,.T.);
#31584=EDGE_CURVE('',#25445,#25446,#11367,.T.);
#31585=EDGE_CURVE('',#25446,#25444,#23685,.T.);
#31586=EDGE_CURVE('',#25447,#25445,#23686,.T.);
#31587=EDGE_CURVE('',#25447,#25448,#11368,.T.);
#31588=EDGE_CURVE('',#25448,#25446,#23687,.T.);
#31589=EDGE_CURVE('',#25449,#25447,#23688,.T.);
#31590=EDGE_CURVE('',#25449,#25450,#11369,.T.);
#31591=EDGE_CURVE('',#25450,#25448,#23689,.T.);
#31592=EDGE_CURVE('',#25451,#25449,#23690,.T.);
#31593=EDGE_CURVE('',#25451,#25452,#11370,.T.);
#31594=EDGE_CURVE('',#25452,#25450,#23691,.T.);
#31595=EDGE_CURVE('',#25453,#25451,#23692,.T.);
#31596=EDGE_CURVE('',#25453,#25454,#11371,.T.);
#31597=EDGE_CURVE('',#25454,#25452,#23693,.T.);
#31598=EDGE_CURVE('',#25455,#25453,#23694,.T.);
#31599=EDGE_CURVE('',#25455,#25456,#11372,.T.);
#31600=EDGE_CURVE('',#25456,#25454,#23695,.T.);
#31601=EDGE_CURVE('',#25457,#25455,#23696,.T.);
#31602=EDGE_CURVE('',#25457,#25458,#11373,.T.);
#31603=EDGE_CURVE('',#25458,#25456,#23697,.T.);
#31604=EDGE_CURVE('',#25459,#25457,#23698,.T.);
#31605=EDGE_CURVE('',#25459,#25460,#11374,.T.);
#31606=EDGE_CURVE('',#25460,#25458,#23699,.T.);
#31607=EDGE_CURVE('',#25438,#25459,#23700,.T.);
#31608=EDGE_CURVE('',#25440,#25460,#23701,.T.);
#31609=EDGE_CURVE('',#25461,#25462,#11375,.T.);
#31610=EDGE_CURVE('',#25461,#25463,#11376,.T.);
#31611=EDGE_CURVE('',#25463,#25464,#11377,.T.);
#31612=EDGE_CURVE('',#25462,#25464,#11378,.T.);
#31613=EDGE_CURVE('',#25465,#25461,#23702,.T.);
#31614=EDGE_CURVE('',#25465,#25466,#11379,.T.);
#31615=EDGE_CURVE('',#25466,#25463,#23703,.T.);
#31616=EDGE_CURVE('',#25467,#25465,#23704,.T.);
#31617=EDGE_CURVE('',#25467,#25468,#11380,.T.);
#31618=EDGE_CURVE('',#25468,#25466,#23705,.T.);
#31619=EDGE_CURVE('',#25469,#25467,#11381,.T.);
#31620=EDGE_CURVE('',#25469,#25470,#11382,.T.);
#31621=EDGE_CURVE('',#25470,#25468,#11383,.T.);
#31622=EDGE_CURVE('',#25471,#25469,#23706,.T.);
#31623=EDGE_CURVE('',#25471,#25472,#11384,.T.);
#31624=EDGE_CURVE('',#25472,#25470,#23707,.T.);
#31625=EDGE_CURVE('',#25473,#25471,#23708,.T.);
#31626=EDGE_CURVE('',#25473,#25474,#11385,.T.);
#31627=EDGE_CURVE('',#25474,#25472,#23709,.T.);
#31628=EDGE_CURVE('',#25475,#25473,#11386,.T.);
#31629=EDGE_CURVE('',#25475,#25476,#11387,.T.);
#31630=EDGE_CURVE('',#25476,#25474,#11388,.T.);
#31631=EDGE_CURVE('',#25477,#25475,#11389,.T.);
#31632=EDGE_CURVE('',#25477,#25478,#11390,.T.);
#31633=EDGE_CURVE('',#25478,#25476,#11391,.T.);
#31634=EDGE_CURVE('',#25462,#25477,#11392,.T.);
#31635=EDGE_CURVE('',#25464,#25478,#11393,.T.);
#31636=EDGE_CURVE('',#25479,#25480,#23710,.T.);
#31637=EDGE_CURVE('',#25479,#25481,#11394,.T.);
#31638=EDGE_CURVE('',#25481,#25482,#23711,.T.);
#31639=EDGE_CURVE('',#25480,#25482,#11395,.T.);
#31640=EDGE_CURVE('',#25483,#25479,#23712,.T.);
#31641=EDGE_CURVE('',#25483,#25484,#11396,.T.);
#31642=EDGE_CURVE('',#25484,#25481,#23713,.T.);
#31643=EDGE_CURVE('',#25485,#25483,#23714,.T.);
#31644=EDGE_CURVE('',#25485,#25486,#11397,.T.);
#31645=EDGE_CURVE('',#25486,#25484,#23715,.T.);
#31646=EDGE_CURVE('',#25487,#25485,#23716,.T.);
#31647=EDGE_CURVE('',#25487,#25488,#11398,.T.);
#31648=EDGE_CURVE('',#25488,#25486,#23717,.T.);
#31649=EDGE_CURVE('',#25489,#25487,#23718,.T.);
#31650=EDGE_CURVE('',#25489,#25490,#11399,.T.);
#31651=EDGE_CURVE('',#25490,#25488,#23719,.T.);
#31652=EDGE_CURVE('',#25491,#25489,#23720,.T.);
#31653=EDGE_CURVE('',#25491,#25492,#11400,.T.);
#31654=EDGE_CURVE('',#25492,#25490,#23721,.T.);
#31655=EDGE_CURVE('',#25493,#25491,#23722,.T.);
#31656=EDGE_CURVE('',#25493,#25494,#11401,.T.);
#31657=EDGE_CURVE('',#25494,#25492,#23723,.T.);
#31658=EDGE_CURVE('',#25480,#25493,#23724,.T.);
#31659=EDGE_CURVE('',#25482,#25494,#23725,.T.);
#31660=EDGE_CURVE('',#25495,#25496,#23726,.T.);
#31661=EDGE_CURVE('',#25495,#25497,#11402,.T.);
#31662=EDGE_CURVE('',#25497,#25498,#23727,.T.);
#31663=EDGE_CURVE('',#25496,#25498,#11403,.T.);
#31664=EDGE_CURVE('',#25499,#25495,#23728,.T.);
#31665=EDGE_CURVE('',#25499,#25500,#11404,.T.);
#31666=EDGE_CURVE('',#25500,#25497,#23729,.T.);
#31667=EDGE_CURVE('',#25501,#25499,#23730,.T.);
#31668=EDGE_CURVE('',#25501,#25502,#11405,.T.);
#31669=EDGE_CURVE('',#25502,#25500,#23731,.T.);
#31670=EDGE_CURVE('',#25503,#25501,#23732,.T.);
#31671=EDGE_CURVE('',#25503,#25504,#11406,.T.);
#31672=EDGE_CURVE('',#25504,#25502,#23733,.T.);
#31673=EDGE_CURVE('',#25505,#25503,#23734,.T.);
#31674=EDGE_CURVE('',#25505,#25506,#11407,.T.);
#31675=EDGE_CURVE('',#25506,#25504,#23735,.T.);
#31676=EDGE_CURVE('',#25507,#25505,#23736,.T.);
#31677=EDGE_CURVE('',#25507,#25508,#11408,.T.);
#31678=EDGE_CURVE('',#25508,#25506,#23737,.T.);
#31679=EDGE_CURVE('',#25509,#25507,#23738,.T.);
#31680=EDGE_CURVE('',#25509,#25510,#11409,.T.);
#31681=EDGE_CURVE('',#25510,#25508,#23739,.T.);
#31682=EDGE_CURVE('',#25511,#25509,#23740,.T.);
#31683=EDGE_CURVE('',#25511,#25512,#11410,.T.);
#31684=EDGE_CURVE('',#25512,#25510,#23741,.T.);
#31685=EDGE_CURVE('',#25513,#25511,#23742,.T.);
#31686=EDGE_CURVE('',#25513,#25514,#11411,.T.);
#31687=EDGE_CURVE('',#25514,#25512,#23743,.T.);
#31688=EDGE_CURVE('',#25515,#25513,#23744,.T.);
#31689=EDGE_CURVE('',#25515,#25516,#11412,.T.);
#31690=EDGE_CURVE('',#25516,#25514,#23745,.T.);
#31691=EDGE_CURVE('',#25517,#25515,#23746,.T.);
#31692=EDGE_CURVE('',#25517,#25518,#11413,.T.);
#31693=EDGE_CURVE('',#25518,#25516,#23747,.T.);
#31694=EDGE_CURVE('',#25496,#25517,#23748,.T.);
#31695=EDGE_CURVE('',#25498,#25518,#23749,.T.);
#31696=EDGE_CURVE('',#25519,#25520,#23750,.T.);
#31697=EDGE_CURVE('',#25519,#25521,#11414,.T.);
#31698=EDGE_CURVE('',#25521,#25522,#23751,.T.);
#31699=EDGE_CURVE('',#25520,#25522,#11415,.T.);
#31700=EDGE_CURVE('',#25523,#25519,#23752,.T.);
#31701=EDGE_CURVE('',#25523,#25524,#11416,.T.);
#31702=EDGE_CURVE('',#25524,#25521,#23753,.T.);
#31703=EDGE_CURVE('',#25525,#25523,#23754,.T.);
#31704=EDGE_CURVE('',#25525,#25526,#11417,.T.);
#31705=EDGE_CURVE('',#25526,#25524,#23755,.T.);
#31706=EDGE_CURVE('',#25527,#25525,#23756,.T.);
#31707=EDGE_CURVE('',#25527,#25528,#11418,.T.);
#31708=EDGE_CURVE('',#25528,#25526,#23757,.T.);
#31709=EDGE_CURVE('',#25529,#25527,#23758,.T.);
#31710=EDGE_CURVE('',#25529,#25530,#11419,.T.);
#31711=EDGE_CURVE('',#25530,#25528,#23759,.T.);
#31712=EDGE_CURVE('',#25531,#25529,#23760,.T.);
#31713=EDGE_CURVE('',#25531,#25532,#11420,.T.);
#31714=EDGE_CURVE('',#25532,#25530,#23761,.T.);
#31715=EDGE_CURVE('',#25533,#25531,#23762,.T.);
#31716=EDGE_CURVE('',#25533,#25534,#11421,.T.);
#31717=EDGE_CURVE('',#25534,#25532,#23763,.T.);
#31718=EDGE_CURVE('',#25535,#25533,#23764,.T.);
#31719=EDGE_CURVE('',#25535,#25536,#11422,.T.);
#31720=EDGE_CURVE('',#25536,#25534,#23765,.T.);
#31721=EDGE_CURVE('',#25537,#25535,#23766,.T.);
#31722=EDGE_CURVE('',#25537,#25538,#11423,.T.);
#31723=EDGE_CURVE('',#25538,#25536,#23767,.T.);
#31724=EDGE_CURVE('',#25539,#25537,#11424,.T.);
#31725=EDGE_CURVE('',#25539,#25540,#11425,.T.);
#31726=EDGE_CURVE('',#25540,#25538,#11426,.T.);
#31727=EDGE_CURVE('',#25541,#25539,#23768,.T.);
#31728=EDGE_CURVE('',#25541,#25542,#11427,.T.);
#31729=EDGE_CURVE('',#25542,#25540,#23769,.T.);
#31730=EDGE_CURVE('',#25543,#25541,#23770,.T.);
#31731=EDGE_CURVE('',#25543,#25544,#11428,.T.);
#31732=EDGE_CURVE('',#25544,#25542,#23771,.T.);
#31733=EDGE_CURVE('',#25545,#25543,#23772,.T.);
#31734=EDGE_CURVE('',#25545,#25546,#11429,.T.);
#31735=EDGE_CURVE('',#25546,#25544,#23773,.T.);
#31736=EDGE_CURVE('',#25547,#25545,#23774,.T.);
#31737=EDGE_CURVE('',#25547,#25548,#11430,.T.);
#31738=EDGE_CURVE('',#25548,#25546,#23775,.T.);
#31739=EDGE_CURVE('',#25549,#25547,#23776,.T.);
#31740=EDGE_CURVE('',#25549,#25550,#11431,.T.);
#31741=EDGE_CURVE('',#25550,#25548,#23777,.T.);
#31742=EDGE_CURVE('',#25551,#25549,#23778,.T.);
#31743=EDGE_CURVE('',#25551,#25552,#11432,.T.);
#31744=EDGE_CURVE('',#25552,#25550,#23779,.T.);
#31745=EDGE_CURVE('',#25553,#25551,#23780,.T.);
#31746=EDGE_CURVE('',#25553,#25554,#11433,.T.);
#31747=EDGE_CURVE('',#25554,#25552,#23781,.T.);
#31748=EDGE_CURVE('',#25555,#25553,#23782,.T.);
#31749=EDGE_CURVE('',#25555,#25556,#11434,.T.);
#31750=EDGE_CURVE('',#25556,#25554,#23783,.T.);
#31751=EDGE_CURVE('',#25557,#25555,#23784,.T.);
#31752=EDGE_CURVE('',#25557,#25558,#11435,.T.);
#31753=EDGE_CURVE('',#25558,#25556,#23785,.T.);
#31754=EDGE_CURVE('',#25559,#25557,#11436,.T.);
#31755=EDGE_CURVE('',#25559,#25560,#11437,.T.);
#31756=EDGE_CURVE('',#25560,#25558,#11438,.T.);
#31757=EDGE_CURVE('',#25561,#25559,#11439,.T.);
#31758=EDGE_CURVE('',#25561,#25562,#11440,.T.);
#31759=EDGE_CURVE('',#25562,#25560,#11441,.T.);
#31760=EDGE_CURVE('',#25520,#25561,#11442,.T.);
#31761=EDGE_CURVE('',#25522,#25562,#11443,.T.);
#31762=EDGE_CURVE('',#25563,#25564,#23786,.T.);
#31763=EDGE_CURVE('',#25563,#25565,#11444,.T.);
#31764=EDGE_CURVE('',#25565,#25566,#23787,.T.);
#31765=EDGE_CURVE('',#25564,#25566,#11445,.T.);
#31766=EDGE_CURVE('',#25567,#25563,#23788,.T.);
#31767=EDGE_CURVE('',#25567,#25568,#11446,.T.);
#31768=EDGE_CURVE('',#25568,#25565,#23789,.T.);
#31769=EDGE_CURVE('',#25569,#25567,#23790,.T.);
#31770=EDGE_CURVE('',#25569,#25570,#11447,.T.);
#31771=EDGE_CURVE('',#25570,#25568,#23791,.T.);
#31772=EDGE_CURVE('',#25571,#25569,#23792,.T.);
#31773=EDGE_CURVE('',#25571,#25572,#11448,.T.);
#31774=EDGE_CURVE('',#25572,#25570,#23793,.T.);
#31775=EDGE_CURVE('',#25573,#25571,#23794,.T.);
#31776=EDGE_CURVE('',#25573,#25574,#11449,.T.);
#31777=EDGE_CURVE('',#25574,#25572,#23795,.T.);
#31778=EDGE_CURVE('',#25575,#25573,#23796,.T.);
#31779=EDGE_CURVE('',#25575,#25576,#11450,.T.);
#31780=EDGE_CURVE('',#25576,#25574,#23797,.T.);
#31781=EDGE_CURVE('',#25577,#25575,#23798,.T.);
#31782=EDGE_CURVE('',#25577,#25578,#11451,.T.);
#31783=EDGE_CURVE('',#25578,#25576,#23799,.T.);
#31784=EDGE_CURVE('',#25564,#25577,#23800,.T.);
#31785=EDGE_CURVE('',#25566,#25578,#23801,.T.);
#31786=EDGE_CURVE('',#25579,#25580,#23802,.T.);
#31787=EDGE_CURVE('',#25579,#25581,#11452,.T.);
#31788=EDGE_CURVE('',#25581,#25582,#23803,.T.);
#31789=EDGE_CURVE('',#25580,#25582,#11453,.T.);
#31790=EDGE_CURVE('',#25583,#25579,#23804,.T.);
#31791=EDGE_CURVE('',#25583,#25584,#11454,.T.);
#31792=EDGE_CURVE('',#25584,#25581,#23805,.T.);
#31793=EDGE_CURVE('',#25585,#25583,#23806,.T.);
#31794=EDGE_CURVE('',#25585,#25586,#11455,.T.);
#31795=EDGE_CURVE('',#25586,#25584,#23807,.T.);
#31796=EDGE_CURVE('',#25587,#25585,#23808,.T.);
#31797=EDGE_CURVE('',#25587,#25588,#11456,.T.);
#31798=EDGE_CURVE('',#25588,#25586,#23809,.T.);
#31799=EDGE_CURVE('',#25589,#25587,#23810,.T.);
#31800=EDGE_CURVE('',#25589,#25590,#11457,.T.);
#31801=EDGE_CURVE('',#25590,#25588,#23811,.T.);
#31802=EDGE_CURVE('',#25591,#25589,#23812,.T.);
#31803=EDGE_CURVE('',#25591,#25592,#11458,.T.);
#31804=EDGE_CURVE('',#25592,#25590,#23813,.T.);
#31805=EDGE_CURVE('',#25593,#25591,#23814,.T.);
#31806=EDGE_CURVE('',#25593,#25594,#11459,.T.);
#31807=EDGE_CURVE('',#25594,#25592,#23815,.T.);
#31808=EDGE_CURVE('',#25595,#25593,#23816,.T.);
#31809=EDGE_CURVE('',#25595,#25596,#11460,.T.);
#31810=EDGE_CURVE('',#25596,#25594,#23817,.T.);
#31811=EDGE_CURVE('',#25597,#25595,#23818,.T.);
#31812=EDGE_CURVE('',#25597,#25598,#11461,.T.);
#31813=EDGE_CURVE('',#25598,#25596,#23819,.T.);
#31814=EDGE_CURVE('',#25599,#25597,#23820,.T.);
#31815=EDGE_CURVE('',#25599,#25600,#11462,.T.);
#31816=EDGE_CURVE('',#25600,#25598,#23821,.T.);
#31817=EDGE_CURVE('',#25601,#25599,#23822,.T.);
#31818=EDGE_CURVE('',#25601,#25602,#11463,.T.);
#31819=EDGE_CURVE('',#25602,#25600,#23823,.T.);
#31820=EDGE_CURVE('',#25580,#25601,#23824,.T.);
#31821=EDGE_CURVE('',#25582,#25602,#23825,.T.);
#31822=EDGE_CURVE('',#25603,#25604,#23826,.T.);
#31823=EDGE_CURVE('',#25603,#25605,#11464,.T.);
#31824=EDGE_CURVE('',#25605,#25606,#23827,.T.);
#31825=EDGE_CURVE('',#25604,#25606,#11465,.T.);
#31826=EDGE_CURVE('',#25607,#25603,#23828,.T.);
#31827=EDGE_CURVE('',#25607,#25608,#11466,.T.);
#31828=EDGE_CURVE('',#25608,#25605,#23829,.T.);
#31829=EDGE_CURVE('',#25609,#25607,#23830,.T.);
#31830=EDGE_CURVE('',#25609,#25610,#11467,.T.);
#31831=EDGE_CURVE('',#25610,#25608,#23831,.T.);
#31832=EDGE_CURVE('',#25611,#25609,#23832,.T.);
#31833=EDGE_CURVE('',#25611,#25612,#11468,.T.);
#31834=EDGE_CURVE('',#25612,#25610,#23833,.T.);
#31835=EDGE_CURVE('',#25613,#25611,#23834,.T.);
#31836=EDGE_CURVE('',#25613,#25614,#11469,.T.);
#31837=EDGE_CURVE('',#25614,#25612,#23835,.T.);
#31838=EDGE_CURVE('',#25615,#25613,#23836,.T.);
#31839=EDGE_CURVE('',#25615,#25616,#11470,.T.);
#31840=EDGE_CURVE('',#25616,#25614,#23837,.T.);
#31841=EDGE_CURVE('',#25617,#25615,#23838,.T.);
#31842=EDGE_CURVE('',#25617,#25618,#11471,.T.);
#31843=EDGE_CURVE('',#25618,#25616,#23839,.T.);
#31844=EDGE_CURVE('',#25619,#25617,#23840,.T.);
#31845=EDGE_CURVE('',#25619,#25620,#11472,.T.);
#31846=EDGE_CURVE('',#25620,#25618,#23841,.T.);
#31847=EDGE_CURVE('',#25621,#25619,#23842,.T.);
#31848=EDGE_CURVE('',#25621,#25622,#11473,.T.);
#31849=EDGE_CURVE('',#25622,#25620,#23843,.T.);
#31850=EDGE_CURVE('',#25623,#25621,#23844,.T.);
#31851=EDGE_CURVE('',#25623,#25624,#11474,.T.);
#31852=EDGE_CURVE('',#25624,#25622,#23845,.T.);
#31853=EDGE_CURVE('',#25625,#25623,#23846,.T.);
#31854=EDGE_CURVE('',#25625,#25626,#11475,.T.);
#31855=EDGE_CURVE('',#25626,#25624,#23847,.T.);
#31856=EDGE_CURVE('',#25627,#25625,#23848,.T.);
#31857=EDGE_CURVE('',#25627,#25628,#11476,.T.);
#31858=EDGE_CURVE('',#25628,#25626,#23849,.T.);
#31859=EDGE_CURVE('',#25629,#25627,#11477,.T.);
#31860=EDGE_CURVE('',#25629,#25630,#11478,.T.);
#31861=EDGE_CURVE('',#25630,#25628,#11479,.T.);
#31862=EDGE_CURVE('',#25631,#25629,#23850,.T.);
#31863=EDGE_CURVE('',#25631,#25632,#11480,.T.);
#31864=EDGE_CURVE('',#25632,#25630,#23851,.T.);
#31865=EDGE_CURVE('',#25633,#25631,#23852,.T.);
#31866=EDGE_CURVE('',#25633,#25634,#11481,.T.);
#31867=EDGE_CURVE('',#25634,#25632,#23853,.T.);
#31868=EDGE_CURVE('',#25635,#25633,#23854,.T.);
#31869=EDGE_CURVE('',#25635,#25636,#11482,.T.);
#31870=EDGE_CURVE('',#25636,#25634,#23855,.T.);
#31871=EDGE_CURVE('',#25637,#25635,#23856,.T.);
#31872=EDGE_CURVE('',#25637,#25638,#11483,.T.);
#31873=EDGE_CURVE('',#25638,#25636,#23857,.T.);
#31874=EDGE_CURVE('',#25639,#25637,#23858,.T.);
#31875=EDGE_CURVE('',#25639,#25640,#11484,.T.);
#31876=EDGE_CURVE('',#25640,#25638,#23859,.T.);
#31877=EDGE_CURVE('',#25641,#25639,#23860,.T.);
#31878=EDGE_CURVE('',#25641,#25642,#11485,.T.);
#31879=EDGE_CURVE('',#25642,#25640,#23861,.T.);
#31880=EDGE_CURVE('',#25643,#25641,#23862,.T.);
#31881=EDGE_CURVE('',#25643,#25644,#11486,.T.);
#31882=EDGE_CURVE('',#25644,#25642,#23863,.T.);
#31883=EDGE_CURVE('',#25645,#25643,#11487,.T.);
#31884=EDGE_CURVE('',#25645,#25646,#11488,.T.);
#31885=EDGE_CURVE('',#25646,#25644,#11489,.T.);
#31886=EDGE_CURVE('',#25647,#25645,#23864,.T.);
#31887=EDGE_CURVE('',#25647,#25648,#11490,.T.);
#31888=EDGE_CURVE('',#25648,#25646,#23865,.T.);
#31889=EDGE_CURVE('',#25649,#25647,#23866,.T.);
#31890=EDGE_CURVE('',#25649,#25650,#11491,.T.);
#31891=EDGE_CURVE('',#25650,#25648,#23867,.T.);
#31892=EDGE_CURVE('',#25651,#25649,#23868,.T.);
#31893=EDGE_CURVE('',#25651,#25652,#11492,.T.);
#31894=EDGE_CURVE('',#25652,#25650,#23869,.T.);
#31895=EDGE_CURVE('',#25653,#25651,#23870,.T.);
#31896=EDGE_CURVE('',#25653,#25654,#11493,.T.);
#31897=EDGE_CURVE('',#25654,#25652,#23871,.T.);
#31898=EDGE_CURVE('',#25655,#25653,#23872,.T.);
#31899=EDGE_CURVE('',#25655,#25656,#11494,.T.);
#31900=EDGE_CURVE('',#25656,#25654,#23873,.T.);
#31901=EDGE_CURVE('',#25657,#25655,#23874,.T.);
#31902=EDGE_CURVE('',#25657,#25658,#11495,.T.);
#31903=EDGE_CURVE('',#25658,#25656,#23875,.T.);
#31904=EDGE_CURVE('',#25659,#25657,#23876,.T.);
#31905=EDGE_CURVE('',#25659,#25660,#11496,.T.);
#31906=EDGE_CURVE('',#25660,#25658,#23877,.T.);
#31907=EDGE_CURVE('',#25661,#25659,#11497,.T.);
#31908=EDGE_CURVE('',#25661,#25662,#11498,.T.);
#31909=EDGE_CURVE('',#25662,#25660,#11499,.T.);
#31910=EDGE_CURVE('',#25604,#25661,#23878,.T.);
#31911=EDGE_CURVE('',#25606,#25662,#23879,.T.);
#31912=EDGE_CURVE('',#25663,#25664,#23880,.T.);
#31913=EDGE_CURVE('',#25663,#25665,#11500,.T.);
#31914=EDGE_CURVE('',#25665,#25666,#23881,.T.);
#31915=EDGE_CURVE('',#25664,#25666,#11501,.T.);
#31916=EDGE_CURVE('',#25667,#25663,#23882,.T.);
#31917=EDGE_CURVE('',#25667,#25668,#11502,.T.);
#31918=EDGE_CURVE('',#25668,#25665,#23883,.T.);
#31919=EDGE_CURVE('',#25669,#25667,#23884,.T.);
#31920=EDGE_CURVE('',#25669,#25670,#11503,.T.);
#31921=EDGE_CURVE('',#25670,#25668,#23885,.T.);
#31922=EDGE_CURVE('',#25671,#25669,#23886,.T.);
#31923=EDGE_CURVE('',#25671,#25672,#11504,.T.);
#31924=EDGE_CURVE('',#25672,#25670,#23887,.T.);
#31925=EDGE_CURVE('',#25673,#25671,#23888,.T.);
#31926=EDGE_CURVE('',#25673,#25674,#11505,.T.);
#31927=EDGE_CURVE('',#25674,#25672,#23889,.T.);
#31928=EDGE_CURVE('',#25675,#25673,#23890,.T.);
#31929=EDGE_CURVE('',#25675,#25676,#11506,.T.);
#31930=EDGE_CURVE('',#25676,#25674,#23891,.T.);
#31931=EDGE_CURVE('',#25677,#25675,#23892,.T.);
#31932=EDGE_CURVE('',#25677,#25678,#11507,.T.);
#31933=EDGE_CURVE('',#25678,#25676,#23893,.T.);
#31934=EDGE_CURVE('',#25664,#25677,#23894,.T.);
#31935=EDGE_CURVE('',#25666,#25678,#23895,.T.);
#31936=EDGE_CURVE('',#25679,#25680,#23896,.T.);
#31937=EDGE_CURVE('',#25679,#25681,#11508,.T.);
#31938=EDGE_CURVE('',#25681,#25682,#23897,.T.);
#31939=EDGE_CURVE('',#25680,#25682,#11509,.T.);
#31940=EDGE_CURVE('',#25683,#25679,#23898,.T.);
#31941=EDGE_CURVE('',#25683,#25684,#11510,.T.);
#31942=EDGE_CURVE('',#25684,#25681,#23899,.T.);
#31943=EDGE_CURVE('',#25685,#25683,#23900,.T.);
#31944=EDGE_CURVE('',#25685,#25686,#11511,.T.);
#31945=EDGE_CURVE('',#25686,#25684,#23901,.T.);
#31946=EDGE_CURVE('',#25687,#25685,#23902,.T.);
#31947=EDGE_CURVE('',#25687,#25688,#11512,.T.);
#31948=EDGE_CURVE('',#25688,#25686,#23903,.T.);
#31949=EDGE_CURVE('',#25689,#25687,#23904,.T.);
#31950=EDGE_CURVE('',#25689,#25690,#11513,.T.);
#31951=EDGE_CURVE('',#25690,#25688,#23905,.T.);
#31952=EDGE_CURVE('',#25691,#25689,#23906,.T.);
#31953=EDGE_CURVE('',#25691,#25692,#11514,.T.);
#31954=EDGE_CURVE('',#25692,#25690,#23907,.T.);
#31955=EDGE_CURVE('',#25693,#25691,#23908,.T.);
#31956=EDGE_CURVE('',#25693,#25694,#11515,.T.);
#31957=EDGE_CURVE('',#25694,#25692,#23909,.T.);
#31958=EDGE_CURVE('',#25695,#25693,#23910,.T.);
#31959=EDGE_CURVE('',#25695,#25696,#11516,.T.);
#31960=EDGE_CURVE('',#25696,#25694,#23911,.T.);
#31961=EDGE_CURVE('',#25697,#25695,#23912,.T.);
#31962=EDGE_CURVE('',#25697,#25698,#11517,.T.);
#31963=EDGE_CURVE('',#25698,#25696,#23913,.T.);
#31964=EDGE_CURVE('',#25699,#25697,#23914,.T.);
#31965=EDGE_CURVE('',#25699,#25700,#11518,.T.);
#31966=EDGE_CURVE('',#25700,#25698,#23915,.T.);
#31967=EDGE_CURVE('',#25701,#25699,#23916,.T.);
#31968=EDGE_CURVE('',#25701,#25702,#11519,.T.);
#31969=EDGE_CURVE('',#25702,#25700,#23917,.T.);
#31970=EDGE_CURVE('',#25680,#25701,#23918,.T.);
#31971=EDGE_CURVE('',#25682,#25702,#23919,.T.);
#31972=EDGE_CURVE('',#25703,#25704,#11520,.T.);
#31973=EDGE_CURVE('',#25703,#25705,#11521,.T.);
#31974=EDGE_CURVE('',#25705,#25706,#11522,.T.);
#31975=EDGE_CURVE('',#25704,#25706,#11523,.T.);
#31976=EDGE_CURVE('',#25707,#25703,#11524,.T.);
#31977=EDGE_CURVE('',#25707,#25708,#11525,.T.);
#31978=EDGE_CURVE('',#25708,#25705,#11526,.T.);
#31979=EDGE_CURVE('',#25704,#25707,#11527,.T.);
#31980=EDGE_CURVE('',#25706,#25708,#11528,.T.);
#31981=EDGE_CURVE('',#25709,#25710,#11529,.T.);
#31982=EDGE_CURVE('',#25709,#25711,#11530,.T.);
#31983=EDGE_CURVE('',#25711,#25712,#11531,.T.);
#31984=EDGE_CURVE('',#25710,#25712,#11532,.T.);
#31985=EDGE_CURVE('',#25713,#25709,#11533,.T.);
#31986=EDGE_CURVE('',#25713,#25714,#11534,.T.);
#31987=EDGE_CURVE('',#25714,#25711,#11535,.T.);
#31988=EDGE_CURVE('',#25715,#25713,#11536,.T.);
#31989=EDGE_CURVE('',#25715,#25716,#11537,.T.);
#31990=EDGE_CURVE('',#25716,#25714,#11538,.T.);
#31991=EDGE_CURVE('',#25717,#25715,#11539,.T.);
#31992=EDGE_CURVE('',#25717,#25718,#11540,.T.);
#31993=EDGE_CURVE('',#25718,#25716,#11541,.T.);
#31994=EDGE_CURVE('',#25719,#25717,#11542,.T.);
#31995=EDGE_CURVE('',#25719,#25720,#11543,.T.);
#31996=EDGE_CURVE('',#25720,#25718,#11544,.T.);
#31997=EDGE_CURVE('',#25721,#25719,#11545,.T.);
#31998=EDGE_CURVE('',#25721,#25722,#11546,.T.);
#31999=EDGE_CURVE('',#25722,#25720,#11547,.T.);
#32000=EDGE_CURVE('',#25723,#25721,#11548,.T.);
#32001=EDGE_CURVE('',#25723,#25724,#11549,.T.);
#32002=EDGE_CURVE('',#25724,#25722,#11550,.T.);
#32003=EDGE_CURVE('',#25725,#25723,#11551,.T.);
#32004=EDGE_CURVE('',#25725,#25726,#11552,.T.);
#32005=EDGE_CURVE('',#25726,#25724,#11553,.T.);
#32006=EDGE_CURVE('',#25727,#25725,#11554,.T.);
#32007=EDGE_CURVE('',#25727,#25728,#11555,.T.);
#32008=EDGE_CURVE('',#25728,#25726,#11556,.T.);
#32009=EDGE_CURVE('',#25729,#25727,#11557,.T.);
#32010=EDGE_CURVE('',#25729,#25730,#11558,.T.);
#32011=EDGE_CURVE('',#25730,#25728,#11559,.T.);
#32012=EDGE_CURVE('',#25710,#25729,#11560,.T.);
#32013=EDGE_CURVE('',#25712,#25730,#11561,.T.);
#32014=EDGE_CURVE('',#25731,#25732,#23920,.T.);
#32015=EDGE_CURVE('',#25731,#25733,#11562,.T.);
#32016=EDGE_CURVE('',#25733,#25734,#23921,.T.);
#32017=EDGE_CURVE('',#25732,#25734,#11563,.T.);
#32018=EDGE_CURVE('',#25735,#25731,#23922,.T.);
#32019=EDGE_CURVE('',#25735,#25736,#11564,.T.);
#32020=EDGE_CURVE('',#25736,#25733,#23923,.T.);
#32021=EDGE_CURVE('',#25737,#25735,#23924,.T.);
#32022=EDGE_CURVE('',#25737,#25738,#11565,.T.);
#32023=EDGE_CURVE('',#25738,#25736,#23925,.T.);
#32024=EDGE_CURVE('',#25739,#25737,#23926,.T.);
#32025=EDGE_CURVE('',#25739,#25740,#11566,.T.);
#32026=EDGE_CURVE('',#25740,#25738,#23927,.T.);
#32027=EDGE_CURVE('',#25741,#25739,#23928,.T.);
#32028=EDGE_CURVE('',#25741,#25742,#11567,.T.);
#32029=EDGE_CURVE('',#25742,#25740,#23929,.T.);
#32030=EDGE_CURVE('',#25743,#25741,#23930,.T.);
#32031=EDGE_CURVE('',#25743,#25744,#11568,.T.);
#32032=EDGE_CURVE('',#25744,#25742,#23931,.T.);
#32033=EDGE_CURVE('',#25745,#25743,#23932,.T.);
#32034=EDGE_CURVE('',#25745,#25746,#11569,.T.);
#32035=EDGE_CURVE('',#25746,#25744,#23933,.T.);
#32036=EDGE_CURVE('',#25732,#25745,#23934,.T.);
#32037=EDGE_CURVE('',#25734,#25746,#23935,.T.);
#32038=EDGE_CURVE('',#25747,#25748,#23936,.T.);
#32039=EDGE_CURVE('',#25747,#25749,#11570,.T.);
#32040=EDGE_CURVE('',#25749,#25750,#23937,.T.);
#32041=EDGE_CURVE('',#25748,#25750,#11571,.T.);
#32042=EDGE_CURVE('',#25751,#25747,#23938,.T.);
#32043=EDGE_CURVE('',#25751,#25752,#11572,.T.);
#32044=EDGE_CURVE('',#25752,#25749,#23939,.T.);
#32045=EDGE_CURVE('',#25753,#25751,#23940,.T.);
#32046=EDGE_CURVE('',#25753,#25754,#11573,.T.);
#32047=EDGE_CURVE('',#25754,#25752,#23941,.T.);
#32048=EDGE_CURVE('',#25755,#25753,#23942,.T.);
#32049=EDGE_CURVE('',#25755,#25756,#11574,.T.);
#32050=EDGE_CURVE('',#25756,#25754,#23943,.T.);
#32051=EDGE_CURVE('',#25757,#25755,#23944,.T.);
#32052=EDGE_CURVE('',#25757,#25758,#11575,.T.);
#32053=EDGE_CURVE('',#25758,#25756,#23945,.T.);
#32054=EDGE_CURVE('',#25759,#25757,#23946,.T.);
#32055=EDGE_CURVE('',#25759,#25760,#11576,.T.);
#32056=EDGE_CURVE('',#25760,#25758,#23947,.T.);
#32057=EDGE_CURVE('',#25761,#25759,#23948,.T.);
#32058=EDGE_CURVE('',#25761,#25762,#11577,.T.);
#32059=EDGE_CURVE('',#25762,#25760,#23949,.T.);
#32060=EDGE_CURVE('',#25763,#25761,#23950,.T.);
#32061=EDGE_CURVE('',#25763,#25764,#11578,.T.);
#32062=EDGE_CURVE('',#25764,#25762,#23951,.T.);
#32063=EDGE_CURVE('',#25765,#25763,#23952,.T.);
#32064=EDGE_CURVE('',#25765,#25766,#11579,.T.);
#32065=EDGE_CURVE('',#25766,#25764,#23953,.T.);
#32066=EDGE_CURVE('',#25767,#25765,#23954,.T.);
#32067=EDGE_CURVE('',#25767,#25768,#11580,.T.);
#32068=EDGE_CURVE('',#25768,#25766,#23955,.T.);
#32069=EDGE_CURVE('',#25769,#25767,#23956,.T.);
#32070=EDGE_CURVE('',#25769,#25770,#11581,.T.);
#32071=EDGE_CURVE('',#25770,#25768,#23957,.T.);
#32072=EDGE_CURVE('',#25748,#25769,#23958,.T.);
#32073=EDGE_CURVE('',#25750,#25770,#23959,.T.);
#32074=EDGE_CURVE('',#25771,#25772,#23960,.T.);
#32075=EDGE_CURVE('',#25771,#25773,#11582,.T.);
#32076=EDGE_CURVE('',#25773,#25774,#23961,.T.);
#32077=EDGE_CURVE('',#25772,#25774,#11583,.T.);
#32078=EDGE_CURVE('',#25775,#25771,#23962,.T.);
#32079=EDGE_CURVE('',#25775,#25776,#11584,.T.);
#32080=EDGE_CURVE('',#25776,#25773,#23963,.T.);
#32081=EDGE_CURVE('',#25777,#25775,#23964,.T.);
#32082=EDGE_CURVE('',#25777,#25778,#11585,.T.);
#32083=EDGE_CURVE('',#25778,#25776,#23965,.T.);
#32084=EDGE_CURVE('',#25779,#25777,#23966,.T.);
#32085=EDGE_CURVE('',#25779,#25780,#11586,.T.);
#32086=EDGE_CURVE('',#25780,#25778,#23967,.T.);
#32087=EDGE_CURVE('',#25781,#25779,#23968,.T.);
#32088=EDGE_CURVE('',#25781,#25782,#11587,.T.);
#32089=EDGE_CURVE('',#25782,#25780,#23969,.T.);
#32090=EDGE_CURVE('',#25783,#25781,#23970,.T.);
#32091=EDGE_CURVE('',#25783,#25784,#11588,.T.);
#32092=EDGE_CURVE('',#25784,#25782,#23971,.T.);
#32093=EDGE_CURVE('',#25785,#25783,#11589,.T.);
#32094=EDGE_CURVE('',#25785,#25786,#11590,.T.);
#32095=EDGE_CURVE('',#25786,#25784,#11591,.T.);
#32096=EDGE_CURVE('',#25787,#25785,#11592,.T.);
#32097=EDGE_CURVE('',#25787,#25788,#11593,.T.);
#32098=EDGE_CURVE('',#25788,#25786,#11594,.T.);
#32099=EDGE_CURVE('',#25789,#25787,#11595,.T.);
#32100=EDGE_CURVE('',#25789,#25790,#11596,.T.);
#32101=EDGE_CURVE('',#25790,#25788,#11597,.T.);
#32102=EDGE_CURVE('',#25791,#25789,#11598,.T.);
#32103=EDGE_CURVE('',#25791,#25792,#11599,.T.);
#32104=EDGE_CURVE('',#25792,#25790,#11600,.T.);
#32105=EDGE_CURVE('',#25793,#25791,#11601,.T.);
#32106=EDGE_CURVE('',#25793,#25794,#11602,.T.);
#32107=EDGE_CURVE('',#25794,#25792,#11603,.T.);
#32108=EDGE_CURVE('',#25795,#25793,#11604,.T.);
#32109=EDGE_CURVE('',#25795,#25796,#11605,.T.);
#32110=EDGE_CURVE('',#25796,#25794,#11606,.T.);
#32111=EDGE_CURVE('',#25797,#25795,#23972,.T.);
#32112=EDGE_CURVE('',#25797,#25798,#11607,.T.);
#32113=EDGE_CURVE('',#25798,#25796,#23973,.T.);
#32114=EDGE_CURVE('',#25799,#25797,#23974,.T.);
#32115=EDGE_CURVE('',#25799,#25800,#11608,.T.);
#32116=EDGE_CURVE('',#25800,#25798,#23975,.T.);
#32117=EDGE_CURVE('',#25801,#25799,#23976,.T.);
#32118=EDGE_CURVE('',#25801,#25802,#11609,.T.);
#32119=EDGE_CURVE('',#25802,#25800,#23977,.T.);
#32120=EDGE_CURVE('',#25803,#25801,#23978,.T.);
#32121=EDGE_CURVE('',#25803,#25804,#11610,.T.);
#32122=EDGE_CURVE('',#25804,#25802,#23979,.T.);
#32123=EDGE_CURVE('',#25805,#25803,#23980,.T.);
#32124=EDGE_CURVE('',#25805,#25806,#11611,.T.);
#32125=EDGE_CURVE('',#25806,#25804,#23981,.T.);
#32126=EDGE_CURVE('',#25807,#25805,#23982,.T.);
#32127=EDGE_CURVE('',#25807,#25808,#11612,.T.);
#32128=EDGE_CURVE('',#25808,#25806,#23983,.T.);
#32129=EDGE_CURVE('',#25809,#25807,#23984,.T.);
#32130=EDGE_CURVE('',#25809,#25810,#11613,.T.);
#32131=EDGE_CURVE('',#25810,#25808,#23985,.T.);
#32132=EDGE_CURVE('',#25811,#25809,#23986,.T.);
#32133=EDGE_CURVE('',#25811,#25812,#11614,.T.);
#32134=EDGE_CURVE('',#25812,#25810,#23987,.T.);
#32135=EDGE_CURVE('',#25813,#25811,#11615,.T.);
#32136=EDGE_CURVE('',#25813,#25814,#11616,.T.);
#32137=EDGE_CURVE('',#25814,#25812,#11617,.T.);
#32138=EDGE_CURVE('',#25772,#25813,#23988,.T.);
#32139=EDGE_CURVE('',#25774,#25814,#23989,.T.);
#32140=EDGE_CURVE('',#25815,#25816,#23990,.T.);
#32141=EDGE_CURVE('',#25815,#25817,#11618,.T.);
#32142=EDGE_CURVE('',#25817,#25818,#23991,.T.);
#32143=EDGE_CURVE('',#25816,#25818,#11619,.T.);
#32144=EDGE_CURVE('',#25819,#25815,#23992,.T.);
#32145=EDGE_CURVE('',#25819,#25820,#11620,.T.);
#32146=EDGE_CURVE('',#25820,#25817,#23993,.T.);
#32147=EDGE_CURVE('',#25821,#25819,#23994,.T.);
#32148=EDGE_CURVE('',#25821,#25822,#11621,.T.);
#32149=EDGE_CURVE('',#25822,#25820,#23995,.T.);
#32150=EDGE_CURVE('',#25823,#25821,#23996,.T.);
#32151=EDGE_CURVE('',#25823,#25824,#11622,.T.);
#32152=EDGE_CURVE('',#25824,#25822,#23997,.T.);
#32153=EDGE_CURVE('',#25825,#25823,#23998,.T.);
#32154=EDGE_CURVE('',#25825,#25826,#11623,.T.);
#32155=EDGE_CURVE('',#25826,#25824,#23999,.T.);
#32156=EDGE_CURVE('',#25827,#25825,#24000,.T.);
#32157=EDGE_CURVE('',#25827,#25828,#11624,.T.);
#32158=EDGE_CURVE('',#25828,#25826,#24001,.T.);
#32159=EDGE_CURVE('',#25829,#25827,#24002,.T.);
#32160=EDGE_CURVE('',#25829,#25830,#11625,.T.);
#32161=EDGE_CURVE('',#25830,#25828,#24003,.T.);
#32162=EDGE_CURVE('',#25816,#25829,#24004,.T.);
#32163=EDGE_CURVE('',#25818,#25830,#24005,.T.);
#32164=EDGE_CURVE('',#25831,#25832,#24006,.T.);
#32165=EDGE_CURVE('',#25831,#25833,#11626,.T.);
#32166=EDGE_CURVE('',#25833,#25834,#24007,.T.);
#32167=EDGE_CURVE('',#25832,#25834,#11627,.T.);
#32168=EDGE_CURVE('',#25835,#25831,#24008,.T.);
#32169=EDGE_CURVE('',#25835,#25836,#11628,.T.);
#32170=EDGE_CURVE('',#25836,#25833,#24009,.T.);
#32171=EDGE_CURVE('',#25837,#25835,#24010,.T.);
#32172=EDGE_CURVE('',#25837,#25838,#11629,.T.);
#32173=EDGE_CURVE('',#25838,#25836,#24011,.T.);
#32174=EDGE_CURVE('',#25839,#25837,#24012,.T.);
#32175=EDGE_CURVE('',#25839,#25840,#11630,.T.);
#32176=EDGE_CURVE('',#25840,#25838,#24013,.T.);
#32177=EDGE_CURVE('',#25841,#25839,#24014,.T.);
#32178=EDGE_CURVE('',#25841,#25842,#11631,.T.);
#32179=EDGE_CURVE('',#25842,#25840,#24015,.T.);
#32180=EDGE_CURVE('',#25843,#25841,#24016,.T.);
#32181=EDGE_CURVE('',#25843,#25844,#11632,.T.);
#32182=EDGE_CURVE('',#25844,#25842,#24017,.T.);
#32183=EDGE_CURVE('',#25845,#25843,#24018,.T.);
#32184=EDGE_CURVE('',#25845,#25846,#11633,.T.);
#32185=EDGE_CURVE('',#25846,#25844,#24019,.T.);
#32186=EDGE_CURVE('',#25847,#25845,#24020,.T.);
#32187=EDGE_CURVE('',#25847,#25848,#11634,.T.);
#32188=EDGE_CURVE('',#25848,#25846,#24021,.T.);
#32189=EDGE_CURVE('',#25849,#25847,#24022,.T.);
#32190=EDGE_CURVE('',#25849,#25850,#11635,.T.);
#32191=EDGE_CURVE('',#25850,#25848,#24023,.T.);
#32192=EDGE_CURVE('',#25851,#25849,#24024,.T.);
#32193=EDGE_CURVE('',#25851,#25852,#11636,.T.);
#32194=EDGE_CURVE('',#25852,#25850,#24025,.T.);
#32195=EDGE_CURVE('',#25853,#25851,#24026,.T.);
#32196=EDGE_CURVE('',#25853,#25854,#11637,.T.);
#32197=EDGE_CURVE('',#25854,#25852,#24027,.T.);
#32198=EDGE_CURVE('',#25832,#25853,#24028,.T.);
#32199=EDGE_CURVE('',#25834,#25854,#24029,.T.);
#32200=EDGE_CURVE('',#25855,#25856,#24030,.T.);
#32201=EDGE_CURVE('',#25855,#25857,#11638,.T.);
#32202=EDGE_CURVE('',#25857,#25858,#24031,.T.);
#32203=EDGE_CURVE('',#25856,#25858,#11639,.T.);
#32204=EDGE_CURVE('',#25859,#25855,#24032,.T.);
#32205=EDGE_CURVE('',#25859,#25860,#11640,.T.);
#32206=EDGE_CURVE('',#25860,#25857,#24033,.T.);
#32207=EDGE_CURVE('',#25861,#25859,#24034,.T.);
#32208=EDGE_CURVE('',#25861,#25862,#11641,.T.);
#32209=EDGE_CURVE('',#25862,#25860,#24035,.T.);
#32210=EDGE_CURVE('',#25863,#25861,#24036,.T.);
#32211=EDGE_CURVE('',#25863,#25864,#11642,.T.);
#32212=EDGE_CURVE('',#25864,#25862,#24037,.T.);
#32213=EDGE_CURVE('',#25865,#25863,#24038,.T.);
#32214=EDGE_CURVE('',#25865,#25866,#11643,.T.);
#32215=EDGE_CURVE('',#25866,#25864,#24039,.T.);
#32216=EDGE_CURVE('',#25867,#25865,#24040,.T.);
#32217=EDGE_CURVE('',#25867,#25868,#11644,.T.);
#32218=EDGE_CURVE('',#25868,#25866,#24041,.T.);
#32219=EDGE_CURVE('',#25869,#25867,#24042,.T.);
#32220=EDGE_CURVE('',#25869,#25870,#11645,.T.);
#32221=EDGE_CURVE('',#25870,#25868,#24043,.T.);
#32222=EDGE_CURVE('',#25871,#25869,#24044,.T.);
#32223=EDGE_CURVE('',#25871,#25872,#11646,.T.);
#32224=EDGE_CURVE('',#25872,#25870,#24045,.T.);
#32225=EDGE_CURVE('',#25856,#25871,#24046,.T.);
#32226=EDGE_CURVE('',#25858,#25872,#24047,.T.);
#32227=EDGE_CURVE('',#25873,#25874,#24048,.T.);
#32228=EDGE_CURVE('',#25873,#25875,#11647,.T.);
#32229=EDGE_CURVE('',#25875,#25876,#24049,.T.);
#32230=EDGE_CURVE('',#25874,#25876,#11648,.T.);
#32231=EDGE_CURVE('',#25877,#25873,#24050,.T.);
#32232=EDGE_CURVE('',#25877,#25878,#11649,.T.);
#32233=EDGE_CURVE('',#25878,#25875,#24051,.T.);
#32234=EDGE_CURVE('',#25879,#25877,#24052,.T.);
#32235=EDGE_CURVE('',#25879,#25880,#11650,.T.);
#32236=EDGE_CURVE('',#25880,#25878,#24053,.T.);
#32237=EDGE_CURVE('',#25881,#25879,#24054,.T.);
#32238=EDGE_CURVE('',#25881,#25882,#11651,.T.);
#32239=EDGE_CURVE('',#25882,#25880,#24055,.T.);
#32240=EDGE_CURVE('',#25883,#25881,#24056,.T.);
#32241=EDGE_CURVE('',#25883,#25884,#11652,.T.);
#32242=EDGE_CURVE('',#25884,#25882,#24057,.T.);
#32243=EDGE_CURVE('',#25885,#25883,#24058,.T.);
#32244=EDGE_CURVE('',#25885,#25886,#11653,.T.);
#32245=EDGE_CURVE('',#25886,#25884,#24059,.T.);
#32246=EDGE_CURVE('',#25887,#25885,#24060,.T.);
#32247=EDGE_CURVE('',#25887,#25888,#11654,.T.);
#32248=EDGE_CURVE('',#25888,#25886,#24061,.T.);
#32249=EDGE_CURVE('',#25889,#25887,#24062,.T.);
#32250=EDGE_CURVE('',#25889,#25890,#11655,.T.);
#32251=EDGE_CURVE('',#25890,#25888,#24063,.T.);
#32252=EDGE_CURVE('',#25891,#25889,#24064,.T.);
#32253=EDGE_CURVE('',#25891,#25892,#11656,.T.);
#32254=EDGE_CURVE('',#25892,#25890,#24065,.T.);
#32255=EDGE_CURVE('',#25893,#25891,#24066,.T.);
#32256=EDGE_CURVE('',#25893,#25894,#11657,.T.);
#32257=EDGE_CURVE('',#25894,#25892,#24067,.T.);
#32258=EDGE_CURVE('',#25895,#25893,#24068,.T.);
#32259=EDGE_CURVE('',#25895,#25896,#11658,.T.);
#32260=EDGE_CURVE('',#25896,#25894,#24069,.T.);
#32261=EDGE_CURVE('',#25897,#25895,#24070,.T.);
#32262=EDGE_CURVE('',#25897,#25898,#11659,.T.);
#32263=EDGE_CURVE('',#25898,#25896,#24071,.T.);
#32264=EDGE_CURVE('',#25899,#25897,#24072,.T.);
#32265=EDGE_CURVE('',#25899,#25900,#11660,.T.);
#32266=EDGE_CURVE('',#25900,#25898,#24073,.T.);
#32267=EDGE_CURVE('',#25901,#25899,#24074,.T.);
#32268=EDGE_CURVE('',#25901,#25902,#11661,.T.);
#32269=EDGE_CURVE('',#25902,#25900,#24075,.T.);
#32270=EDGE_CURVE('',#25903,#25901,#24076,.T.);
#32271=EDGE_CURVE('',#25903,#25904,#11662,.T.);
#32272=EDGE_CURVE('',#25904,#25902,#24077,.T.);
#32273=EDGE_CURVE('',#25905,#25903,#24078,.T.);
#32274=EDGE_CURVE('',#25905,#25906,#11663,.T.);
#32275=EDGE_CURVE('',#25906,#25904,#24079,.T.);
#32276=EDGE_CURVE('',#25907,#25905,#24080,.T.);
#32277=EDGE_CURVE('',#25907,#25908,#11664,.T.);
#32278=EDGE_CURVE('',#25908,#25906,#24081,.T.);
#32279=EDGE_CURVE('',#25909,#25907,#11665,.T.);
#32280=EDGE_CURVE('',#25909,#25910,#11666,.T.);
#32281=EDGE_CURVE('',#25910,#25908,#11667,.T.);
#32282=EDGE_CURVE('',#25874,#25909,#24082,.T.);
#32283=EDGE_CURVE('',#25876,#25910,#24083,.T.);
#32284=EDGE_CURVE('',#25911,#25912,#24084,.T.);
#32285=EDGE_CURVE('',#25911,#25913,#11668,.T.);
#32286=EDGE_CURVE('',#25913,#25914,#24085,.T.);
#32287=EDGE_CURVE('',#25912,#25914,#11669,.T.);
#32288=EDGE_CURVE('',#25915,#25911,#24086,.T.);
#32289=EDGE_CURVE('',#25915,#25916,#11670,.T.);
#32290=EDGE_CURVE('',#25916,#25913,#24087,.T.);
#32291=EDGE_CURVE('',#25917,#25915,#24088,.T.);
#32292=EDGE_CURVE('',#25917,#25918,#11671,.T.);
#32293=EDGE_CURVE('',#25918,#25916,#24089,.T.);
#32294=EDGE_CURVE('',#25919,#25917,#24090,.T.);
#32295=EDGE_CURVE('',#25919,#25920,#11672,.T.);
#32296=EDGE_CURVE('',#25920,#25918,#24091,.T.);
#32297=EDGE_CURVE('',#25921,#25919,#24092,.T.);
#32298=EDGE_CURVE('',#25921,#25922,#11673,.T.);
#32299=EDGE_CURVE('',#25922,#25920,#24093,.T.);
#32300=EDGE_CURVE('',#25923,#25921,#24094,.T.);
#32301=EDGE_CURVE('',#25923,#25924,#11674,.T.);
#32302=EDGE_CURVE('',#25924,#25922,#24095,.T.);
#32303=EDGE_CURVE('',#25925,#25923,#24096,.T.);
#32304=EDGE_CURVE('',#25925,#25926,#11675,.T.);
#32305=EDGE_CURVE('',#25926,#25924,#24097,.T.);
#32306=EDGE_CURVE('',#25912,#25925,#24098,.T.);
#32307=EDGE_CURVE('',#25914,#25926,#24099,.T.);
#32308=EDGE_CURVE('',#25927,#25928,#24100,.T.);
#32309=EDGE_CURVE('',#25927,#25929,#11676,.T.);
#32310=EDGE_CURVE('',#25929,#25930,#24101,.T.);
#32311=EDGE_CURVE('',#25928,#25930,#11677,.T.);
#32312=EDGE_CURVE('',#25931,#25927,#24102,.T.);
#32313=EDGE_CURVE('',#25931,#25932,#11678,.T.);
#32314=EDGE_CURVE('',#25932,#25929,#24103,.T.);
#32315=EDGE_CURVE('',#25933,#25931,#24104,.T.);
#32316=EDGE_CURVE('',#25933,#25934,#11679,.T.);
#32317=EDGE_CURVE('',#25934,#25932,#24105,.T.);
#32318=EDGE_CURVE('',#25935,#25933,#24106,.T.);
#32319=EDGE_CURVE('',#25935,#25936,#11680,.T.);
#32320=EDGE_CURVE('',#25936,#25934,#24107,.T.);
#32321=EDGE_CURVE('',#25937,#25935,#24108,.T.);
#32322=EDGE_CURVE('',#25937,#25938,#11681,.T.);
#32323=EDGE_CURVE('',#25938,#25936,#24109,.T.);
#32324=EDGE_CURVE('',#25939,#25937,#24110,.T.);
#32325=EDGE_CURVE('',#25939,#25940,#11682,.T.);
#32326=EDGE_CURVE('',#25940,#25938,#24111,.T.);
#32327=EDGE_CURVE('',#25941,#25939,#24112,.T.);
#32328=EDGE_CURVE('',#25941,#25942,#11683,.T.);
#32329=EDGE_CURVE('',#25942,#25940,#24113,.T.);
#32330=EDGE_CURVE('',#25943,#25941,#24114,.T.);
#32331=EDGE_CURVE('',#25943,#25944,#11684,.T.);
#32332=EDGE_CURVE('',#25944,#25942,#24115,.T.);
#32333=EDGE_CURVE('',#25945,#25943,#24116,.T.);
#32334=EDGE_CURVE('',#25945,#25946,#11685,.T.);
#32335=EDGE_CURVE('',#25946,#25944,#24117,.T.);
#32336=EDGE_CURVE('',#25947,#25945,#24118,.T.);
#32337=EDGE_CURVE('',#25947,#25948,#11686,.T.);
#32338=EDGE_CURVE('',#25948,#25946,#24119,.T.);
#32339=EDGE_CURVE('',#25949,#25947,#24120,.T.);
#32340=EDGE_CURVE('',#25949,#25950,#11687,.T.);
#32341=EDGE_CURVE('',#25950,#25948,#24121,.T.);
#32342=EDGE_CURVE('',#25928,#25949,#24122,.T.);
#32343=EDGE_CURVE('',#25930,#25950,#24123,.T.);
#32344=EDGE_CURVE('',#25951,#25952,#24124,.T.);
#32345=EDGE_CURVE('',#25951,#25953,#11688,.T.);
#32346=EDGE_CURVE('',#25953,#25954,#24125,.T.);
#32347=EDGE_CURVE('',#25952,#25954,#11689,.T.);
#32348=EDGE_CURVE('',#25955,#25951,#24126,.T.);
#32349=EDGE_CURVE('',#25955,#25956,#11690,.T.);
#32350=EDGE_CURVE('',#25956,#25953,#24127,.T.);
#32351=EDGE_CURVE('',#25957,#25955,#24128,.T.);
#32352=EDGE_CURVE('',#25957,#25958,#11691,.T.);
#32353=EDGE_CURVE('',#25958,#25956,#24129,.T.);
#32354=EDGE_CURVE('',#25959,#25957,#11692,.T.);
#32355=EDGE_CURVE('',#25959,#25960,#11693,.T.);
#32356=EDGE_CURVE('',#25960,#25958,#11694,.T.);
#32357=EDGE_CURVE('',#25961,#25959,#24130,.T.);
#32358=EDGE_CURVE('',#25961,#25962,#11695,.T.);
#32359=EDGE_CURVE('',#25962,#25960,#24131,.T.);
#32360=EDGE_CURVE('',#25963,#25961,#24132,.T.);
#32361=EDGE_CURVE('',#25963,#25964,#11696,.T.);
#32362=EDGE_CURVE('',#25964,#25962,#24133,.T.);
#32363=EDGE_CURVE('',#25965,#25963,#24134,.T.);
#32364=EDGE_CURVE('',#25965,#25966,#11697,.T.);
#32365=EDGE_CURVE('',#25966,#25964,#24135,.T.);
#32366=EDGE_CURVE('',#25967,#25965,#11698,.T.);
#32367=EDGE_CURVE('',#25967,#25968,#11699,.T.);
#32368=EDGE_CURVE('',#25968,#25966,#11700,.T.);
#32369=EDGE_CURVE('',#25969,#25967,#11701,.T.);
#32370=EDGE_CURVE('',#25969,#25970,#11702,.T.);
#32371=EDGE_CURVE('',#25970,#25968,#11703,.T.);
#32372=EDGE_CURVE('',#25971,#25969,#11704,.T.);
#32373=EDGE_CURVE('',#25971,#25972,#11705,.T.);
#32374=EDGE_CURVE('',#25972,#25970,#11706,.T.);
#32375=EDGE_CURVE('',#25952,#25971,#11707,.T.);
#32376=EDGE_CURVE('',#25954,#25972,#11708,.T.);
#32377=EDGE_CURVE('',#25973,#25974,#24136,.T.);
#32378=EDGE_CURVE('',#25973,#25975,#11709,.T.);
#32379=EDGE_CURVE('',#25975,#25976,#24137,.T.);
#32380=EDGE_CURVE('',#25974,#25976,#11710,.T.);
#32381=EDGE_CURVE('',#25977,#25973,#24138,.T.);
#32382=EDGE_CURVE('',#25977,#25978,#11711,.T.);
#32383=EDGE_CURVE('',#25978,#25975,#24139,.T.);
#32384=EDGE_CURVE('',#25979,#25977,#24140,.T.);
#32385=EDGE_CURVE('',#25979,#25980,#11712,.T.);
#32386=EDGE_CURVE('',#25980,#25978,#24141,.T.);
#32387=EDGE_CURVE('',#25981,#25979,#24142,.T.);
#32388=EDGE_CURVE('',#25981,#25982,#11713,.T.);
#32389=EDGE_CURVE('',#25982,#25980,#24143,.T.);
#32390=EDGE_CURVE('',#25983,#25981,#24144,.T.);
#32391=EDGE_CURVE('',#25983,#25984,#11714,.T.);
#32392=EDGE_CURVE('',#25984,#25982,#24145,.T.);
#32393=EDGE_CURVE('',#25985,#25983,#24146,.T.);
#32394=EDGE_CURVE('',#25985,#25986,#11715,.T.);
#32395=EDGE_CURVE('',#25986,#25984,#24147,.T.);
#32396=EDGE_CURVE('',#25987,#25985,#24148,.T.);
#32397=EDGE_CURVE('',#25987,#25988,#11716,.T.);
#32398=EDGE_CURVE('',#25988,#25986,#24149,.T.);
#32399=EDGE_CURVE('',#25974,#25987,#24150,.T.);
#32400=EDGE_CURVE('',#25976,#25988,#24151,.T.);
#32401=EDGE_CURVE('',#25989,#25990,#24152,.T.);
#32402=EDGE_CURVE('',#25989,#25991,#11717,.T.);
#32403=EDGE_CURVE('',#25991,#25992,#24153,.T.);
#32404=EDGE_CURVE('',#25990,#25992,#11718,.T.);
#32405=EDGE_CURVE('',#25993,#25989,#24154,.T.);
#32406=EDGE_CURVE('',#25993,#25994,#11719,.T.);
#32407=EDGE_CURVE('',#25994,#25991,#24155,.T.);
#32408=EDGE_CURVE('',#25995,#25993,#24156,.T.);
#32409=EDGE_CURVE('',#25995,#25996,#11720,.T.);
#32410=EDGE_CURVE('',#25996,#25994,#24157,.T.);
#32411=EDGE_CURVE('',#25997,#25995,#24158,.T.);
#32412=EDGE_CURVE('',#25997,#25998,#11721,.T.);
#32413=EDGE_CURVE('',#25998,#25996,#24159,.T.);
#32414=EDGE_CURVE('',#25999,#25997,#24160,.T.);
#32415=EDGE_CURVE('',#25999,#26000,#11722,.T.);
#32416=EDGE_CURVE('',#26000,#25998,#24161,.T.);
#32417=EDGE_CURVE('',#26001,#25999,#24162,.T.);
#32418=EDGE_CURVE('',#26001,#26002,#11723,.T.);
#32419=EDGE_CURVE('',#26002,#26000,#24163,.T.);
#32420=EDGE_CURVE('',#26003,#26001,#24164,.T.);
#32421=EDGE_CURVE('',#26003,#26004,#11724,.T.);
#32422=EDGE_CURVE('',#26004,#26002,#24165,.T.);
#32423=EDGE_CURVE('',#26005,#26003,#24166,.T.);
#32424=EDGE_CURVE('',#26005,#26006,#11725,.T.);
#32425=EDGE_CURVE('',#26006,#26004,#24167,.T.);
#32426=EDGE_CURVE('',#26007,#26005,#24168,.T.);
#32427=EDGE_CURVE('',#26007,#26008,#11726,.T.);
#32428=EDGE_CURVE('',#26008,#26006,#24169,.T.);
#32429=EDGE_CURVE('',#26009,#26007,#24170,.T.);
#32430=EDGE_CURVE('',#26009,#26010,#11727,.T.);
#32431=EDGE_CURVE('',#26010,#26008,#24171,.T.);
#32432=EDGE_CURVE('',#26011,#26009,#24172,.T.);
#32433=EDGE_CURVE('',#26011,#26012,#11728,.T.);
#32434=EDGE_CURVE('',#26012,#26010,#24173,.T.);
#32435=EDGE_CURVE('',#25990,#26011,#24174,.T.);
#32436=EDGE_CURVE('',#25992,#26012,#24175,.T.);
#32437=EDGE_CURVE('',#26013,#26014,#24176,.T.);
#32438=EDGE_CURVE('',#26013,#26015,#11729,.T.);
#32439=EDGE_CURVE('',#26015,#26016,#24177,.T.);
#32440=EDGE_CURVE('',#26014,#26016,#11730,.T.);
#32441=EDGE_CURVE('',#26017,#26013,#24178,.T.);
#32442=EDGE_CURVE('',#26017,#26018,#11731,.T.);
#32443=EDGE_CURVE('',#26018,#26015,#24179,.T.);
#32444=EDGE_CURVE('',#26019,#26017,#24180,.T.);
#32445=EDGE_CURVE('',#26019,#26020,#11732,.T.);
#32446=EDGE_CURVE('',#26020,#26018,#24181,.T.);
#32447=EDGE_CURVE('',#26021,#26019,#24182,.T.);
#32448=EDGE_CURVE('',#26021,#26022,#11733,.T.);
#32449=EDGE_CURVE('',#26022,#26020,#24183,.T.);
#32450=EDGE_CURVE('',#26023,#26021,#24184,.T.);
#32451=EDGE_CURVE('',#26023,#26024,#11734,.T.);
#32452=EDGE_CURVE('',#26024,#26022,#24185,.T.);
#32453=EDGE_CURVE('',#26025,#26023,#24186,.T.);
#32454=EDGE_CURVE('',#26025,#26026,#11735,.T.);
#32455=EDGE_CURVE('',#26026,#26024,#24187,.T.);
#32456=EDGE_CURVE('',#26027,#26025,#24188,.T.);
#32457=EDGE_CURVE('',#26027,#26028,#11736,.T.);
#32458=EDGE_CURVE('',#26028,#26026,#24189,.T.);
#32459=EDGE_CURVE('',#26014,#26027,#24190,.T.);
#32460=EDGE_CURVE('',#26016,#26028,#24191,.T.);
#32461=EDGE_CURVE('',#26029,#26030,#24192,.T.);
#32462=EDGE_CURVE('',#26029,#26031,#11737,.T.);
#32463=EDGE_CURVE('',#26031,#26032,#24193,.T.);
#32464=EDGE_CURVE('',#26030,#26032,#11738,.T.);
#32465=EDGE_CURVE('',#26033,#26029,#24194,.T.);
#32466=EDGE_CURVE('',#26033,#26034,#11739,.T.);
#32467=EDGE_CURVE('',#26034,#26031,#24195,.T.);
#32468=EDGE_CURVE('',#26035,#26033,#24196,.T.);
#32469=EDGE_CURVE('',#26035,#26036,#11740,.T.);
#32470=EDGE_CURVE('',#26036,#26034,#24197,.T.);
#32471=EDGE_CURVE('',#26037,#26035,#24198,.T.);
#32472=EDGE_CURVE('',#26037,#26038,#11741,.T.);
#32473=EDGE_CURVE('',#26038,#26036,#24199,.T.);
#32474=EDGE_CURVE('',#26039,#26037,#24200,.T.);
#32475=EDGE_CURVE('',#26039,#26040,#11742,.T.);
#32476=EDGE_CURVE('',#26040,#26038,#24201,.T.);
#32477=EDGE_CURVE('',#26041,#26039,#24202,.T.);
#32478=EDGE_CURVE('',#26041,#26042,#11743,.T.);
#32479=EDGE_CURVE('',#26042,#26040,#24203,.T.);
#32480=EDGE_CURVE('',#26043,#26041,#24204,.T.);
#32481=EDGE_CURVE('',#26043,#26044,#11744,.T.);
#32482=EDGE_CURVE('',#26044,#26042,#24205,.T.);
#32483=EDGE_CURVE('',#26045,#26043,#24206,.T.);
#32484=EDGE_CURVE('',#26045,#26046,#11745,.T.);
#32485=EDGE_CURVE('',#26046,#26044,#24207,.T.);
#32486=EDGE_CURVE('',#26030,#26045,#24208,.T.);
#32487=EDGE_CURVE('',#26032,#26046,#24209,.T.);
#32488=EDGE_CURVE('',#26047,#26048,#24210,.T.);
#32489=EDGE_CURVE('',#26047,#26049,#11746,.T.);
#32490=EDGE_CURVE('',#26049,#26050,#24211,.T.);
#32491=EDGE_CURVE('',#26048,#26050,#11747,.T.);
#32492=EDGE_CURVE('',#26051,#26047,#24212,.T.);
#32493=EDGE_CURVE('',#26051,#26052,#11748,.T.);
#32494=EDGE_CURVE('',#26052,#26049,#24213,.T.);
#32495=EDGE_CURVE('',#26053,#26051,#24214,.T.);
#32496=EDGE_CURVE('',#26053,#26054,#11749,.T.);
#32497=EDGE_CURVE('',#26054,#26052,#24215,.T.);
#32498=EDGE_CURVE('',#26055,#26053,#24216,.T.);
#32499=EDGE_CURVE('',#26055,#26056,#11750,.T.);
#32500=EDGE_CURVE('',#26056,#26054,#24217,.T.);
#32501=EDGE_CURVE('',#26057,#26055,#24218,.T.);
#32502=EDGE_CURVE('',#26057,#26058,#11751,.T.);
#32503=EDGE_CURVE('',#26058,#26056,#24219,.T.);
#32504=EDGE_CURVE('',#26059,#26057,#24220,.T.);
#32505=EDGE_CURVE('',#26059,#26060,#11752,.T.);
#32506=EDGE_CURVE('',#26060,#26058,#24221,.T.);
#32507=EDGE_CURVE('',#26061,#26059,#24222,.T.);
#32508=EDGE_CURVE('',#26061,#26062,#11753,.T.);
#32509=EDGE_CURVE('',#26062,#26060,#24223,.T.);
#32510=EDGE_CURVE('',#26063,#26061,#24224,.T.);
#32511=EDGE_CURVE('',#26063,#26064,#11754,.T.);
#32512=EDGE_CURVE('',#26064,#26062,#24225,.T.);
#32513=EDGE_CURVE('',#26065,#26063,#24226,.T.);
#32514=EDGE_CURVE('',#26065,#26066,#11755,.T.);
#32515=EDGE_CURVE('',#26066,#26064,#24227,.T.);
#32516=EDGE_CURVE('',#26067,#26065,#24228,.T.);
#32517=EDGE_CURVE('',#26067,#26068,#11756,.T.);
#32518=EDGE_CURVE('',#26068,#26066,#24229,.T.);
#32519=EDGE_CURVE('',#26069,#26067,#24230,.T.);
#32520=EDGE_CURVE('',#26069,#26070,#11757,.T.);
#32521=EDGE_CURVE('',#26070,#26068,#24231,.T.);
#32522=EDGE_CURVE('',#26071,#26069,#24232,.T.);
#32523=EDGE_CURVE('',#26071,#26072,#11758,.T.);
#32524=EDGE_CURVE('',#26072,#26070,#24233,.T.);
#32525=EDGE_CURVE('',#26073,#26071,#24234,.T.);
#32526=EDGE_CURVE('',#26073,#26074,#11759,.T.);
#32527=EDGE_CURVE('',#26074,#26072,#24235,.T.);
#32528=EDGE_CURVE('',#26075,#26073,#24236,.T.);
#32529=EDGE_CURVE('',#26075,#26076,#11760,.T.);
#32530=EDGE_CURVE('',#26076,#26074,#24237,.T.);
#32531=EDGE_CURVE('',#26077,#26075,#24238,.T.);
#32532=EDGE_CURVE('',#26077,#26078,#11761,.T.);
#32533=EDGE_CURVE('',#26078,#26076,#24239,.T.);
#32534=EDGE_CURVE('',#26048,#26077,#24240,.T.);
#32535=EDGE_CURVE('',#26050,#26078,#24241,.T.);
#32536=EDGE_CURVE('',#26079,#26080,#24242,.T.);
#32537=EDGE_CURVE('',#26079,#26081,#11762,.T.);
#32538=EDGE_CURVE('',#26081,#26082,#24243,.T.);
#32539=EDGE_CURVE('',#26080,#26082,#11763,.T.);
#32540=EDGE_CURVE('',#26083,#26079,#24244,.T.);
#32541=EDGE_CURVE('',#26083,#26084,#11764,.T.);
#32542=EDGE_CURVE('',#26084,#26081,#24245,.T.);
#32543=EDGE_CURVE('',#26085,#26083,#24246,.T.);
#32544=EDGE_CURVE('',#26085,#26086,#11765,.T.);
#32545=EDGE_CURVE('',#26086,#26084,#24247,.T.);
#32546=EDGE_CURVE('',#26087,#26085,#24248,.T.);
#32547=EDGE_CURVE('',#26087,#26088,#11766,.T.);
#32548=EDGE_CURVE('',#26088,#26086,#24249,.T.);
#32549=EDGE_CURVE('',#26089,#26087,#24250,.T.);
#32550=EDGE_CURVE('',#26089,#26090,#11767,.T.);
#32551=EDGE_CURVE('',#26090,#26088,#24251,.T.);
#32552=EDGE_CURVE('',#26091,#26089,#24252,.T.);
#32553=EDGE_CURVE('',#26091,#26092,#11768,.T.);
#32554=EDGE_CURVE('',#26092,#26090,#24253,.T.);
#32555=EDGE_CURVE('',#26093,#26091,#24254,.T.);
#32556=EDGE_CURVE('',#26093,#26094,#11769,.T.);
#32557=EDGE_CURVE('',#26094,#26092,#24255,.T.);
#32558=EDGE_CURVE('',#26080,#26093,#24256,.T.);
#32559=EDGE_CURVE('',#26082,#26094,#24257,.T.);
#32560=EDGE_CURVE('',#26095,#26096,#24258,.T.);
#32561=EDGE_CURVE('',#26095,#26097,#11770,.T.);
#32562=EDGE_CURVE('',#26097,#26098,#24259,.T.);
#32563=EDGE_CURVE('',#26096,#26098,#11771,.T.);
#32564=EDGE_CURVE('',#26099,#26095,#24260,.T.);
#32565=EDGE_CURVE('',#26099,#26100,#11772,.T.);
#32566=EDGE_CURVE('',#26100,#26097,#24261,.T.);
#32567=EDGE_CURVE('',#26101,#26099,#24262,.T.);
#32568=EDGE_CURVE('',#26101,#26102,#11773,.T.);
#32569=EDGE_CURVE('',#26102,#26100,#24263,.T.);
#32570=EDGE_CURVE('',#26103,#26101,#24264,.T.);
#32571=EDGE_CURVE('',#26103,#26104,#11774,.T.);
#32572=EDGE_CURVE('',#26104,#26102,#24265,.T.);
#32573=EDGE_CURVE('',#26105,#26103,#24266,.T.);
#32574=EDGE_CURVE('',#26105,#26106,#11775,.T.);
#32575=EDGE_CURVE('',#26106,#26104,#24267,.T.);
#32576=EDGE_CURVE('',#26107,#26105,#24268,.T.);
#32577=EDGE_CURVE('',#26107,#26108,#11776,.T.);
#32578=EDGE_CURVE('',#26108,#26106,#24269,.T.);
#32579=EDGE_CURVE('',#26109,#26107,#24270,.T.);
#32580=EDGE_CURVE('',#26109,#26110,#11777,.T.);
#32581=EDGE_CURVE('',#26110,#26108,#24271,.T.);
#32582=EDGE_CURVE('',#26111,#26109,#24272,.T.);
#32583=EDGE_CURVE('',#26111,#26112,#11778,.T.);
#32584=EDGE_CURVE('',#26112,#26110,#24273,.T.);
#32585=EDGE_CURVE('',#26113,#26111,#24274,.T.);
#32586=EDGE_CURVE('',#26113,#26114,#11779,.T.);
#32587=EDGE_CURVE('',#26114,#26112,#24275,.T.);
#32588=EDGE_CURVE('',#26115,#26113,#24276,.T.);
#32589=EDGE_CURVE('',#26115,#26116,#11780,.T.);
#32590=EDGE_CURVE('',#26116,#26114,#24277,.T.);
#32591=EDGE_CURVE('',#26117,#26115,#24278,.T.);
#32592=EDGE_CURVE('',#26117,#26118,#11781,.T.);
#32593=EDGE_CURVE('',#26118,#26116,#24279,.T.);
#32594=EDGE_CURVE('',#26096,#26117,#24280,.T.);
#32595=EDGE_CURVE('',#26098,#26118,#24281,.T.);
#32596=EDGE_CURVE('',#26119,#26120,#24282,.T.);
#32597=EDGE_CURVE('',#26119,#26121,#11782,.T.);
#32598=EDGE_CURVE('',#26121,#26122,#24283,.T.);
#32599=EDGE_CURVE('',#26120,#26122,#11783,.T.);
#32600=EDGE_CURVE('',#26123,#26119,#24284,.T.);
#32601=EDGE_CURVE('',#26123,#26124,#11784,.T.);
#32602=EDGE_CURVE('',#26124,#26121,#24285,.T.);
#32603=EDGE_CURVE('',#26125,#26123,#24286,.T.);
#32604=EDGE_CURVE('',#26125,#26126,#11785,.T.);
#32605=EDGE_CURVE('',#26126,#26124,#24287,.T.);
#32606=EDGE_CURVE('',#26127,#26125,#24288,.T.);
#32607=EDGE_CURVE('',#26127,#26128,#11786,.T.);
#32608=EDGE_CURVE('',#26128,#26126,#24289,.T.);
#32609=EDGE_CURVE('',#26129,#26127,#24290,.T.);
#32610=EDGE_CURVE('',#26129,#26130,#11787,.T.);
#32611=EDGE_CURVE('',#26130,#26128,#24291,.T.);
#32612=EDGE_CURVE('',#26131,#26129,#24292,.T.);
#32613=EDGE_CURVE('',#26131,#26132,#11788,.T.);
#32614=EDGE_CURVE('',#26132,#26130,#24293,.T.);
#32615=EDGE_CURVE('',#26133,#26131,#24294,.T.);
#32616=EDGE_CURVE('',#26133,#26134,#11789,.T.);
#32617=EDGE_CURVE('',#26134,#26132,#24295,.T.);
#32618=EDGE_CURVE('',#26120,#26133,#24296,.T.);
#32619=EDGE_CURVE('',#26122,#26134,#24297,.T.);
#32620=EDGE_CURVE('',#26135,#26136,#24298,.T.);
#32621=EDGE_CURVE('',#26135,#26137,#11790,.T.);
#32622=EDGE_CURVE('',#26137,#26138,#24299,.T.);
#32623=EDGE_CURVE('',#26136,#26138,#11791,.T.);
#32624=EDGE_CURVE('',#26139,#26135,#24300,.T.);
#32625=EDGE_CURVE('',#26139,#26140,#11792,.T.);
#32626=EDGE_CURVE('',#26140,#26137,#24301,.T.);
#32627=EDGE_CURVE('',#26141,#26139,#24302,.T.);
#32628=EDGE_CURVE('',#26141,#26142,#11793,.T.);
#32629=EDGE_CURVE('',#26142,#26140,#24303,.T.);
#32630=EDGE_CURVE('',#26143,#26141,#24304,.T.);
#32631=EDGE_CURVE('',#26143,#26144,#11794,.T.);
#32632=EDGE_CURVE('',#26144,#26142,#24305,.T.);
#32633=EDGE_CURVE('',#26145,#26143,#24306,.T.);
#32634=EDGE_CURVE('',#26145,#26146,#11795,.T.);
#32635=EDGE_CURVE('',#26146,#26144,#24307,.T.);
#32636=EDGE_CURVE('',#26147,#26145,#24308,.T.);
#32637=EDGE_CURVE('',#26147,#26148,#11796,.T.);
#32638=EDGE_CURVE('',#26148,#26146,#24309,.T.);
#32639=EDGE_CURVE('',#26149,#26147,#24310,.T.);
#32640=EDGE_CURVE('',#26149,#26150,#11797,.T.);
#32641=EDGE_CURVE('',#26150,#26148,#24311,.T.);
#32642=EDGE_CURVE('',#26151,#26149,#24312,.T.);
#32643=EDGE_CURVE('',#26151,#26152,#11798,.T.);
#32644=EDGE_CURVE('',#26152,#26150,#24313,.T.);
#32645=EDGE_CURVE('',#26153,#26151,#24314,.T.);
#32646=EDGE_CURVE('',#26153,#26154,#11799,.T.);
#32647=EDGE_CURVE('',#26154,#26152,#24315,.T.);
#32648=EDGE_CURVE('',#26155,#26153,#24316,.T.);
#32649=EDGE_CURVE('',#26155,#26156,#11800,.T.);
#32650=EDGE_CURVE('',#26156,#26154,#24317,.T.);
#32651=EDGE_CURVE('',#26157,#26155,#24318,.T.);
#32652=EDGE_CURVE('',#26157,#26158,#11801,.T.);
#32653=EDGE_CURVE('',#26158,#26156,#24319,.T.);
#32654=EDGE_CURVE('',#26159,#26157,#24320,.T.);
#32655=EDGE_CURVE('',#26159,#26160,#11802,.T.);
#32656=EDGE_CURVE('',#26160,#26158,#24321,.T.);
#32657=EDGE_CURVE('',#26161,#26159,#24322,.T.);
#32658=EDGE_CURVE('',#26161,#26162,#11803,.T.);
#32659=EDGE_CURVE('',#26162,#26160,#24323,.T.);
#32660=EDGE_CURVE('',#26163,#26161,#24324,.T.);
#32661=EDGE_CURVE('',#26163,#26164,#11804,.T.);
#32662=EDGE_CURVE('',#26164,#26162,#24325,.T.);
#32663=EDGE_CURVE('',#26165,#26163,#24326,.T.);
#32664=EDGE_CURVE('',#26165,#26166,#11805,.T.);
#32665=EDGE_CURVE('',#26166,#26164,#24327,.T.);
#32666=EDGE_CURVE('',#26167,#26165,#24328,.T.);
#32667=EDGE_CURVE('',#26167,#26168,#11806,.T.);
#32668=EDGE_CURVE('',#26168,#26166,#24329,.T.);
#32669=EDGE_CURVE('',#26169,#26167,#24330,.T.);
#32670=EDGE_CURVE('',#26169,#26170,#11807,.T.);
#32671=EDGE_CURVE('',#26170,#26168,#24331,.T.);
#32672=EDGE_CURVE('',#26171,#26169,#24332,.T.);
#32673=EDGE_CURVE('',#26171,#26172,#11808,.T.);
#32674=EDGE_CURVE('',#26172,#26170,#24333,.T.);
#32675=EDGE_CURVE('',#26173,#26171,#24334,.T.);
#32676=EDGE_CURVE('',#26173,#26174,#11809,.T.);
#32677=EDGE_CURVE('',#26174,#26172,#24335,.T.);
#32678=EDGE_CURVE('',#26175,#26173,#24336,.T.);
#32679=EDGE_CURVE('',#26175,#26176,#11810,.T.);
#32680=EDGE_CURVE('',#26176,#26174,#24337,.T.);
#32681=EDGE_CURVE('',#26177,#26175,#11811,.T.);
#32682=EDGE_CURVE('',#26177,#26178,#11812,.T.);
#32683=EDGE_CURVE('',#26178,#26176,#11813,.T.);
#32684=EDGE_CURVE('',#26136,#26177,#24338,.T.);
#32685=EDGE_CURVE('',#26138,#26178,#24339,.T.);
#32686=EDGE_CURVE('',#26179,#26180,#11814,.T.);
#32687=EDGE_CURVE('',#26179,#26181,#11815,.T.);
#32688=EDGE_CURVE('',#26181,#26182,#11816,.T.);
#32689=EDGE_CURVE('',#26180,#26182,#11817,.T.);
#32690=EDGE_CURVE('',#26183,#26179,#11818,.T.);
#32691=EDGE_CURVE('',#26183,#26184,#11819,.T.);
#32692=EDGE_CURVE('',#26184,#26181,#11820,.T.);
#32693=EDGE_CURVE('',#26185,#26183,#11821,.T.);
#32694=EDGE_CURVE('',#26185,#26186,#11822,.T.);
#32695=EDGE_CURVE('',#26186,#26184,#11823,.T.);
#32696=EDGE_CURVE('',#26180,#26185,#11824,.T.);
#32697=EDGE_CURVE('',#26182,#26186,#11825,.T.);
#32698=EDGE_CURVE('',#26187,#26188,#11826,.T.);
#32699=EDGE_CURVE('',#26187,#26189,#11827,.T.);
#32700=EDGE_CURVE('',#26189,#26190,#11828,.T.);
#32701=EDGE_CURVE('',#26188,#26190,#11829,.T.);
#32702=EDGE_CURVE('',#26191,#26187,#11830,.T.);
#32703=EDGE_CURVE('',#26191,#26192,#11831,.T.);
#32704=EDGE_CURVE('',#26192,#26189,#11832,.T.);
#32705=EDGE_CURVE('',#26193,#26191,#11833,.T.);
#32706=EDGE_CURVE('',#26193,#26194,#11834,.T.);
#32707=EDGE_CURVE('',#26194,#26192,#11835,.T.);
#32708=EDGE_CURVE('',#26188,#26193,#11836,.T.);
#32709=EDGE_CURVE('',#26190,#26194,#11837,.T.);
#32710=EDGE_CURVE('',#26195,#26196,#11838,.T.);
#32711=EDGE_CURVE('',#26195,#26197,#11839,.T.);
#32712=EDGE_CURVE('',#26197,#26198,#11840,.T.);
#32713=EDGE_CURVE('',#26196,#26198,#11841,.T.);
#32714=EDGE_CURVE('',#26199,#26195,#11842,.T.);
#32715=EDGE_CURVE('',#26199,#26200,#11843,.T.);
#32716=EDGE_CURVE('',#26200,#26197,#11844,.T.);
#32717=EDGE_CURVE('',#26201,#26199,#11845,.T.);
#32718=EDGE_CURVE('',#26201,#26202,#11846,.T.);
#32719=EDGE_CURVE('',#26202,#26200,#11847,.T.);
#32720=EDGE_CURVE('',#26196,#26201,#11848,.T.);
#32721=EDGE_CURVE('',#26198,#26202,#11849,.T.);
#32722=EDGE_CURVE('',#26203,#26204,#11850,.T.);
#32723=EDGE_CURVE('',#26203,#26205,#11851,.T.);
#32724=EDGE_CURVE('',#26205,#26206,#11852,.T.);
#32725=EDGE_CURVE('',#26204,#26206,#11853,.T.);
#32726=EDGE_CURVE('',#26207,#26203,#11854,.T.);
#32727=EDGE_CURVE('',#26207,#26208,#11855,.T.);
#32728=EDGE_CURVE('',#26208,#26205,#11856,.T.);
#32729=EDGE_CURVE('',#26209,#26207,#11857,.T.);
#32730=EDGE_CURVE('',#26209,#26210,#11858,.T.);
#32731=EDGE_CURVE('',#26210,#26208,#11859,.T.);
#32732=EDGE_CURVE('',#26204,#26209,#11860,.T.);
#32733=EDGE_CURVE('',#26206,#26210,#11861,.T.);
#32734=EDGE_CURVE('',#26211,#26212,#11862,.T.);
#32735=EDGE_CURVE('',#26211,#26213,#11863,.T.);
#32736=EDGE_CURVE('',#26213,#26214,#11864,.T.);
#32737=EDGE_CURVE('',#26212,#26214,#11865,.T.);
#32738=EDGE_CURVE('',#26215,#26211,#11866,.T.);
#32739=EDGE_CURVE('',#26215,#26216,#11867,.T.);
#32740=EDGE_CURVE('',#26216,#26213,#11868,.T.);
#32741=EDGE_CURVE('',#26217,#26215,#11869,.T.);
#32742=EDGE_CURVE('',#26217,#26218,#11870,.T.);
#32743=EDGE_CURVE('',#26218,#26216,#11871,.T.);
#32744=EDGE_CURVE('',#26212,#26217,#11872,.T.);
#32745=EDGE_CURVE('',#26214,#26218,#11873,.T.);
#32746=EDGE_CURVE('',#26219,#26220,#11874,.T.);
#32747=EDGE_CURVE('',#26219,#26221,#11875,.T.);
#32748=EDGE_CURVE('',#26221,#26222,#11876,.T.);
#32749=EDGE_CURVE('',#26220,#26222,#11877,.T.);
#32750=EDGE_CURVE('',#26223,#26219,#11878,.T.);
#32751=EDGE_CURVE('',#26223,#26224,#11879,.T.);
#32752=EDGE_CURVE('',#26224,#26221,#11880,.T.);
#32753=EDGE_CURVE('',#26225,#26223,#11881,.T.);
#32754=EDGE_CURVE('',#26225,#26226,#11882,.T.);
#32755=EDGE_CURVE('',#26226,#26224,#11883,.T.);
#32756=EDGE_CURVE('',#26220,#26225,#11884,.T.);
#32757=EDGE_CURVE('',#26222,#26226,#11885,.T.);
#32758=EDGE_CURVE('',#26227,#26228,#11886,.T.);
#32759=EDGE_CURVE('',#26227,#26229,#11887,.T.);
#32760=EDGE_CURVE('',#26229,#26230,#11888,.T.);
#32761=EDGE_CURVE('',#26228,#26230,#11889,.T.);
#32762=EDGE_CURVE('',#26231,#26227,#11890,.T.);
#32763=EDGE_CURVE('',#26231,#26232,#11891,.T.);
#32764=EDGE_CURVE('',#26232,#26229,#11892,.T.);
#32765=EDGE_CURVE('',#26233,#26231,#11893,.T.);
#32766=EDGE_CURVE('',#26233,#26234,#11894,.T.);
#32767=EDGE_CURVE('',#26234,#26232,#11895,.T.);
#32768=EDGE_CURVE('',#26228,#26233,#11896,.T.);
#32769=EDGE_CURVE('',#26230,#26234,#11897,.T.);
#32770=EDGE_CURVE('',#26235,#26236,#11898,.T.);
#32771=EDGE_CURVE('',#26235,#26237,#11899,.T.);
#32772=EDGE_CURVE('',#26237,#26238,#11900,.T.);
#32773=EDGE_CURVE('',#26236,#26238,#11901,.T.);
#32774=EDGE_CURVE('',#26239,#26235,#11902,.T.);
#32775=EDGE_CURVE('',#26239,#26240,#11903,.T.);
#32776=EDGE_CURVE('',#26240,#26237,#11904,.T.);
#32777=EDGE_CURVE('',#26241,#26239,#11905,.T.);
#32778=EDGE_CURVE('',#26241,#26242,#11906,.T.);
#32779=EDGE_CURVE('',#26242,#26240,#11907,.T.);
#32780=EDGE_CURVE('',#26236,#26241,#11908,.T.);
#32781=EDGE_CURVE('',#26238,#26242,#11909,.T.);
#32782=EDGE_CURVE('',#26243,#26244,#11910,.T.);
#32783=EDGE_CURVE('',#26243,#26245,#11911,.T.);
#32784=EDGE_CURVE('',#26245,#26246,#11912,.T.);
#32785=EDGE_CURVE('',#26244,#26246,#11913,.T.);
#32786=EDGE_CURVE('',#26247,#26243,#11914,.T.);
#32787=EDGE_CURVE('',#26247,#26248,#11915,.T.);
#32788=EDGE_CURVE('',#26248,#26245,#11916,.T.);
#32789=EDGE_CURVE('',#26249,#26247,#11917,.T.);
#32790=EDGE_CURVE('',#26249,#26250,#11918,.T.);
#32791=EDGE_CURVE('',#26250,#26248,#11919,.T.);
#32792=EDGE_CURVE('',#26244,#26249,#11920,.T.);
#32793=EDGE_CURVE('',#26246,#26250,#11921,.T.);
#32794=EDGE_CURVE('',#26251,#26252,#11922,.T.);
#32795=EDGE_CURVE('',#26251,#26253,#11923,.T.);
#32796=EDGE_CURVE('',#26253,#26254,#11924,.T.);
#32797=EDGE_CURVE('',#26252,#26254,#11925,.T.);
#32798=EDGE_CURVE('',#26255,#26251,#11926,.T.);
#32799=EDGE_CURVE('',#26255,#26256,#11927,.T.);
#32800=EDGE_CURVE('',#26256,#26253,#11928,.T.);
#32801=EDGE_CURVE('',#26257,#26255,#11929,.T.);
#32802=EDGE_CURVE('',#26257,#26258,#11930,.T.);
#32803=EDGE_CURVE('',#26258,#26256,#11931,.T.);
#32804=EDGE_CURVE('',#26252,#26257,#11932,.T.);
#32805=EDGE_CURVE('',#26254,#26258,#11933,.T.);
#32806=EDGE_CURVE('',#26259,#26260,#11934,.T.);
#32807=EDGE_CURVE('',#26259,#26261,#11935,.T.);
#32808=EDGE_CURVE('',#26261,#26262,#11936,.T.);
#32809=EDGE_CURVE('',#26260,#26262,#11937,.T.);
#32810=EDGE_CURVE('',#26263,#26259,#11938,.T.);
#32811=EDGE_CURVE('',#26263,#26264,#11939,.T.);
#32812=EDGE_CURVE('',#26264,#26261,#11940,.T.);
#32813=EDGE_CURVE('',#26265,#26263,#11941,.T.);
#32814=EDGE_CURVE('',#26265,#26266,#11942,.T.);
#32815=EDGE_CURVE('',#26266,#26264,#11943,.T.);
#32816=EDGE_CURVE('',#26260,#26265,#11944,.T.);
#32817=EDGE_CURVE('',#26262,#26266,#11945,.T.);
#32818=EDGE_CURVE('',#26267,#26268,#11946,.T.);
#32819=EDGE_CURVE('',#26267,#26269,#11947,.T.);
#32820=EDGE_CURVE('',#26269,#26270,#11948,.T.);
#32821=EDGE_CURVE('',#26268,#26270,#11949,.T.);
#32822=EDGE_CURVE('',#26271,#26267,#11950,.T.);
#32823=EDGE_CURVE('',#26271,#26272,#11951,.T.);
#32824=EDGE_CURVE('',#26272,#26269,#11952,.T.);
#32825=EDGE_CURVE('',#26273,#26271,#11953,.T.);
#32826=EDGE_CURVE('',#26273,#26274,#11954,.T.);
#32827=EDGE_CURVE('',#26274,#26272,#11955,.T.);
#32828=EDGE_CURVE('',#26268,#26273,#11956,.T.);
#32829=EDGE_CURVE('',#26270,#26274,#11957,.T.);
#32830=EDGE_CURVE('',#26275,#26276,#11958,.T.);
#32831=EDGE_CURVE('',#26275,#26277,#11959,.T.);
#32832=EDGE_CURVE('',#26277,#26278,#11960,.T.);
#32833=EDGE_CURVE('',#26276,#26278,#11961,.T.);
#32834=EDGE_CURVE('',#26279,#26275,#11962,.T.);
#32835=EDGE_CURVE('',#26279,#26280,#11963,.T.);
#32836=EDGE_CURVE('',#26280,#26277,#11964,.T.);
#32837=EDGE_CURVE('',#26281,#26279,#11965,.T.);
#32838=EDGE_CURVE('',#26281,#26282,#11966,.T.);
#32839=EDGE_CURVE('',#26282,#26280,#11967,.T.);
#32840=EDGE_CURVE('',#26276,#26281,#11968,.T.);
#32841=EDGE_CURVE('',#26278,#26282,#11969,.T.);
#32842=EDGE_CURVE('',#26283,#26284,#11970,.T.);
#32843=EDGE_CURVE('',#26283,#26285,#11971,.T.);
#32844=EDGE_CURVE('',#26285,#26286,#11972,.T.);
#32845=EDGE_CURVE('',#26284,#26286,#11973,.T.);
#32846=EDGE_CURVE('',#26287,#26283,#11974,.T.);
#32847=EDGE_CURVE('',#26287,#26288,#11975,.T.);
#32848=EDGE_CURVE('',#26288,#26285,#11976,.T.);
#32849=EDGE_CURVE('',#26289,#26287,#11977,.T.);
#32850=EDGE_CURVE('',#26289,#26290,#11978,.T.);
#32851=EDGE_CURVE('',#26290,#26288,#11979,.T.);
#32852=EDGE_CURVE('',#26284,#26289,#11980,.T.);
#32853=EDGE_CURVE('',#26286,#26290,#11981,.T.);
#32854=EDGE_CURVE('',#26291,#26292,#11982,.T.);
#32855=EDGE_CURVE('',#26291,#26293,#11983,.T.);
#32856=EDGE_CURVE('',#26293,#26294,#11984,.T.);
#32857=EDGE_CURVE('',#26292,#26294,#11985,.T.);
#32858=EDGE_CURVE('',#26295,#26291,#11986,.T.);
#32859=EDGE_CURVE('',#26295,#26296,#11987,.T.);
#32860=EDGE_CURVE('',#26296,#26293,#11988,.T.);
#32861=EDGE_CURVE('',#26297,#26295,#11989,.T.);
#32862=EDGE_CURVE('',#26297,#26298,#11990,.T.);
#32863=EDGE_CURVE('',#26298,#26296,#11991,.T.);
#32864=EDGE_CURVE('',#26292,#26297,#11992,.T.);
#32865=EDGE_CURVE('',#26294,#26298,#11993,.T.);
#32866=EDGE_CURVE('',#26299,#26300,#11994,.T.);
#32867=EDGE_CURVE('',#26299,#26301,#11995,.T.);
#32868=EDGE_CURVE('',#26301,#26302,#11996,.T.);
#32869=EDGE_CURVE('',#26300,#26302,#11997,.T.);
#32870=EDGE_CURVE('',#26303,#26299,#11998,.T.);
#32871=EDGE_CURVE('',#26303,#26304,#11999,.T.);
#32872=EDGE_CURVE('',#26304,#26301,#12000,.T.);
#32873=EDGE_CURVE('',#26305,#26303,#12001,.T.);
#32874=EDGE_CURVE('',#26305,#26306,#12002,.T.);
#32875=EDGE_CURVE('',#26306,#26304,#12003,.T.);
#32876=EDGE_CURVE('',#26300,#26305,#12004,.T.);
#32877=EDGE_CURVE('',#26302,#26306,#12005,.T.);
#32878=EDGE_CURVE('',#26307,#26308,#12006,.T.);
#32879=EDGE_CURVE('',#26307,#26309,#12007,.T.);
#32880=EDGE_CURVE('',#26309,#26310,#12008,.T.);
#32881=EDGE_CURVE('',#26308,#26310,#12009,.T.);
#32882=EDGE_CURVE('',#26311,#26307,#12010,.T.);
#32883=EDGE_CURVE('',#26311,#26312,#12011,.T.);
#32884=EDGE_CURVE('',#26312,#26309,#12012,.T.);
#32885=EDGE_CURVE('',#26313,#26311,#12013,.T.);
#32886=EDGE_CURVE('',#26313,#26314,#12014,.T.);
#32887=EDGE_CURVE('',#26314,#26312,#12015,.T.);
#32888=EDGE_CURVE('',#26308,#26313,#12016,.T.);
#32889=EDGE_CURVE('',#26310,#26314,#12017,.T.);
#32890=EDGE_CURVE('',#26315,#26316,#12018,.T.);
#32891=EDGE_CURVE('',#26315,#26317,#12019,.T.);
#32892=EDGE_CURVE('',#26317,#26318,#12020,.T.);
#32893=EDGE_CURVE('',#26316,#26318,#12021,.T.);
#32894=EDGE_CURVE('',#26319,#26315,#12022,.T.);
#32895=EDGE_CURVE('',#26319,#26320,#12023,.T.);
#32896=EDGE_CURVE('',#26320,#26317,#12024,.T.);
#32897=EDGE_CURVE('',#26321,#26319,#12025,.T.);
#32898=EDGE_CURVE('',#26321,#26322,#12026,.T.);
#32899=EDGE_CURVE('',#26322,#26320,#12027,.T.);
#32900=EDGE_CURVE('',#26316,#26321,#12028,.T.);
#32901=EDGE_CURVE('',#26318,#26322,#12029,.T.);
#32902=EDGE_CURVE('',#26323,#26324,#12030,.T.);
#32903=EDGE_CURVE('',#26323,#26325,#12031,.T.);
#32904=EDGE_CURVE('',#26325,#26326,#12032,.T.);
#32905=EDGE_CURVE('',#26324,#26326,#12033,.T.);
#32906=EDGE_CURVE('',#26327,#26323,#12034,.T.);
#32907=EDGE_CURVE('',#26327,#26328,#12035,.T.);
#32908=EDGE_CURVE('',#26328,#26325,#12036,.T.);
#32909=EDGE_CURVE('',#26329,#26327,#12037,.T.);
#32910=EDGE_CURVE('',#26329,#26330,#12038,.T.);
#32911=EDGE_CURVE('',#26330,#26328,#12039,.T.);
#32912=EDGE_CURVE('',#26324,#26329,#12040,.T.);
#32913=EDGE_CURVE('',#26326,#26330,#12041,.T.);
#32914=EDGE_CURVE('',#26331,#26332,#12042,.T.);
#32915=EDGE_CURVE('',#26331,#26333,#12043,.T.);
#32916=EDGE_CURVE('',#26333,#26334,#12044,.T.);
#32917=EDGE_CURVE('',#26332,#26334,#12045,.T.);
#32918=EDGE_CURVE('',#26335,#26331,#12046,.T.);
#32919=EDGE_CURVE('',#26335,#26336,#12047,.T.);
#32920=EDGE_CURVE('',#26336,#26333,#12048,.T.);
#32921=EDGE_CURVE('',#26337,#26335,#12049,.T.);
#32922=EDGE_CURVE('',#26337,#26338,#12050,.T.);
#32923=EDGE_CURVE('',#26338,#26336,#12051,.T.);
#32924=EDGE_CURVE('',#26332,#26337,#12052,.T.);
#32925=EDGE_CURVE('',#26334,#26338,#12053,.T.);
#32926=EDGE_CURVE('',#26339,#26340,#12054,.T.);
#32927=EDGE_CURVE('',#26339,#26341,#12055,.T.);
#32928=EDGE_CURVE('',#26341,#26342,#12056,.T.);
#32929=EDGE_CURVE('',#26340,#26342,#12057,.T.);
#32930=EDGE_CURVE('',#26343,#26339,#12058,.T.);
#32931=EDGE_CURVE('',#26343,#26344,#12059,.T.);
#32932=EDGE_CURVE('',#26344,#26341,#12060,.T.);
#32933=EDGE_CURVE('',#26345,#26343,#12061,.T.);
#32934=EDGE_CURVE('',#26345,#26346,#12062,.T.);
#32935=EDGE_CURVE('',#26346,#26344,#12063,.T.);
#32936=EDGE_CURVE('',#26340,#26345,#12064,.T.);
#32937=EDGE_CURVE('',#26342,#26346,#12065,.T.);
#32938=EDGE_CURVE('',#26347,#26348,#12066,.T.);
#32939=EDGE_CURVE('',#26347,#26349,#12067,.T.);
#32940=EDGE_CURVE('',#26349,#26350,#12068,.T.);
#32941=EDGE_CURVE('',#26348,#26350,#12069,.T.);
#32942=EDGE_CURVE('',#26351,#26347,#12070,.T.);
#32943=EDGE_CURVE('',#26351,#26352,#12071,.T.);
#32944=EDGE_CURVE('',#26352,#26349,#12072,.T.);
#32945=EDGE_CURVE('',#26353,#26351,#12073,.T.);
#32946=EDGE_CURVE('',#26353,#26354,#12074,.T.);
#32947=EDGE_CURVE('',#26354,#26352,#12075,.T.);
#32948=EDGE_CURVE('',#26348,#26353,#12076,.T.);
#32949=EDGE_CURVE('',#26350,#26354,#12077,.T.);
#32950=EDGE_CURVE('',#26355,#26356,#12078,.T.);
#32951=EDGE_CURVE('',#26355,#26357,#12079,.T.);
#32952=EDGE_CURVE('',#26357,#26358,#12080,.T.);
#32953=EDGE_CURVE('',#26356,#26358,#12081,.T.);
#32954=EDGE_CURVE('',#26359,#26355,#12082,.T.);
#32955=EDGE_CURVE('',#26359,#26360,#12083,.T.);
#32956=EDGE_CURVE('',#26360,#26357,#12084,.T.);
#32957=EDGE_CURVE('',#26361,#26359,#12085,.T.);
#32958=EDGE_CURVE('',#26361,#26362,#12086,.T.);
#32959=EDGE_CURVE('',#26362,#26360,#12087,.T.);
#32960=EDGE_CURVE('',#26356,#26361,#12088,.T.);
#32961=EDGE_CURVE('',#26358,#26362,#12089,.T.);
#32962=EDGE_CURVE('',#26363,#26364,#12090,.T.);
#32963=EDGE_CURVE('',#26363,#26365,#12091,.T.);
#32964=EDGE_CURVE('',#26365,#26366,#12092,.T.);
#32965=EDGE_CURVE('',#26364,#26366,#12093,.T.);
#32966=EDGE_CURVE('',#26367,#26363,#12094,.T.);
#32967=EDGE_CURVE('',#26367,#26368,#12095,.T.);
#32968=EDGE_CURVE('',#26368,#26365,#12096,.T.);
#32969=EDGE_CURVE('',#26369,#26367,#12097,.T.);
#32970=EDGE_CURVE('',#26369,#26370,#12098,.T.);
#32971=EDGE_CURVE('',#26370,#26368,#12099,.T.);
#32972=EDGE_CURVE('',#26364,#26369,#12100,.T.);
#32973=EDGE_CURVE('',#26366,#26370,#12101,.T.);
#32974=EDGE_CURVE('',#26371,#26372,#12102,.T.);
#32975=EDGE_CURVE('',#26371,#26373,#12103,.T.);
#32976=EDGE_CURVE('',#26373,#26374,#12104,.T.);
#32977=EDGE_CURVE('',#26372,#26374,#12105,.T.);
#32978=EDGE_CURVE('',#26375,#26371,#12106,.T.);
#32979=EDGE_CURVE('',#26375,#26376,#12107,.T.);
#32980=EDGE_CURVE('',#26376,#26373,#12108,.T.);
#32981=EDGE_CURVE('',#26377,#26375,#12109,.T.);
#32982=EDGE_CURVE('',#26377,#26378,#12110,.T.);
#32983=EDGE_CURVE('',#26378,#26376,#12111,.T.);
#32984=EDGE_CURVE('',#26372,#26377,#12112,.T.);
#32985=EDGE_CURVE('',#26374,#26378,#12113,.T.);
#32986=EDGE_CURVE('',#26379,#26380,#12114,.T.);
#32987=EDGE_CURVE('',#26379,#26381,#12115,.T.);
#32988=EDGE_CURVE('',#26381,#26382,#12116,.T.);
#32989=EDGE_CURVE('',#26380,#26382,#12117,.T.);
#32990=EDGE_CURVE('',#26383,#26379,#12118,.T.);
#32991=EDGE_CURVE('',#26383,#26384,#12119,.T.);
#32992=EDGE_CURVE('',#26384,#26381,#12120,.T.);
#32993=EDGE_CURVE('',#26385,#26383,#12121,.T.);
#32994=EDGE_CURVE('',#26385,#26386,#12122,.T.);
#32995=EDGE_CURVE('',#26386,#26384,#12123,.T.);
#32996=EDGE_CURVE('',#26380,#26385,#12124,.T.);
#32997=EDGE_CURVE('',#26382,#26386,#12125,.T.);
#32998=EDGE_CURVE('',#26387,#26388,#12126,.T.);
#32999=EDGE_CURVE('',#26387,#26389,#12127,.T.);
#33000=EDGE_CURVE('',#26389,#26390,#12128,.T.);
#33001=EDGE_CURVE('',#26388,#26390,#12129,.T.);
#33002=EDGE_CURVE('',#26391,#26387,#12130,.T.);
#33003=EDGE_CURVE('',#26391,#26392,#12131,.T.);
#33004=EDGE_CURVE('',#26392,#26389,#12132,.T.);
#33005=EDGE_CURVE('',#26393,#26391,#12133,.T.);
#33006=EDGE_CURVE('',#26393,#26394,#12134,.T.);
#33007=EDGE_CURVE('',#26394,#26392,#12135,.T.);
#33008=EDGE_CURVE('',#26388,#26393,#12136,.T.);
#33009=EDGE_CURVE('',#26390,#26394,#12137,.T.);
#33010=EDGE_CURVE('',#26395,#26396,#12138,.T.);
#33011=EDGE_CURVE('',#26395,#26397,#12139,.T.);
#33012=EDGE_CURVE('',#26397,#26398,#12140,.T.);
#33013=EDGE_CURVE('',#26396,#26398,#12141,.T.);
#33014=EDGE_CURVE('',#26399,#26395,#12142,.T.);
#33015=EDGE_CURVE('',#26399,#26400,#12143,.T.);
#33016=EDGE_CURVE('',#26400,#26397,#12144,.T.);
#33017=EDGE_CURVE('',#26401,#26399,#12145,.T.);
#33018=EDGE_CURVE('',#26401,#26402,#12146,.T.);
#33019=EDGE_CURVE('',#26402,#26400,#12147,.T.);
#33020=EDGE_CURVE('',#26396,#26401,#12148,.T.);
#33021=EDGE_CURVE('',#26398,#26402,#12149,.T.);
#33022=EDGE_CURVE('',#26403,#26404,#12150,.T.);
#33023=EDGE_CURVE('',#26403,#26405,#12151,.T.);
#33024=EDGE_CURVE('',#26405,#26406,#12152,.T.);
#33025=EDGE_CURVE('',#26404,#26406,#12153,.T.);
#33026=EDGE_CURVE('',#26407,#26403,#12154,.T.);
#33027=EDGE_CURVE('',#26407,#26408,#12155,.T.);
#33028=EDGE_CURVE('',#26408,#26405,#12156,.T.);
#33029=EDGE_CURVE('',#26409,#26407,#12157,.T.);
#33030=EDGE_CURVE('',#26409,#26410,#12158,.T.);
#33031=EDGE_CURVE('',#26410,#26408,#12159,.T.);
#33032=EDGE_CURVE('',#26404,#26409,#12160,.T.);
#33033=EDGE_CURVE('',#26406,#26410,#12161,.T.);
#33034=EDGE_CURVE('',#26411,#26412,#12162,.T.);
#33035=EDGE_CURVE('',#26411,#26413,#12163,.T.);
#33036=EDGE_CURVE('',#26413,#26414,#12164,.T.);
#33037=EDGE_CURVE('',#26412,#26414,#12165,.T.);
#33038=EDGE_CURVE('',#26415,#26411,#12166,.T.);
#33039=EDGE_CURVE('',#26415,#26416,#12167,.T.);
#33040=EDGE_CURVE('',#26416,#26413,#12168,.T.);
#33041=EDGE_CURVE('',#26417,#26415,#12169,.T.);
#33042=EDGE_CURVE('',#26417,#26418,#12170,.T.);
#33043=EDGE_CURVE('',#26418,#26416,#12171,.T.);
#33044=EDGE_CURVE('',#26412,#26417,#12172,.T.);
#33045=EDGE_CURVE('',#26414,#26418,#12173,.T.);
#33046=EDGE_CURVE('',#26419,#26420,#12174,.T.);
#33047=EDGE_CURVE('',#26419,#26421,#12175,.T.);
#33048=EDGE_CURVE('',#26421,#26422,#12176,.T.);
#33049=EDGE_CURVE('',#26420,#26422,#12177,.T.);
#33050=EDGE_CURVE('',#26423,#26419,#12178,.T.);
#33051=EDGE_CURVE('',#26423,#26424,#12179,.T.);
#33052=EDGE_CURVE('',#26424,#26421,#12180,.T.);
#33053=EDGE_CURVE('',#26425,#26423,#12181,.T.);
#33054=EDGE_CURVE('',#26425,#26426,#12182,.T.);
#33055=EDGE_CURVE('',#26426,#26424,#12183,.T.);
#33056=EDGE_CURVE('',#26420,#26425,#12184,.T.);
#33057=EDGE_CURVE('',#26422,#26426,#12185,.T.);
#33058=EDGE_CURVE('',#26427,#26428,#12186,.T.);
#33059=EDGE_CURVE('',#26427,#26429,#12187,.T.);
#33060=EDGE_CURVE('',#26429,#26430,#12188,.T.);
#33061=EDGE_CURVE('',#26428,#26430,#12189,.T.);
#33062=EDGE_CURVE('',#26431,#26427,#12190,.T.);
#33063=EDGE_CURVE('',#26431,#26432,#12191,.T.);
#33064=EDGE_CURVE('',#26432,#26429,#12192,.T.);
#33065=EDGE_CURVE('',#26433,#26431,#12193,.T.);
#33066=EDGE_CURVE('',#26433,#26434,#12194,.T.);
#33067=EDGE_CURVE('',#26434,#26432,#12195,.T.);
#33068=EDGE_CURVE('',#26428,#26433,#12196,.T.);
#33069=EDGE_CURVE('',#26430,#26434,#12197,.T.);
#33070=EDGE_CURVE('',#26435,#26436,#12198,.T.);
#33071=EDGE_CURVE('',#26435,#26437,#12199,.T.);
#33072=EDGE_CURVE('',#26437,#26438,#12200,.T.);
#33073=EDGE_CURVE('',#26436,#26438,#12201,.T.);
#33074=EDGE_CURVE('',#26439,#26435,#12202,.T.);
#33075=EDGE_CURVE('',#26439,#26440,#12203,.T.);
#33076=EDGE_CURVE('',#26440,#26437,#12204,.T.);
#33077=EDGE_CURVE('',#26441,#26439,#12205,.T.);
#33078=EDGE_CURVE('',#26441,#26442,#12206,.T.);
#33079=EDGE_CURVE('',#26442,#26440,#12207,.T.);
#33080=EDGE_CURVE('',#26436,#26441,#12208,.T.);
#33081=EDGE_CURVE('',#26438,#26442,#12209,.T.);
#33082=EDGE_CURVE('',#26443,#26444,#12210,.T.);
#33083=EDGE_CURVE('',#26443,#26445,#12211,.T.);
#33084=EDGE_CURVE('',#26445,#26446,#12212,.T.);
#33085=EDGE_CURVE('',#26444,#26446,#12213,.T.);
#33086=EDGE_CURVE('',#26447,#26443,#12214,.T.);
#33087=EDGE_CURVE('',#26447,#26448,#12215,.T.);
#33088=EDGE_CURVE('',#26448,#26445,#12216,.T.);
#33089=EDGE_CURVE('',#26449,#26447,#12217,.T.);
#33090=EDGE_CURVE('',#26449,#26450,#12218,.T.);
#33091=EDGE_CURVE('',#26450,#26448,#12219,.T.);
#33092=EDGE_CURVE('',#26444,#26449,#12220,.T.);
#33093=EDGE_CURVE('',#26446,#26450,#12221,.T.);
#33094=EDGE_CURVE('',#26451,#26452,#12222,.T.);
#33095=EDGE_CURVE('',#26451,#26453,#12223,.T.);
#33096=EDGE_CURVE('',#26453,#26454,#12224,.T.);
#33097=EDGE_CURVE('',#26452,#26454,#12225,.T.);
#33098=EDGE_CURVE('',#26455,#26451,#12226,.T.);
#33099=EDGE_CURVE('',#26455,#26456,#12227,.T.);
#33100=EDGE_CURVE('',#26456,#26453,#12228,.T.);
#33101=EDGE_CURVE('',#26457,#26455,#12229,.T.);
#33102=EDGE_CURVE('',#26457,#26458,#12230,.T.);
#33103=EDGE_CURVE('',#26458,#26456,#12231,.T.);
#33104=EDGE_CURVE('',#26452,#26457,#12232,.T.);
#33105=EDGE_CURVE('',#26454,#26458,#12233,.T.);
#33106=EDGE_CURVE('',#26459,#26460,#12234,.T.);
#33107=EDGE_CURVE('',#26459,#26461,#12235,.T.);
#33108=EDGE_CURVE('',#26461,#26462,#12236,.T.);
#33109=EDGE_CURVE('',#26460,#26462,#12237,.T.);
#33110=EDGE_CURVE('',#26463,#26459,#12238,.T.);
#33111=EDGE_CURVE('',#26463,#26464,#12239,.T.);
#33112=EDGE_CURVE('',#26464,#26461,#12240,.T.);
#33113=EDGE_CURVE('',#26465,#26463,#12241,.T.);
#33114=EDGE_CURVE('',#26465,#26466,#12242,.T.);
#33115=EDGE_CURVE('',#26466,#26464,#12243,.T.);
#33116=EDGE_CURVE('',#26460,#26465,#12244,.T.);
#33117=EDGE_CURVE('',#26462,#26466,#12245,.T.);
#33118=EDGE_CURVE('',#26467,#26468,#12246,.T.);
#33119=EDGE_CURVE('',#26467,#26469,#12247,.T.);
#33120=EDGE_CURVE('',#26469,#26470,#12248,.T.);
#33121=EDGE_CURVE('',#26468,#26470,#12249,.T.);
#33122=EDGE_CURVE('',#26471,#26467,#12250,.T.);
#33123=EDGE_CURVE('',#26471,#26472,#12251,.T.);
#33124=EDGE_CURVE('',#26472,#26469,#12252,.T.);
#33125=EDGE_CURVE('',#26473,#26471,#12253,.T.);
#33126=EDGE_CURVE('',#26473,#26474,#12254,.T.);
#33127=EDGE_CURVE('',#26474,#26472,#12255,.T.);
#33128=EDGE_CURVE('',#26468,#26473,#12256,.T.);
#33129=EDGE_CURVE('',#26470,#26474,#12257,.T.);
#33130=EDGE_CURVE('',#26475,#26476,#12258,.T.);
#33131=EDGE_CURVE('',#26475,#26477,#12259,.T.);
#33132=EDGE_CURVE('',#26477,#26478,#12260,.T.);
#33133=EDGE_CURVE('',#26476,#26478,#12261,.T.);
#33134=EDGE_CURVE('',#26479,#26475,#12262,.T.);
#33135=EDGE_CURVE('',#26479,#26480,#12263,.T.);
#33136=EDGE_CURVE('',#26480,#26477,#12264,.T.);
#33137=EDGE_CURVE('',#26481,#26479,#12265,.T.);
#33138=EDGE_CURVE('',#26481,#26482,#12266,.T.);
#33139=EDGE_CURVE('',#26482,#26480,#12267,.T.);
#33140=EDGE_CURVE('',#26476,#26481,#12268,.T.);
#33141=EDGE_CURVE('',#26478,#26482,#12269,.T.);
#33142=EDGE_CURVE('',#26483,#26484,#12270,.T.);
#33143=EDGE_CURVE('',#26483,#26485,#12271,.T.);
#33144=EDGE_CURVE('',#26485,#26486,#12272,.T.);
#33145=EDGE_CURVE('',#26484,#26486,#12273,.T.);
#33146=EDGE_CURVE('',#26487,#26483,#12274,.T.);
#33147=EDGE_CURVE('',#26487,#26488,#12275,.T.);
#33148=EDGE_CURVE('',#26488,#26485,#12276,.T.);
#33149=EDGE_CURVE('',#26489,#26487,#12277,.T.);
#33150=EDGE_CURVE('',#26489,#26490,#12278,.T.);
#33151=EDGE_CURVE('',#26490,#26488,#12279,.T.);
#33152=EDGE_CURVE('',#26484,#26489,#12280,.T.);
#33153=EDGE_CURVE('',#26486,#26490,#12281,.T.);
#33154=EDGE_CURVE('',#26491,#26492,#12282,.T.);
#33155=EDGE_CURVE('',#26491,#26493,#12283,.T.);
#33156=EDGE_CURVE('',#26493,#26494,#12284,.T.);
#33157=EDGE_CURVE('',#26492,#26494,#12285,.T.);
#33158=EDGE_CURVE('',#26495,#26491,#12286,.T.);
#33159=EDGE_CURVE('',#26495,#26496,#12287,.T.);
#33160=EDGE_CURVE('',#26496,#26493,#12288,.T.);
#33161=EDGE_CURVE('',#26497,#26495,#12289,.T.);
#33162=EDGE_CURVE('',#26497,#26498,#12290,.T.);
#33163=EDGE_CURVE('',#26498,#26496,#12291,.T.);
#33164=EDGE_CURVE('',#26492,#26497,#12292,.T.);
#33165=EDGE_CURVE('',#26494,#26498,#12293,.T.);
#33166=EDGE_CURVE('',#26499,#26500,#12294,.T.);
#33167=EDGE_CURVE('',#26499,#26501,#12295,.T.);
#33168=EDGE_CURVE('',#26501,#26502,#12296,.T.);
#33169=EDGE_CURVE('',#26500,#26502,#12297,.T.);
#33170=EDGE_CURVE('',#26503,#26499,#12298,.T.);
#33171=EDGE_CURVE('',#26503,#26504,#12299,.T.);
#33172=EDGE_CURVE('',#26504,#26501,#12300,.T.);
#33173=EDGE_CURVE('',#26505,#26503,#12301,.T.);
#33174=EDGE_CURVE('',#26505,#26506,#12302,.T.);
#33175=EDGE_CURVE('',#26506,#26504,#12303,.T.);
#33176=EDGE_CURVE('',#26500,#26505,#12304,.T.);
#33177=EDGE_CURVE('',#26502,#26506,#12305,.T.);
#33178=EDGE_CURVE('',#26507,#26508,#12306,.T.);
#33179=EDGE_CURVE('',#26507,#26509,#12307,.T.);
#33180=EDGE_CURVE('',#26509,#26510,#12308,.T.);
#33181=EDGE_CURVE('',#26508,#26510,#12309,.T.);
#33182=EDGE_CURVE('',#26511,#26507,#12310,.T.);
#33183=EDGE_CURVE('',#26511,#26512,#12311,.T.);
#33184=EDGE_CURVE('',#26512,#26509,#12312,.T.);
#33185=EDGE_CURVE('',#26513,#26511,#12313,.T.);
#33186=EDGE_CURVE('',#26513,#26514,#12314,.T.);
#33187=EDGE_CURVE('',#26514,#26512,#12315,.T.);
#33188=EDGE_CURVE('',#26508,#26513,#12316,.T.);
#33189=EDGE_CURVE('',#26510,#26514,#12317,.T.);
#33190=EDGE_CURVE('',#26515,#26516,#12318,.T.);
#33191=EDGE_CURVE('',#26515,#26517,#12319,.T.);
#33192=EDGE_CURVE('',#26517,#26518,#12320,.T.);
#33193=EDGE_CURVE('',#26516,#26518,#12321,.T.);
#33194=EDGE_CURVE('',#26519,#26515,#12322,.T.);
#33195=EDGE_CURVE('',#26519,#26520,#12323,.T.);
#33196=EDGE_CURVE('',#26520,#26517,#12324,.T.);
#33197=EDGE_CURVE('',#26521,#26519,#12325,.T.);
#33198=EDGE_CURVE('',#26521,#26522,#12326,.T.);
#33199=EDGE_CURVE('',#26522,#26520,#12327,.T.);
#33200=EDGE_CURVE('',#26516,#26521,#12328,.T.);
#33201=EDGE_CURVE('',#26518,#26522,#12329,.T.);
#33202=EDGE_CURVE('',#26523,#26524,#12330,.T.);
#33203=EDGE_CURVE('',#26523,#26525,#12331,.T.);
#33204=EDGE_CURVE('',#26525,#26526,#12332,.T.);
#33205=EDGE_CURVE('',#26524,#26526,#12333,.T.);
#33206=EDGE_CURVE('',#26527,#26523,#12334,.T.);
#33207=EDGE_CURVE('',#26527,#26528,#12335,.T.);
#33208=EDGE_CURVE('',#26528,#26525,#12336,.T.);
#33209=EDGE_CURVE('',#26529,#26527,#12337,.T.);
#33210=EDGE_CURVE('',#26529,#26530,#12338,.T.);
#33211=EDGE_CURVE('',#26530,#26528,#12339,.T.);
#33212=EDGE_CURVE('',#26524,#26529,#12340,.T.);
#33213=EDGE_CURVE('',#26526,#26530,#12341,.T.);
#33214=EDGE_CURVE('',#26531,#26532,#12342,.T.);
#33215=EDGE_CURVE('',#26531,#26533,#12343,.T.);
#33216=EDGE_CURVE('',#26533,#26534,#12344,.T.);
#33217=EDGE_CURVE('',#26532,#26534,#12345,.T.);
#33218=EDGE_CURVE('',#26535,#26531,#12346,.T.);
#33219=EDGE_CURVE('',#26535,#26536,#12347,.T.);
#33220=EDGE_CURVE('',#26536,#26533,#12348,.T.);
#33221=EDGE_CURVE('',#26537,#26535,#12349,.T.);
#33222=EDGE_CURVE('',#26537,#26538,#12350,.T.);
#33223=EDGE_CURVE('',#26538,#26536,#12351,.T.);
#33224=EDGE_CURVE('',#26532,#26537,#12352,.T.);
#33225=EDGE_CURVE('',#26534,#26538,#12353,.T.);
#33226=EDGE_CURVE('',#26539,#26540,#12354,.T.);
#33227=EDGE_CURVE('',#26539,#26541,#12355,.T.);
#33228=EDGE_CURVE('',#26541,#26542,#12356,.T.);
#33229=EDGE_CURVE('',#26540,#26542,#12357,.T.);
#33230=EDGE_CURVE('',#26543,#26539,#12358,.T.);
#33231=EDGE_CURVE('',#26543,#26544,#12359,.T.);
#33232=EDGE_CURVE('',#26544,#26541,#12360,.T.);
#33233=EDGE_CURVE('',#26545,#26543,#12361,.T.);
#33234=EDGE_CURVE('',#26545,#26546,#12362,.T.);
#33235=EDGE_CURVE('',#26546,#26544,#12363,.T.);
#33236=EDGE_CURVE('',#26540,#26545,#12364,.T.);
#33237=EDGE_CURVE('',#26542,#26546,#12365,.T.);
#33238=EDGE_CURVE('',#26547,#26548,#12366,.T.);
#33239=EDGE_CURVE('',#26547,#26549,#12367,.T.);
#33240=EDGE_CURVE('',#26549,#26550,#12368,.T.);
#33241=EDGE_CURVE('',#26548,#26550,#12369,.T.);
#33242=EDGE_CURVE('',#26551,#26547,#12370,.T.);
#33243=EDGE_CURVE('',#26551,#26552,#12371,.T.);
#33244=EDGE_CURVE('',#26552,#26549,#12372,.T.);
#33245=EDGE_CURVE('',#26553,#26551,#12373,.T.);
#33246=EDGE_CURVE('',#26553,#26554,#12374,.T.);
#33247=EDGE_CURVE('',#26554,#26552,#12375,.T.);
#33248=EDGE_CURVE('',#26548,#26553,#12376,.T.);
#33249=EDGE_CURVE('',#26550,#26554,#12377,.T.);
#33250=EDGE_CURVE('',#26555,#26556,#12378,.T.);
#33251=EDGE_CURVE('',#26555,#26557,#12379,.T.);
#33252=EDGE_CURVE('',#26557,#26558,#12380,.T.);
#33253=EDGE_CURVE('',#26556,#26558,#12381,.T.);
#33254=EDGE_CURVE('',#26559,#26555,#12382,.T.);
#33255=EDGE_CURVE('',#26559,#26560,#12383,.T.);
#33256=EDGE_CURVE('',#26560,#26557,#12384,.T.);
#33257=EDGE_CURVE('',#26561,#26559,#12385,.T.);
#33258=EDGE_CURVE('',#26561,#26562,#12386,.T.);
#33259=EDGE_CURVE('',#26562,#26560,#12387,.T.);
#33260=EDGE_CURVE('',#26556,#26561,#12388,.T.);
#33261=EDGE_CURVE('',#26558,#26562,#12389,.T.);
#33262=EDGE_CURVE('',#26563,#26564,#12390,.T.);
#33263=EDGE_CURVE('',#26563,#26565,#12391,.T.);
#33264=EDGE_CURVE('',#26565,#26566,#12392,.T.);
#33265=EDGE_CURVE('',#26564,#26566,#12393,.T.);
#33266=EDGE_CURVE('',#26567,#26563,#12394,.T.);
#33267=EDGE_CURVE('',#26567,#26568,#12395,.T.);
#33268=EDGE_CURVE('',#26568,#26565,#12396,.T.);
#33269=EDGE_CURVE('',#26569,#26567,#12397,.T.);
#33270=EDGE_CURVE('',#26569,#26570,#12398,.T.);
#33271=EDGE_CURVE('',#26570,#26568,#12399,.T.);
#33272=EDGE_CURVE('',#26564,#26569,#12400,.T.);
#33273=EDGE_CURVE('',#26566,#26570,#12401,.T.);
#33274=EDGE_CURVE('',#26571,#26572,#12402,.T.);
#33275=EDGE_CURVE('',#26571,#26573,#12403,.T.);
#33276=EDGE_CURVE('',#26573,#26574,#12404,.T.);
#33277=EDGE_CURVE('',#26572,#26574,#12405,.T.);
#33278=EDGE_CURVE('',#26575,#26571,#12406,.T.);
#33279=EDGE_CURVE('',#26575,#26576,#12407,.T.);
#33280=EDGE_CURVE('',#26576,#26573,#12408,.T.);
#33281=EDGE_CURVE('',#26577,#26575,#12409,.T.);
#33282=EDGE_CURVE('',#26577,#26578,#12410,.T.);
#33283=EDGE_CURVE('',#26578,#26576,#12411,.T.);
#33284=EDGE_CURVE('',#26572,#26577,#12412,.T.);
#33285=EDGE_CURVE('',#26574,#26578,#12413,.T.);
#33286=EDGE_CURVE('',#26579,#26580,#12414,.T.);
#33287=EDGE_CURVE('',#26579,#26581,#12415,.T.);
#33288=EDGE_CURVE('',#26581,#26582,#12416,.T.);
#33289=EDGE_CURVE('',#26580,#26582,#12417,.T.);
#33290=EDGE_CURVE('',#26583,#26579,#12418,.T.);
#33291=EDGE_CURVE('',#26583,#26584,#12419,.T.);
#33292=EDGE_CURVE('',#26584,#26581,#12420,.T.);
#33293=EDGE_CURVE('',#26585,#26583,#12421,.T.);
#33294=EDGE_CURVE('',#26585,#26586,#12422,.T.);
#33295=EDGE_CURVE('',#26586,#26584,#12423,.T.);
#33296=EDGE_CURVE('',#26580,#26585,#12424,.T.);
#33297=EDGE_CURVE('',#26582,#26586,#12425,.T.);
#33298=EDGE_CURVE('',#26587,#26588,#12426,.T.);
#33299=EDGE_CURVE('',#26587,#26589,#12427,.T.);
#33300=EDGE_CURVE('',#26589,#26590,#12428,.T.);
#33301=EDGE_CURVE('',#26588,#26590,#12429,.T.);
#33302=EDGE_CURVE('',#26591,#26587,#12430,.T.);
#33303=EDGE_CURVE('',#26591,#26592,#12431,.T.);
#33304=EDGE_CURVE('',#26592,#26589,#12432,.T.);
#33305=EDGE_CURVE('',#26593,#26591,#12433,.T.);
#33306=EDGE_CURVE('',#26593,#26594,#12434,.T.);
#33307=EDGE_CURVE('',#26594,#26592,#12435,.T.);
#33308=EDGE_CURVE('',#26588,#26593,#12436,.T.);
#33309=EDGE_CURVE('',#26590,#26594,#12437,.T.);
#33310=EDGE_CURVE('',#26595,#26596,#12438,.T.);
#33311=EDGE_CURVE('',#26595,#26597,#12439,.T.);
#33312=EDGE_CURVE('',#26597,#26598,#12440,.T.);
#33313=EDGE_CURVE('',#26596,#26598,#12441,.T.);
#33314=EDGE_CURVE('',#26599,#26595,#12442,.T.);
#33315=EDGE_CURVE('',#26599,#26600,#12443,.T.);
#33316=EDGE_CURVE('',#26600,#26597,#12444,.T.);
#33317=EDGE_CURVE('',#26601,#26599,#12445,.T.);
#33318=EDGE_CURVE('',#26601,#26602,#12446,.T.);
#33319=EDGE_CURVE('',#26602,#26600,#12447,.T.);
#33320=EDGE_CURVE('',#26596,#26601,#12448,.T.);
#33321=EDGE_CURVE('',#26598,#26602,#12449,.T.);
#33322=EDGE_CURVE('',#26603,#26604,#12450,.T.);
#33323=EDGE_CURVE('',#26603,#26605,#12451,.T.);
#33324=EDGE_CURVE('',#26605,#26606,#12452,.T.);
#33325=EDGE_CURVE('',#26604,#26606,#12453,.T.);
#33326=EDGE_CURVE('',#26607,#26603,#12454,.T.);
#33327=EDGE_CURVE('',#26607,#26608,#12455,.T.);
#33328=EDGE_CURVE('',#26608,#26605,#12456,.T.);
#33329=EDGE_CURVE('',#26609,#26607,#12457,.T.);
#33330=EDGE_CURVE('',#26609,#26610,#12458,.T.);
#33331=EDGE_CURVE('',#26610,#26608,#12459,.T.);
#33332=EDGE_CURVE('',#26604,#26609,#12460,.T.);
#33333=EDGE_CURVE('',#26606,#26610,#12461,.T.);
#33334=EDGE_CURVE('',#26611,#26612,#12462,.T.);
#33335=EDGE_CURVE('',#26611,#26613,#12463,.T.);
#33336=EDGE_CURVE('',#26613,#26614,#12464,.T.);
#33337=EDGE_CURVE('',#26612,#26614,#12465,.T.);
#33338=EDGE_CURVE('',#26615,#26611,#12466,.T.);
#33339=EDGE_CURVE('',#26615,#26616,#12467,.T.);
#33340=EDGE_CURVE('',#26616,#26613,#12468,.T.);
#33341=EDGE_CURVE('',#26617,#26615,#12469,.T.);
#33342=EDGE_CURVE('',#26617,#26618,#12470,.T.);
#33343=EDGE_CURVE('',#26618,#26616,#12471,.T.);
#33344=EDGE_CURVE('',#26612,#26617,#12472,.T.);
#33345=EDGE_CURVE('',#26614,#26618,#12473,.T.);
#33346=EDGE_CURVE('',#26619,#26620,#12474,.T.);
#33347=EDGE_CURVE('',#26619,#26621,#12475,.T.);
#33348=EDGE_CURVE('',#26621,#26622,#12476,.T.);
#33349=EDGE_CURVE('',#26620,#26622,#12477,.T.);
#33350=EDGE_CURVE('',#26623,#26619,#12478,.T.);
#33351=EDGE_CURVE('',#26623,#26624,#12479,.T.);
#33352=EDGE_CURVE('',#26624,#26621,#12480,.T.);
#33353=EDGE_CURVE('',#26625,#26623,#12481,.T.);
#33354=EDGE_CURVE('',#26625,#26626,#12482,.T.);
#33355=EDGE_CURVE('',#26626,#26624,#12483,.T.);
#33356=EDGE_CURVE('',#26620,#26625,#12484,.T.);
#33357=EDGE_CURVE('',#26622,#26626,#12485,.T.);
#33358=EDGE_CURVE('',#26627,#26628,#12486,.T.);
#33359=EDGE_CURVE('',#26627,#26629,#12487,.T.);
#33360=EDGE_CURVE('',#26629,#26630,#12488,.T.);
#33361=EDGE_CURVE('',#26628,#26630,#12489,.T.);
#33362=EDGE_CURVE('',#26631,#26627,#12490,.T.);
#33363=EDGE_CURVE('',#26631,#26632,#12491,.T.);
#33364=EDGE_CURVE('',#26632,#26629,#12492,.T.);
#33365=EDGE_CURVE('',#26633,#26631,#12493,.T.);
#33366=EDGE_CURVE('',#26633,#26634,#12494,.T.);
#33367=EDGE_CURVE('',#26634,#26632,#12495,.T.);
#33368=EDGE_CURVE('',#26628,#26633,#12496,.T.);
#33369=EDGE_CURVE('',#26630,#26634,#12497,.T.);
#33370=EDGE_CURVE('',#26635,#26636,#12498,.T.);
#33371=EDGE_CURVE('',#26635,#26637,#12499,.T.);
#33372=EDGE_CURVE('',#26637,#26638,#12500,.T.);
#33373=EDGE_CURVE('',#26636,#26638,#12501,.T.);
#33374=EDGE_CURVE('',#26639,#26635,#12502,.T.);
#33375=EDGE_CURVE('',#26639,#26640,#12503,.T.);
#33376=EDGE_CURVE('',#26640,#26637,#12504,.T.);
#33377=EDGE_CURVE('',#26641,#26639,#12505,.T.);
#33378=EDGE_CURVE('',#26641,#26642,#12506,.T.);
#33379=EDGE_CURVE('',#26642,#26640,#12507,.T.);
#33380=EDGE_CURVE('',#26636,#26641,#12508,.T.);
#33381=EDGE_CURVE('',#26638,#26642,#12509,.T.);
#33382=EDGE_CURVE('',#26643,#26644,#12510,.T.);
#33383=EDGE_CURVE('',#26643,#26645,#12511,.T.);
#33384=EDGE_CURVE('',#26645,#26646,#12512,.T.);
#33385=EDGE_CURVE('',#26644,#26646,#12513,.T.);
#33386=EDGE_CURVE('',#26647,#26643,#12514,.T.);
#33387=EDGE_CURVE('',#26647,#26648,#12515,.T.);
#33388=EDGE_CURVE('',#26648,#26645,#12516,.T.);
#33389=EDGE_CURVE('',#26649,#26647,#12517,.T.);
#33390=EDGE_CURVE('',#26649,#26650,#12518,.T.);
#33391=EDGE_CURVE('',#26650,#26648,#12519,.T.);
#33392=EDGE_CURVE('',#26644,#26649,#12520,.T.);
#33393=EDGE_CURVE('',#26646,#26650,#12521,.T.);
#33394=EDGE_CURVE('',#26651,#26652,#12522,.T.);
#33395=EDGE_CURVE('',#26651,#26653,#12523,.T.);
#33396=EDGE_CURVE('',#26653,#26654,#12524,.T.);
#33397=EDGE_CURVE('',#26652,#26654,#12525,.T.);
#33398=EDGE_CURVE('',#26655,#26651,#12526,.T.);
#33399=EDGE_CURVE('',#26655,#26656,#12527,.T.);
#33400=EDGE_CURVE('',#26656,#26653,#12528,.T.);
#33401=EDGE_CURVE('',#26657,#26655,#12529,.T.);
#33402=EDGE_CURVE('',#26657,#26658,#12530,.T.);
#33403=EDGE_CURVE('',#26658,#26656,#12531,.T.);
#33404=EDGE_CURVE('',#26652,#26657,#12532,.T.);
#33405=EDGE_CURVE('',#26654,#26658,#12533,.T.);
#33406=EDGE_CURVE('',#26659,#26660,#12534,.T.);
#33407=EDGE_CURVE('',#26659,#26661,#12535,.T.);
#33408=EDGE_CURVE('',#26661,#26662,#12536,.T.);
#33409=EDGE_CURVE('',#26660,#26662,#12537,.T.);
#33410=EDGE_CURVE('',#26663,#26659,#12538,.T.);
#33411=EDGE_CURVE('',#26663,#26664,#12539,.T.);
#33412=EDGE_CURVE('',#26664,#26661,#12540,.T.);
#33413=EDGE_CURVE('',#26665,#26663,#12541,.T.);
#33414=EDGE_CURVE('',#26665,#26666,#12542,.T.);
#33415=EDGE_CURVE('',#26666,#26664,#12543,.T.);
#33416=EDGE_CURVE('',#26660,#26665,#12544,.T.);
#33417=EDGE_CURVE('',#26662,#26666,#12545,.T.);
#33418=EDGE_CURVE('',#26667,#26668,#12546,.T.);
#33419=EDGE_CURVE('',#26667,#26669,#12547,.T.);
#33420=EDGE_CURVE('',#26669,#26670,#12548,.T.);
#33421=EDGE_CURVE('',#26668,#26670,#12549,.T.);
#33422=EDGE_CURVE('',#26671,#26667,#12550,.T.);
#33423=EDGE_CURVE('',#26671,#26672,#12551,.T.);
#33424=EDGE_CURVE('',#26672,#26669,#12552,.T.);
#33425=EDGE_CURVE('',#26673,#26671,#12553,.T.);
#33426=EDGE_CURVE('',#26673,#26674,#12554,.T.);
#33427=EDGE_CURVE('',#26674,#26672,#12555,.T.);
#33428=EDGE_CURVE('',#26668,#26673,#12556,.T.);
#33429=EDGE_CURVE('',#26670,#26674,#12557,.T.);
#33430=EDGE_CURVE('',#26675,#26676,#12558,.T.);
#33431=EDGE_CURVE('',#26675,#26677,#12559,.T.);
#33432=EDGE_CURVE('',#26677,#26678,#12560,.T.);
#33433=EDGE_CURVE('',#26676,#26678,#12561,.T.);
#33434=EDGE_CURVE('',#26679,#26675,#12562,.T.);
#33435=EDGE_CURVE('',#26679,#26680,#12563,.T.);
#33436=EDGE_CURVE('',#26680,#26677,#12564,.T.);
#33437=EDGE_CURVE('',#26681,#26679,#12565,.T.);
#33438=EDGE_CURVE('',#26681,#26682,#12566,.T.);
#33439=EDGE_CURVE('',#26682,#26680,#12567,.T.);
#33440=EDGE_CURVE('',#26676,#26681,#12568,.T.);
#33441=EDGE_CURVE('',#26678,#26682,#12569,.T.);
#33442=EDGE_CURVE('',#26683,#26684,#12570,.T.);
#33443=EDGE_CURVE('',#26683,#26685,#12571,.T.);
#33444=EDGE_CURVE('',#26685,#26686,#12572,.T.);
#33445=EDGE_CURVE('',#26684,#26686,#12573,.T.);
#33446=EDGE_CURVE('',#26687,#26683,#12574,.T.);
#33447=EDGE_CURVE('',#26687,#26688,#12575,.T.);
#33448=EDGE_CURVE('',#26688,#26685,#12576,.T.);
#33449=EDGE_CURVE('',#26689,#26687,#12577,.T.);
#33450=EDGE_CURVE('',#26689,#26690,#12578,.T.);
#33451=EDGE_CURVE('',#26690,#26688,#12579,.T.);
#33452=EDGE_CURVE('',#26684,#26689,#12580,.T.);
#33453=EDGE_CURVE('',#26686,#26690,#12581,.T.);
#33454=EDGE_CURVE('',#26691,#26692,#12582,.T.);
#33455=EDGE_CURVE('',#26691,#26693,#12583,.T.);
#33456=EDGE_CURVE('',#26693,#26694,#12584,.T.);
#33457=EDGE_CURVE('',#26692,#26694,#12585,.T.);
#33458=EDGE_CURVE('',#26695,#26691,#12586,.T.);
#33459=EDGE_CURVE('',#26695,#26696,#12587,.T.);
#33460=EDGE_CURVE('',#26696,#26693,#12588,.T.);
#33461=EDGE_CURVE('',#26697,#26695,#12589,.T.);
#33462=EDGE_CURVE('',#26697,#26698,#12590,.T.);
#33463=EDGE_CURVE('',#26698,#26696,#12591,.T.);
#33464=EDGE_CURVE('',#26692,#26697,#12592,.T.);
#33465=EDGE_CURVE('',#26694,#26698,#12593,.T.);
#33466=EDGE_CURVE('',#26699,#26700,#12594,.T.);
#33467=EDGE_CURVE('',#26699,#26701,#12595,.T.);
#33468=EDGE_CURVE('',#26701,#26702,#12596,.T.);
#33469=EDGE_CURVE('',#26700,#26702,#12597,.T.);
#33470=EDGE_CURVE('',#26703,#26699,#12598,.T.);
#33471=EDGE_CURVE('',#26703,#26704,#12599,.T.);
#33472=EDGE_CURVE('',#26704,#26701,#12600,.T.);
#33473=EDGE_CURVE('',#26705,#26703,#12601,.T.);
#33474=EDGE_CURVE('',#26705,#26706,#12602,.T.);
#33475=EDGE_CURVE('',#26706,#26704,#12603,.T.);
#33476=EDGE_CURVE('',#26700,#26705,#12604,.T.);
#33477=EDGE_CURVE('',#26702,#26706,#12605,.T.);
#33478=EDGE_CURVE('',#26707,#26708,#12606,.T.);
#33479=EDGE_CURVE('',#26707,#26709,#12607,.T.);
#33480=EDGE_CURVE('',#26709,#26710,#12608,.T.);
#33481=EDGE_CURVE('',#26708,#26710,#12609,.T.);
#33482=EDGE_CURVE('',#26711,#26707,#12610,.T.);
#33483=EDGE_CURVE('',#26711,#26712,#12611,.T.);
#33484=EDGE_CURVE('',#26712,#26709,#12612,.T.);
#33485=EDGE_CURVE('',#26713,#26711,#12613,.T.);
#33486=EDGE_CURVE('',#26713,#26714,#12614,.T.);
#33487=EDGE_CURVE('',#26714,#26712,#12615,.T.);
#33488=EDGE_CURVE('',#26708,#26713,#12616,.T.);
#33489=EDGE_CURVE('',#26710,#26714,#12617,.T.);
#33490=EDGE_CURVE('',#26715,#26716,#12618,.T.);
#33491=EDGE_CURVE('',#26715,#26717,#12619,.T.);
#33492=EDGE_CURVE('',#26717,#26718,#12620,.T.);
#33493=EDGE_CURVE('',#26716,#26718,#12621,.T.);
#33494=EDGE_CURVE('',#26719,#26715,#12622,.T.);
#33495=EDGE_CURVE('',#26719,#26720,#12623,.T.);
#33496=EDGE_CURVE('',#26720,#26717,#12624,.T.);
#33497=EDGE_CURVE('',#26721,#26719,#12625,.T.);
#33498=EDGE_CURVE('',#26721,#26722,#12626,.T.);
#33499=EDGE_CURVE('',#26722,#26720,#12627,.T.);
#33500=EDGE_CURVE('',#26716,#26721,#12628,.T.);
#33501=EDGE_CURVE('',#26718,#26722,#12629,.T.);
#33502=EDGE_CURVE('',#26723,#26724,#12630,.T.);
#33503=EDGE_CURVE('',#26723,#26725,#12631,.T.);
#33504=EDGE_CURVE('',#26725,#26726,#12632,.T.);
#33505=EDGE_CURVE('',#26724,#26726,#12633,.T.);
#33506=EDGE_CURVE('',#26727,#26723,#12634,.T.);
#33507=EDGE_CURVE('',#26727,#26728,#12635,.T.);
#33508=EDGE_CURVE('',#26728,#26725,#12636,.T.);
#33509=EDGE_CURVE('',#26729,#26727,#12637,.T.);
#33510=EDGE_CURVE('',#26729,#26730,#12638,.T.);
#33511=EDGE_CURVE('',#26730,#26728,#12639,.T.);
#33512=EDGE_CURVE('',#26724,#26729,#12640,.T.);
#33513=EDGE_CURVE('',#26726,#26730,#12641,.T.);
#33514=EDGE_CURVE('',#26731,#26732,#12642,.T.);
#33515=EDGE_CURVE('',#26731,#26733,#12643,.T.);
#33516=EDGE_CURVE('',#26733,#26734,#12644,.T.);
#33517=EDGE_CURVE('',#26732,#26734,#12645,.T.);
#33518=EDGE_CURVE('',#26735,#26731,#12646,.T.);
#33519=EDGE_CURVE('',#26735,#26736,#12647,.T.);
#33520=EDGE_CURVE('',#26736,#26733,#12648,.T.);
#33521=EDGE_CURVE('',#26737,#26735,#12649,.T.);
#33522=EDGE_CURVE('',#26737,#26738,#12650,.T.);
#33523=EDGE_CURVE('',#26738,#26736,#12651,.T.);
#33524=EDGE_CURVE('',#26732,#26737,#12652,.T.);
#33525=EDGE_CURVE('',#26734,#26738,#12653,.T.);
#33526=EDGE_CURVE('',#26739,#26740,#12654,.T.);
#33527=EDGE_CURVE('',#26739,#26741,#12655,.T.);
#33528=EDGE_CURVE('',#26741,#26742,#12656,.T.);
#33529=EDGE_CURVE('',#26740,#26742,#12657,.T.);
#33530=EDGE_CURVE('',#26743,#26739,#12658,.T.);
#33531=EDGE_CURVE('',#26743,#26744,#12659,.T.);
#33532=EDGE_CURVE('',#26744,#26741,#12660,.T.);
#33533=EDGE_CURVE('',#26745,#26743,#12661,.T.);
#33534=EDGE_CURVE('',#26745,#26746,#12662,.T.);
#33535=EDGE_CURVE('',#26746,#26744,#12663,.T.);
#33536=EDGE_CURVE('',#26740,#26745,#12664,.T.);
#33537=EDGE_CURVE('',#26742,#26746,#12665,.T.);
#33538=EDGE_CURVE('',#26747,#26748,#12666,.T.);
#33539=EDGE_CURVE('',#26747,#26749,#12667,.T.);
#33540=EDGE_CURVE('',#26749,#26750,#12668,.T.);
#33541=EDGE_CURVE('',#26748,#26750,#12669,.T.);
#33542=EDGE_CURVE('',#26751,#26747,#12670,.T.);
#33543=EDGE_CURVE('',#26751,#26752,#12671,.T.);
#33544=EDGE_CURVE('',#26752,#26749,#12672,.T.);
#33545=EDGE_CURVE('',#26753,#26751,#12673,.T.);
#33546=EDGE_CURVE('',#26753,#26754,#12674,.T.);
#33547=EDGE_CURVE('',#26754,#26752,#12675,.T.);
#33548=EDGE_CURVE('',#26748,#26753,#12676,.T.);
#33549=EDGE_CURVE('',#26750,#26754,#12677,.T.);
#33550=EDGE_CURVE('',#26755,#26756,#12678,.T.);
#33551=EDGE_CURVE('',#26755,#26757,#12679,.T.);
#33552=EDGE_CURVE('',#26757,#26758,#12680,.T.);
#33553=EDGE_CURVE('',#26756,#26758,#12681,.T.);
#33554=EDGE_CURVE('',#26759,#26755,#12682,.T.);
#33555=EDGE_CURVE('',#26759,#26760,#12683,.T.);
#33556=EDGE_CURVE('',#26760,#26757,#12684,.T.);
#33557=EDGE_CURVE('',#26761,#26759,#12685,.T.);
#33558=EDGE_CURVE('',#26761,#26762,#12686,.T.);
#33559=EDGE_CURVE('',#26762,#26760,#12687,.T.);
#33560=EDGE_CURVE('',#26756,#26761,#12688,.T.);
#33561=EDGE_CURVE('',#26758,#26762,#12689,.T.);
#33562=EDGE_CURVE('',#26763,#26764,#12690,.T.);
#33563=EDGE_CURVE('',#26763,#26765,#12691,.T.);
#33564=EDGE_CURVE('',#26765,#26766,#12692,.T.);
#33565=EDGE_CURVE('',#26764,#26766,#12693,.T.);
#33566=EDGE_CURVE('',#26767,#26763,#12694,.T.);
#33567=EDGE_CURVE('',#26767,#26768,#12695,.T.);
#33568=EDGE_CURVE('',#26768,#26765,#12696,.T.);
#33569=EDGE_CURVE('',#26769,#26767,#12697,.T.);
#33570=EDGE_CURVE('',#26769,#26770,#12698,.T.);
#33571=EDGE_CURVE('',#26770,#26768,#12699,.T.);
#33572=EDGE_CURVE('',#26764,#26769,#12700,.T.);
#33573=EDGE_CURVE('',#26766,#26770,#12701,.T.);
#33574=EDGE_CURVE('',#26771,#26772,#12702,.T.);
#33575=EDGE_CURVE('',#26771,#26773,#12703,.T.);
#33576=EDGE_CURVE('',#26773,#26774,#12704,.T.);
#33577=EDGE_CURVE('',#26772,#26774,#12705,.T.);
#33578=EDGE_CURVE('',#26775,#26771,#12706,.T.);
#33579=EDGE_CURVE('',#26775,#26776,#12707,.T.);
#33580=EDGE_CURVE('',#26776,#26773,#12708,.T.);
#33581=EDGE_CURVE('',#26777,#26775,#12709,.T.);
#33582=EDGE_CURVE('',#26777,#26778,#12710,.T.);
#33583=EDGE_CURVE('',#26778,#26776,#12711,.T.);
#33584=EDGE_CURVE('',#26772,#26777,#12712,.T.);
#33585=EDGE_CURVE('',#26774,#26778,#12713,.T.);
#33586=EDGE_CURVE('',#26779,#26780,#12714,.T.);
#33587=EDGE_CURVE('',#26779,#26781,#12715,.T.);
#33588=EDGE_CURVE('',#26781,#26782,#12716,.T.);
#33589=EDGE_CURVE('',#26780,#26782,#12717,.T.);
#33590=EDGE_CURVE('',#26783,#26779,#12718,.T.);
#33591=EDGE_CURVE('',#26783,#26784,#12719,.T.);
#33592=EDGE_CURVE('',#26784,#26781,#12720,.T.);
#33593=EDGE_CURVE('',#26785,#26783,#12721,.T.);
#33594=EDGE_CURVE('',#26785,#26786,#12722,.T.);
#33595=EDGE_CURVE('',#26786,#26784,#12723,.T.);
#33596=EDGE_CURVE('',#26780,#26785,#12724,.T.);
#33597=EDGE_CURVE('',#26782,#26786,#12725,.T.);
#33598=EDGE_CURVE('',#26787,#26788,#12726,.T.);
#33599=EDGE_CURVE('',#26787,#26789,#12727,.T.);
#33600=EDGE_CURVE('',#26789,#26790,#12728,.T.);
#33601=EDGE_CURVE('',#26788,#26790,#12729,.T.);
#33602=EDGE_CURVE('',#26791,#26787,#12730,.T.);
#33603=EDGE_CURVE('',#26791,#26792,#12731,.T.);
#33604=EDGE_CURVE('',#26792,#26789,#12732,.T.);
#33605=EDGE_CURVE('',#26793,#26791,#12733,.T.);
#33606=EDGE_CURVE('',#26793,#26794,#12734,.T.);
#33607=EDGE_CURVE('',#26794,#26792,#12735,.T.);
#33608=EDGE_CURVE('',#26788,#26793,#12736,.T.);
#33609=EDGE_CURVE('',#26790,#26794,#12737,.T.);
#33610=EDGE_CURVE('',#26795,#26796,#12738,.T.);
#33611=EDGE_CURVE('',#26795,#26797,#12739,.T.);
#33612=EDGE_CURVE('',#26797,#26798,#12740,.T.);
#33613=EDGE_CURVE('',#26796,#26798,#12741,.T.);
#33614=EDGE_CURVE('',#26799,#26795,#12742,.T.);
#33615=EDGE_CURVE('',#26799,#26800,#12743,.T.);
#33616=EDGE_CURVE('',#26800,#26797,#12744,.T.);
#33617=EDGE_CURVE('',#26801,#26799,#12745,.T.);
#33618=EDGE_CURVE('',#26801,#26802,#12746,.T.);
#33619=EDGE_CURVE('',#26802,#26800,#12747,.T.);
#33620=EDGE_CURVE('',#26796,#26801,#12748,.T.);
#33621=EDGE_CURVE('',#26798,#26802,#12749,.T.);
#33622=EDGE_CURVE('',#26803,#26804,#12750,.T.);
#33623=EDGE_CURVE('',#26803,#26805,#12751,.T.);
#33624=EDGE_CURVE('',#26805,#26806,#12752,.T.);
#33625=EDGE_CURVE('',#26804,#26806,#12753,.T.);
#33626=EDGE_CURVE('',#26807,#26803,#12754,.T.);
#33627=EDGE_CURVE('',#26807,#26808,#12755,.T.);
#33628=EDGE_CURVE('',#26808,#26805,#12756,.T.);
#33629=EDGE_CURVE('',#26809,#26807,#12757,.T.);
#33630=EDGE_CURVE('',#26809,#26810,#12758,.T.);
#33631=EDGE_CURVE('',#26810,#26808,#12759,.T.);
#33632=EDGE_CURVE('',#26804,#26809,#12760,.T.);
#33633=EDGE_CURVE('',#26806,#26810,#12761,.T.);
#33634=EDGE_CURVE('',#26811,#26812,#12762,.T.);
#33635=EDGE_CURVE('',#26811,#26813,#12763,.T.);
#33636=EDGE_CURVE('',#26813,#26814,#12764,.T.);
#33637=EDGE_CURVE('',#26812,#26814,#12765,.T.);
#33638=EDGE_CURVE('',#26815,#26811,#12766,.T.);
#33639=EDGE_CURVE('',#26815,#26816,#12767,.T.);
#33640=EDGE_CURVE('',#26816,#26813,#12768,.T.);
#33641=EDGE_CURVE('',#26817,#26815,#12769,.T.);
#33642=EDGE_CURVE('',#26817,#26818,#12770,.T.);
#33643=EDGE_CURVE('',#26818,#26816,#12771,.T.);
#33644=EDGE_CURVE('',#26812,#26817,#12772,.T.);
#33645=EDGE_CURVE('',#26814,#26818,#12773,.T.);
#33646=EDGE_CURVE('',#26819,#26820,#12774,.T.);
#33647=EDGE_CURVE('',#26819,#26821,#12775,.T.);
#33648=EDGE_CURVE('',#26821,#26822,#12776,.T.);
#33649=EDGE_CURVE('',#26820,#26822,#12777,.T.);
#33650=EDGE_CURVE('',#26823,#26819,#12778,.T.);
#33651=EDGE_CURVE('',#26823,#26824,#12779,.T.);
#33652=EDGE_CURVE('',#26824,#26821,#12780,.T.);
#33653=EDGE_CURVE('',#26825,#26823,#12781,.T.);
#33654=EDGE_CURVE('',#26825,#26826,#12782,.T.);
#33655=EDGE_CURVE('',#26826,#26824,#12783,.T.);
#33656=EDGE_CURVE('',#26820,#26825,#12784,.T.);
#33657=EDGE_CURVE('',#26822,#26826,#12785,.T.);
#33658=EDGE_CURVE('',#26827,#26828,#12786,.T.);
#33659=EDGE_CURVE('',#26827,#26829,#12787,.T.);
#33660=EDGE_CURVE('',#26829,#26830,#12788,.T.);
#33661=EDGE_CURVE('',#26828,#26830,#12789,.T.);
#33662=EDGE_CURVE('',#26831,#26827,#12790,.T.);
#33663=EDGE_CURVE('',#26831,#26832,#12791,.T.);
#33664=EDGE_CURVE('',#26832,#26829,#12792,.T.);
#33665=EDGE_CURVE('',#26833,#26831,#12793,.T.);
#33666=EDGE_CURVE('',#26833,#26834,#12794,.T.);
#33667=EDGE_CURVE('',#26834,#26832,#12795,.T.);
#33668=EDGE_CURVE('',#26828,#26833,#12796,.T.);
#33669=EDGE_CURVE('',#26830,#26834,#12797,.T.);
#33670=EDGE_CURVE('',#26835,#26836,#12798,.T.);
#33671=EDGE_CURVE('',#26835,#26837,#12799,.T.);
#33672=EDGE_CURVE('',#26837,#26838,#12800,.T.);
#33673=EDGE_CURVE('',#26836,#26838,#12801,.T.);
#33674=EDGE_CURVE('',#26839,#26835,#12802,.T.);
#33675=EDGE_CURVE('',#26839,#26840,#12803,.T.);
#33676=EDGE_CURVE('',#26840,#26837,#12804,.T.);
#33677=EDGE_CURVE('',#26841,#26839,#12805,.T.);
#33678=EDGE_CURVE('',#26841,#26842,#12806,.T.);
#33679=EDGE_CURVE('',#26842,#26840,#12807,.T.);
#33680=EDGE_CURVE('',#26836,#26841,#12808,.T.);
#33681=EDGE_CURVE('',#26838,#26842,#12809,.T.);
#33682=EDGE_CURVE('',#26843,#26844,#12810,.T.);
#33683=EDGE_CURVE('',#26843,#26845,#12811,.T.);
#33684=EDGE_CURVE('',#26845,#26846,#12812,.T.);
#33685=EDGE_CURVE('',#26844,#26846,#12813,.T.);
#33686=EDGE_CURVE('',#26847,#26843,#12814,.T.);
#33687=EDGE_CURVE('',#26847,#26848,#12815,.T.);
#33688=EDGE_CURVE('',#26848,#26845,#12816,.T.);
#33689=EDGE_CURVE('',#26849,#26847,#12817,.T.);
#33690=EDGE_CURVE('',#26849,#26850,#12818,.T.);
#33691=EDGE_CURVE('',#26850,#26848,#12819,.T.);
#33692=EDGE_CURVE('',#26844,#26849,#12820,.T.);
#33693=EDGE_CURVE('',#26846,#26850,#12821,.T.);
#33694=EDGE_CURVE('',#26851,#26852,#12822,.T.);
#33695=EDGE_CURVE('',#26851,#26853,#12823,.T.);
#33696=EDGE_CURVE('',#26853,#26854,#12824,.T.);
#33697=EDGE_CURVE('',#26852,#26854,#12825,.T.);
#33698=EDGE_CURVE('',#26855,#26851,#12826,.T.);
#33699=EDGE_CURVE('',#26855,#26856,#12827,.T.);
#33700=EDGE_CURVE('',#26856,#26853,#12828,.T.);
#33701=EDGE_CURVE('',#26857,#26855,#12829,.T.);
#33702=EDGE_CURVE('',#26857,#26858,#12830,.T.);
#33703=EDGE_CURVE('',#26858,#26856,#12831,.T.);
#33704=EDGE_CURVE('',#26852,#26857,#12832,.T.);
#33705=EDGE_CURVE('',#26854,#26858,#12833,.T.);
#33706=EDGE_CURVE('',#26859,#26860,#12834,.T.);
#33707=EDGE_CURVE('',#26859,#26861,#12835,.T.);
#33708=EDGE_CURVE('',#26861,#26862,#12836,.T.);
#33709=EDGE_CURVE('',#26860,#26862,#12837,.T.);
#33710=EDGE_CURVE('',#26863,#26859,#12838,.T.);
#33711=EDGE_CURVE('',#26863,#26864,#12839,.T.);
#33712=EDGE_CURVE('',#26864,#26861,#12840,.T.);
#33713=EDGE_CURVE('',#26865,#26863,#12841,.T.);
#33714=EDGE_CURVE('',#26865,#26866,#12842,.T.);
#33715=EDGE_CURVE('',#26866,#26864,#12843,.T.);
#33716=EDGE_CURVE('',#26860,#26865,#12844,.T.);
#33717=EDGE_CURVE('',#26862,#26866,#12845,.T.);
#33718=EDGE_CURVE('',#26867,#26868,#12846,.T.);
#33719=EDGE_CURVE('',#26867,#26869,#12847,.T.);
#33720=EDGE_CURVE('',#26869,#26870,#12848,.T.);
#33721=EDGE_CURVE('',#26868,#26870,#12849,.T.);
#33722=EDGE_CURVE('',#26871,#26867,#12850,.T.);
#33723=EDGE_CURVE('',#26871,#26872,#12851,.T.);
#33724=EDGE_CURVE('',#26872,#26869,#12852,.T.);
#33725=EDGE_CURVE('',#26873,#26871,#12853,.T.);
#33726=EDGE_CURVE('',#26873,#26874,#12854,.T.);
#33727=EDGE_CURVE('',#26874,#26872,#12855,.T.);
#33728=EDGE_CURVE('',#26868,#26873,#12856,.T.);
#33729=EDGE_CURVE('',#26870,#26874,#12857,.T.);
#33730=EDGE_CURVE('',#26875,#26876,#12858,.T.);
#33731=EDGE_CURVE('',#26875,#26877,#12859,.T.);
#33732=EDGE_CURVE('',#26877,#26878,#12860,.T.);
#33733=EDGE_CURVE('',#26876,#26878,#12861,.T.);
#33734=EDGE_CURVE('',#26879,#26875,#12862,.T.);
#33735=EDGE_CURVE('',#26879,#26880,#12863,.T.);
#33736=EDGE_CURVE('',#26880,#26877,#12864,.T.);
#33737=EDGE_CURVE('',#26881,#26879,#12865,.T.);
#33738=EDGE_CURVE('',#26881,#26882,#12866,.T.);
#33739=EDGE_CURVE('',#26882,#26880,#12867,.T.);
#33740=EDGE_CURVE('',#26876,#26881,#12868,.T.);
#33741=EDGE_CURVE('',#26878,#26882,#12869,.T.);
#33742=EDGE_CURVE('',#26883,#26884,#12870,.T.);
#33743=EDGE_CURVE('',#26883,#26885,#12871,.T.);
#33744=EDGE_CURVE('',#26885,#26886,#12872,.T.);
#33745=EDGE_CURVE('',#26884,#26886,#12873,.T.);
#33746=EDGE_CURVE('',#26887,#26883,#12874,.T.);
#33747=EDGE_CURVE('',#26887,#26888,#12875,.T.);
#33748=EDGE_CURVE('',#26888,#26885,#12876,.T.);
#33749=EDGE_CURVE('',#26889,#26887,#12877,.T.);
#33750=EDGE_CURVE('',#26889,#26890,#12878,.T.);
#33751=EDGE_CURVE('',#26890,#26888,#12879,.T.);
#33752=EDGE_CURVE('',#26884,#26889,#12880,.T.);
#33753=EDGE_CURVE('',#26886,#26890,#12881,.T.);
#33754=EDGE_CURVE('',#26891,#26892,#12882,.T.);
#33755=EDGE_CURVE('',#26891,#26893,#12883,.T.);
#33756=EDGE_CURVE('',#26893,#26894,#12884,.T.);
#33757=EDGE_CURVE('',#26892,#26894,#12885,.T.);
#33758=EDGE_CURVE('',#26895,#26891,#12886,.T.);
#33759=EDGE_CURVE('',#26895,#26896,#12887,.T.);
#33760=EDGE_CURVE('',#26896,#26893,#12888,.T.);
#33761=EDGE_CURVE('',#26897,#26895,#12889,.T.);
#33762=EDGE_CURVE('',#26897,#26898,#12890,.T.);
#33763=EDGE_CURVE('',#26898,#26896,#12891,.T.);
#33764=EDGE_CURVE('',#26892,#26897,#12892,.T.);
#33765=EDGE_CURVE('',#26894,#26898,#12893,.T.);
#33766=EDGE_CURVE('',#26899,#26900,#12894,.T.);
#33767=EDGE_CURVE('',#26899,#26901,#12895,.T.);
#33768=EDGE_CURVE('',#26901,#26902,#12896,.T.);
#33769=EDGE_CURVE('',#26900,#26902,#12897,.T.);
#33770=EDGE_CURVE('',#26903,#26899,#12898,.T.);
#33771=EDGE_CURVE('',#26903,#26904,#12899,.T.);
#33772=EDGE_CURVE('',#26904,#26901,#12900,.T.);
#33773=EDGE_CURVE('',#26905,#26903,#12901,.T.);
#33774=EDGE_CURVE('',#26905,#26906,#12902,.T.);
#33775=EDGE_CURVE('',#26906,#26904,#12903,.T.);
#33776=EDGE_CURVE('',#26900,#26905,#12904,.T.);
#33777=EDGE_CURVE('',#26902,#26906,#12905,.T.);
#33778=EDGE_CURVE('',#26907,#26908,#12906,.T.);
#33779=EDGE_CURVE('',#26907,#26909,#12907,.T.);
#33780=EDGE_CURVE('',#26909,#26910,#12908,.T.);
#33781=EDGE_CURVE('',#26908,#26910,#12909,.T.);
#33782=EDGE_CURVE('',#26911,#26907,#12910,.T.);
#33783=EDGE_CURVE('',#26911,#26912,#12911,.T.);
#33784=EDGE_CURVE('',#26912,#26909,#12912,.T.);
#33785=EDGE_CURVE('',#26913,#26911,#12913,.T.);
#33786=EDGE_CURVE('',#26913,#26914,#12914,.T.);
#33787=EDGE_CURVE('',#26914,#26912,#12915,.T.);
#33788=EDGE_CURVE('',#26908,#26913,#12916,.T.);
#33789=EDGE_CURVE('',#26910,#26914,#12917,.T.);
#33790=EDGE_CURVE('',#26915,#26916,#12918,.T.);
#33791=EDGE_CURVE('',#26915,#26917,#12919,.T.);
#33792=EDGE_CURVE('',#26917,#26918,#12920,.T.);
#33793=EDGE_CURVE('',#26916,#26918,#12921,.T.);
#33794=EDGE_CURVE('',#26919,#26915,#12922,.T.);
#33795=EDGE_CURVE('',#26919,#26920,#12923,.T.);
#33796=EDGE_CURVE('',#26920,#26917,#12924,.T.);
#33797=EDGE_CURVE('',#26921,#26919,#12925,.T.);
#33798=EDGE_CURVE('',#26921,#26922,#12926,.T.);
#33799=EDGE_CURVE('',#26922,#26920,#12927,.T.);
#33800=EDGE_CURVE('',#26916,#26921,#12928,.T.);
#33801=EDGE_CURVE('',#26918,#26922,#12929,.T.);
#33802=EDGE_CURVE('',#26923,#26924,#12930,.T.);
#33803=EDGE_CURVE('',#26923,#26925,#12931,.T.);
#33804=EDGE_CURVE('',#26925,#26926,#12932,.T.);
#33805=EDGE_CURVE('',#26924,#26926,#12933,.T.);
#33806=EDGE_CURVE('',#26927,#26923,#12934,.T.);
#33807=EDGE_CURVE('',#26927,#26928,#12935,.T.);
#33808=EDGE_CURVE('',#26928,#26925,#12936,.T.);
#33809=EDGE_CURVE('',#26929,#26927,#12937,.T.);
#33810=EDGE_CURVE('',#26929,#26930,#12938,.T.);
#33811=EDGE_CURVE('',#26930,#26928,#12939,.T.);
#33812=EDGE_CURVE('',#26924,#26929,#12940,.T.);
#33813=EDGE_CURVE('',#26926,#26930,#12941,.T.);
#33814=EDGE_CURVE('',#26931,#26932,#12942,.T.);
#33815=EDGE_CURVE('',#26931,#26933,#12943,.T.);
#33816=EDGE_CURVE('',#26933,#26934,#12944,.T.);
#33817=EDGE_CURVE('',#26932,#26934,#12945,.T.);
#33818=EDGE_CURVE('',#26935,#26931,#12946,.T.);
#33819=EDGE_CURVE('',#26935,#26936,#12947,.T.);
#33820=EDGE_CURVE('',#26936,#26933,#12948,.T.);
#33821=EDGE_CURVE('',#26937,#26935,#12949,.T.);
#33822=EDGE_CURVE('',#26937,#26938,#12950,.T.);
#33823=EDGE_CURVE('',#26938,#26936,#12951,.T.);
#33824=EDGE_CURVE('',#26932,#26937,#12952,.T.);
#33825=EDGE_CURVE('',#26934,#26938,#12953,.T.);
#33826=EDGE_CURVE('',#26939,#26940,#12954,.T.);
#33827=EDGE_CURVE('',#26939,#26941,#12955,.T.);
#33828=EDGE_CURVE('',#26941,#26942,#12956,.T.);
#33829=EDGE_CURVE('',#26940,#26942,#12957,.T.);
#33830=EDGE_CURVE('',#26943,#26939,#12958,.T.);
#33831=EDGE_CURVE('',#26943,#26944,#12959,.T.);
#33832=EDGE_CURVE('',#26944,#26941,#12960,.T.);
#33833=EDGE_CURVE('',#26945,#26943,#12961,.T.);
#33834=EDGE_CURVE('',#26945,#26946,#12962,.T.);
#33835=EDGE_CURVE('',#26946,#26944,#12963,.T.);
#33836=EDGE_CURVE('',#26940,#26945,#12964,.T.);
#33837=EDGE_CURVE('',#26942,#26946,#12965,.T.);
#33838=EDGE_CURVE('',#26947,#26948,#12966,.T.);
#33839=EDGE_CURVE('',#26947,#26949,#12967,.T.);
#33840=EDGE_CURVE('',#26949,#26950,#12968,.T.);
#33841=EDGE_CURVE('',#26948,#26950,#12969,.T.);
#33842=EDGE_CURVE('',#26951,#26947,#12970,.T.);
#33843=EDGE_CURVE('',#26951,#26952,#12971,.T.);
#33844=EDGE_CURVE('',#26952,#26949,#12972,.T.);
#33845=EDGE_CURVE('',#26953,#26951,#12973,.T.);
#33846=EDGE_CURVE('',#26953,#26954,#12974,.T.);
#33847=EDGE_CURVE('',#26954,#26952,#12975,.T.);
#33848=EDGE_CURVE('',#26948,#26953,#12976,.T.);
#33849=EDGE_CURVE('',#26950,#26954,#12977,.T.);
#33850=EDGE_CURVE('',#26955,#26956,#12978,.T.);
#33851=EDGE_CURVE('',#26955,#26957,#12979,.T.);
#33852=EDGE_CURVE('',#26957,#26958,#12980,.T.);
#33853=EDGE_CURVE('',#26956,#26958,#12981,.T.);
#33854=EDGE_CURVE('',#26959,#26955,#12982,.T.);
#33855=EDGE_CURVE('',#26959,#26960,#12983,.T.);
#33856=EDGE_CURVE('',#26960,#26957,#12984,.T.);
#33857=EDGE_CURVE('',#26961,#26959,#12985,.T.);
#33858=EDGE_CURVE('',#26961,#26962,#12986,.T.);
#33859=EDGE_CURVE('',#26962,#26960,#12987,.T.);
#33860=EDGE_CURVE('',#26956,#26961,#12988,.T.);
#33861=EDGE_CURVE('',#26958,#26962,#12989,.T.);
#33862=EDGE_CURVE('',#26963,#26964,#12990,.T.);
#33863=EDGE_CURVE('',#26963,#26965,#12991,.T.);
#33864=EDGE_CURVE('',#26965,#26966,#12992,.T.);
#33865=EDGE_CURVE('',#26964,#26966,#12993,.T.);
#33866=EDGE_CURVE('',#26967,#26963,#12994,.T.);
#33867=EDGE_CURVE('',#26967,#26968,#12995,.T.);
#33868=EDGE_CURVE('',#26968,#26965,#12996,.T.);
#33869=EDGE_CURVE('',#26969,#26967,#12997,.T.);
#33870=EDGE_CURVE('',#26969,#26970,#12998,.T.);
#33871=EDGE_CURVE('',#26970,#26968,#12999,.T.);
#33872=EDGE_CURVE('',#26964,#26969,#13000,.T.);
#33873=EDGE_CURVE('',#26966,#26970,#13001,.T.);
#33874=EDGE_CURVE('',#26971,#26972,#13002,.T.);
#33875=EDGE_CURVE('',#26971,#26973,#13003,.T.);
#33876=EDGE_CURVE('',#26973,#26974,#13004,.T.);
#33877=EDGE_CURVE('',#26972,#26974,#13005,.T.);
#33878=EDGE_CURVE('',#26975,#26971,#13006,.T.);
#33879=EDGE_CURVE('',#26975,#26976,#13007,.T.);
#33880=EDGE_CURVE('',#26976,#26973,#13008,.T.);
#33881=EDGE_CURVE('',#26977,#26975,#13009,.T.);
#33882=EDGE_CURVE('',#26977,#26978,#13010,.T.);
#33883=EDGE_CURVE('',#26978,#26976,#13011,.T.);
#33884=EDGE_CURVE('',#26972,#26977,#13012,.T.);
#33885=EDGE_CURVE('',#26974,#26978,#13013,.T.);
#33886=EDGE_CURVE('',#26979,#26980,#13014,.T.);
#33887=EDGE_CURVE('',#26979,#26981,#13015,.T.);
#33888=EDGE_CURVE('',#26981,#26982,#13016,.T.);
#33889=EDGE_CURVE('',#26980,#26982,#13017,.T.);
#33890=EDGE_CURVE('',#26983,#26979,#13018,.T.);
#33891=EDGE_CURVE('',#26983,#26984,#13019,.T.);
#33892=EDGE_CURVE('',#26984,#26981,#13020,.T.);
#33893=EDGE_CURVE('',#26985,#26983,#13021,.T.);
#33894=EDGE_CURVE('',#26985,#26986,#13022,.T.);
#33895=EDGE_CURVE('',#26986,#26984,#13023,.T.);
#33896=EDGE_CURVE('',#26980,#26985,#13024,.T.);
#33897=EDGE_CURVE('',#26982,#26986,#13025,.T.);
#33898=EDGE_CURVE('',#26987,#26988,#13026,.T.);
#33899=EDGE_CURVE('',#26987,#26989,#13027,.T.);
#33900=EDGE_CURVE('',#26989,#26990,#13028,.T.);
#33901=EDGE_CURVE('',#26988,#26990,#13029,.T.);
#33902=EDGE_CURVE('',#26991,#26987,#13030,.T.);
#33903=EDGE_CURVE('',#26991,#26992,#13031,.T.);
#33904=EDGE_CURVE('',#26992,#26989,#13032,.T.);
#33905=EDGE_CURVE('',#26993,#26991,#13033,.T.);
#33906=EDGE_CURVE('',#26993,#26994,#13034,.T.);
#33907=EDGE_CURVE('',#26994,#26992,#13035,.T.);
#33908=EDGE_CURVE('',#26988,#26993,#13036,.T.);
#33909=EDGE_CURVE('',#26990,#26994,#13037,.T.);
#33910=EDGE_CURVE('',#26995,#26996,#13038,.T.);
#33911=EDGE_CURVE('',#26995,#26997,#13039,.T.);
#33912=EDGE_CURVE('',#26997,#26998,#13040,.T.);
#33913=EDGE_CURVE('',#26996,#26998,#13041,.T.);
#33914=EDGE_CURVE('',#26999,#26995,#13042,.T.);
#33915=EDGE_CURVE('',#26999,#27000,#13043,.T.);
#33916=EDGE_CURVE('',#27000,#26997,#13044,.T.);
#33917=EDGE_CURVE('',#27001,#26999,#13045,.T.);
#33918=EDGE_CURVE('',#27001,#27002,#13046,.T.);
#33919=EDGE_CURVE('',#27002,#27000,#13047,.T.);
#33920=EDGE_CURVE('',#26996,#27001,#13048,.T.);
#33921=EDGE_CURVE('',#26998,#27002,#13049,.T.);
#33922=EDGE_CURVE('',#27003,#27004,#13050,.T.);
#33923=EDGE_CURVE('',#27003,#27005,#13051,.T.);
#33924=EDGE_CURVE('',#27005,#27006,#13052,.T.);
#33925=EDGE_CURVE('',#27004,#27006,#13053,.T.);
#33926=EDGE_CURVE('',#27007,#27003,#13054,.T.);
#33927=EDGE_CURVE('',#27007,#27008,#13055,.T.);
#33928=EDGE_CURVE('',#27008,#27005,#13056,.T.);
#33929=EDGE_CURVE('',#27009,#27007,#13057,.T.);
#33930=EDGE_CURVE('',#27009,#27010,#13058,.T.);
#33931=EDGE_CURVE('',#27010,#27008,#13059,.T.);
#33932=EDGE_CURVE('',#27004,#27009,#13060,.T.);
#33933=EDGE_CURVE('',#27006,#27010,#13061,.T.);
#33934=EDGE_CURVE('',#27011,#27012,#13062,.T.);
#33935=EDGE_CURVE('',#27011,#27013,#13063,.T.);
#33936=EDGE_CURVE('',#27013,#27014,#13064,.T.);
#33937=EDGE_CURVE('',#27012,#27014,#13065,.T.);
#33938=EDGE_CURVE('',#27015,#27011,#13066,.T.);
#33939=EDGE_CURVE('',#27015,#27016,#13067,.T.);
#33940=EDGE_CURVE('',#27016,#27013,#13068,.T.);
#33941=EDGE_CURVE('',#27017,#27015,#13069,.T.);
#33942=EDGE_CURVE('',#27017,#27018,#13070,.T.);
#33943=EDGE_CURVE('',#27018,#27016,#13071,.T.);
#33944=EDGE_CURVE('',#27012,#27017,#13072,.T.);
#33945=EDGE_CURVE('',#27014,#27018,#13073,.T.);
#33946=EDGE_CURVE('',#27019,#27020,#13074,.T.);
#33947=EDGE_CURVE('',#27019,#27021,#13075,.T.);
#33948=EDGE_CURVE('',#27021,#27022,#13076,.T.);
#33949=EDGE_CURVE('',#27020,#27022,#13077,.T.);
#33950=EDGE_CURVE('',#27023,#27019,#13078,.T.);
#33951=EDGE_CURVE('',#27023,#27024,#13079,.T.);
#33952=EDGE_CURVE('',#27024,#27021,#13080,.T.);
#33953=EDGE_CURVE('',#27025,#27023,#13081,.T.);
#33954=EDGE_CURVE('',#27025,#27026,#13082,.T.);
#33955=EDGE_CURVE('',#27026,#27024,#13083,.T.);
#33956=EDGE_CURVE('',#27020,#27025,#13084,.T.);
#33957=EDGE_CURVE('',#27022,#27026,#13085,.T.);
#33958=EDGE_CURVE('',#27027,#27028,#13086,.T.);
#33959=EDGE_CURVE('',#27027,#27029,#13087,.T.);
#33960=EDGE_CURVE('',#27029,#27030,#13088,.T.);
#33961=EDGE_CURVE('',#27028,#27030,#13089,.T.);
#33962=EDGE_CURVE('',#27031,#27027,#13090,.T.);
#33963=EDGE_CURVE('',#27031,#27032,#13091,.T.);
#33964=EDGE_CURVE('',#27032,#27029,#13092,.T.);
#33965=EDGE_CURVE('',#27033,#27031,#13093,.T.);
#33966=EDGE_CURVE('',#27033,#27034,#13094,.T.);
#33967=EDGE_CURVE('',#27034,#27032,#13095,.T.);
#33968=EDGE_CURVE('',#27028,#27033,#13096,.T.);
#33969=EDGE_CURVE('',#27030,#27034,#13097,.T.);
#33970=EDGE_CURVE('',#27035,#27036,#13098,.T.);
#33971=EDGE_CURVE('',#27035,#27037,#13099,.T.);
#33972=EDGE_CURVE('',#27037,#27038,#13100,.T.);
#33973=EDGE_CURVE('',#27036,#27038,#13101,.T.);
#33974=EDGE_CURVE('',#27039,#27035,#13102,.T.);
#33975=EDGE_CURVE('',#27039,#27040,#13103,.T.);
#33976=EDGE_CURVE('',#27040,#27037,#13104,.T.);
#33977=EDGE_CURVE('',#27041,#27039,#13105,.T.);
#33978=EDGE_CURVE('',#27041,#27042,#13106,.T.);
#33979=EDGE_CURVE('',#27042,#27040,#13107,.T.);
#33980=EDGE_CURVE('',#27036,#27041,#13108,.T.);
#33981=EDGE_CURVE('',#27038,#27042,#13109,.T.);
#33982=EDGE_CURVE('',#27043,#27044,#13110,.T.);
#33983=EDGE_CURVE('',#27043,#27045,#13111,.T.);
#33984=EDGE_CURVE('',#27045,#27046,#13112,.T.);
#33985=EDGE_CURVE('',#27044,#27046,#13113,.T.);
#33986=EDGE_CURVE('',#27047,#27043,#13114,.T.);
#33987=EDGE_CURVE('',#27047,#27048,#13115,.T.);
#33988=EDGE_CURVE('',#27048,#27045,#13116,.T.);
#33989=EDGE_CURVE('',#27049,#27047,#13117,.T.);
#33990=EDGE_CURVE('',#27049,#27050,#13118,.T.);
#33991=EDGE_CURVE('',#27050,#27048,#13119,.T.);
#33992=EDGE_CURVE('',#27044,#27049,#13120,.T.);
#33993=EDGE_CURVE('',#27046,#27050,#13121,.T.);
#33994=EDGE_CURVE('',#27051,#27052,#13122,.T.);
#33995=EDGE_CURVE('',#27051,#27053,#13123,.T.);
#33996=EDGE_CURVE('',#27053,#27054,#13124,.T.);
#33997=EDGE_CURVE('',#27052,#27054,#13125,.T.);
#33998=EDGE_CURVE('',#27055,#27051,#13126,.T.);
#33999=EDGE_CURVE('',#27055,#27056,#13127,.T.);
#34000=EDGE_CURVE('',#27056,#27053,#13128,.T.);
#34001=EDGE_CURVE('',#27057,#27055,#13129,.T.);
#34002=EDGE_CURVE('',#27057,#27058,#13130,.T.);
#34003=EDGE_CURVE('',#27058,#27056,#13131,.T.);
#34004=EDGE_CURVE('',#27052,#27057,#13132,.T.);
#34005=EDGE_CURVE('',#27054,#27058,#13133,.T.);
#34006=EDGE_CURVE('',#27059,#27060,#13134,.T.);
#34007=EDGE_CURVE('',#27059,#27061,#13135,.T.);
#34008=EDGE_CURVE('',#27061,#27062,#13136,.T.);
#34009=EDGE_CURVE('',#27060,#27062,#13137,.T.);
#34010=EDGE_CURVE('',#27063,#27059,#13138,.T.);
#34011=EDGE_CURVE('',#27063,#27064,#13139,.T.);
#34012=EDGE_CURVE('',#27064,#27061,#13140,.T.);
#34013=EDGE_CURVE('',#27065,#27063,#13141,.T.);
#34014=EDGE_CURVE('',#27065,#27066,#13142,.T.);
#34015=EDGE_CURVE('',#27066,#27064,#13143,.T.);
#34016=EDGE_CURVE('',#27060,#27065,#13144,.T.);
#34017=EDGE_CURVE('',#27062,#27066,#13145,.T.);
#34018=EDGE_CURVE('',#27067,#27068,#13146,.T.);
#34019=EDGE_CURVE('',#27067,#27069,#13147,.T.);
#34020=EDGE_CURVE('',#27069,#27070,#13148,.T.);
#34021=EDGE_CURVE('',#27068,#27070,#13149,.T.);
#34022=EDGE_CURVE('',#27071,#27067,#13150,.T.);
#34023=EDGE_CURVE('',#27071,#27072,#13151,.T.);
#34024=EDGE_CURVE('',#27072,#27069,#13152,.T.);
#34025=EDGE_CURVE('',#27073,#27071,#13153,.T.);
#34026=EDGE_CURVE('',#27073,#27074,#13154,.T.);
#34027=EDGE_CURVE('',#27074,#27072,#13155,.T.);
#34028=EDGE_CURVE('',#27068,#27073,#13156,.T.);
#34029=EDGE_CURVE('',#27070,#27074,#13157,.T.);
#34030=EDGE_CURVE('',#27075,#27076,#13158,.T.);
#34031=EDGE_CURVE('',#27075,#27077,#13159,.T.);
#34032=EDGE_CURVE('',#27077,#27078,#13160,.T.);
#34033=EDGE_CURVE('',#27076,#27078,#13161,.T.);
#34034=EDGE_CURVE('',#27079,#27075,#13162,.T.);
#34035=EDGE_CURVE('',#27079,#27080,#13163,.T.);
#34036=EDGE_CURVE('',#27080,#27077,#13164,.T.);
#34037=EDGE_CURVE('',#27081,#27079,#13165,.T.);
#34038=EDGE_CURVE('',#27081,#27082,#13166,.T.);
#34039=EDGE_CURVE('',#27082,#27080,#13167,.T.);
#34040=EDGE_CURVE('',#27076,#27081,#13168,.T.);
#34041=EDGE_CURVE('',#27078,#27082,#13169,.T.);
#34042=EDGE_CURVE('',#27083,#27084,#13170,.T.);
#34043=EDGE_CURVE('',#27083,#27085,#13171,.T.);
#34044=EDGE_CURVE('',#27085,#27086,#13172,.T.);
#34045=EDGE_CURVE('',#27084,#27086,#13173,.T.);
#34046=EDGE_CURVE('',#27087,#27083,#13174,.T.);
#34047=EDGE_CURVE('',#27087,#27088,#13175,.T.);
#34048=EDGE_CURVE('',#27088,#27085,#13176,.T.);
#34049=EDGE_CURVE('',#27089,#27087,#13177,.T.);
#34050=EDGE_CURVE('',#27089,#27090,#13178,.T.);
#34051=EDGE_CURVE('',#27090,#27088,#13179,.T.);
#34052=EDGE_CURVE('',#27084,#27089,#13180,.T.);
#34053=EDGE_CURVE('',#27086,#27090,#13181,.T.);
#34054=EDGE_CURVE('',#27091,#27092,#13182,.T.);
#34055=EDGE_CURVE('',#27091,#27093,#13183,.T.);
#34056=EDGE_CURVE('',#27093,#27094,#13184,.T.);
#34057=EDGE_CURVE('',#27092,#27094,#13185,.T.);
#34058=EDGE_CURVE('',#27095,#27091,#13186,.T.);
#34059=EDGE_CURVE('',#27095,#27096,#13187,.T.);
#34060=EDGE_CURVE('',#27096,#27093,#13188,.T.);
#34061=EDGE_CURVE('',#27097,#27095,#13189,.T.);
#34062=EDGE_CURVE('',#27097,#27098,#13190,.T.);
#34063=EDGE_CURVE('',#27098,#27096,#13191,.T.);
#34064=EDGE_CURVE('',#27092,#27097,#13192,.T.);
#34065=EDGE_CURVE('',#27094,#27098,#13193,.T.);
#34066=EDGE_CURVE('',#27099,#27100,#13194,.T.);
#34067=EDGE_CURVE('',#27099,#27101,#13195,.T.);
#34068=EDGE_CURVE('',#27101,#27102,#13196,.T.);
#34069=EDGE_CURVE('',#27100,#27102,#13197,.T.);
#34070=EDGE_CURVE('',#27103,#27099,#13198,.T.);
#34071=EDGE_CURVE('',#27103,#27104,#13199,.T.);
#34072=EDGE_CURVE('',#27104,#27101,#13200,.T.);
#34073=EDGE_CURVE('',#27105,#27103,#13201,.T.);
#34074=EDGE_CURVE('',#27105,#27106,#13202,.T.);
#34075=EDGE_CURVE('',#27106,#27104,#13203,.T.);
#34076=EDGE_CURVE('',#27100,#27105,#13204,.T.);
#34077=EDGE_CURVE('',#27102,#27106,#13205,.T.);
#34078=EDGE_CURVE('',#27107,#27108,#13206,.T.);
#34079=EDGE_CURVE('',#27107,#27109,#13207,.T.);
#34080=EDGE_CURVE('',#27109,#27110,#13208,.T.);
#34081=EDGE_CURVE('',#27108,#27110,#13209,.T.);
#34082=EDGE_CURVE('',#27111,#27107,#13210,.T.);
#34083=EDGE_CURVE('',#27111,#27112,#13211,.T.);
#34084=EDGE_CURVE('',#27112,#27109,#13212,.T.);
#34085=EDGE_CURVE('',#27113,#27111,#13213,.T.);
#34086=EDGE_CURVE('',#27113,#27114,#13214,.T.);
#34087=EDGE_CURVE('',#27114,#27112,#13215,.T.);
#34088=EDGE_CURVE('',#27108,#27113,#13216,.T.);
#34089=EDGE_CURVE('',#27110,#27114,#13217,.T.);
#34090=EDGE_CURVE('',#27115,#27116,#13218,.T.);
#34091=EDGE_CURVE('',#27115,#27117,#13219,.T.);
#34092=EDGE_CURVE('',#27117,#27118,#13220,.T.);
#34093=EDGE_CURVE('',#27116,#27118,#13221,.T.);
#34094=EDGE_CURVE('',#27119,#27115,#13222,.T.);
#34095=EDGE_CURVE('',#27119,#27120,#13223,.T.);
#34096=EDGE_CURVE('',#27120,#27117,#13224,.T.);
#34097=EDGE_CURVE('',#27121,#27119,#13225,.T.);
#34098=EDGE_CURVE('',#27121,#27122,#13226,.T.);
#34099=EDGE_CURVE('',#27122,#27120,#13227,.T.);
#34100=EDGE_CURVE('',#27116,#27121,#13228,.T.);
#34101=EDGE_CURVE('',#27118,#27122,#13229,.T.);
#34102=EDGE_CURVE('',#27123,#27124,#13230,.T.);
#34103=EDGE_CURVE('',#27123,#27125,#13231,.T.);
#34104=EDGE_CURVE('',#27125,#27126,#13232,.T.);
#34105=EDGE_CURVE('',#27124,#27126,#13233,.T.);
#34106=EDGE_CURVE('',#27127,#27123,#13234,.T.);
#34107=EDGE_CURVE('',#27127,#27128,#13235,.T.);
#34108=EDGE_CURVE('',#27128,#27125,#13236,.T.);
#34109=EDGE_CURVE('',#27129,#27127,#13237,.T.);
#34110=EDGE_CURVE('',#27129,#27130,#13238,.T.);
#34111=EDGE_CURVE('',#27130,#27128,#13239,.T.);
#34112=EDGE_CURVE('',#27124,#27129,#13240,.T.);
#34113=EDGE_CURVE('',#27126,#27130,#13241,.T.);
#34114=EDGE_CURVE('',#27131,#27132,#13242,.T.);
#34115=EDGE_CURVE('',#27131,#27133,#13243,.T.);
#34116=EDGE_CURVE('',#27133,#27134,#13244,.T.);
#34117=EDGE_CURVE('',#27132,#27134,#13245,.T.);
#34118=EDGE_CURVE('',#27135,#27131,#13246,.T.);
#34119=EDGE_CURVE('',#27135,#27136,#13247,.T.);
#34120=EDGE_CURVE('',#27136,#27133,#13248,.T.);
#34121=EDGE_CURVE('',#27137,#27135,#13249,.T.);
#34122=EDGE_CURVE('',#27137,#27138,#13250,.T.);
#34123=EDGE_CURVE('',#27138,#27136,#13251,.T.);
#34124=EDGE_CURVE('',#27132,#27137,#13252,.T.);
#34125=EDGE_CURVE('',#27134,#27138,#13253,.T.);
#34126=EDGE_CURVE('',#27139,#27140,#13254,.T.);
#34127=EDGE_CURVE('',#27139,#27141,#13255,.T.);
#34128=EDGE_CURVE('',#27141,#27142,#13256,.T.);
#34129=EDGE_CURVE('',#27140,#27142,#13257,.T.);
#34130=EDGE_CURVE('',#27143,#27139,#13258,.T.);
#34131=EDGE_CURVE('',#27143,#27144,#13259,.T.);
#34132=EDGE_CURVE('',#27144,#27141,#13260,.T.);
#34133=EDGE_CURVE('',#27145,#27143,#13261,.T.);
#34134=EDGE_CURVE('',#27145,#27146,#13262,.T.);
#34135=EDGE_CURVE('',#27146,#27144,#13263,.T.);
#34136=EDGE_CURVE('',#27140,#27145,#13264,.T.);
#34137=EDGE_CURVE('',#27142,#27146,#13265,.T.);
#34138=EDGE_CURVE('',#27147,#27148,#13266,.T.);
#34139=EDGE_CURVE('',#27147,#27149,#13267,.T.);
#34140=EDGE_CURVE('',#27149,#27150,#13268,.T.);
#34141=EDGE_CURVE('',#27148,#27150,#13269,.T.);
#34142=EDGE_CURVE('',#27151,#27147,#13270,.T.);
#34143=EDGE_CURVE('',#27151,#27152,#13271,.T.);
#34144=EDGE_CURVE('',#27152,#27149,#13272,.T.);
#34145=EDGE_CURVE('',#27153,#27151,#13273,.T.);
#34146=EDGE_CURVE('',#27153,#27154,#13274,.T.);
#34147=EDGE_CURVE('',#27154,#27152,#13275,.T.);
#34148=EDGE_CURVE('',#27148,#27153,#13276,.T.);
#34149=EDGE_CURVE('',#27150,#27154,#13277,.T.);
#34150=EDGE_CURVE('',#27155,#27156,#13278,.T.);
#34151=EDGE_CURVE('',#27155,#27157,#13279,.T.);
#34152=EDGE_CURVE('',#27157,#27158,#13280,.T.);
#34153=EDGE_CURVE('',#27156,#27158,#13281,.T.);
#34154=EDGE_CURVE('',#27159,#27155,#13282,.T.);
#34155=EDGE_CURVE('',#27159,#27160,#13283,.T.);
#34156=EDGE_CURVE('',#27160,#27157,#13284,.T.);
#34157=EDGE_CURVE('',#27161,#27159,#13285,.T.);
#34158=EDGE_CURVE('',#27161,#27162,#13286,.T.);
#34159=EDGE_CURVE('',#27162,#27160,#13287,.T.);
#34160=EDGE_CURVE('',#27156,#27161,#13288,.T.);
#34161=EDGE_CURVE('',#27158,#27162,#13289,.T.);
#34162=EDGE_CURVE('',#27163,#27164,#13290,.T.);
#34163=EDGE_CURVE('',#27163,#27165,#13291,.T.);
#34164=EDGE_CURVE('',#27165,#27166,#13292,.T.);
#34165=EDGE_CURVE('',#27164,#27166,#13293,.T.);
#34166=EDGE_CURVE('',#27167,#27163,#13294,.T.);
#34167=EDGE_CURVE('',#27167,#27168,#13295,.T.);
#34168=EDGE_CURVE('',#27168,#27165,#13296,.T.);
#34169=EDGE_CURVE('',#27169,#27167,#13297,.T.);
#34170=EDGE_CURVE('',#27169,#27170,#13298,.T.);
#34171=EDGE_CURVE('',#27170,#27168,#13299,.T.);
#34172=EDGE_CURVE('',#27164,#27169,#13300,.T.);
#34173=EDGE_CURVE('',#27166,#27170,#13301,.T.);
#34174=EDGE_CURVE('',#27171,#27172,#13302,.T.);
#34175=EDGE_CURVE('',#27171,#27173,#13303,.T.);
#34176=EDGE_CURVE('',#27173,#27174,#13304,.T.);
#34177=EDGE_CURVE('',#27172,#27174,#13305,.T.);
#34178=EDGE_CURVE('',#27175,#27171,#13306,.T.);
#34179=EDGE_CURVE('',#27175,#27176,#13307,.T.);
#34180=EDGE_CURVE('',#27176,#27173,#13308,.T.);
#34181=EDGE_CURVE('',#27177,#27175,#13309,.T.);
#34182=EDGE_CURVE('',#27177,#27178,#13310,.T.);
#34183=EDGE_CURVE('',#27178,#27176,#13311,.T.);
#34184=EDGE_CURVE('',#27172,#27177,#13312,.T.);
#34185=EDGE_CURVE('',#27174,#27178,#13313,.T.);
#34186=EDGE_CURVE('',#27179,#27180,#13314,.T.);
#34187=EDGE_CURVE('',#27179,#27181,#13315,.T.);
#34188=EDGE_CURVE('',#27181,#27182,#13316,.T.);
#34189=EDGE_CURVE('',#27180,#27182,#13317,.T.);
#34190=EDGE_CURVE('',#27183,#27179,#13318,.T.);
#34191=EDGE_CURVE('',#27183,#27184,#13319,.T.);
#34192=EDGE_CURVE('',#27184,#27181,#13320,.T.);
#34193=EDGE_CURVE('',#27185,#27183,#13321,.T.);
#34194=EDGE_CURVE('',#27185,#27186,#13322,.T.);
#34195=EDGE_CURVE('',#27186,#27184,#13323,.T.);
#34196=EDGE_CURVE('',#27180,#27185,#13324,.T.);
#34197=EDGE_CURVE('',#27182,#27186,#13325,.T.);
#34198=EDGE_CURVE('',#27187,#27188,#13326,.T.);
#34199=EDGE_CURVE('',#27187,#27189,#13327,.T.);
#34200=EDGE_CURVE('',#27189,#27190,#13328,.T.);
#34201=EDGE_CURVE('',#27188,#27190,#13329,.T.);
#34202=EDGE_CURVE('',#27191,#27187,#13330,.T.);
#34203=EDGE_CURVE('',#27191,#27192,#13331,.T.);
#34204=EDGE_CURVE('',#27192,#27189,#13332,.T.);
#34205=EDGE_CURVE('',#27193,#27191,#13333,.T.);
#34206=EDGE_CURVE('',#27193,#27194,#13334,.T.);
#34207=EDGE_CURVE('',#27194,#27192,#13335,.T.);
#34208=EDGE_CURVE('',#27188,#27193,#13336,.T.);
#34209=EDGE_CURVE('',#27190,#27194,#13337,.T.);
#34210=EDGE_CURVE('',#27195,#27196,#13338,.T.);
#34211=EDGE_CURVE('',#27195,#27197,#13339,.T.);
#34212=EDGE_CURVE('',#27197,#27198,#13340,.T.);
#34213=EDGE_CURVE('',#27196,#27198,#13341,.T.);
#34214=EDGE_CURVE('',#27199,#27195,#13342,.T.);
#34215=EDGE_CURVE('',#27199,#27200,#13343,.T.);
#34216=EDGE_CURVE('',#27200,#27197,#13344,.T.);
#34217=EDGE_CURVE('',#27201,#27199,#13345,.T.);
#34218=EDGE_CURVE('',#27201,#27202,#13346,.T.);
#34219=EDGE_CURVE('',#27202,#27200,#13347,.T.);
#34220=EDGE_CURVE('',#27196,#27201,#13348,.T.);
#34221=EDGE_CURVE('',#27198,#27202,#13349,.T.);
#34222=EDGE_CURVE('',#27203,#27204,#13350,.T.);
#34223=EDGE_CURVE('',#27203,#27205,#13351,.T.);
#34224=EDGE_CURVE('',#27205,#27206,#13352,.T.);
#34225=EDGE_CURVE('',#27204,#27206,#13353,.T.);
#34226=EDGE_CURVE('',#27207,#27203,#13354,.T.);
#34227=EDGE_CURVE('',#27207,#27208,#13355,.T.);
#34228=EDGE_CURVE('',#27208,#27205,#13356,.T.);
#34229=EDGE_CURVE('',#27209,#27207,#13357,.T.);
#34230=EDGE_CURVE('',#27209,#27210,#13358,.T.);
#34231=EDGE_CURVE('',#27210,#27208,#13359,.T.);
#34232=EDGE_CURVE('',#27204,#27209,#13360,.T.);
#34233=EDGE_CURVE('',#27206,#27210,#13361,.T.);
#34234=EDGE_CURVE('',#27211,#27212,#13362,.T.);
#34235=EDGE_CURVE('',#27211,#27213,#13363,.T.);
#34236=EDGE_CURVE('',#27213,#27214,#13364,.T.);
#34237=EDGE_CURVE('',#27212,#27214,#13365,.T.);
#34238=EDGE_CURVE('',#27215,#27211,#13366,.T.);
#34239=EDGE_CURVE('',#27215,#27216,#13367,.T.);
#34240=EDGE_CURVE('',#27216,#27213,#13368,.T.);
#34241=EDGE_CURVE('',#27217,#27215,#13369,.T.);
#34242=EDGE_CURVE('',#27217,#27218,#13370,.T.);
#34243=EDGE_CURVE('',#27218,#27216,#13371,.T.);
#34244=EDGE_CURVE('',#27212,#27217,#13372,.T.);
#34245=EDGE_CURVE('',#27214,#27218,#13373,.T.);
#34246=EDGE_CURVE('',#27219,#27220,#13374,.T.);
#34247=EDGE_CURVE('',#27219,#27221,#13375,.T.);
#34248=EDGE_CURVE('',#27221,#27222,#13376,.T.);
#34249=EDGE_CURVE('',#27220,#27222,#13377,.T.);
#34250=EDGE_CURVE('',#27223,#27219,#13378,.T.);
#34251=EDGE_CURVE('',#27223,#27224,#13379,.T.);
#34252=EDGE_CURVE('',#27224,#27221,#13380,.T.);
#34253=EDGE_CURVE('',#27225,#27223,#13381,.T.);
#34254=EDGE_CURVE('',#27225,#27226,#13382,.T.);
#34255=EDGE_CURVE('',#27226,#27224,#13383,.T.);
#34256=EDGE_CURVE('',#27220,#27225,#13384,.T.);
#34257=EDGE_CURVE('',#27222,#27226,#13385,.T.);
#34258=EDGE_CURVE('',#27227,#27228,#13386,.T.);
#34259=EDGE_CURVE('',#27227,#27229,#13387,.T.);
#34260=EDGE_CURVE('',#27229,#27230,#13388,.T.);
#34261=EDGE_CURVE('',#27228,#27230,#13389,.T.);
#34262=EDGE_CURVE('',#27231,#27227,#13390,.T.);
#34263=EDGE_CURVE('',#27231,#27232,#13391,.T.);
#34264=EDGE_CURVE('',#27232,#27229,#13392,.T.);
#34265=EDGE_CURVE('',#27233,#27231,#13393,.T.);
#34266=EDGE_CURVE('',#27233,#27234,#13394,.T.);
#34267=EDGE_CURVE('',#27234,#27232,#13395,.T.);
#34268=EDGE_CURVE('',#27228,#27233,#13396,.T.);
#34269=EDGE_CURVE('',#27230,#27234,#13397,.T.);
#34270=EDGE_CURVE('',#27235,#27236,#13398,.T.);
#34271=EDGE_CURVE('',#27235,#27237,#13399,.T.);
#34272=EDGE_CURVE('',#27237,#27238,#13400,.T.);
#34273=EDGE_CURVE('',#27236,#27238,#13401,.T.);
#34274=EDGE_CURVE('',#27239,#27235,#13402,.T.);
#34275=EDGE_CURVE('',#27239,#27240,#13403,.T.);
#34276=EDGE_CURVE('',#27240,#27237,#13404,.T.);
#34277=EDGE_CURVE('',#27241,#27239,#13405,.T.);
#34278=EDGE_CURVE('',#27241,#27242,#13406,.T.);
#34279=EDGE_CURVE('',#27242,#27240,#13407,.T.);
#34280=EDGE_CURVE('',#27236,#27241,#13408,.T.);
#34281=EDGE_CURVE('',#27238,#27242,#13409,.T.);
#34282=EDGE_CURVE('',#27243,#27244,#13410,.T.);
#34283=EDGE_CURVE('',#27243,#27245,#13411,.T.);
#34284=EDGE_CURVE('',#27245,#27246,#13412,.T.);
#34285=EDGE_CURVE('',#27244,#27246,#13413,.T.);
#34286=EDGE_CURVE('',#27247,#27243,#13414,.T.);
#34287=EDGE_CURVE('',#27247,#27248,#13415,.T.);
#34288=EDGE_CURVE('',#27248,#27245,#13416,.T.);
#34289=EDGE_CURVE('',#27249,#27247,#13417,.T.);
#34290=EDGE_CURVE('',#27249,#27250,#13418,.T.);
#34291=EDGE_CURVE('',#27250,#27248,#13419,.T.);
#34292=EDGE_CURVE('',#27244,#27249,#13420,.T.);
#34293=EDGE_CURVE('',#27246,#27250,#13421,.T.);
#34294=EDGE_CURVE('',#27251,#27252,#13422,.T.);
#34295=EDGE_CURVE('',#27251,#27253,#13423,.T.);
#34296=EDGE_CURVE('',#27253,#27254,#13424,.T.);
#34297=EDGE_CURVE('',#27252,#27254,#13425,.T.);
#34298=EDGE_CURVE('',#27255,#27251,#13426,.T.);
#34299=EDGE_CURVE('',#27255,#27256,#13427,.T.);
#34300=EDGE_CURVE('',#27256,#27253,#13428,.T.);
#34301=EDGE_CURVE('',#27257,#27255,#13429,.T.);
#34302=EDGE_CURVE('',#27257,#27258,#13430,.T.);
#34303=EDGE_CURVE('',#27258,#27256,#13431,.T.);
#34304=EDGE_CURVE('',#27252,#27257,#13432,.T.);
#34305=EDGE_CURVE('',#27254,#27258,#13433,.T.);
#34306=EDGE_CURVE('',#27259,#27260,#13434,.T.);
#34307=EDGE_CURVE('',#27259,#27261,#13435,.T.);
#34308=EDGE_CURVE('',#27261,#27262,#13436,.T.);
#34309=EDGE_CURVE('',#27260,#27262,#13437,.T.);
#34310=EDGE_CURVE('',#27263,#27259,#13438,.T.);
#34311=EDGE_CURVE('',#27263,#27264,#13439,.T.);
#34312=EDGE_CURVE('',#27264,#27261,#13440,.T.);
#34313=EDGE_CURVE('',#27265,#27263,#13441,.T.);
#34314=EDGE_CURVE('',#27265,#27266,#13442,.T.);
#34315=EDGE_CURVE('',#27266,#27264,#13443,.T.);
#34316=EDGE_CURVE('',#27260,#27265,#13444,.T.);
#34317=EDGE_CURVE('',#27262,#27266,#13445,.T.);
#34318=EDGE_CURVE('',#27267,#27268,#13446,.T.);
#34319=EDGE_CURVE('',#27267,#27269,#13447,.T.);
#34320=EDGE_CURVE('',#27269,#27270,#13448,.T.);
#34321=EDGE_CURVE('',#27268,#27270,#13449,.T.);
#34322=EDGE_CURVE('',#27271,#27267,#13450,.T.);
#34323=EDGE_CURVE('',#27271,#27272,#13451,.T.);
#34324=EDGE_CURVE('',#27272,#27269,#13452,.T.);
#34325=EDGE_CURVE('',#27273,#27271,#13453,.T.);
#34326=EDGE_CURVE('',#27273,#27274,#13454,.T.);
#34327=EDGE_CURVE('',#27274,#27272,#13455,.T.);
#34328=EDGE_CURVE('',#27268,#27273,#13456,.T.);
#34329=EDGE_CURVE('',#27270,#27274,#13457,.T.);
#34330=EDGE_CURVE('',#27275,#27276,#13458,.T.);
#34331=EDGE_CURVE('',#27275,#27277,#13459,.T.);
#34332=EDGE_CURVE('',#27277,#27278,#13460,.T.);
#34333=EDGE_CURVE('',#27276,#27278,#13461,.T.);
#34334=EDGE_CURVE('',#27279,#27275,#13462,.T.);
#34335=EDGE_CURVE('',#27279,#27280,#13463,.T.);
#34336=EDGE_CURVE('',#27280,#27277,#13464,.T.);
#34337=EDGE_CURVE('',#27281,#27279,#13465,.T.);
#34338=EDGE_CURVE('',#27281,#27282,#13466,.T.);
#34339=EDGE_CURVE('',#27282,#27280,#13467,.T.);
#34340=EDGE_CURVE('',#27276,#27281,#13468,.T.);
#34341=EDGE_CURVE('',#27278,#27282,#13469,.T.);
#34342=EDGE_CURVE('',#27283,#27284,#13470,.T.);
#34343=EDGE_CURVE('',#27283,#27285,#13471,.T.);
#34344=EDGE_CURVE('',#27285,#27286,#13472,.T.);
#34345=EDGE_CURVE('',#27284,#27286,#13473,.T.);
#34346=EDGE_CURVE('',#27287,#27283,#13474,.T.);
#34347=EDGE_CURVE('',#27287,#27288,#13475,.T.);
#34348=EDGE_CURVE('',#27288,#27285,#13476,.T.);
#34349=EDGE_CURVE('',#27289,#27287,#13477,.T.);
#34350=EDGE_CURVE('',#27289,#27290,#13478,.T.);
#34351=EDGE_CURVE('',#27290,#27288,#13479,.T.);
#34352=EDGE_CURVE('',#27284,#27289,#13480,.T.);
#34353=EDGE_CURVE('',#27286,#27290,#13481,.T.);
#34354=EDGE_CURVE('',#27291,#27292,#13482,.T.);
#34355=EDGE_CURVE('',#27291,#27293,#13483,.T.);
#34356=EDGE_CURVE('',#27293,#27294,#13484,.T.);
#34357=EDGE_CURVE('',#27292,#27294,#13485,.T.);
#34358=EDGE_CURVE('',#27295,#27291,#13486,.T.);
#34359=EDGE_CURVE('',#27295,#27296,#13487,.T.);
#34360=EDGE_CURVE('',#27296,#27293,#13488,.T.);
#34361=EDGE_CURVE('',#27297,#27295,#13489,.T.);
#34362=EDGE_CURVE('',#27297,#27298,#13490,.T.);
#34363=EDGE_CURVE('',#27298,#27296,#13491,.T.);
#34364=EDGE_CURVE('',#27292,#27297,#13492,.T.);
#34365=EDGE_CURVE('',#27294,#27298,#13493,.T.);
#34366=EDGE_CURVE('',#27299,#27300,#13494,.T.);
#34367=EDGE_CURVE('',#27299,#27301,#13495,.T.);
#34368=EDGE_CURVE('',#27301,#27302,#13496,.T.);
#34369=EDGE_CURVE('',#27300,#27302,#13497,.T.);
#34370=EDGE_CURVE('',#27303,#27299,#13498,.T.);
#34371=EDGE_CURVE('',#27303,#27304,#13499,.T.);
#34372=EDGE_CURVE('',#27304,#27301,#13500,.T.);
#34373=EDGE_CURVE('',#27305,#27303,#13501,.T.);
#34374=EDGE_CURVE('',#27305,#27306,#13502,.T.);
#34375=EDGE_CURVE('',#27306,#27304,#13503,.T.);
#34376=EDGE_CURVE('',#27300,#27305,#13504,.T.);
#34377=EDGE_CURVE('',#27302,#27306,#13505,.T.);
#34378=EDGE_CURVE('',#27307,#27308,#13506,.T.);
#34379=EDGE_CURVE('',#27307,#27309,#13507,.T.);
#34380=EDGE_CURVE('',#27309,#27310,#13508,.T.);
#34381=EDGE_CURVE('',#27308,#27310,#13509,.T.);
#34382=EDGE_CURVE('',#27311,#27307,#13510,.T.);
#34383=EDGE_CURVE('',#27311,#27312,#13511,.T.);
#34384=EDGE_CURVE('',#27312,#27309,#13512,.T.);
#34385=EDGE_CURVE('',#27313,#27311,#13513,.T.);
#34386=EDGE_CURVE('',#27313,#27314,#13514,.T.);
#34387=EDGE_CURVE('',#27314,#27312,#13515,.T.);
#34388=EDGE_CURVE('',#27308,#27313,#13516,.T.);
#34389=EDGE_CURVE('',#27310,#27314,#13517,.T.);
#34390=EDGE_CURVE('',#27315,#27316,#13518,.T.);
#34391=EDGE_CURVE('',#27315,#27317,#13519,.T.);
#34392=EDGE_CURVE('',#27317,#27318,#13520,.T.);
#34393=EDGE_CURVE('',#27316,#27318,#13521,.T.);
#34394=EDGE_CURVE('',#27319,#27315,#13522,.T.);
#34395=EDGE_CURVE('',#27319,#27320,#13523,.T.);
#34396=EDGE_CURVE('',#27320,#27317,#13524,.T.);
#34397=EDGE_CURVE('',#27321,#27319,#13525,.T.);
#34398=EDGE_CURVE('',#27321,#27322,#13526,.T.);
#34399=EDGE_CURVE('',#27322,#27320,#13527,.T.);
#34400=EDGE_CURVE('',#27316,#27321,#13528,.T.);
#34401=EDGE_CURVE('',#27318,#27322,#13529,.T.);
#34402=EDGE_CURVE('',#27323,#27324,#13530,.T.);
#34403=EDGE_CURVE('',#27323,#27325,#13531,.T.);
#34404=EDGE_CURVE('',#27325,#27326,#13532,.T.);
#34405=EDGE_CURVE('',#27324,#27326,#13533,.T.);
#34406=EDGE_CURVE('',#27327,#27323,#13534,.T.);
#34407=EDGE_CURVE('',#27327,#27328,#13535,.T.);
#34408=EDGE_CURVE('',#27328,#27325,#13536,.T.);
#34409=EDGE_CURVE('',#27329,#27327,#13537,.T.);
#34410=EDGE_CURVE('',#27329,#27330,#13538,.T.);
#34411=EDGE_CURVE('',#27330,#27328,#13539,.T.);
#34412=EDGE_CURVE('',#27324,#27329,#13540,.T.);
#34413=EDGE_CURVE('',#27326,#27330,#13541,.T.);
#34414=EDGE_CURVE('',#27331,#27332,#13542,.T.);
#34415=EDGE_CURVE('',#27331,#27333,#13543,.T.);
#34416=EDGE_CURVE('',#27333,#27334,#13544,.T.);
#34417=EDGE_CURVE('',#27332,#27334,#13545,.T.);
#34418=EDGE_CURVE('',#27335,#27331,#13546,.T.);
#34419=EDGE_CURVE('',#27335,#27336,#13547,.T.);
#34420=EDGE_CURVE('',#27336,#27333,#13548,.T.);
#34421=EDGE_CURVE('',#27337,#27335,#13549,.T.);
#34422=EDGE_CURVE('',#27337,#27338,#13550,.T.);
#34423=EDGE_CURVE('',#27338,#27336,#13551,.T.);
#34424=EDGE_CURVE('',#27332,#27337,#13552,.T.);
#34425=EDGE_CURVE('',#27334,#27338,#13553,.T.);
#34426=EDGE_CURVE('',#27339,#27340,#13554,.T.);
#34427=EDGE_CURVE('',#27339,#27341,#13555,.T.);
#34428=EDGE_CURVE('',#27341,#27342,#13556,.T.);
#34429=EDGE_CURVE('',#27340,#27342,#13557,.T.);
#34430=EDGE_CURVE('',#27343,#27339,#13558,.T.);
#34431=EDGE_CURVE('',#27343,#27344,#13559,.T.);
#34432=EDGE_CURVE('',#27344,#27341,#13560,.T.);
#34433=EDGE_CURVE('',#27345,#27343,#13561,.T.);
#34434=EDGE_CURVE('',#27345,#27346,#13562,.T.);
#34435=EDGE_CURVE('',#27346,#27344,#13563,.T.);
#34436=EDGE_CURVE('',#27340,#27345,#13564,.T.);
#34437=EDGE_CURVE('',#27342,#27346,#13565,.T.);
#34438=EDGE_CURVE('',#27347,#27348,#13566,.T.);
#34439=EDGE_CURVE('',#27347,#27349,#13567,.T.);
#34440=EDGE_CURVE('',#27349,#27350,#13568,.T.);
#34441=EDGE_CURVE('',#27348,#27350,#13569,.T.);
#34442=EDGE_CURVE('',#27351,#27347,#13570,.T.);
#34443=EDGE_CURVE('',#27351,#27352,#13571,.T.);
#34444=EDGE_CURVE('',#27352,#27349,#13572,.T.);
#34445=EDGE_CURVE('',#27353,#27351,#13573,.T.);
#34446=EDGE_CURVE('',#27353,#27354,#13574,.T.);
#34447=EDGE_CURVE('',#27354,#27352,#13575,.T.);
#34448=EDGE_CURVE('',#27348,#27353,#13576,.T.);
#34449=EDGE_CURVE('',#27350,#27354,#13577,.T.);
#34450=EDGE_CURVE('',#27355,#27356,#13578,.T.);
#34451=EDGE_CURVE('',#27355,#27357,#13579,.T.);
#34452=EDGE_CURVE('',#27357,#27358,#13580,.T.);
#34453=EDGE_CURVE('',#27356,#27358,#13581,.T.);
#34454=EDGE_CURVE('',#27359,#27355,#13582,.T.);
#34455=EDGE_CURVE('',#27359,#27360,#13583,.T.);
#34456=EDGE_CURVE('',#27360,#27357,#13584,.T.);
#34457=EDGE_CURVE('',#27361,#27359,#13585,.T.);
#34458=EDGE_CURVE('',#27361,#27362,#13586,.T.);
#34459=EDGE_CURVE('',#27362,#27360,#13587,.T.);
#34460=EDGE_CURVE('',#27356,#27361,#13588,.T.);
#34461=EDGE_CURVE('',#27358,#27362,#13589,.T.);
#34462=EDGE_CURVE('',#27363,#27364,#13590,.T.);
#34463=EDGE_CURVE('',#27363,#27365,#13591,.T.);
#34464=EDGE_CURVE('',#27365,#27366,#13592,.T.);
#34465=EDGE_CURVE('',#27364,#27366,#13593,.T.);
#34466=EDGE_CURVE('',#27367,#27363,#13594,.T.);
#34467=EDGE_CURVE('',#27367,#27368,#13595,.T.);
#34468=EDGE_CURVE('',#27368,#27365,#13596,.T.);
#34469=EDGE_CURVE('',#27369,#27367,#13597,.T.);
#34470=EDGE_CURVE('',#27369,#27370,#13598,.T.);
#34471=EDGE_CURVE('',#27370,#27368,#13599,.T.);
#34472=EDGE_CURVE('',#27364,#27369,#13600,.T.);
#34473=EDGE_CURVE('',#27366,#27370,#13601,.T.);
#34474=EDGE_CURVE('',#27371,#27372,#13602,.T.);
#34475=EDGE_CURVE('',#27371,#27373,#13603,.T.);
#34476=EDGE_CURVE('',#27373,#27374,#13604,.T.);
#34477=EDGE_CURVE('',#27372,#27374,#13605,.T.);
#34478=EDGE_CURVE('',#27375,#27371,#13606,.T.);
#34479=EDGE_CURVE('',#27375,#27376,#13607,.T.);
#34480=EDGE_CURVE('',#27376,#27373,#13608,.T.);
#34481=EDGE_CURVE('',#27377,#27375,#13609,.T.);
#34482=EDGE_CURVE('',#27377,#27378,#13610,.T.);
#34483=EDGE_CURVE('',#27378,#27376,#13611,.T.);
#34484=EDGE_CURVE('',#27372,#27377,#13612,.T.);
#34485=EDGE_CURVE('',#27374,#27378,#13613,.T.);
#34486=EDGE_CURVE('',#27379,#27380,#13614,.T.);
#34487=EDGE_CURVE('',#27379,#27381,#13615,.T.);
#34488=EDGE_CURVE('',#27381,#27382,#13616,.T.);
#34489=EDGE_CURVE('',#27380,#27382,#13617,.T.);
#34490=EDGE_CURVE('',#27383,#27379,#13618,.T.);
#34491=EDGE_CURVE('',#27383,#27384,#13619,.T.);
#34492=EDGE_CURVE('',#27384,#27381,#13620,.T.);
#34493=EDGE_CURVE('',#27385,#27383,#13621,.T.);
#34494=EDGE_CURVE('',#27385,#27386,#13622,.T.);
#34495=EDGE_CURVE('',#27386,#27384,#13623,.T.);
#34496=EDGE_CURVE('',#27380,#27385,#13624,.T.);
#34497=EDGE_CURVE('',#27382,#27386,#13625,.T.);
#34498=EDGE_CURVE('',#27387,#27388,#13626,.T.);
#34499=EDGE_CURVE('',#27387,#27389,#13627,.T.);
#34500=EDGE_CURVE('',#27389,#27390,#13628,.T.);
#34501=EDGE_CURVE('',#27388,#27390,#13629,.T.);
#34502=EDGE_CURVE('',#27391,#27387,#13630,.T.);
#34503=EDGE_CURVE('',#27391,#27392,#13631,.T.);
#34504=EDGE_CURVE('',#27392,#27389,#13632,.T.);
#34505=EDGE_CURVE('',#27393,#27391,#13633,.T.);
#34506=EDGE_CURVE('',#27393,#27394,#13634,.T.);
#34507=EDGE_CURVE('',#27394,#27392,#13635,.T.);
#34508=EDGE_CURVE('',#27388,#27393,#13636,.T.);
#34509=EDGE_CURVE('',#27390,#27394,#13637,.T.);
#34510=EDGE_CURVE('',#27395,#27396,#13638,.T.);
#34511=EDGE_CURVE('',#27395,#27397,#13639,.T.);
#34512=EDGE_CURVE('',#27397,#27398,#13640,.T.);
#34513=EDGE_CURVE('',#27396,#27398,#13641,.T.);
#34514=EDGE_CURVE('',#27399,#27395,#13642,.T.);
#34515=EDGE_CURVE('',#27399,#27400,#13643,.T.);
#34516=EDGE_CURVE('',#27400,#27397,#13644,.T.);
#34517=EDGE_CURVE('',#27401,#27399,#13645,.T.);
#34518=EDGE_CURVE('',#27401,#27402,#13646,.T.);
#34519=EDGE_CURVE('',#27402,#27400,#13647,.T.);
#34520=EDGE_CURVE('',#27396,#27401,#13648,.T.);
#34521=EDGE_CURVE('',#27398,#27402,#13649,.T.);
#34522=EDGE_CURVE('',#27403,#27404,#13650,.T.);
#34523=EDGE_CURVE('',#27403,#27405,#13651,.T.);
#34524=EDGE_CURVE('',#27405,#27406,#13652,.T.);
#34525=EDGE_CURVE('',#27404,#27406,#13653,.T.);
#34526=EDGE_CURVE('',#27407,#27403,#13654,.T.);
#34527=EDGE_CURVE('',#27407,#27408,#13655,.T.);
#34528=EDGE_CURVE('',#27408,#27405,#13656,.T.);
#34529=EDGE_CURVE('',#27409,#27407,#13657,.T.);
#34530=EDGE_CURVE('',#27409,#27410,#13658,.T.);
#34531=EDGE_CURVE('',#27410,#27408,#13659,.T.);
#34532=EDGE_CURVE('',#27404,#27409,#13660,.T.);
#34533=EDGE_CURVE('',#27406,#27410,#13661,.T.);
#34534=EDGE_CURVE('',#27411,#27412,#13662,.T.);
#34535=EDGE_CURVE('',#27411,#27413,#13663,.T.);
#34536=EDGE_CURVE('',#27413,#27414,#13664,.T.);
#34537=EDGE_CURVE('',#27412,#27414,#13665,.T.);
#34538=EDGE_CURVE('',#27415,#27411,#13666,.T.);
#34539=EDGE_CURVE('',#27415,#27416,#13667,.T.);
#34540=EDGE_CURVE('',#27416,#27413,#13668,.T.);
#34541=EDGE_CURVE('',#27417,#27415,#13669,.T.);
#34542=EDGE_CURVE('',#27417,#27418,#13670,.T.);
#34543=EDGE_CURVE('',#27418,#27416,#13671,.T.);
#34544=EDGE_CURVE('',#27412,#27417,#13672,.T.);
#34545=EDGE_CURVE('',#27414,#27418,#13673,.T.);
#34546=EDGE_CURVE('',#27419,#27420,#13674,.T.);
#34547=EDGE_CURVE('',#27419,#27421,#13675,.T.);
#34548=EDGE_CURVE('',#27421,#27422,#13676,.T.);
#34549=EDGE_CURVE('',#27420,#27422,#13677,.T.);
#34550=EDGE_CURVE('',#27423,#27419,#13678,.T.);
#34551=EDGE_CURVE('',#27423,#27424,#13679,.T.);
#34552=EDGE_CURVE('',#27424,#27421,#13680,.T.);
#34553=EDGE_CURVE('',#27425,#27423,#13681,.T.);
#34554=EDGE_CURVE('',#27425,#27426,#13682,.T.);
#34555=EDGE_CURVE('',#27426,#27424,#13683,.T.);
#34556=EDGE_CURVE('',#27420,#27425,#13684,.T.);
#34557=EDGE_CURVE('',#27422,#27426,#13685,.T.);
#34558=EDGE_CURVE('',#27427,#27428,#13686,.T.);
#34559=EDGE_CURVE('',#27427,#27429,#13687,.T.);
#34560=EDGE_CURVE('',#27429,#27430,#13688,.T.);
#34561=EDGE_CURVE('',#27428,#27430,#13689,.T.);
#34562=EDGE_CURVE('',#27431,#27427,#13690,.T.);
#34563=EDGE_CURVE('',#27431,#27432,#13691,.T.);
#34564=EDGE_CURVE('',#27432,#27429,#13692,.T.);
#34565=EDGE_CURVE('',#27433,#27431,#13693,.T.);
#34566=EDGE_CURVE('',#27433,#27434,#13694,.T.);
#34567=EDGE_CURVE('',#27434,#27432,#13695,.T.);
#34568=EDGE_CURVE('',#27428,#27433,#13696,.T.);
#34569=EDGE_CURVE('',#27430,#27434,#13697,.T.);
#34570=EDGE_CURVE('',#27435,#27436,#13698,.T.);
#34571=EDGE_CURVE('',#27435,#27437,#13699,.T.);
#34572=EDGE_CURVE('',#27437,#27438,#13700,.T.);
#34573=EDGE_CURVE('',#27436,#27438,#13701,.T.);
#34574=EDGE_CURVE('',#27439,#27435,#13702,.T.);
#34575=EDGE_CURVE('',#27439,#27440,#13703,.T.);
#34576=EDGE_CURVE('',#27440,#27437,#13704,.T.);
#34577=EDGE_CURVE('',#27441,#27439,#13705,.T.);
#34578=EDGE_CURVE('',#27441,#27442,#13706,.T.);
#34579=EDGE_CURVE('',#27442,#27440,#13707,.T.);
#34580=EDGE_CURVE('',#27436,#27441,#13708,.T.);
#34581=EDGE_CURVE('',#27438,#27442,#13709,.T.);
#34582=EDGE_CURVE('',#27443,#27444,#13710,.T.);
#34583=EDGE_CURVE('',#27443,#27445,#13711,.T.);
#34584=EDGE_CURVE('',#27445,#27446,#13712,.T.);
#34585=EDGE_CURVE('',#27444,#27446,#13713,.T.);
#34586=EDGE_CURVE('',#27447,#27443,#13714,.T.);
#34587=EDGE_CURVE('',#27447,#27448,#13715,.T.);
#34588=EDGE_CURVE('',#27448,#27445,#13716,.T.);
#34589=EDGE_CURVE('',#27449,#27447,#13717,.T.);
#34590=EDGE_CURVE('',#27449,#27450,#13718,.T.);
#34591=EDGE_CURVE('',#27450,#27448,#13719,.T.);
#34592=EDGE_CURVE('',#27444,#27449,#13720,.T.);
#34593=EDGE_CURVE('',#27446,#27450,#13721,.T.);
#34594=EDGE_CURVE('',#27451,#27452,#13722,.T.);
#34595=EDGE_CURVE('',#27451,#27453,#13723,.T.);
#34596=EDGE_CURVE('',#27453,#27454,#13724,.T.);
#34597=EDGE_CURVE('',#27452,#27454,#13725,.T.);
#34598=EDGE_CURVE('',#27455,#27451,#13726,.T.);
#34599=EDGE_CURVE('',#27455,#27456,#13727,.T.);
#34600=EDGE_CURVE('',#27456,#27453,#13728,.T.);
#34601=EDGE_CURVE('',#27457,#27455,#13729,.T.);
#34602=EDGE_CURVE('',#27457,#27458,#13730,.T.);
#34603=EDGE_CURVE('',#27458,#27456,#13731,.T.);
#34604=EDGE_CURVE('',#27452,#27457,#13732,.T.);
#34605=EDGE_CURVE('',#27454,#27458,#13733,.T.);
#34606=EDGE_CURVE('',#27459,#27460,#13734,.T.);
#34607=EDGE_CURVE('',#27459,#27461,#13735,.T.);
#34608=EDGE_CURVE('',#27461,#27462,#13736,.T.);
#34609=EDGE_CURVE('',#27460,#27462,#13737,.T.);
#34610=EDGE_CURVE('',#27463,#27459,#13738,.T.);
#34611=EDGE_CURVE('',#27463,#27464,#13739,.T.);
#34612=EDGE_CURVE('',#27464,#27461,#13740,.T.);
#34613=EDGE_CURVE('',#27465,#27463,#13741,.T.);
#34614=EDGE_CURVE('',#27465,#27466,#13742,.T.);
#34615=EDGE_CURVE('',#27466,#27464,#13743,.T.);
#34616=EDGE_CURVE('',#27460,#27465,#13744,.T.);
#34617=EDGE_CURVE('',#27462,#27466,#13745,.T.);
#34618=EDGE_CURVE('',#27467,#27468,#13746,.T.);
#34619=EDGE_CURVE('',#27467,#27469,#13747,.T.);
#34620=EDGE_CURVE('',#27469,#27470,#13748,.T.);
#34621=EDGE_CURVE('',#27468,#27470,#13749,.T.);
#34622=EDGE_CURVE('',#27471,#27467,#13750,.T.);
#34623=EDGE_CURVE('',#27471,#27472,#13751,.T.);
#34624=EDGE_CURVE('',#27472,#27469,#13752,.T.);
#34625=EDGE_CURVE('',#27473,#27471,#13753,.T.);
#34626=EDGE_CURVE('',#27473,#27474,#13754,.T.);
#34627=EDGE_CURVE('',#27474,#27472,#13755,.T.);
#34628=EDGE_CURVE('',#27468,#27473,#13756,.T.);
#34629=EDGE_CURVE('',#27470,#27474,#13757,.T.);
#34630=EDGE_CURVE('',#27475,#27476,#13758,.T.);
#34631=EDGE_CURVE('',#27475,#27477,#13759,.T.);
#34632=EDGE_CURVE('',#27477,#27478,#13760,.T.);
#34633=EDGE_CURVE('',#27476,#27478,#13761,.T.);
#34634=EDGE_CURVE('',#27479,#27475,#13762,.T.);
#34635=EDGE_CURVE('',#27479,#27480,#13763,.T.);
#34636=EDGE_CURVE('',#27480,#27477,#13764,.T.);
#34637=EDGE_CURVE('',#27481,#27479,#13765,.T.);
#34638=EDGE_CURVE('',#27481,#27482,#13766,.T.);
#34639=EDGE_CURVE('',#27482,#27480,#13767,.T.);
#34640=EDGE_CURVE('',#27476,#27481,#13768,.T.);
#34641=EDGE_CURVE('',#27478,#27482,#13769,.T.);
#34642=EDGE_CURVE('',#27483,#27484,#13770,.T.);
#34643=EDGE_CURVE('',#27483,#27485,#13771,.T.);
#34644=EDGE_CURVE('',#27485,#27486,#13772,.T.);
#34645=EDGE_CURVE('',#27484,#27486,#13773,.T.);
#34646=EDGE_CURVE('',#27487,#27483,#13774,.T.);
#34647=EDGE_CURVE('',#27487,#27488,#13775,.T.);
#34648=EDGE_CURVE('',#27488,#27485,#13776,.T.);
#34649=EDGE_CURVE('',#27489,#27487,#13777,.T.);
#34650=EDGE_CURVE('',#27489,#27490,#13778,.T.);
#34651=EDGE_CURVE('',#27490,#27488,#13779,.T.);
#34652=EDGE_CURVE('',#27484,#27489,#13780,.T.);
#34653=EDGE_CURVE('',#27486,#27490,#13781,.T.);
#34654=EDGE_CURVE('',#27491,#27492,#13782,.T.);
#34655=EDGE_CURVE('',#27491,#27493,#13783,.T.);
#34656=EDGE_CURVE('',#27493,#27494,#13784,.T.);
#34657=EDGE_CURVE('',#27492,#27494,#13785,.T.);
#34658=EDGE_CURVE('',#27495,#27491,#13786,.T.);
#34659=EDGE_CURVE('',#27495,#27496,#13787,.T.);
#34660=EDGE_CURVE('',#27496,#27493,#13788,.T.);
#34661=EDGE_CURVE('',#27497,#27495,#13789,.T.);
#34662=EDGE_CURVE('',#27497,#27498,#13790,.T.);
#34663=EDGE_CURVE('',#27498,#27496,#13791,.T.);
#34664=EDGE_CURVE('',#27492,#27497,#13792,.T.);
#34665=EDGE_CURVE('',#27494,#27498,#13793,.T.);
#34666=EDGE_CURVE('',#27499,#27500,#13794,.T.);
#34667=EDGE_CURVE('',#27499,#27501,#13795,.T.);
#34668=EDGE_CURVE('',#27501,#27502,#13796,.T.);
#34669=EDGE_CURVE('',#27500,#27502,#13797,.T.);
#34670=EDGE_CURVE('',#27503,#27499,#13798,.T.);
#34671=EDGE_CURVE('',#27503,#27504,#13799,.T.);
#34672=EDGE_CURVE('',#27504,#27501,#13800,.T.);
#34673=EDGE_CURVE('',#27505,#27503,#13801,.T.);
#34674=EDGE_CURVE('',#27505,#27506,#13802,.T.);
#34675=EDGE_CURVE('',#27506,#27504,#13803,.T.);
#34676=EDGE_CURVE('',#27500,#27505,#13804,.T.);
#34677=EDGE_CURVE('',#27502,#27506,#13805,.T.);
#34678=EDGE_CURVE('',#27507,#27508,#13806,.T.);
#34679=EDGE_CURVE('',#27507,#27509,#13807,.T.);
#34680=EDGE_CURVE('',#27509,#27510,#13808,.T.);
#34681=EDGE_CURVE('',#27508,#27510,#13809,.T.);
#34682=EDGE_CURVE('',#27511,#27507,#13810,.T.);
#34683=EDGE_CURVE('',#27511,#27512,#13811,.T.);
#34684=EDGE_CURVE('',#27512,#27509,#13812,.T.);
#34685=EDGE_CURVE('',#27513,#27511,#13813,.T.);
#34686=EDGE_CURVE('',#27513,#27514,#13814,.T.);
#34687=EDGE_CURVE('',#27514,#27512,#13815,.T.);
#34688=EDGE_CURVE('',#27508,#27513,#13816,.T.);
#34689=EDGE_CURVE('',#27510,#27514,#13817,.T.);
#34690=EDGE_CURVE('',#27515,#27516,#13818,.T.);
#34691=EDGE_CURVE('',#27515,#27517,#13819,.T.);
#34692=EDGE_CURVE('',#27517,#27518,#13820,.T.);
#34693=EDGE_CURVE('',#27516,#27518,#13821,.T.);
#34694=EDGE_CURVE('',#27519,#27515,#13822,.T.);
#34695=EDGE_CURVE('',#27519,#27520,#13823,.T.);
#34696=EDGE_CURVE('',#27520,#27517,#13824,.T.);
#34697=EDGE_CURVE('',#27521,#27519,#13825,.T.);
#34698=EDGE_CURVE('',#27521,#27522,#13826,.T.);
#34699=EDGE_CURVE('',#27522,#27520,#13827,.T.);
#34700=EDGE_CURVE('',#27516,#27521,#13828,.T.);
#34701=EDGE_CURVE('',#27518,#27522,#13829,.T.);
#34702=EDGE_CURVE('',#27523,#27524,#13830,.T.);
#34703=EDGE_CURVE('',#27523,#27525,#13831,.T.);
#34704=EDGE_CURVE('',#27525,#27526,#13832,.T.);
#34705=EDGE_CURVE('',#27524,#27526,#13833,.T.);
#34706=EDGE_CURVE('',#27527,#27523,#13834,.T.);
#34707=EDGE_CURVE('',#27527,#27528,#13835,.T.);
#34708=EDGE_CURVE('',#27528,#27525,#13836,.T.);
#34709=EDGE_CURVE('',#27529,#27527,#13837,.T.);
#34710=EDGE_CURVE('',#27529,#27530,#13838,.T.);
#34711=EDGE_CURVE('',#27530,#27528,#13839,.T.);
#34712=EDGE_CURVE('',#27524,#27529,#13840,.T.);
#34713=EDGE_CURVE('',#27526,#27530,#13841,.T.);
#34714=EDGE_CURVE('',#27531,#27532,#13842,.T.);
#34715=EDGE_CURVE('',#27531,#27533,#13843,.T.);
#34716=EDGE_CURVE('',#27533,#27534,#13844,.T.);
#34717=EDGE_CURVE('',#27532,#27534,#13845,.T.);
#34718=EDGE_CURVE('',#27535,#27531,#13846,.T.);
#34719=EDGE_CURVE('',#27535,#27536,#13847,.T.);
#34720=EDGE_CURVE('',#27536,#27533,#13848,.T.);
#34721=EDGE_CURVE('',#27537,#27535,#13849,.T.);
#34722=EDGE_CURVE('',#27537,#27538,#13850,.T.);
#34723=EDGE_CURVE('',#27538,#27536,#13851,.T.);
#34724=EDGE_CURVE('',#27532,#27537,#13852,.T.);
#34725=EDGE_CURVE('',#27534,#27538,#13853,.T.);
#34726=EDGE_CURVE('',#27539,#27540,#13854,.T.);
#34727=EDGE_CURVE('',#27539,#27541,#13855,.T.);
#34728=EDGE_CURVE('',#27541,#27542,#13856,.T.);
#34729=EDGE_CURVE('',#27540,#27542,#13857,.T.);
#34730=EDGE_CURVE('',#27543,#27539,#13858,.T.);
#34731=EDGE_CURVE('',#27543,#27544,#13859,.T.);
#34732=EDGE_CURVE('',#27544,#27541,#13860,.T.);
#34733=EDGE_CURVE('',#27545,#27543,#13861,.T.);
#34734=EDGE_CURVE('',#27545,#27546,#13862,.T.);
#34735=EDGE_CURVE('',#27546,#27544,#13863,.T.);
#34736=EDGE_CURVE('',#27540,#27545,#13864,.T.);
#34737=EDGE_CURVE('',#27542,#27546,#13865,.T.);
#34738=EDGE_CURVE('',#27547,#27548,#13866,.T.);
#34739=EDGE_CURVE('',#27547,#27549,#13867,.T.);
#34740=EDGE_CURVE('',#27549,#27550,#13868,.T.);
#34741=EDGE_CURVE('',#27548,#27550,#13869,.T.);
#34742=EDGE_CURVE('',#27551,#27547,#13870,.T.);
#34743=EDGE_CURVE('',#27551,#27552,#13871,.T.);
#34744=EDGE_CURVE('',#27552,#27549,#13872,.T.);
#34745=EDGE_CURVE('',#27553,#27551,#13873,.T.);
#34746=EDGE_CURVE('',#27553,#27554,#13874,.T.);
#34747=EDGE_CURVE('',#27554,#27552,#13875,.T.);
#34748=EDGE_CURVE('',#27548,#27553,#13876,.T.);
#34749=EDGE_CURVE('',#27550,#27554,#13877,.T.);
#34750=EDGE_CURVE('',#27555,#27556,#13878,.T.);
#34751=EDGE_CURVE('',#27555,#27557,#13879,.T.);
#34752=EDGE_CURVE('',#27557,#27558,#13880,.T.);
#34753=EDGE_CURVE('',#27556,#27558,#13881,.T.);
#34754=EDGE_CURVE('',#27559,#27555,#13882,.T.);
#34755=EDGE_CURVE('',#27559,#27560,#13883,.T.);
#34756=EDGE_CURVE('',#27560,#27557,#13884,.T.);
#34757=EDGE_CURVE('',#27561,#27559,#13885,.T.);
#34758=EDGE_CURVE('',#27561,#27562,#13886,.T.);
#34759=EDGE_CURVE('',#27562,#27560,#13887,.T.);
#34760=EDGE_CURVE('',#27556,#27561,#13888,.T.);
#34761=EDGE_CURVE('',#27558,#27562,#13889,.T.);
#34762=EDGE_CURVE('',#27563,#27564,#13890,.T.);
#34763=EDGE_CURVE('',#27563,#27565,#13891,.T.);
#34764=EDGE_CURVE('',#27565,#27566,#13892,.T.);
#34765=EDGE_CURVE('',#27564,#27566,#13893,.T.);
#34766=EDGE_CURVE('',#27567,#27563,#13894,.T.);
#34767=EDGE_CURVE('',#27567,#27568,#13895,.T.);
#34768=EDGE_CURVE('',#27568,#27565,#13896,.T.);
#34769=EDGE_CURVE('',#27569,#27567,#13897,.T.);
#34770=EDGE_CURVE('',#27569,#27570,#13898,.T.);
#34771=EDGE_CURVE('',#27570,#27568,#13899,.T.);
#34772=EDGE_CURVE('',#27564,#27569,#13900,.T.);
#34773=EDGE_CURVE('',#27566,#27570,#13901,.T.);
#34774=EDGE_CURVE('',#27571,#27572,#13902,.T.);
#34775=EDGE_CURVE('',#27571,#27573,#13903,.T.);
#34776=EDGE_CURVE('',#27573,#27574,#13904,.T.);
#34777=EDGE_CURVE('',#27572,#27574,#13905,.T.);
#34778=EDGE_CURVE('',#27575,#27571,#13906,.T.);
#34779=EDGE_CURVE('',#27575,#27576,#13907,.T.);
#34780=EDGE_CURVE('',#27576,#27573,#13908,.T.);
#34781=EDGE_CURVE('',#27577,#27575,#13909,.T.);
#34782=EDGE_CURVE('',#27577,#27578,#13910,.T.);
#34783=EDGE_CURVE('',#27578,#27576,#13911,.T.);
#34784=EDGE_CURVE('',#27572,#27577,#13912,.T.);
#34785=EDGE_CURVE('',#27574,#27578,#13913,.T.);
#34786=EDGE_CURVE('',#27579,#27580,#13914,.T.);
#34787=EDGE_CURVE('',#27579,#27581,#13915,.T.);
#34788=EDGE_CURVE('',#27581,#27582,#13916,.T.);
#34789=EDGE_CURVE('',#27580,#27582,#13917,.T.);
#34790=EDGE_CURVE('',#27583,#27579,#13918,.T.);
#34791=EDGE_CURVE('',#27583,#27584,#13919,.T.);
#34792=EDGE_CURVE('',#27584,#27581,#13920,.T.);
#34793=EDGE_CURVE('',#27585,#27583,#13921,.T.);
#34794=EDGE_CURVE('',#27585,#27586,#13922,.T.);
#34795=EDGE_CURVE('',#27586,#27584,#13923,.T.);
#34796=EDGE_CURVE('',#27580,#27585,#13924,.T.);
#34797=EDGE_CURVE('',#27582,#27586,#13925,.T.);
#34798=EDGE_CURVE('',#27587,#27588,#13926,.T.);
#34799=EDGE_CURVE('',#27587,#27589,#13927,.T.);
#34800=EDGE_CURVE('',#27589,#27590,#13928,.T.);
#34801=EDGE_CURVE('',#27588,#27590,#13929,.T.);
#34802=EDGE_CURVE('',#27591,#27587,#13930,.T.);
#34803=EDGE_CURVE('',#27591,#27592,#13931,.T.);
#34804=EDGE_CURVE('',#27592,#27589,#13932,.T.);
#34805=EDGE_CURVE('',#27593,#27591,#13933,.T.);
#34806=EDGE_CURVE('',#27593,#27594,#13934,.T.);
#34807=EDGE_CURVE('',#27594,#27592,#13935,.T.);
#34808=EDGE_CURVE('',#27588,#27593,#13936,.T.);
#34809=EDGE_CURVE('',#27590,#27594,#13937,.T.);
#34810=EDGE_CURVE('',#27595,#27596,#13938,.T.);
#34811=EDGE_CURVE('',#27595,#27597,#13939,.T.);
#34812=EDGE_CURVE('',#27597,#27598,#13940,.T.);
#34813=EDGE_CURVE('',#27596,#27598,#13941,.T.);
#34814=EDGE_CURVE('',#27599,#27595,#13942,.T.);
#34815=EDGE_CURVE('',#27599,#27600,#13943,.T.);
#34816=EDGE_CURVE('',#27600,#27597,#13944,.T.);
#34817=EDGE_CURVE('',#27601,#27599,#13945,.T.);
#34818=EDGE_CURVE('',#27601,#27602,#13946,.T.);
#34819=EDGE_CURVE('',#27602,#27600,#13947,.T.);
#34820=EDGE_CURVE('',#27596,#27601,#13948,.T.);
#34821=EDGE_CURVE('',#27598,#27602,#13949,.T.);
#34822=EDGE_CURVE('',#27603,#27604,#13950,.T.);
#34823=EDGE_CURVE('',#27603,#27605,#13951,.T.);
#34824=EDGE_CURVE('',#27605,#27606,#13952,.T.);
#34825=EDGE_CURVE('',#27604,#27606,#13953,.T.);
#34826=EDGE_CURVE('',#27607,#27603,#13954,.T.);
#34827=EDGE_CURVE('',#27607,#27608,#13955,.T.);
#34828=EDGE_CURVE('',#27608,#27605,#13956,.T.);
#34829=EDGE_CURVE('',#27609,#27607,#13957,.T.);
#34830=EDGE_CURVE('',#27609,#27610,#13958,.T.);
#34831=EDGE_CURVE('',#27610,#27608,#13959,.T.);
#34832=EDGE_CURVE('',#27604,#27609,#13960,.T.);
#34833=EDGE_CURVE('',#27606,#27610,#13961,.T.);
#34834=EDGE_CURVE('',#27611,#27612,#13962,.T.);
#34835=EDGE_CURVE('',#27611,#27613,#13963,.T.);
#34836=EDGE_CURVE('',#27613,#27614,#13964,.T.);
#34837=EDGE_CURVE('',#27612,#27614,#13965,.T.);
#34838=EDGE_CURVE('',#27615,#27611,#13966,.T.);
#34839=EDGE_CURVE('',#27615,#27616,#13967,.T.);
#34840=EDGE_CURVE('',#27616,#27613,#13968,.T.);
#34841=EDGE_CURVE('',#27617,#27615,#13969,.T.);
#34842=EDGE_CURVE('',#27617,#27618,#13970,.T.);
#34843=EDGE_CURVE('',#27618,#27616,#13971,.T.);
#34844=EDGE_CURVE('',#27612,#27617,#13972,.T.);
#34845=EDGE_CURVE('',#27614,#27618,#13973,.T.);
#34846=EDGE_CURVE('',#27619,#27620,#13974,.T.);
#34847=EDGE_CURVE('',#27619,#27621,#13975,.T.);
#34848=EDGE_CURVE('',#27621,#27622,#13976,.T.);
#34849=EDGE_CURVE('',#27620,#27622,#13977,.T.);
#34850=EDGE_CURVE('',#27623,#27619,#13978,.T.);
#34851=EDGE_CURVE('',#27623,#27624,#13979,.T.);
#34852=EDGE_CURVE('',#27624,#27621,#13980,.T.);
#34853=EDGE_CURVE('',#27625,#27623,#13981,.T.);
#34854=EDGE_CURVE('',#27625,#27626,#13982,.T.);
#34855=EDGE_CURVE('',#27626,#27624,#13983,.T.);
#34856=EDGE_CURVE('',#27620,#27625,#13984,.T.);
#34857=EDGE_CURVE('',#27622,#27626,#13985,.T.);
#34858=EDGE_CURVE('',#27627,#27628,#13986,.T.);
#34859=EDGE_CURVE('',#27629,#27627,#13987,.T.);
#34860=EDGE_CURVE('',#27629,#27630,#13988,.T.);
#34861=EDGE_CURVE('',#27631,#27630,#13989,.T.);
#34862=EDGE_CURVE('',#27632,#27631,#13990,.T.);
#34863=EDGE_CURVE('',#27628,#27632,#13991,.T.);
#34864=EDGE_CURVE('',#27633,#27634,#13992,.T.);
#34865=EDGE_CURVE('',#27635,#27633,#13993,.T.);
#34866=EDGE_CURVE('',#27636,#27635,#13994,.T.);
#34867=EDGE_CURVE('',#27637,#27636,#13995,.T.);
#34868=EDGE_CURVE('',#27637,#27638,#13996,.T.);
#34869=EDGE_CURVE('',#27634,#27638,#13997,.T.);
#34870=EDGE_CURVE('',#27630,#27637,#13998,.T.);
#34871=EDGE_CURVE('',#27638,#27629,#13999,.T.);
#34872=EDGE_CURVE('',#27639,#27636,#14000,.T.);
#34873=EDGE_CURVE('',#27640,#27639,#14001,.T.);
#34874=EDGE_CURVE('',#27641,#27640,#14002,.T.);
#34875=EDGE_CURVE('',#27642,#27641,#14003,.T.);
#34876=EDGE_CURVE('',#27643,#27642,#14004,.T.);
#34877=EDGE_CURVE('',#27643,#27644,#957,.T.);
#34878=EDGE_CURVE('',#27645,#27644,#14005,.T.);
#34879=EDGE_CURVE('',#27646,#27645,#14006,.T.);
#34880=EDGE_CURVE('',#27647,#27646,#14007,.T.);
#34881=EDGE_CURVE('',#27648,#27647,#14008,.T.);
#34882=EDGE_CURVE('',#27649,#27648,#14009,.T.);
#34883=EDGE_CURVE('',#27650,#27649,#14010,.T.);
#34884=EDGE_CURVE('',#27651,#27650,#14011,.T.);
#34885=EDGE_CURVE('',#27652,#27651,#14012,.T.);
#34886=EDGE_CURVE('',#27653,#27652,#14013,.T.);
#34887=EDGE_CURVE('',#27653,#27654,#958,.T.);
#34888=EDGE_CURVE('',#27655,#27654,#14014,.T.);
#34889=EDGE_CURVE('',#27656,#27655,#14015,.T.);
#34890=EDGE_CURVE('',#27657,#27656,#14016,.T.);
#34891=EDGE_CURVE('',#27658,#27657,#14017,.T.);
#34892=EDGE_CURVE('',#27631,#27658,#14018,.T.);
#34893=EDGE_CURVE('',#27634,#27659,#14019,.T.);
#34894=EDGE_CURVE('',#27659,#27660,#14020,.T.);
#34895=EDGE_CURVE('',#27660,#27633,#14021,.T.);
#34896=EDGE_CURVE('',#27628,#27661,#14022,.T.);
#34897=EDGE_CURVE('',#27662,#27661,#14023,.T.);
#34898=EDGE_CURVE('',#27662,#27627,#14024,.T.);
#34899=EDGE_CURVE('',#27635,#27663,#14025,.T.);
#34900=EDGE_CURVE('',#27639,#27663,#14026,.T.);
#34901=EDGE_CURVE('',#27663,#27660,#14027,.T.);
#34902=EDGE_CURVE('',#27664,#27664,#959,.T.);
#34903=EDGE_CURVE('',#27665,#27665,#960,.T.);
#34904=EDGE_CURVE('',#27666,#27666,#961,.T.);
#34905=EDGE_CURVE('',#27667,#27667,#962,.T.);
#34906=EDGE_CURVE('',#27667,#27668,#14028,.T.);
#34907=EDGE_CURVE('',#27669,#27669,#963,.T.);
#34908=EDGE_CURVE('',#27669,#27670,#14029,.T.);
#34909=EDGE_CURVE('',#27671,#27671,#964,.T.);
#34910=EDGE_CURVE('',#27671,#27669,#14030,.T.);
#34911=EDGE_CURVE('',#27672,#27672,#965,.T.);
#34912=EDGE_CURVE('',#27672,#27667,#14031,.T.);
#34913=EDGE_CURVE('',#27673,#27673,#966,.T.);
#34914=EDGE_CURVE('',#27673,#27674,#14032,.T.);
#34915=EDGE_CURVE('',#27674,#27674,#967,.T.);
#34916=EDGE_CURVE('',#27674,#27675,#14033,.T.);
#34917=EDGE_CURVE('',#27675,#27675,#968,.T.);
#34918=EDGE_CURVE('',#27676,#27677,#14034,.T.);
#34919=EDGE_CURVE('',#27678,#27676,#14035,.T.);
#34920=EDGE_CURVE('',#27679,#27678,#14036,.T.);
#34921=EDGE_CURVE('',#27679,#27677,#14037,.T.);
#34922=EDGE_CURVE('',#27680,#27680,#969,.T.);
#34923=EDGE_CURVE('',#27675,#27681,#14038,.T.);
#34924=EDGE_CURVE('',#27680,#27682,#14039,.T.);
#34925=EDGE_CURVE('',#27682,#27682,#970,.T.);
#34926=EDGE_CURVE('',#27682,#27683,#14040,.T.);
#34927=EDGE_CURVE('',#27683,#27683,#971,.T.);
#34928=EDGE_CURVE('',#27683,#27684,#14041,.T.);
#34929=EDGE_CURVE('',#27685,#27685,#972,.T.);
#34930=EDGE_CURVE('',#27685,#27686,#14042,.T.);
#34931=EDGE_CURVE('',#27686,#27686,#973,.T.);
#34932=EDGE_CURVE('',#27687,#27687,#974,.T.);
#34933=EDGE_CURVE('',#27688,#27688,#975,.T.);
#34934=EDGE_CURVE('',#27688,#27689,#14043,.T.);
#34935=EDGE_CURVE('',#27689,#27689,#976,.T.);
#34936=EDGE_CURVE('',#27690,#27690,#977,.T.);
#34937=EDGE_CURVE('',#27691,#27691,#978,.T.);
#34938=EDGE_CURVE('',#27691,#27692,#14044,.T.);
#34939=EDGE_CURVE('',#27692,#27692,#979,.T.);
#34940=EDGE_CURVE('',#27693,#27693,#980,.T.);
#34941=EDGE_CURVE('',#27694,#27694,#981,.T.);
#34942=EDGE_CURVE('',#27694,#27695,#14045,.T.);
#34943=EDGE_CURVE('',#27695,#27695,#982,.T.);
#34944=EDGE_CURVE('',#27696,#27696,#983,.T.);
#34945=EDGE_CURVE('',#27697,#27697,#984,.T.);
#34946=EDGE_CURVE('',#27697,#27698,#14046,.T.);
#34947=EDGE_CURVE('',#27698,#27698,#985,.T.);
#34948=EDGE_CURVE('',#27699,#27699,#986,.T.);
#34949=EDGE_CURVE('',#27700,#27700,#987,.T.);
#34950=EDGE_CURVE('',#27700,#27701,#14047,.T.);
#34951=EDGE_CURVE('',#27701,#27701,#988,.T.);
#34952=EDGE_CURVE('',#27702,#27702,#989,.T.);
#34953=EDGE_CURVE('',#27666,#27703,#14048,.T.);
#34954=EDGE_CURVE('',#27703,#27703,#990,.T.);
#34955=EDGE_CURVE('',#27704,#27632,#14049,.T.);
#34956=EDGE_CURVE('',#27661,#27704,#14050,.T.);
#34957=EDGE_CURVE('',#27705,#27705,#991,.T.);
#34958=EDGE_CURVE('',#27706,#27706,#992,.T.);
#34959=EDGE_CURVE('',#27707,#27707,#993,.T.);
#34960=EDGE_CURVE('',#27703,#27702,#14051,.T.);
#34961=EDGE_CURVE('',#27664,#27708,#14052,.T.);
#34962=EDGE_CURVE('',#27708,#27708,#994,.T.);
#34963=EDGE_CURVE('',#27708,#27699,#14053,.T.);
#34964=EDGE_CURVE('',#27707,#27709,#14054,.T.);
#34965=EDGE_CURVE('',#27709,#27709,#995,.T.);
#34966=EDGE_CURVE('',#27709,#27696,#14055,.T.);
#34967=EDGE_CURVE('',#27665,#27710,#14056,.T.);
#34968=EDGE_CURVE('',#27710,#27710,#996,.T.);
#34969=EDGE_CURVE('',#27710,#27693,#14057,.T.);
#34970=EDGE_CURVE('',#27706,#27711,#14058,.T.);
#34971=EDGE_CURVE('',#27711,#27711,#997,.T.);
#34972=EDGE_CURVE('',#27711,#27690,#14059,.T.);
#34973=EDGE_CURVE('',#27705,#27712,#14060,.T.);
#34974=EDGE_CURVE('',#27712,#27712,#998,.T.);
#34975=EDGE_CURVE('',#27712,#27687,#14061,.T.);
#34976=EDGE_CURVE('',#27713,#27714,#14062,.T.);
#34977=EDGE_CURVE('',#27714,#27715,#587,.T.);
#34978=EDGE_CURVE('',#27715,#27716,#14063,.T.);
#34979=EDGE_CURVE('',#27716,#27713,#14064,.T.);
#34980=EDGE_CURVE('',#27716,#27717,#14065,.T.);
#34981=EDGE_CURVE('',#27717,#27718,#14066,.T.);
#34982=EDGE_CURVE('',#27718,#27713,#14067,.T.);
#34983=EDGE_CURVE('',#27717,#27719,#14068,.T.);
#34984=EDGE_CURVE('',#27719,#27720,#14069,.T.);
#34985=EDGE_CURVE('',#27720,#27718,#14070,.T.);
#34986=EDGE_CURVE('',#27721,#27722,#14071,.T.);
#34987=EDGE_CURVE('',#27722,#27723,#14072,.T.);
#34988=EDGE_CURVE('',#27723,#27676,#14073,.T.);
#34989=EDGE_CURVE('',#27676,#27721,#14074,.T.);
#34990=EDGE_CURVE('',#27722,#27724,#14075,.T.);
#34991=EDGE_CURVE('',#27724,#27725,#14076,.T.);
#34992=EDGE_CURVE('',#27725,#27723,#14077,.T.);
#34993=EDGE_CURVE('',#27724,#27726,#14078,.T.);
#34994=EDGE_CURVE('',#27726,#27727,#14079,.T.);
#34995=EDGE_CURVE('',#27727,#27725,#14080,.T.);
#34996=EDGE_CURVE('',#27726,#27728,#14081,.T.);
#34997=EDGE_CURVE('',#27728,#27729,#588,.T.);
#34998=EDGE_CURVE('',#27729,#27727,#14082,.T.);
#34999=EDGE_CURVE('',#27730,#27721,#14083,.T.);
#35000=EDGE_CURVE('',#27677,#27730,#14084,.T.);
#35001=EDGE_CURVE('',#27719,#27730,#14085,.T.);
#35002=EDGE_CURVE('',#27677,#27720,#14086,.T.);
#35003=EDGE_CURVE('',#27731,#27714,#14087,.T.);
#35004=EDGE_CURVE('',#27644,#27731,#589,.T.);
#35005=EDGE_CURVE('',#27732,#27643,#590,.T.);
#35006=EDGE_CURVE('',#27733,#27732,#14088,.T.);
#35007=EDGE_CURVE('',#27734,#27733,#591,.T.);
#35008=EDGE_CURVE('',#27715,#27734,#999,.T.);
#35009=EDGE_CURVE('',#27735,#27713,#14089,.T.);
#35010=EDGE_CURVE('',#27731,#27735,#14090,.T.);
#35011=EDGE_CURVE('',#27718,#27736,#14091,.T.);
#35012=EDGE_CURVE('',#27735,#27736,#14092,.T.);
#35013=EDGE_CURVE('',#27720,#27737,#14093,.T.);
#35014=EDGE_CURVE('',#27736,#27737,#14094,.T.);
#35015=EDGE_CURVE('',#27737,#27679,#14095,.T.);
#35016=EDGE_CURVE('',#27738,#27723,#14096,.T.);
#35017=EDGE_CURVE('',#27678,#27738,#14097,.T.);
#35018=EDGE_CURVE('',#27739,#27740,#14098,.T.);
#35019=EDGE_CURVE('',#27740,#27741,#592,.T.);
#35020=EDGE_CURVE('',#27741,#27742,#14099,.T.);
#35021=EDGE_CURVE('',#27742,#27739,#14100,.T.);
#35022=EDGE_CURVE('',#27742,#27743,#14101,.T.);
#35023=EDGE_CURVE('',#27743,#27744,#14102,.T.);
#35024=EDGE_CURVE('',#27744,#27739,#14103,.T.);
#35025=EDGE_CURVE('',#27743,#27745,#14104,.T.);
#35026=EDGE_CURVE('',#27745,#27746,#14105,.T.);
#35027=EDGE_CURVE('',#27746,#27744,#14106,.T.);
#35028=EDGE_CURVE('',#27745,#27662,#14107,.T.);
#35029=EDGE_CURVE('',#27661,#27746,#14108,.T.);
#35030=EDGE_CURVE('',#27659,#27747,#14109,.T.);
#35031=EDGE_CURVE('',#27747,#27748,#14110,.T.);
#35032=EDGE_CURVE('',#27748,#27660,#14111,.T.);
#35033=EDGE_CURVE('',#27747,#27749,#14112,.T.);
#35034=EDGE_CURVE('',#27749,#27750,#14113,.T.);
#35035=EDGE_CURVE('',#27750,#27748,#14114,.T.);
#35036=EDGE_CURVE('',#27749,#27751,#14115,.T.);
#35037=EDGE_CURVE('',#27751,#27752,#14116,.T.);
#35038=EDGE_CURVE('',#27752,#27750,#14117,.T.);
#35039=EDGE_CURVE('',#27751,#27734,#14118,.T.);
#35040=EDGE_CURVE('',#27733,#27752,#14119,.T.);
#35041=EDGE_CURVE('',#27753,#27739,#14120,.T.);
#35042=EDGE_CURVE('',#27754,#27753,#14121,.T.);
#35043=EDGE_CURVE('',#27754,#27740,#14122,.T.);
#35044=EDGE_CURVE('',#27744,#27755,#14123,.T.);
#35045=EDGE_CURVE('',#27753,#27755,#14124,.T.);
#35046=EDGE_CURVE('',#27756,#27746,#14125,.T.);
#35047=EDGE_CURVE('',#27755,#27756,#14126,.T.);
#35048=EDGE_CURVE('',#27756,#27704,#14127,.T.);
#35049=EDGE_CURVE('',#27748,#27757,#14128,.T.);
#35050=EDGE_CURVE('',#27663,#27757,#14129,.T.);
#35051=EDGE_CURVE('',#27758,#27750,#14130,.T.);
#35052=EDGE_CURVE('',#27757,#27758,#14131,.T.);
#35053=EDGE_CURVE('',#27752,#27759,#14132,.T.);
#35054=EDGE_CURVE('',#27758,#27759,#14133,.T.);
#35055=EDGE_CURVE('',#27759,#27732,#14134,.T.);
#35056=EDGE_CURVE('',#27760,#27761,#14135,.T.);
#35057=EDGE_CURVE('',#27761,#27653,#593,.T.);
#35058=EDGE_CURVE('',#27652,#27760,#14136,.T.);
#35059=EDGE_CURVE('',#27651,#27762,#14137,.T.);
#35060=EDGE_CURVE('',#27762,#27760,#14138,.T.);
#35061=EDGE_CURVE('',#27650,#27738,#14139,.T.);
#35062=EDGE_CURVE('',#27738,#27762,#14140,.T.);
#35063=EDGE_CURVE('',#27649,#27678,#14141,.T.);
#35064=EDGE_CURVE('',#27648,#27679,#14142,.T.);
#35065=EDGE_CURVE('',#27647,#27737,#14143,.T.);
#35066=EDGE_CURVE('',#27646,#27736,#14144,.T.);
#35067=EDGE_CURVE('',#27645,#27735,#14145,.T.);
#35068=EDGE_CURVE('',#27642,#27759,#14146,.T.);
#35069=EDGE_CURVE('',#27641,#27758,#14147,.T.);
#35070=EDGE_CURVE('',#27640,#27757,#14148,.T.);
#35071=EDGE_CURVE('',#27658,#27704,#14149,.T.);
#35072=EDGE_CURVE('',#27657,#27756,#14150,.T.);
#35073=EDGE_CURVE('',#27656,#27755,#14151,.T.);
#35074=EDGE_CURVE('',#27655,#27753,#14152,.T.);
#35075=EDGE_CURVE('',#27654,#27754,#594,.T.);
#35076=EDGE_CURVE('',#27741,#27728,#1000,.T.);
#35077=EDGE_CURVE('',#27762,#27725,#14153,.T.);
#35078=EDGE_CURVE('',#27729,#27761,#14154,.T.);
#35079=EDGE_CURVE('',#27727,#27760,#14155,.T.);
#35080=EDGE_CURVE('',#27763,#27764,#14156,.T.);
#35081=EDGE_CURVE('',#27763,#27765,#1001,.T.);
#35082=EDGE_CURVE('',#27765,#27766,#142,.T.);
#35083=EDGE_CURVE('',#27766,#27764,#1002,.T.);
#35084=EDGE_CURVE('',#27767,#27768,#1003,.T.);
#35085=EDGE_CURVE('',#27768,#27769,#14157,.T.);
#35086=EDGE_CURVE('',#27769,#27769,#1004,.T.);
#35087=EDGE_CURVE('',#27768,#27767,#1005,.T.);
#35088=EDGE_CURVE('',#27770,#27771,#14158,.T.);
#35089=EDGE_CURVE('',#27772,#27770,#14159,.T.);
#35090=EDGE_CURVE('',#27773,#27772,#1006,.T.);
#35091=EDGE_CURVE('',#27772,#27773,#1007,.T.);
#35092=EDGE_CURVE('',#27767,#27772,#14160,.T.);
#35093=EDGE_CURVE('',#27774,#27767,#14161,.T.);
#35094=EDGE_CURVE('',#27775,#27774,#14162,.T.);
#35095=EDGE_CURVE('',#27771,#27775,#14163,.T.);
#35096=EDGE_CURVE('',#27776,#27776,#1008,.T.);
#35097=EDGE_CURVE('',#27769,#27777,#14164,.T.);
#35098=EDGE_CURVE('',#27777,#27777,#1009,.T.);
#35099=EDGE_CURVE('',#27773,#27778,#14165,.T.);
#35100=EDGE_CURVE('',#27778,#27778,#1010,.T.);
#35101=EDGE_CURVE('',#27778,#27779,#14166,.T.);
#35102=EDGE_CURVE('',#27779,#27779,#1011,.T.);
#35103=EDGE_CURVE('',#27780,#27777,#14167,.T.);
#35104=EDGE_CURVE('',#27781,#27779,#14168,.T.);
#35105=EDGE_CURVE('',#27782,#27783,#143,.T.);
#35106=EDGE_CURVE('',#27783,#27784,#1012,.T.);
#35107=EDGE_CURVE('',#27784,#27785,#14169,.T.);
#35108=EDGE_CURVE('',#27785,#27785,#1013,.T.);
#35109=EDGE_CURVE('',#27784,#27782,#1014,.T.);
#35110=EDGE_CURVE('',#27782,#27786,#14170,.T.);
#35111=EDGE_CURVE('',#27786,#27787,#14171,.T.);
#35112=EDGE_CURVE('',#27787,#27788,#14172,.T.);
#35113=EDGE_CURVE('',#27788,#27789,#14173,.T.);
#35114=EDGE_CURVE('',#27789,#27790,#14174,.T.);
#35115=EDGE_CURVE('',#27791,#27790,#144,.T.);
#35116=EDGE_CURVE('',#27791,#27792,#14175,.T.);
#35117=EDGE_CURVE('',#27766,#27792,#145,.T.);
#35118=EDGE_CURVE('',#27765,#27783,#14176,.T.);
#35119=EDGE_CURVE('',#27785,#27793,#14177,.T.);
#35120=EDGE_CURVE('',#27793,#27793,#595,.T.);
#35121=EDGE_CURVE('',#27790,#27794,#1015,.T.);
#35122=EDGE_CURVE('',#27794,#27795,#14178,.T.);
#35123=EDGE_CURVE('',#27795,#27795,#1016,.T.);
#35124=EDGE_CURVE('',#27794,#27791,#1017,.T.);
#35125=EDGE_CURVE('',#27795,#27796,#14179,.T.);
#35126=EDGE_CURVE('',#27796,#27796,#596,.T.);
#35127=EDGE_CURVE('',#27764,#27766,#1018,.T.);
#35128=EDGE_CURVE('',#27792,#27763,#1019,.T.);
#35129=EDGE_CURVE('',#27764,#27797,#14180,.T.);
#35130=EDGE_CURVE('',#27797,#27797,#597,.T.);
#35131=EDGE_CURVE('',#27798,#27789,#14181,.T.);
#35132=EDGE_CURVE('',#27799,#27798,#14182,.T.);
#35133=EDGE_CURVE('',#27786,#27799,#14183,.T.);
#35134=EDGE_CURVE('',#27800,#27801,#146,.T.);
#35135=EDGE_CURVE('',#27801,#27802,#1020,.T.);
#35136=EDGE_CURVE('',#27802,#27803,#14184,.T.);
#35137=EDGE_CURVE('',#27803,#27803,#1021,.T.);
#35138=EDGE_CURVE('',#27802,#27800,#1022,.T.);
#35139=EDGE_CURVE('',#27800,#27804,#14185,.T.);
#35140=EDGE_CURVE('',#27804,#27771,#14186,.T.);
#35141=EDGE_CURVE('',#27775,#27805,#14187,.T.);
#35142=EDGE_CURVE('',#27805,#27801,#14188,.T.);
#35143=EDGE_CURVE('',#27803,#27806,#14189,.T.);
#35144=EDGE_CURVE('',#27806,#27807,#1023,.T.);
#35145=EDGE_CURVE('',#27807,#27808,#1024,.T.);
#35146=EDGE_CURVE('',#27808,#27806,#1025,.T.);
#35147=EDGE_CURVE('',#27809,#27809,#1026,.T.);
#35148=EDGE_CURVE('',#27809,#27810,#14190,.T.);
#35149=EDGE_CURVE('',#27810,#27810,#1027,.T.);
#35150=EDGE_CURVE('',#27811,#27805,#14191,.T.);
#35151=EDGE_CURVE('',#27812,#27811,#14192,.T.);
#35152=EDGE_CURVE('',#27804,#27812,#14193,.T.);
#35153=EDGE_CURVE('',#27813,#27813,#1028,.T.);
#35154=EDGE_CURVE('',#27814,#27814,#1029,.T.);
#35155=EDGE_CURVE('',#27815,#27815,#1030,.T.);
#35156=EDGE_CURVE('',#27816,#27816,#1031,.T.);
#35157=EDGE_CURVE('',#27817,#27817,#1032,.T.);
#35158=EDGE_CURVE('',#27810,#27818,#14194,.T.);
#35159=EDGE_CURVE('',#27818,#27819,#1033,.T.);
#35160=EDGE_CURVE('',#27819,#27820,#1034,.T.);
#35161=EDGE_CURVE('',#27820,#27818,#1035,.T.);
#35162=EDGE_CURVE('',#27813,#27821,#14195,.T.);
#35163=EDGE_CURVE('',#27821,#27821,#1036,.T.);
#35164=EDGE_CURVE('',#27821,#27822,#14196,.T.);
#35165=EDGE_CURVE('',#27822,#27823,#1037,.T.);
#35166=EDGE_CURVE('',#27823,#27824,#1038,.T.);
#35167=EDGE_CURVE('',#27824,#27822,#1039,.T.);
#35168=EDGE_CURVE('',#27823,#27824,#14197,.T.);
#35169=EDGE_CURVE('',#27823,#27824,#14198,.T.);
#35170=EDGE_CURVE('',#27819,#27820,#14199,.T.);
#35171=EDGE_CURVE('',#27819,#27820,#14200,.T.);
#35172=EDGE_CURVE('',#27807,#27808,#14201,.T.);
#35173=EDGE_CURVE('',#27807,#27808,#14202,.T.);
#35174=EDGE_CURVE('',#27814,#27825,#14203,.T.);
#35175=EDGE_CURVE('',#27825,#27825,#1040,.T.);
#35176=EDGE_CURVE('',#27825,#27826,#14204,.T.);
#35177=EDGE_CURVE('',#27826,#27826,#1041,.T.);
#35178=EDGE_CURVE('',#27817,#27827,#14205,.T.);
#35179=EDGE_CURVE('',#27827,#27827,#1042,.T.);
#35180=EDGE_CURVE('',#27827,#27828,#14206,.T.);
#35181=EDGE_CURVE('',#27828,#27828,#1043,.T.);
#35182=EDGE_CURVE('',#27815,#27829,#14207,.T.);
#35183=EDGE_CURVE('',#27829,#27829,#1044,.T.);
#35184=EDGE_CURVE('',#27829,#27830,#14208,.T.);
#35185=EDGE_CURVE('',#27830,#27830,#1045,.T.);
#35186=EDGE_CURVE('',#27816,#27831,#14209,.T.);
#35187=EDGE_CURVE('',#27831,#27831,#1046,.T.);
#35188=EDGE_CURVE('',#27831,#27832,#14210,.T.);
#35189=EDGE_CURVE('',#27832,#27832,#1047,.T.);
#35190=EDGE_CURVE('',#27826,#27833,#14211,.T.);
#35191=EDGE_CURVE('',#27832,#27834,#14212,.T.);
#35192=EDGE_CURVE('',#27830,#27835,#14213,.T.);
#35193=EDGE_CURVE('',#27828,#27836,#14214,.T.);
#35194=EDGE_CURVE('',#27776,#27837,#14215,.T.);
#35195=EDGE_CURVE('',#27837,#27838,#1048,.T.);
#35196=EDGE_CURVE('',#27838,#27837,#1049,.T.);
#35197=EDGE_CURVE('',#27838,#27808,#14216,.T.);
#35198=EDGE_CURVE('',#27807,#27820,#14217,.T.);
#35199=EDGE_CURVE('',#27819,#27824,#14218,.T.);
#35200=EDGE_CURVE('',#27823,#27839,#14219,.T.);
#35201=EDGE_CURVE('',#27839,#27840,#1050,.T.);
#35202=EDGE_CURVE('',#27841,#27840,#14220,.T.);
#35203=EDGE_CURVE('',#27842,#27841,#1051,.T.);
#35204=EDGE_CURVE('',#27843,#27842,#14221,.T.);
#35205=EDGE_CURVE('',#27843,#27839,#1052,.T.);
#35206=EDGE_CURVE('',#27844,#27845,#14222,.T.);
#35207=EDGE_CURVE('',#27845,#27845,#1053,.T.);
#35208=EDGE_CURVE('',#27846,#27846,#1054,.T.);
#35209=EDGE_CURVE('',#27846,#27845,#14223,.T.);
#35210=EDGE_CURVE('',#27840,#27843,#14224,.T.);
#35211=EDGE_CURVE('',#27847,#27842,#14225,.T.);
#35212=EDGE_CURVE('',#27848,#27847,#14226,.T.);
#35213=EDGE_CURVE('',#27848,#27849,#14227,.T.);
#35214=EDGE_CURVE('',#27850,#27849,#14228,.T.);
#35215=EDGE_CURVE('',#27841,#27850,#14229,.T.);
#35216=EDGE_CURVE('',#27851,#27852,#14230,.T.);
#35217=EDGE_CURVE('',#27849,#27851,#14231,.T.);
#35218=EDGE_CURVE('',#27852,#27848,#14232,.T.);
#35219=EDGE_CURVE('',#27853,#27850,#14233,.T.);
#35220=EDGE_CURVE('',#27854,#27853,#14234,.T.);
#35221=EDGE_CURVE('',#27847,#27854,#14235,.T.);
#35222=EDGE_CURVE('',#27854,#27855,#14236,.T.);
#35223=EDGE_CURVE('',#27855,#27856,#14237,.T.);
#35224=EDGE_CURVE('',#27857,#27856,#14238,.T.);
#35225=EDGE_CURVE('',#27858,#27857,#14239,.T.);
#35226=EDGE_CURVE('',#27859,#27858,#14240,.T.);
#35227=EDGE_CURVE('',#27860,#27859,#14241,.T.);
#35228=EDGE_CURVE('',#27861,#27860,#14242,.T.);
#35229=EDGE_CURVE('',#27861,#27862,#14243,.T.);
#35230=EDGE_CURVE('',#27862,#27852,#14244,.T.);
#35231=EDGE_CURVE('',#27863,#27853,#14245,.T.);
#35232=EDGE_CURVE('',#27855,#27863,#14246,.T.);
#35233=EDGE_CURVE('',#27856,#27864,#14247,.T.);
#35234=EDGE_CURVE('',#27865,#27863,#14248,.T.);
#35235=EDGE_CURVE('',#27866,#27865,#14249,.T.);
#35236=EDGE_CURVE('',#27864,#27866,#14250,.T.);
#35237=EDGE_CURVE('',#27867,#27861,#14251,.T.);
#35238=EDGE_CURVE('',#27868,#27867,#14252,.T.);
#35239=EDGE_CURVE('',#27869,#27868,#14253,.T.);
#35240=EDGE_CURVE('',#27870,#27869,#14254,.T.);
#35241=EDGE_CURVE('',#27862,#27870,#14255,.T.);
#35242=EDGE_CURVE('',#27851,#27870,#14256,.T.);
#35243=EDGE_CURVE('',#27864,#27871,#14257,.T.);
#35244=EDGE_CURVE('',#27871,#27857,#14258,.T.);
#35245=EDGE_CURVE('',#27860,#27788,#14259,.T.);
#35246=EDGE_CURVE('',#27788,#27867,#14260,.T.);
#35247=EDGE_CURVE('',#27872,#27866,#14261,.T.);
#35248=EDGE_CURVE('',#27871,#27872,#14262,.T.);
#35249=EDGE_CURVE('',#27865,#27873,#14263,.T.);
#35250=EDGE_CURVE('',#27873,#27872,#14264,.T.);
#35251=EDGE_CURVE('',#27774,#27873,#14265,.T.);
#35252=EDGE_CURVE('',#27872,#27774,#14266,.T.);
#35253=EDGE_CURVE('',#27805,#27874,#14267,.T.);
#35254=EDGE_CURVE('',#27874,#27775,#14268,.T.);
#35255=EDGE_CURVE('',#27770,#27871,#14269,.T.);
#35256=EDGE_CURVE('',#27857,#27770,#14270,.T.);
#35257=EDGE_CURVE('',#27787,#27875,#14271,.T.);
#35258=EDGE_CURVE('',#27875,#27786,#14272,.T.);
#35259=EDGE_CURVE('',#27858,#27804,#14273,.T.);
#35260=EDGE_CURVE('',#27771,#27858,#14274,.T.);
#35261=EDGE_CURVE('',#27799,#27876,#14275,.T.);
#35262=EDGE_CURVE('',#27811,#27799,#14276,.T.);
#35263=EDGE_CURVE('',#27876,#27811,#14277,.T.);
#35264=EDGE_CURVE('',#27789,#27860,#14278,.T.);
#35265=EDGE_CURVE('',#27859,#27798,#14279,.T.);
#35266=EDGE_CURVE('',#27812,#27859,#14280,.T.);
#35267=EDGE_CURVE('',#27798,#27812,#14281,.T.);
#35268=EDGE_CURVE('',#27874,#27876,#14282,.T.);
#35269=EDGE_CURVE('',#27876,#27875,#14283,.T.);
#35270=EDGE_CURVE('',#27868,#27787,#14284,.T.);
#35271=EDGE_CURVE('',#27875,#27869,#14285,.T.);
#35272=EDGE_CURVE('',#27873,#27874,#14286,.T.);
#35273=EDGE_CURVE('',#27877,#27877,#598,.T.);
#35274=EDGE_CURVE('',#27877,#27878,#14287,.T.);
#35275=EDGE_CURVE('',#27879,#27879,#599,.T.);
#35276=EDGE_CURVE('',#27879,#27880,#14288,.T.);
#35277=EDGE_CURVE('',#27881,#27881,#600,.T.);
#35278=EDGE_CURVE('',#27881,#27882,#14289,.T.);
#35279=EDGE_CURVE('',#27883,#27884,#14290,.T.);
#35280=EDGE_CURVE('',#27884,#27885,#14291,.T.);
#35281=EDGE_CURVE('',#27885,#27886,#14292,.T.);
#35282=EDGE_CURVE('',#27883,#27886,#14293,.T.);
#35283=EDGE_CURVE('',#27884,#27887,#14294,.T.);
#35284=EDGE_CURVE('',#27887,#27888,#14295,.T.);
#35285=EDGE_CURVE('',#27888,#27885,#14296,.T.);
#35286=EDGE_CURVE('',#27887,#27889,#14297,.T.);
#35287=EDGE_CURVE('',#27889,#27890,#14298,.T.);
#35288=EDGE_CURVE('',#27890,#27888,#14299,.T.);
#35289=EDGE_CURVE('',#27886,#27890,#14300,.T.);
#35290=EDGE_CURVE('',#27889,#27883,#14301,.T.);
#35291=EDGE_CURVE('',#27891,#27886,#14302,.T.);
#35292=EDGE_CURVE('',#27892,#27891,#14303,.T.);
#35293=EDGE_CURVE('',#27892,#27890,#14304,.T.);
#35294=EDGE_CURVE('',#27893,#27885,#14305,.T.);
#35295=EDGE_CURVE('',#27891,#27893,#14306,.T.);
#35296=EDGE_CURVE('',#27894,#27895,#14307,.T.);
#35297=EDGE_CURVE('',#27895,#27891,#14308,.T.);
#35298=EDGE_CURVE('',#27894,#27893,#14309,.T.);
#35299=EDGE_CURVE('',#27895,#27896,#14310,.T.);
#35300=EDGE_CURVE('',#27896,#27892,#14311,.T.);
#35301=EDGE_CURVE('',#27893,#27897,#14312,.T.);
#35302=EDGE_CURVE('',#27897,#27898,#14313,.T.);
#35303=EDGE_CURVE('',#27898,#27894,#14314,.T.);
#35304=EDGE_CURVE('',#27896,#27898,#14315,.T.);
#35305=EDGE_CURVE('',#27897,#27892,#14316,.T.);
#35306=EDGE_CURVE('',#27897,#27888,#14317,.T.);
#35307=EDGE_CURVE('',#27899,#27900,#1055,.T.);
#35308=EDGE_CURVE('',#27899,#27900,#14318,.T.);
#35309=EDGE_CURVE('',#27901,#27902,#1056,.T.);
#35310=EDGE_CURVE('',#27901,#27902,#14319,.T.);
#35311=EDGE_CURVE('',#27902,#27899,#14320,.T.);
#35312=EDGE_CURVE('',#27900,#27901,#14321,.T.);
#35313=EDGE_CURVE('',#27903,#27904,#1057,.T.);
#35314=EDGE_CURVE('',#27903,#27904,#14322,.T.);
#35315=EDGE_CURVE('',#27905,#27906,#1058,.T.);
#35316=EDGE_CURVE('',#27905,#27906,#14323,.T.);
#35317=EDGE_CURVE('',#27906,#27903,#14324,.T.);
#35318=EDGE_CURVE('',#27904,#27905,#14325,.T.);
#35319=EDGE_CURVE('',#27907,#27907,#1059,.T.);
#35320=EDGE_CURVE('',#27908,#27908,#1060,.T.);
#35321=EDGE_CURVE('',#27908,#27907,#14326,.T.);
#35322=EDGE_CURVE('',#27909,#27909,#1061,.T.);
#35323=EDGE_CURVE('',#27909,#27908,#14327,.T.);
#35324=EDGE_CURVE('',#27910,#27910,#1062,.T.);
#35325=EDGE_CURVE('',#27910,#27909,#14328,.T.);
#35326=EDGE_CURVE('',#27911,#27912,#14329,.T.);
#35327=EDGE_CURVE('',#27912,#27911,#1063,.T.);
#35328=EDGE_CURVE('',#27913,#27914,#24340,.T.);
#35329=EDGE_CURVE('',#27915,#27913,#24341,.T.);
#35330=EDGE_CURVE('',#27914,#27915,#24342,.T.);
#35331=EDGE_CURVE('',#27914,#27916,#14330,.T.);
#35332=EDGE_CURVE('',#27916,#27917,#1064,.T.);
#35333=EDGE_CURVE('',#27912,#27917,#24343,.T.);
#35334=EDGE_CURVE('',#27918,#27911,#24344,.T.);
#35335=EDGE_CURVE('',#27918,#27916,#1065,.T.);
#35336=EDGE_CURVE('',#27917,#27918,#14331,.T.);
#35337=EDGE_CURVE('',#27919,#27920,#14332,.T.);
#35338=EDGE_CURVE('',#27921,#27919,#14333,.T.);
#35339=EDGE_CURVE('',#27921,#27922,#14334,.T.);
#35340=EDGE_CURVE('',#27920,#27922,#14335,.T.);
#35341=EDGE_CURVE('',#27923,#27924,#14336,.T.);
#35342=EDGE_CURVE('',#27925,#27923,#14337,.T.);
#35343=EDGE_CURVE('',#27926,#27925,#14338,.T.);
#35344=EDGE_CURVE('',#27924,#27926,#14339,.T.);
#35345=EDGE_CURVE('',#27926,#27927,#147,.T.);
#35346=EDGE_CURVE('',#27928,#27925,#148,.T.);
#35347=EDGE_CURVE('',#27927,#27928,#14340,.T.);
#35348=EDGE_CURVE('',#27927,#27929,#1066,.T.);
#35349=EDGE_CURVE('',#27930,#27928,#1067,.T.);
#35350=EDGE_CURVE('',#27929,#27930,#14341,.T.);
#35351=EDGE_CURVE('',#27921,#27929,#149,.T.);
#35352=EDGE_CURVE('',#27922,#27930,#150,.T.);
#35353=EDGE_CURVE('',#27924,#27919,#1068,.T.);
#35354=EDGE_CURVE('',#27931,#27931,#1069,.T.);
#35355=EDGE_CURVE('',#27931,#27932,#14342,.T.);
#35356=EDGE_CURVE('',#27932,#27933,#1070,.T.);
#35357=EDGE_CURVE('',#27933,#27934,#14343,.T.);
#35358=EDGE_CURVE('',#27934,#27935,#1071,.T.);
#35359=EDGE_CURVE('',#27935,#27936,#14344,.T.);
#35360=EDGE_CURVE('',#27936,#27937,#1072,.T.);
#35361=EDGE_CURVE('',#27937,#27938,#14345,.T.);
#35362=EDGE_CURVE('',#27938,#27939,#1073,.T.);
#35363=EDGE_CURVE('',#27939,#27940,#14346,.T.);
#35364=EDGE_CURVE('',#27940,#27941,#1074,.T.);
#35365=EDGE_CURVE('',#27941,#27942,#14347,.T.);
#35366=EDGE_CURVE('',#27942,#27923,#1075,.T.);
#35367=EDGE_CURVE('',#27920,#27943,#1076,.T.);
#35368=EDGE_CURVE('',#27943,#27944,#14348,.T.);
#35369=EDGE_CURVE('',#27944,#27945,#1077,.T.);
#35370=EDGE_CURVE('',#27945,#27946,#14349,.T.);
#35371=EDGE_CURVE('',#27946,#27947,#1078,.T.);
#35372=EDGE_CURVE('',#27947,#27948,#14350,.T.);
#35373=EDGE_CURVE('',#27948,#27949,#1079,.T.);
#35374=EDGE_CURVE('',#27949,#27950,#14351,.T.);
#35375=EDGE_CURVE('',#27950,#27951,#1080,.T.);
#35376=EDGE_CURVE('',#27951,#27952,#14352,.T.);
#35377=EDGE_CURVE('',#27952,#27953,#1081,.T.);
#35378=EDGE_CURVE('',#27953,#27954,#14353,.T.);
#35379=EDGE_CURVE('',#27954,#27955,#1082,.T.);
#35380=EDGE_CURVE('',#27955,#27956,#14354,.T.);
#35381=EDGE_CURVE('',#27956,#27957,#1083,.T.);
#35382=EDGE_CURVE('',#27957,#27958,#14355,.T.);
#35383=EDGE_CURVE('',#27958,#27959,#1084,.T.);
#35384=EDGE_CURVE('',#27959,#27960,#14356,.T.);
#35385=EDGE_CURVE('',#27960,#27961,#1085,.T.);
#35386=EDGE_CURVE('',#27961,#27962,#14357,.T.);
#35387=EDGE_CURVE('',#27962,#27963,#1086,.T.);
#35388=EDGE_CURVE('',#27963,#27964,#14358,.T.);
#35389=EDGE_CURVE('',#27964,#27965,#1087,.T.);
#35390=EDGE_CURVE('',#27965,#27966,#14359,.T.);
#35391=EDGE_CURVE('',#27966,#27967,#1088,.T.);
#35392=EDGE_CURVE('',#27967,#27968,#14360,.T.);
#35393=EDGE_CURVE('',#27968,#27969,#1089,.T.);
#35394=EDGE_CURVE('',#27969,#27970,#14361,.T.);
#35395=EDGE_CURVE('',#27970,#27971,#1090,.T.);
#35396=EDGE_CURVE('',#27971,#27972,#14362,.T.);
#35397=EDGE_CURVE('',#27972,#27973,#1091,.T.);
#35398=EDGE_CURVE('',#27973,#27974,#14363,.T.);
#35399=EDGE_CURVE('',#27974,#27975,#1092,.T.);
#35400=EDGE_CURVE('',#27975,#27976,#14364,.T.);
#35401=EDGE_CURVE('',#27976,#27977,#1093,.T.);
#35402=EDGE_CURVE('',#27977,#27978,#14365,.T.);
#35403=EDGE_CURVE('',#27978,#27979,#1094,.T.);
#35404=EDGE_CURVE('',#27979,#27980,#14366,.T.);
#35405=EDGE_CURVE('',#27980,#27981,#1095,.T.);
#35406=EDGE_CURVE('',#27981,#27982,#14367,.T.);
#35407=EDGE_CURVE('',#27982,#27983,#1096,.T.);
#35408=EDGE_CURVE('',#27983,#27984,#14368,.T.);
#35409=EDGE_CURVE('',#27984,#27985,#1097,.T.);
#35410=EDGE_CURVE('',#27985,#27986,#14369,.T.);
#35411=EDGE_CURVE('',#27986,#27987,#1098,.T.);
#35412=EDGE_CURVE('',#27987,#27988,#14370,.T.);
#35413=EDGE_CURVE('',#27988,#27989,#1099,.T.);
#35414=EDGE_CURVE('',#27989,#27990,#14371,.T.);
#35415=EDGE_CURVE('',#27990,#27991,#1100,.T.);
#35416=EDGE_CURVE('',#27991,#27992,#14372,.T.);
#35417=EDGE_CURVE('',#27992,#27932,#1101,.T.);
#35418=EDGE_CURVE('',#27993,#27941,#14373,.T.);
#35419=EDGE_CURVE('',#27993,#27994,#14374,.T.);
#35420=EDGE_CURVE('',#27942,#27994,#14375,.T.);
#35421=EDGE_CURVE('',#27995,#27939,#14376,.T.);
#35422=EDGE_CURVE('',#27996,#27995,#14377,.T.);
#35423=EDGE_CURVE('',#27940,#27996,#14378,.T.);
#35424=EDGE_CURVE('',#27996,#27997,#151,.T.);
#35425=EDGE_CURVE('',#27998,#27995,#152,.T.);
#35426=EDGE_CURVE('',#27997,#27998,#14379,.T.);
#35427=EDGE_CURVE('',#27997,#27999,#1102,.T.);
#35428=EDGE_CURVE('',#28000,#27998,#1103,.T.);
#35429=EDGE_CURVE('',#27999,#28000,#14380,.T.);
#35430=EDGE_CURVE('',#27993,#27999,#153,.T.);
#35431=EDGE_CURVE('',#27994,#28000,#154,.T.);
#35432=EDGE_CURVE('',#28001,#27937,#14381,.T.);
#35433=EDGE_CURVE('',#28001,#28002,#14382,.T.);
#35434=EDGE_CURVE('',#27938,#28002,#14383,.T.);
#35435=EDGE_CURVE('',#28003,#27935,#14384,.T.);
#35436=EDGE_CURVE('',#28004,#28003,#14385,.T.);
#35437=EDGE_CURVE('',#27936,#28004,#14386,.T.);
#35438=EDGE_CURVE('',#28004,#28005,#155,.T.);
#35439=EDGE_CURVE('',#28006,#28003,#156,.T.);
#35440=EDGE_CURVE('',#28005,#28006,#14387,.T.);
#35441=EDGE_CURVE('',#28005,#28007,#1104,.T.);
#35442=EDGE_CURVE('',#28008,#28006,#1105,.T.);
#35443=EDGE_CURVE('',#28007,#28008,#14388,.T.);
#35444=EDGE_CURVE('',#28001,#28007,#157,.T.);
#35445=EDGE_CURVE('',#28002,#28008,#158,.T.);
#35446=EDGE_CURVE('',#28009,#27933,#14389,.T.);
#35447=EDGE_CURVE('',#28009,#28010,#14390,.T.);
#35448=EDGE_CURVE('',#27934,#28010,#14391,.T.);
#35449=EDGE_CURVE('',#28011,#27991,#14392,.T.);
#35450=EDGE_CURVE('',#28012,#28011,#14393,.T.);
#35451=EDGE_CURVE('',#27992,#28012,#14394,.T.);
#35452=EDGE_CURVE('',#28012,#28013,#159,.T.);
#35453=EDGE_CURVE('',#28014,#28011,#160,.T.);
#35454=EDGE_CURVE('',#28013,#28014,#14395,.T.);
#35455=EDGE_CURVE('',#28013,#28015,#1106,.T.);
#35456=EDGE_CURVE('',#28016,#28014,#1107,.T.);
#35457=EDGE_CURVE('',#28015,#28016,#14396,.T.);
#35458=EDGE_CURVE('',#28009,#28015,#161,.T.);
#35459=EDGE_CURVE('',#28010,#28016,#162,.T.);
#35460=EDGE_CURVE('',#28017,#27989,#14397,.T.);
#35461=EDGE_CURVE('',#28017,#28018,#14398,.T.);
#35462=EDGE_CURVE('',#27990,#28018,#14399,.T.);
#35463=EDGE_CURVE('',#28019,#27987,#14400,.T.);
#35464=EDGE_CURVE('',#28020,#28019,#14401,.T.);
#35465=EDGE_CURVE('',#27988,#28020,#14402,.T.);
#35466=EDGE_CURVE('',#28020,#28021,#163,.T.);
#35467=EDGE_CURVE('',#28022,#28019,#164,.T.);
#35468=EDGE_CURVE('',#28021,#28022,#14403,.T.);
#35469=EDGE_CURVE('',#28021,#28023,#1108,.T.);
#35470=EDGE_CURVE('',#28024,#28022,#1109,.T.);
#35471=EDGE_CURVE('',#28023,#28024,#14404,.T.);
#35472=EDGE_CURVE('',#28017,#28023,#165,.T.);
#35473=EDGE_CURVE('',#28018,#28024,#166,.T.);
#35474=EDGE_CURVE('',#28025,#27985,#14405,.T.);
#35475=EDGE_CURVE('',#28025,#28026,#14406,.T.);
#35476=EDGE_CURVE('',#27986,#28026,#14407,.T.);
#35477=EDGE_CURVE('',#28027,#27983,#14408,.T.);
#35478=EDGE_CURVE('',#28028,#28027,#14409,.T.);
#35479=EDGE_CURVE('',#27984,#28028,#14410,.T.);
#35480=EDGE_CURVE('',#28028,#28029,#167,.T.);
#35481=EDGE_CURVE('',#28030,#28027,#168,.T.);
#35482=EDGE_CURVE('',#28029,#28030,#14411,.T.);
#35483=EDGE_CURVE('',#28029,#28031,#1110,.T.);
#35484=EDGE_CURVE('',#28032,#28030,#1111,.T.);
#35485=EDGE_CURVE('',#28031,#28032,#14412,.T.);
#35486=EDGE_CURVE('',#28025,#28031,#169,.T.);
#35487=EDGE_CURVE('',#28026,#28032,#170,.T.);
#35488=EDGE_CURVE('',#28033,#27981,#14413,.T.);
#35489=EDGE_CURVE('',#28033,#28034,#14414,.T.);
#35490=EDGE_CURVE('',#27982,#28034,#14415,.T.);
#35491=EDGE_CURVE('',#28035,#27979,#14416,.T.);
#35492=EDGE_CURVE('',#28036,#28035,#14417,.T.);
#35493=EDGE_CURVE('',#27980,#28036,#14418,.T.);
#35494=EDGE_CURVE('',#28036,#28037,#171,.T.);
#35495=EDGE_CURVE('',#28038,#28035,#172,.T.);
#35496=EDGE_CURVE('',#28037,#28038,#14419,.T.);
#35497=EDGE_CURVE('',#28037,#28039,#1112,.T.);
#35498=EDGE_CURVE('',#28040,#28038,#1113,.T.);
#35499=EDGE_CURVE('',#28039,#28040,#14420,.T.);
#35500=EDGE_CURVE('',#28033,#28039,#173,.T.);
#35501=EDGE_CURVE('',#28034,#28040,#174,.T.);
#35502=EDGE_CURVE('',#28041,#27977,#14421,.T.);
#35503=EDGE_CURVE('',#28041,#28042,#14422,.T.);
#35504=EDGE_CURVE('',#27978,#28042,#14423,.T.);
#35505=EDGE_CURVE('',#28043,#27975,#14424,.T.);
#35506=EDGE_CURVE('',#28044,#28043,#14425,.T.);
#35507=EDGE_CURVE('',#27976,#28044,#14426,.T.);
#35508=EDGE_CURVE('',#28044,#28045,#175,.T.);
#35509=EDGE_CURVE('',#28046,#28043,#176,.T.);
#35510=EDGE_CURVE('',#28045,#28046,#14427,.T.);
#35511=EDGE_CURVE('',#28045,#28047,#1114,.T.);
#35512=EDGE_CURVE('',#28048,#28046,#1115,.T.);
#35513=EDGE_CURVE('',#28047,#28048,#14428,.T.);
#35514=EDGE_CURVE('',#28041,#28047,#177,.T.);
#35515=EDGE_CURVE('',#28042,#28048,#178,.T.);
#35516=EDGE_CURVE('',#28049,#27973,#14429,.T.);
#35517=EDGE_CURVE('',#28049,#28050,#14430,.T.);
#35518=EDGE_CURVE('',#27974,#28050,#14431,.T.);
#35519=EDGE_CURVE('',#28051,#27971,#14432,.T.);
#35520=EDGE_CURVE('',#28052,#28051,#14433,.T.);
#35521=EDGE_CURVE('',#27972,#28052,#14434,.T.);
#35522=EDGE_CURVE('',#28052,#28053,#179,.T.);
#35523=EDGE_CURVE('',#28054,#28051,#180,.T.);
#35524=EDGE_CURVE('',#28053,#28054,#14435,.T.);
#35525=EDGE_CURVE('',#28053,#28055,#1116,.T.);
#35526=EDGE_CURVE('',#28056,#28054,#1117,.T.);
#35527=EDGE_CURVE('',#28055,#28056,#14436,.T.);
#35528=EDGE_CURVE('',#28049,#28055,#181,.T.);
#35529=EDGE_CURVE('',#28050,#28056,#182,.T.);
#35530=EDGE_CURVE('',#28057,#27969,#14437,.T.);
#35531=EDGE_CURVE('',#28057,#28058,#14438,.T.);
#35532=EDGE_CURVE('',#27970,#28058,#14439,.T.);
#35533=EDGE_CURVE('',#28059,#27967,#14440,.T.);
#35534=EDGE_CURVE('',#28060,#28059,#14441,.T.);
#35535=EDGE_CURVE('',#27968,#28060,#14442,.T.);
#35536=EDGE_CURVE('',#28060,#28061,#183,.T.);
#35537=EDGE_CURVE('',#28062,#28059,#184,.T.);
#35538=EDGE_CURVE('',#28061,#28062,#14443,.T.);
#35539=EDGE_CURVE('',#28061,#28063,#1118,.T.);
#35540=EDGE_CURVE('',#28064,#28062,#1119,.T.);
#35541=EDGE_CURVE('',#28063,#28064,#14444,.T.);
#35542=EDGE_CURVE('',#28057,#28063,#185,.T.);
#35543=EDGE_CURVE('',#28058,#28064,#186,.T.);
#35544=EDGE_CURVE('',#28065,#27965,#14445,.T.);
#35545=EDGE_CURVE('',#28065,#28066,#14446,.T.);
#35546=EDGE_CURVE('',#27966,#28066,#14447,.T.);
#35547=EDGE_CURVE('',#28067,#27963,#14448,.T.);
#35548=EDGE_CURVE('',#28068,#28067,#14449,.T.);
#35549=EDGE_CURVE('',#27964,#28068,#14450,.T.);
#35550=EDGE_CURVE('',#28068,#28069,#187,.T.);
#35551=EDGE_CURVE('',#28070,#28067,#188,.T.);
#35552=EDGE_CURVE('',#28069,#28070,#14451,.T.);
#35553=EDGE_CURVE('',#28069,#28071,#1120,.T.);
#35554=EDGE_CURVE('',#28072,#28070,#1121,.T.);
#35555=EDGE_CURVE('',#28071,#28072,#14452,.T.);
#35556=EDGE_CURVE('',#28065,#28071,#189,.T.);
#35557=EDGE_CURVE('',#28066,#28072,#190,.T.);
#35558=EDGE_CURVE('',#28073,#27961,#14453,.T.);
#35559=EDGE_CURVE('',#28073,#28074,#14454,.T.);
#35560=EDGE_CURVE('',#27962,#28074,#14455,.T.);
#35561=EDGE_CURVE('',#28075,#27959,#14456,.T.);
#35562=EDGE_CURVE('',#28076,#28075,#14457,.T.);
#35563=EDGE_CURVE('',#27960,#28076,#14458,.T.);
#35564=EDGE_CURVE('',#28076,#28077,#191,.T.);
#35565=EDGE_CURVE('',#28078,#28075,#192,.T.);
#35566=EDGE_CURVE('',#28077,#28078,#14459,.T.);
#35567=EDGE_CURVE('',#28077,#28079,#1122,.T.);
#35568=EDGE_CURVE('',#28080,#28078,#1123,.T.);
#35569=EDGE_CURVE('',#28079,#28080,#14460,.T.);
#35570=EDGE_CURVE('',#28073,#28079,#193,.T.);
#35571=EDGE_CURVE('',#28074,#28080,#194,.T.);
#35572=EDGE_CURVE('',#28081,#27957,#14461,.T.);
#35573=EDGE_CURVE('',#28081,#28082,#14462,.T.);
#35574=EDGE_CURVE('',#27958,#28082,#14463,.T.);
#35575=EDGE_CURVE('',#28083,#27955,#14464,.T.);
#35576=EDGE_CURVE('',#28084,#28083,#14465,.T.);
#35577=EDGE_CURVE('',#27956,#28084,#14466,.T.);
#35578=EDGE_CURVE('',#28084,#28085,#195,.T.);
#35579=EDGE_CURVE('',#28086,#28083,#196,.T.);
#35580=EDGE_CURVE('',#28085,#28086,#14467,.T.);
#35581=EDGE_CURVE('',#28085,#28087,#1124,.T.);
#35582=EDGE_CURVE('',#28088,#28086,#1125,.T.);
#35583=EDGE_CURVE('',#28087,#28088,#14468,.T.);
#35584=EDGE_CURVE('',#28081,#28087,#197,.T.);
#35585=EDGE_CURVE('',#28082,#28088,#198,.T.);
#35586=EDGE_CURVE('',#28089,#27953,#14469,.T.);
#35587=EDGE_CURVE('',#28089,#28090,#14470,.T.);
#35588=EDGE_CURVE('',#27954,#28090,#14471,.T.);
#35589=EDGE_CURVE('',#28091,#27951,#14472,.T.);
#35590=EDGE_CURVE('',#28092,#28091,#14473,.T.);
#35591=EDGE_CURVE('',#27952,#28092,#14474,.T.);
#35592=EDGE_CURVE('',#28092,#28093,#199,.T.);
#35593=EDGE_CURVE('',#28094,#28091,#200,.T.);
#35594=EDGE_CURVE('',#28093,#28094,#14475,.T.);
#35595=EDGE_CURVE('',#28093,#28095,#1126,.T.);
#35596=EDGE_CURVE('',#28096,#28094,#1127,.T.);
#35597=EDGE_CURVE('',#28095,#28096,#14476,.T.);
#35598=EDGE_CURVE('',#28089,#28095,#201,.T.);
#35599=EDGE_CURVE('',#28090,#28096,#202,.T.);
#35600=EDGE_CURVE('',#28097,#27949,#14477,.T.);
#35601=EDGE_CURVE('',#28097,#28098,#14478,.T.);
#35602=EDGE_CURVE('',#27950,#28098,#14479,.T.);
#35603=EDGE_CURVE('',#28099,#27947,#14480,.T.);
#35604=EDGE_CURVE('',#28100,#28099,#14481,.T.);
#35605=EDGE_CURVE('',#27948,#28100,#14482,.T.);
#35606=EDGE_CURVE('',#28100,#28101,#203,.T.);
#35607=EDGE_CURVE('',#28102,#28099,#204,.T.);
#35608=EDGE_CURVE('',#28101,#28102,#14483,.T.);
#35609=EDGE_CURVE('',#28101,#28103,#1128,.T.);
#35610=EDGE_CURVE('',#28104,#28102,#1129,.T.);
#35611=EDGE_CURVE('',#28103,#28104,#14484,.T.);
#35612=EDGE_CURVE('',#28097,#28103,#205,.T.);
#35613=EDGE_CURVE('',#28098,#28104,#206,.T.);
#35614=EDGE_CURVE('',#28105,#27943,#14485,.T.);
#35615=EDGE_CURVE('',#28106,#28105,#14486,.T.);
#35616=EDGE_CURVE('',#27944,#28106,#14487,.T.);
#35617=EDGE_CURVE('',#28106,#28107,#207,.T.);
#35618=EDGE_CURVE('',#28108,#28105,#208,.T.);
#35619=EDGE_CURVE('',#28107,#28108,#14488,.T.);
#35620=EDGE_CURVE('',#28107,#28109,#1130,.T.);
#35621=EDGE_CURVE('',#28110,#28108,#1131,.T.);
#35622=EDGE_CURVE('',#28109,#28110,#14489,.T.);
#35623=EDGE_CURVE('',#28111,#28109,#209,.T.);
#35624=EDGE_CURVE('',#28112,#28110,#210,.T.);
#35625=EDGE_CURVE('',#28111,#28112,#14490,.T.);
#35626=EDGE_CURVE('',#28111,#27945,#14491,.T.);
#35627=EDGE_CURVE('',#27946,#28112,#14492,.T.);
#35628=EDGE_CURVE('',#28113,#28113,#1132,.T.);
#35629=EDGE_CURVE('',#28113,#28114,#14493,.T.);
#35630=EDGE_CURVE('',#28114,#28114,#1133,.T.);
#35631=EDGE_CURVE('',#28115,#28115,#1134,.T.);
#35632=EDGE_CURVE('',#28116,#28116,#1135,.T.);
#35633=EDGE_CURVE('',#28116,#28115,#14494,.T.);
#35634=EDGE_CURVE('',#28117,#28117,#1136,.T.);
#35635=EDGE_CURVE('',#28117,#28116,#14495,.T.);
#35636=EDGE_CURVE('',#28118,#28119,#14496,.T.);
#35637=EDGE_CURVE('',#28120,#28118,#1137,.T.);
#35638=EDGE_CURVE('',#28119,#28120,#1138,.T.);
#35639=EDGE_CURVE('',#28121,#28122,#24345,.T.);
#35640=EDGE_CURVE('',#28123,#28121,#24346,.T.);
#35641=EDGE_CURVE('',#28122,#28123,#24347,.T.);
#35642=EDGE_CURVE('',#28122,#28120,#14497,.T.);
#35643=EDGE_CURVE('',#28124,#28118,#24348,.T.);
#35644=EDGE_CURVE('',#28124,#28125,#1139,.T.);
#35645=EDGE_CURVE('',#28119,#28125,#24349,.T.);
#35646=EDGE_CURVE('',#28125,#28124,#14498,.T.);
#35647=EDGE_CURVE('',#28126,#28127,#211,.T.);
#35648=EDGE_CURVE('',#28126,#28128,#14499,.T.);
#35649=EDGE_CURVE('',#28129,#28128,#212,.T.);
#35650=EDGE_CURVE('',#28127,#28129,#14500,.T.);
#35651=EDGE_CURVE('',#28130,#28126,#213,.T.);
#35652=EDGE_CURVE('',#28131,#28130,#14501,.T.);
#35653=EDGE_CURVE('',#28128,#28131,#214,.T.);
#35654=EDGE_CURVE('',#28132,#28131,#1140,.T.);
#35655=EDGE_CURVE('',#28132,#28133,#215,.T.);
#35656=EDGE_CURVE('',#28133,#28134,#216,.T.);
#35657=EDGE_CURVE('',#28135,#28134,#1141,.T.);
#35658=EDGE_CURVE('',#28135,#28136,#217,.T.);
#35659=EDGE_CURVE('',#28136,#28137,#218,.T.);
#35660=EDGE_CURVE('',#28138,#28137,#1142,.T.);
#35661=EDGE_CURVE('',#28138,#28139,#219,.T.);
#35662=EDGE_CURVE('',#28139,#28140,#220,.T.);
#35663=EDGE_CURVE('',#28141,#28140,#1143,.T.);
#35664=EDGE_CURVE('',#28141,#28142,#221,.T.);
#35665=EDGE_CURVE('',#28142,#28143,#222,.T.);
#35666=EDGE_CURVE('',#28144,#28143,#1144,.T.);
#35667=EDGE_CURVE('',#28144,#28145,#223,.T.);
#35668=EDGE_CURVE('',#28145,#28146,#224,.T.);
#35669=EDGE_CURVE('',#28147,#28146,#1145,.T.);
#35670=EDGE_CURVE('',#28147,#28148,#225,.T.);
#35671=EDGE_CURVE('',#28148,#28149,#226,.T.);
#35672=EDGE_CURVE('',#28150,#28149,#1146,.T.);
#35673=EDGE_CURVE('',#28150,#28151,#227,.T.);
#35674=EDGE_CURVE('',#28151,#28152,#228,.T.);
#35675=EDGE_CURVE('',#28153,#28152,#1147,.T.);
#35676=EDGE_CURVE('',#28153,#28154,#229,.T.);
#35677=EDGE_CURVE('',#28154,#28155,#230,.T.);
#35678=EDGE_CURVE('',#28156,#28155,#1148,.T.);
#35679=EDGE_CURVE('',#28156,#28157,#231,.T.);
#35680=EDGE_CURVE('',#28157,#28158,#232,.T.);
#35681=EDGE_CURVE('',#28159,#28158,#1149,.T.);
#35682=EDGE_CURVE('',#28159,#28160,#233,.T.);
#35683=EDGE_CURVE('',#28160,#28161,#234,.T.);
#35684=EDGE_CURVE('',#28162,#28161,#1150,.T.);
#35685=EDGE_CURVE('',#28162,#28163,#235,.T.);
#35686=EDGE_CURVE('',#28163,#28164,#236,.T.);
#35687=EDGE_CURVE('',#28165,#28164,#1151,.T.);
#35688=EDGE_CURVE('',#28165,#28166,#237,.T.);
#35689=EDGE_CURVE('',#28166,#28167,#238,.T.);
#35690=EDGE_CURVE('',#28168,#28167,#1152,.T.);
#35691=EDGE_CURVE('',#28168,#28169,#239,.T.);
#35692=EDGE_CURVE('',#28169,#28170,#240,.T.);
#35693=EDGE_CURVE('',#28171,#28170,#1153,.T.);
#35694=EDGE_CURVE('',#28171,#28172,#241,.T.);
#35695=EDGE_CURVE('',#28172,#28173,#242,.T.);
#35696=EDGE_CURVE('',#28174,#28173,#1154,.T.);
#35697=EDGE_CURVE('',#28174,#28175,#243,.T.);
#35698=EDGE_CURVE('',#28175,#28176,#244,.T.);
#35699=EDGE_CURVE('',#28177,#28176,#1155,.T.);
#35700=EDGE_CURVE('',#28177,#28178,#245,.T.);
#35701=EDGE_CURVE('',#28178,#28179,#246,.T.);
#35702=EDGE_CURVE('',#28180,#28179,#1156,.T.);
#35703=EDGE_CURVE('',#28180,#28181,#247,.T.);
#35704=EDGE_CURVE('',#28181,#28182,#248,.T.);
#35705=EDGE_CURVE('',#28183,#28182,#1157,.T.);
#35706=EDGE_CURVE('',#28183,#28184,#249,.T.);
#35707=EDGE_CURVE('',#28184,#28185,#250,.T.);
#35708=EDGE_CURVE('',#28186,#28185,#1158,.T.);
#35709=EDGE_CURVE('',#28186,#28187,#251,.T.);
#35710=EDGE_CURVE('',#28187,#28188,#14502,.T.);
#35711=EDGE_CURVE('',#28188,#28188,#1159,.T.);
#35712=EDGE_CURVE('',#28187,#28189,#252,.T.);
#35713=EDGE_CURVE('',#28190,#28189,#1160,.T.);
#35714=EDGE_CURVE('',#28190,#28191,#253,.T.);
#35715=EDGE_CURVE('',#28191,#28192,#254,.T.);
#35716=EDGE_CURVE('',#28193,#28192,#1161,.T.);
#35717=EDGE_CURVE('',#28193,#28194,#255,.T.);
#35718=EDGE_CURVE('',#28194,#28195,#256,.T.);
#35719=EDGE_CURVE('',#28196,#28195,#1162,.T.);
#35720=EDGE_CURVE('',#28196,#28197,#257,.T.);
#35721=EDGE_CURVE('',#28197,#28198,#258,.T.);
#35722=EDGE_CURVE('',#28199,#28198,#1163,.T.);
#35723=EDGE_CURVE('',#28199,#28200,#259,.T.);
#35724=EDGE_CURVE('',#28200,#28201,#260,.T.);
#35725=EDGE_CURVE('',#28202,#28201,#1164,.T.);
#35726=EDGE_CURVE('',#28202,#28203,#261,.T.);
#35727=EDGE_CURVE('',#28203,#28204,#262,.T.);
#35728=EDGE_CURVE('',#28205,#28204,#1165,.T.);
#35729=EDGE_CURVE('',#28205,#28206,#263,.T.);
#35730=EDGE_CURVE('',#28206,#28207,#264,.T.);
#35731=EDGE_CURVE('',#28208,#28207,#1166,.T.);
#35732=EDGE_CURVE('',#28208,#28209,#265,.T.);
#35733=EDGE_CURVE('',#28209,#28210,#266,.T.);
#35734=EDGE_CURVE('',#28211,#28210,#1167,.T.);
#35735=EDGE_CURVE('',#28211,#28212,#267,.T.);
#35736=EDGE_CURVE('',#28212,#28213,#268,.T.);
#35737=EDGE_CURVE('',#28214,#28213,#1168,.T.);
#35738=EDGE_CURVE('',#28214,#28215,#269,.T.);
#35739=EDGE_CURVE('',#28215,#28216,#270,.T.);
#35740=EDGE_CURVE('',#28217,#28216,#1169,.T.);
#35741=EDGE_CURVE('',#28217,#28218,#271,.T.);
#35742=EDGE_CURVE('',#28218,#28219,#272,.T.);
#35743=EDGE_CURVE('',#28220,#28219,#1170,.T.);
#35744=EDGE_CURVE('',#28220,#28221,#273,.T.);
#35745=EDGE_CURVE('',#28221,#28222,#274,.T.);
#35746=EDGE_CURVE('',#28223,#28222,#1171,.T.);
#35747=EDGE_CURVE('',#28223,#28224,#275,.T.);
#35748=EDGE_CURVE('',#28224,#28225,#276,.T.);
#35749=EDGE_CURVE('',#28226,#28225,#1172,.T.);
#35750=EDGE_CURVE('',#28226,#28227,#277,.T.);
#35751=EDGE_CURVE('',#28227,#28228,#278,.T.);
#35752=EDGE_CURVE('',#28229,#28228,#1173,.T.);
#35753=EDGE_CURVE('',#28229,#28230,#279,.T.);
#35754=EDGE_CURVE('',#28230,#28231,#280,.T.);
#35755=EDGE_CURVE('',#28232,#28231,#1174,.T.);
#35756=EDGE_CURVE('',#28232,#28233,#281,.T.);
#35757=EDGE_CURVE('',#28233,#28234,#282,.T.);
#35758=EDGE_CURVE('',#28235,#28234,#1175,.T.);
#35759=EDGE_CURVE('',#28235,#28236,#283,.T.);
#35760=EDGE_CURVE('',#28236,#28237,#284,.T.);
#35761=EDGE_CURVE('',#28238,#28237,#1176,.T.);
#35762=EDGE_CURVE('',#28238,#28239,#285,.T.);
#35763=EDGE_CURVE('',#28239,#28240,#286,.T.);
#35764=EDGE_CURVE('',#28241,#28240,#1177,.T.);
#35765=EDGE_CURVE('',#28241,#28242,#287,.T.);
#35766=EDGE_CURVE('',#28242,#28243,#288,.T.);
#35767=EDGE_CURVE('',#28244,#28243,#1178,.T.);
#35768=EDGE_CURVE('',#28244,#28245,#289,.T.);
#35769=EDGE_CURVE('',#28245,#28246,#290,.T.);
#35770=EDGE_CURVE('',#28247,#28246,#1179,.T.);
#35771=EDGE_CURVE('',#28247,#28248,#291,.T.);
#35772=EDGE_CURVE('',#28248,#28249,#292,.T.);
#35773=EDGE_CURVE('',#28129,#28249,#1180,.T.);
#35774=EDGE_CURVE('',#28250,#28130,#1181,.T.);
#35775=EDGE_CURVE('',#28250,#28132,#14503,.T.);
#35776=EDGE_CURVE('',#28249,#28251,#14504,.T.);
#35777=EDGE_CURVE('',#28127,#28251,#1182,.T.);
#35778=EDGE_CURVE('',#28252,#28133,#14505,.T.);
#35779=EDGE_CURVE('',#28253,#28252,#293,.T.);
#35780=EDGE_CURVE('',#28134,#28253,#14506,.T.);
#35781=EDGE_CURVE('',#28252,#28250,#294,.T.);
#35782=EDGE_CURVE('',#28254,#28253,#1183,.T.);
#35783=EDGE_CURVE('',#28254,#28135,#14507,.T.);
#35784=EDGE_CURVE('',#28255,#28255,#1184,.T.);
#35785=EDGE_CURVE('',#28255,#28256,#14508,.T.);
#35786=EDGE_CURVE('',#28256,#28257,#295,.T.);
#35787=EDGE_CURVE('',#28257,#28258,#1185,.T.);
#35788=EDGE_CURVE('',#28258,#28259,#296,.T.);
#35789=EDGE_CURVE('',#28259,#28260,#297,.T.);
#35790=EDGE_CURVE('',#28260,#28261,#1186,.T.);
#35791=EDGE_CURVE('',#28261,#28262,#298,.T.);
#35792=EDGE_CURVE('',#28262,#28263,#299,.T.);
#35793=EDGE_CURVE('',#28263,#28264,#1187,.T.);
#35794=EDGE_CURVE('',#28264,#28265,#300,.T.);
#35795=EDGE_CURVE('',#28265,#28266,#301,.T.);
#35796=EDGE_CURVE('',#28266,#28267,#1188,.T.);
#35797=EDGE_CURVE('',#28267,#28268,#302,.T.);
#35798=EDGE_CURVE('',#28268,#28269,#303,.T.);
#35799=EDGE_CURVE('',#28269,#28270,#1189,.T.);
#35800=EDGE_CURVE('',#28270,#28271,#304,.T.);
#35801=EDGE_CURVE('',#28271,#28272,#305,.T.);
#35802=EDGE_CURVE('',#28272,#28273,#1190,.T.);
#35803=EDGE_CURVE('',#28273,#28274,#306,.T.);
#35804=EDGE_CURVE('',#28274,#28275,#307,.T.);
#35805=EDGE_CURVE('',#28275,#28276,#1191,.T.);
#35806=EDGE_CURVE('',#28276,#28277,#308,.T.);
#35807=EDGE_CURVE('',#28277,#28278,#309,.T.);
#35808=EDGE_CURVE('',#28278,#28279,#1192,.T.);
#35809=EDGE_CURVE('',#28279,#28280,#310,.T.);
#35810=EDGE_CURVE('',#28280,#28281,#311,.T.);
#35811=EDGE_CURVE('',#28281,#28282,#1193,.T.);
#35812=EDGE_CURVE('',#28282,#28283,#312,.T.);
#35813=EDGE_CURVE('',#28283,#28284,#313,.T.);
#35814=EDGE_CURVE('',#28284,#28285,#1194,.T.);
#35815=EDGE_CURVE('',#28285,#28286,#314,.T.);
#35816=EDGE_CURVE('',#28286,#28287,#315,.T.);
#35817=EDGE_CURVE('',#28287,#28288,#1195,.T.);
#35818=EDGE_CURVE('',#28288,#28289,#316,.T.);
#35819=EDGE_CURVE('',#28289,#28290,#317,.T.);
#35820=EDGE_CURVE('',#28290,#28291,#1196,.T.);
#35821=EDGE_CURVE('',#28291,#28292,#318,.T.);
#35822=EDGE_CURVE('',#28292,#28293,#319,.T.);
#35823=EDGE_CURVE('',#28293,#28294,#1197,.T.);
#35824=EDGE_CURVE('',#28294,#28295,#320,.T.);
#35825=EDGE_CURVE('',#28295,#28296,#321,.T.);
#35826=EDGE_CURVE('',#28296,#28297,#1198,.T.);
#35827=EDGE_CURVE('',#28297,#28298,#322,.T.);
#35828=EDGE_CURVE('',#28298,#28299,#323,.T.);
#35829=EDGE_CURVE('',#28299,#28300,#1199,.T.);
#35830=EDGE_CURVE('',#28300,#28301,#324,.T.);
#35831=EDGE_CURVE('',#28301,#28302,#325,.T.);
#35832=EDGE_CURVE('',#28302,#28303,#1200,.T.);
#35833=EDGE_CURVE('',#28303,#28304,#326,.T.);
#35834=EDGE_CURVE('',#28304,#28305,#327,.T.);
#35835=EDGE_CURVE('',#28305,#28306,#1201,.T.);
#35836=EDGE_CURVE('',#28306,#28307,#328,.T.);
#35837=EDGE_CURVE('',#28307,#28254,#329,.T.);
#35838=EDGE_CURVE('',#28251,#28308,#330,.T.);
#35839=EDGE_CURVE('',#28308,#28309,#331,.T.);
#35840=EDGE_CURVE('',#28309,#28310,#1202,.T.);
#35841=EDGE_CURVE('',#28310,#28311,#332,.T.);
#35842=EDGE_CURVE('',#28311,#28312,#333,.T.);
#35843=EDGE_CURVE('',#28312,#28313,#1203,.T.);
#35844=EDGE_CURVE('',#28313,#28314,#334,.T.);
#35845=EDGE_CURVE('',#28314,#28315,#335,.T.);
#35846=EDGE_CURVE('',#28315,#28316,#1204,.T.);
#35847=EDGE_CURVE('',#28316,#28317,#336,.T.);
#35848=EDGE_CURVE('',#28317,#28318,#337,.T.);
#35849=EDGE_CURVE('',#28318,#28319,#1205,.T.);
#35850=EDGE_CURVE('',#28319,#28320,#338,.T.);
#35851=EDGE_CURVE('',#28320,#28321,#339,.T.);
#35852=EDGE_CURVE('',#28321,#28322,#1206,.T.);
#35853=EDGE_CURVE('',#28322,#28323,#340,.T.);
#35854=EDGE_CURVE('',#28323,#28324,#341,.T.);
#35855=EDGE_CURVE('',#28324,#28325,#1207,.T.);
#35856=EDGE_CURVE('',#28325,#28326,#342,.T.);
#35857=EDGE_CURVE('',#28326,#28327,#343,.T.);
#35858=EDGE_CURVE('',#28327,#28328,#1208,.T.);
#35859=EDGE_CURVE('',#28328,#28329,#344,.T.);
#35860=EDGE_CURVE('',#28329,#28330,#345,.T.);
#35861=EDGE_CURVE('',#28330,#28331,#1209,.T.);
#35862=EDGE_CURVE('',#28331,#28332,#346,.T.);
#35863=EDGE_CURVE('',#28332,#28333,#347,.T.);
#35864=EDGE_CURVE('',#28333,#28334,#1210,.T.);
#35865=EDGE_CURVE('',#28334,#28335,#348,.T.);
#35866=EDGE_CURVE('',#28335,#28336,#349,.T.);
#35867=EDGE_CURVE('',#28336,#28337,#1211,.T.);
#35868=EDGE_CURVE('',#28337,#28338,#350,.T.);
#35869=EDGE_CURVE('',#28338,#28339,#351,.T.);
#35870=EDGE_CURVE('',#28339,#28340,#1212,.T.);
#35871=EDGE_CURVE('',#28340,#28341,#352,.T.);
#35872=EDGE_CURVE('',#28341,#28342,#353,.T.);
#35873=EDGE_CURVE('',#28342,#28343,#1213,.T.);
#35874=EDGE_CURVE('',#28343,#28344,#354,.T.);
#35875=EDGE_CURVE('',#28344,#28345,#355,.T.);
#35876=EDGE_CURVE('',#28345,#28346,#1214,.T.);
#35877=EDGE_CURVE('',#28346,#28347,#356,.T.);
#35878=EDGE_CURVE('',#28347,#28348,#357,.T.);
#35879=EDGE_CURVE('',#28348,#28349,#1215,.T.);
#35880=EDGE_CURVE('',#28349,#28350,#358,.T.);
#35881=EDGE_CURVE('',#28350,#28351,#359,.T.);
#35882=EDGE_CURVE('',#28351,#28352,#1216,.T.);
#35883=EDGE_CURVE('',#28352,#28353,#360,.T.);
#35884=EDGE_CURVE('',#28353,#28354,#361,.T.);
#35885=EDGE_CURVE('',#28354,#28355,#1217,.T.);
#35886=EDGE_CURVE('',#28355,#28356,#362,.T.);
#35887=EDGE_CURVE('',#28356,#28357,#363,.T.);
#35888=EDGE_CURVE('',#28357,#28358,#1218,.T.);
#35889=EDGE_CURVE('',#28358,#28359,#364,.T.);
#35890=EDGE_CURVE('',#28359,#28360,#365,.T.);
#35891=EDGE_CURVE('',#28360,#28361,#1219,.T.);
#35892=EDGE_CURVE('',#28361,#28362,#366,.T.);
#35893=EDGE_CURVE('',#28362,#28363,#367,.T.);
#35894=EDGE_CURVE('',#28363,#28364,#1220,.T.);
#35895=EDGE_CURVE('',#28364,#28365,#368,.T.);
#35896=EDGE_CURVE('',#28365,#28366,#369,.T.);
#35897=EDGE_CURVE('',#28366,#28367,#1221,.T.);
#35898=EDGE_CURVE('',#28367,#28256,#370,.T.);
#35899=EDGE_CURVE('',#28307,#28136,#14509,.T.);
#35900=EDGE_CURVE('',#28137,#28306,#14510,.T.);
#35901=EDGE_CURVE('',#28304,#28139,#14511,.T.);
#35902=EDGE_CURVE('',#28305,#28138,#14512,.T.);
#35903=EDGE_CURVE('',#28140,#28303,#14513,.T.);
#35904=EDGE_CURVE('',#28302,#28141,#14514,.T.);
#35905=EDGE_CURVE('',#28301,#28142,#14515,.T.);
#35906=EDGE_CURVE('',#28143,#28300,#14516,.T.);
#35907=EDGE_CURVE('',#28299,#28144,#14517,.T.);
#35908=EDGE_CURVE('',#28298,#28145,#14518,.T.);
#35909=EDGE_CURVE('',#28146,#28297,#14519,.T.);
#35910=EDGE_CURVE('',#28295,#28148,#14520,.T.);
#35911=EDGE_CURVE('',#28296,#28147,#14521,.T.);
#35912=EDGE_CURVE('',#28149,#28294,#14522,.T.);
#35913=EDGE_CURVE('',#28293,#28150,#14523,.T.);
#35914=EDGE_CURVE('',#28292,#28151,#14524,.T.);
#35915=EDGE_CURVE('',#28152,#28291,#14525,.T.);
#35916=EDGE_CURVE('',#28290,#28153,#14526,.T.);
#35917=EDGE_CURVE('',#28289,#28154,#14527,.T.);
#35918=EDGE_CURVE('',#28155,#28288,#14528,.T.);
#35919=EDGE_CURVE('',#28286,#28157,#14529,.T.);
#35920=EDGE_CURVE('',#28287,#28156,#14530,.T.);
#35921=EDGE_CURVE('',#28158,#28285,#14531,.T.);
#35922=EDGE_CURVE('',#28284,#28159,#14532,.T.);
#35923=EDGE_CURVE('',#28283,#28160,#14533,.T.);
#35924=EDGE_CURVE('',#28161,#28282,#14534,.T.);
#35925=EDGE_CURVE('',#28281,#28162,#14535,.T.);
#35926=EDGE_CURVE('',#28280,#28163,#14536,.T.);
#35927=EDGE_CURVE('',#28164,#28279,#14537,.T.);
#35928=EDGE_CURVE('',#28277,#28166,#14538,.T.);
#35929=EDGE_CURVE('',#28278,#28165,#14539,.T.);
#35930=EDGE_CURVE('',#28167,#28276,#14540,.T.);
#35931=EDGE_CURVE('',#28275,#28168,#14541,.T.);
#35932=EDGE_CURVE('',#28274,#28169,#14542,.T.);
#35933=EDGE_CURVE('',#28170,#28273,#14543,.T.);
#35934=EDGE_CURVE('',#28272,#28171,#14544,.T.);
#35935=EDGE_CURVE('',#28271,#28172,#14545,.T.);
#35936=EDGE_CURVE('',#28173,#28270,#14546,.T.);
#35937=EDGE_CURVE('',#28268,#28175,#14547,.T.);
#35938=EDGE_CURVE('',#28269,#28174,#14548,.T.);
#35939=EDGE_CURVE('',#28176,#28267,#14549,.T.);
#35940=EDGE_CURVE('',#28266,#28177,#14550,.T.);
#35941=EDGE_CURVE('',#28265,#28178,#14551,.T.);
#35942=EDGE_CURVE('',#28179,#28264,#14552,.T.);
#35943=EDGE_CURVE('',#28263,#28180,#14553,.T.);
#35944=EDGE_CURVE('',#28262,#28181,#14554,.T.);
#35945=EDGE_CURVE('',#28182,#28261,#14555,.T.);
#35946=EDGE_CURVE('',#28259,#28184,#14556,.T.);
#35947=EDGE_CURVE('',#28260,#28183,#14557,.T.);
#35948=EDGE_CURVE('',#28185,#28258,#14558,.T.);
#35949=EDGE_CURVE('',#28257,#28186,#14559,.T.);
#35950=EDGE_CURVE('',#28256,#28187,#14560,.T.);
#35951=EDGE_CURVE('',#28189,#28367,#14561,.T.);
#35952=EDGE_CURVE('',#28366,#28190,#14562,.T.);
#35953=EDGE_CURVE('',#28365,#28191,#14563,.T.);
#35954=EDGE_CURVE('',#28192,#28364,#14564,.T.);
#35955=EDGE_CURVE('',#28362,#28194,#14565,.T.);
#35956=EDGE_CURVE('',#28363,#28193,#14566,.T.);
#35957=EDGE_CURVE('',#28195,#28361,#14567,.T.);
#35958=EDGE_CURVE('',#28360,#28196,#14568,.T.);
#35959=EDGE_CURVE('',#28359,#28197,#14569,.T.);
#35960=EDGE_CURVE('',#28198,#28358,#14570,.T.);
#35961=EDGE_CURVE('',#28357,#28199,#14571,.T.);
#35962=EDGE_CURVE('',#28356,#28200,#14572,.T.);
#35963=EDGE_CURVE('',#28201,#28355,#14573,.T.);
#35964=EDGE_CURVE('',#28353,#28203,#14574,.T.);
#35965=EDGE_CURVE('',#28354,#28202,#14575,.T.);
#35966=EDGE_CURVE('',#28204,#28352,#14576,.T.);
#35967=EDGE_CURVE('',#28351,#28205,#14577,.T.);
#35968=EDGE_CURVE('',#28350,#28206,#14578,.T.);
#35969=EDGE_CURVE('',#28207,#28349,#14579,.T.);
#35970=EDGE_CURVE('',#28348,#28208,#14580,.T.);
#35971=EDGE_CURVE('',#28347,#28209,#14581,.T.);
#35972=EDGE_CURVE('',#28210,#28346,#14582,.T.);
#35973=EDGE_CURVE('',#28344,#28212,#14583,.T.);
#35974=EDGE_CURVE('',#28345,#28211,#14584,.T.);
#35975=EDGE_CURVE('',#28213,#28343,#14585,.T.);
#35976=EDGE_CURVE('',#28342,#28214,#14586,.T.);
#35977=EDGE_CURVE('',#28341,#28215,#14587,.T.);
#35978=EDGE_CURVE('',#28216,#28340,#14588,.T.);
#35979=EDGE_CURVE('',#28339,#28217,#14589,.T.);
#35980=EDGE_CURVE('',#28338,#28218,#14590,.T.);
#35981=EDGE_CURVE('',#28219,#28337,#14591,.T.);
#35982=EDGE_CURVE('',#28335,#28221,#14592,.T.);
#35983=EDGE_CURVE('',#28336,#28220,#14593,.T.);
#35984=EDGE_CURVE('',#28222,#28334,#14594,.T.);
#35985=EDGE_CURVE('',#28333,#28223,#14595,.T.);
#35986=EDGE_CURVE('',#28332,#28224,#14596,.T.);
#35987=EDGE_CURVE('',#28225,#28331,#14597,.T.);
#35988=EDGE_CURVE('',#28330,#28226,#14598,.T.);
#35989=EDGE_CURVE('',#28329,#28227,#14599,.T.);
#35990=EDGE_CURVE('',#28228,#28328,#14600,.T.);
#35991=EDGE_CURVE('',#28326,#28230,#14601,.T.);
#35992=EDGE_CURVE('',#28327,#28229,#14602,.T.);
#35993=EDGE_CURVE('',#28231,#28325,#14603,.T.);
#35994=EDGE_CURVE('',#28324,#28232,#14604,.T.);
#35995=EDGE_CURVE('',#28323,#28233,#14605,.T.);
#35996=EDGE_CURVE('',#28234,#28322,#14606,.T.);
#35997=EDGE_CURVE('',#28321,#28235,#14607,.T.);
#35998=EDGE_CURVE('',#28320,#28236,#14608,.T.);
#35999=EDGE_CURVE('',#28237,#28319,#14609,.T.);
#36000=EDGE_CURVE('',#28317,#28239,#14610,.T.);
#36001=EDGE_CURVE('',#28318,#28238,#14611,.T.);
#36002=EDGE_CURVE('',#28240,#28316,#14612,.T.);
#36003=EDGE_CURVE('',#28315,#28241,#14613,.T.);
#36004=EDGE_CURVE('',#28314,#28242,#14614,.T.);
#36005=EDGE_CURVE('',#28243,#28313,#14615,.T.);
#36006=EDGE_CURVE('',#28312,#28244,#14616,.T.);
#36007=EDGE_CURVE('',#28311,#28245,#14617,.T.);
#36008=EDGE_CURVE('',#28246,#28310,#14618,.T.);
#36009=EDGE_CURVE('',#28308,#28248,#14619,.T.);
#36010=EDGE_CURVE('',#28309,#28247,#14620,.T.);
#36011=EDGE_CURVE('',#28368,#28368,#1222,.T.);
#36012=EDGE_CURVE('',#28368,#28369,#14621,.T.);
#36013=EDGE_CURVE('',#28369,#28369,#1223,.T.);
#36014=EDGE_CURVE('',#28370,#28370,#1224,.T.);
#36015=EDGE_CURVE('',#28371,#28371,#1225,.T.);
#36016=EDGE_CURVE('',#28371,#28370,#14622,.T.);
#36017=EDGE_CURVE('',#28372,#28372,#1226,.T.);
#36018=EDGE_CURVE('',#28372,#28371,#14623,.T.);
#36019=EDGE_CURVE('',#28373,#28373,#1227,.T.);
#36020=EDGE_CURVE('',#28373,#28372,#14624,.T.);
#36021=EDGE_CURVE('',#28374,#28374,#1228,.T.);
#36022=EDGE_CURVE('',#28375,#28375,#1229,.T.);
#36023=EDGE_CURVE('',#28375,#28374,#14625,.T.);
#36024=EDGE_CURVE('',#28376,#28376,#1230,.T.);
#36025=EDGE_CURVE('',#28376,#28375,#14626,.T.);
#36026=EDGE_CURVE('',#28377,#28377,#1231,.T.);
#36027=EDGE_CURVE('',#28377,#28378,#14627,.T.);
#36028=EDGE_CURVE('',#28378,#28378,#1232,.T.);
#36029=EDGE_CURVE('',#28379,#28380,#14628,.T.);
#36030=EDGE_CURVE('',#28380,#28380,#1233,.T.);
#36031=EDGE_CURVE('',#28380,#28368,#14629,.T.);
#36032=EDGE_CURVE('',#28381,#28381,#1234,.T.);
#36033=EDGE_CURVE('',#28381,#28382,#14630,.T.);
#36034=EDGE_CURVE('',#28382,#28382,#1235,.T.);
#36035=EDGE_CURVE('',#28383,#28383,#1236,.T.);
#36036=EDGE_CURVE('',#28384,#28384,#1237,.T.);
#36037=EDGE_CURVE('',#28384,#28383,#14631,.T.);
#36038=EDGE_CURVE('',#28385,#28385,#1238,.T.);
#36039=EDGE_CURVE('',#28385,#28384,#14632,.T.);
#36040=EDGE_CURVE('',#28386,#28386,#1239,.T.);
#36041=EDGE_CURVE('',#28387,#28387,#1240,.T.);
#36042=EDGE_CURVE('',#28387,#28386,#14633,.T.);
#36043=EDGE_CURVE('',#28388,#28388,#1241,.T.);
#36044=EDGE_CURVE('',#28388,#28387,#14634,.T.);
#36045=EDGE_CURVE('',#28389,#28389,#1242,.T.);
#36046=EDGE_CURVE('',#28389,#28390,#14635,.T.);
#36047=EDGE_CURVE('',#28390,#28390,#1243,.T.);
#36048=EDGE_CURVE('',#28390,#28381,#14636,.T.);
#36049=EDGE_CURVE('',#28391,#28391,#1244,.T.);
#36050=EDGE_CURVE('',#28391,#28392,#14637,.T.);
#36051=EDGE_CURVE('',#28392,#28392,#1245,.T.);
#36052=EDGE_CURVE('',#28392,#28393,#14638,.T.);
#36053=EDGE_CURVE('',#28393,#28393,#1246,.T.);
#36054=EDGE_CURVE('',#28394,#28395,#14639,.T.);
#36055=EDGE_CURVE('',#28395,#28396,#14640,.T.);
#36056=EDGE_CURVE('',#28397,#28396,#14641,.T.);
#36057=EDGE_CURVE('',#28394,#28397,#14642,.T.);
#36058=EDGE_CURVE('',#28398,#28398,#1247,.T.);
#36059=EDGE_CURVE('',#28398,#28399,#14643,.T.);
#36060=EDGE_CURVE('',#28399,#28399,#1248,.T.);
#36061=EDGE_CURVE('',#28399,#28400,#14644,.T.);
#36062=EDGE_CURVE('',#28400,#28400,#1249,.T.);
#36063=EDGE_CURVE('',#28401,#28402,#14645,.T.);
#36064=EDGE_CURVE('',#28402,#28403,#14646,.T.);
#36065=EDGE_CURVE('',#28404,#28403,#14647,.T.);
#36066=EDGE_CURVE('',#28401,#28404,#14648,.T.);
#36067=EDGE_CURVE('',#28405,#28405,#1250,.T.);
#36068=EDGE_CURVE('',#28406,#28406,#1251,.T.);
#36069=EDGE_CURVE('',#28405,#28407,#14649,.T.);
#36070=EDGE_CURVE('',#28407,#28407,#1252,.T.);
#36071=EDGE_CURVE('',#28406,#28408,#14650,.T.);
#36072=EDGE_CURVE('',#28408,#28408,#1253,.T.);
#36073=EDGE_CURVE('',#28409,#28410,#14651,.T.);
#36074=EDGE_CURVE('',#28410,#28411,#14652,.T.);
#36075=EDGE_CURVE('',#28411,#28412,#14653,.T.);
#36076=EDGE_CURVE('',#28412,#28409,#14654,.T.);
#36077=EDGE_CURVE('',#28413,#28409,#14655,.T.);
#36078=EDGE_CURVE('',#28414,#28413,#14656,.T.);
#36079=EDGE_CURVE('',#28414,#28394,#14657,.T.);
#36080=EDGE_CURVE('',#28410,#28397,#14658,.T.);
#36081=EDGE_CURVE('',#28415,#28412,#14659,.T.);
#36082=EDGE_CURVE('',#28413,#28415,#14660,.T.);
#36083=EDGE_CURVE('',#28415,#28416,#14661,.T.);
#36084=EDGE_CURVE('',#28416,#28414,#14662,.T.);
#36085=EDGE_CURVE('',#28417,#28401,#14663,.T.);
#36086=EDGE_CURVE('',#28418,#28404,#14664,.T.);
#36087=EDGE_CURVE('',#28417,#28418,#14665,.T.);
#36088=EDGE_CURVE('',#28419,#28417,#14666,.T.);
#36089=EDGE_CURVE('',#28420,#28418,#14667,.T.);
#36090=EDGE_CURVE('',#28419,#28420,#14668,.T.);
#36091=EDGE_CURVE('',#28421,#28419,#14669,.T.);
#36092=EDGE_CURVE('',#28422,#28420,#14670,.T.);
#36093=EDGE_CURVE('',#28421,#28422,#14671,.T.);
#36094=EDGE_CURVE('',#28423,#28421,#14672,.T.);
#36095=EDGE_CURVE('',#28424,#28422,#14673,.T.);
#36096=EDGE_CURVE('',#28423,#28424,#14674,.T.);
#36097=EDGE_CURVE('',#28425,#28423,#14675,.T.);
#36098=EDGE_CURVE('',#28426,#28424,#14676,.T.);
#36099=EDGE_CURVE('',#28425,#28426,#14677,.T.);
#36100=EDGE_CURVE('',#28427,#28425,#14678,.T.);
#36101=EDGE_CURVE('',#28428,#28426,#14679,.T.);
#36102=EDGE_CURVE('',#28427,#28428,#14680,.T.);
#36103=EDGE_CURVE('',#28429,#28427,#14681,.T.);
#36104=EDGE_CURVE('',#28430,#28428,#14682,.T.);
#36105=EDGE_CURVE('',#28429,#28430,#14683,.T.);
#36106=EDGE_CURVE('',#28431,#28429,#14684,.T.);
#36107=EDGE_CURVE('',#28432,#28430,#14685,.T.);
#36108=EDGE_CURVE('',#28431,#28432,#14686,.T.);
#36109=EDGE_CURVE('',#28433,#28431,#14687,.T.);
#36110=EDGE_CURVE('',#28434,#28432,#14688,.T.);
#36111=EDGE_CURVE('',#28433,#28434,#14689,.T.);
#36112=EDGE_CURVE('',#28435,#28433,#14690,.T.);
#36113=EDGE_CURVE('',#28436,#28434,#14691,.T.);
#36114=EDGE_CURVE('',#28435,#28436,#14692,.T.);
#36115=EDGE_CURVE('',#28437,#28435,#14693,.T.);
#36116=EDGE_CURVE('',#28438,#28436,#14694,.T.);
#36117=EDGE_CURVE('',#28437,#28438,#14695,.T.);
#36118=EDGE_CURVE('',#28439,#28437,#14696,.T.);
#36119=EDGE_CURVE('',#28440,#28438,#14697,.T.);
#36120=EDGE_CURVE('',#28439,#28440,#14698,.T.);
#36121=EDGE_CURVE('',#28441,#28439,#14699,.T.);
#36122=EDGE_CURVE('',#28442,#28440,#14700,.T.);
#36123=EDGE_CURVE('',#28441,#28442,#14701,.T.);
#36124=EDGE_CURVE('',#28443,#28441,#14702,.T.);
#36125=EDGE_CURVE('',#28444,#28442,#14703,.T.);
#36126=EDGE_CURVE('',#28443,#28444,#14704,.T.);
#36127=EDGE_CURVE('',#28445,#28443,#14705,.T.);
#36128=EDGE_CURVE('',#28446,#28444,#14706,.T.);
#36129=EDGE_CURVE('',#28445,#28446,#14707,.T.);
#36130=EDGE_CURVE('',#28447,#28445,#14708,.T.);
#36131=EDGE_CURVE('',#28448,#28446,#14709,.T.);
#36132=EDGE_CURVE('',#28447,#28448,#14710,.T.);
#36133=EDGE_CURVE('',#28449,#28447,#14711,.T.);
#36134=EDGE_CURVE('',#28450,#28448,#14712,.T.);
#36135=EDGE_CURVE('',#28449,#28450,#14713,.T.);
#36136=EDGE_CURVE('',#28451,#28449,#14714,.T.);
#36137=EDGE_CURVE('',#28452,#28450,#14715,.T.);
#36138=EDGE_CURVE('',#28451,#28452,#14716,.T.);
#36139=EDGE_CURVE('',#28453,#28451,#14717,.T.);
#36140=EDGE_CURVE('',#28454,#28452,#14718,.T.);
#36141=EDGE_CURVE('',#28453,#28454,#14719,.T.);
#36142=EDGE_CURVE('',#28455,#28453,#14720,.T.);
#36143=EDGE_CURVE('',#28456,#28454,#14721,.T.);
#36144=EDGE_CURVE('',#28455,#28456,#14722,.T.);
#36145=EDGE_CURVE('',#28457,#28455,#14723,.T.);
#36146=EDGE_CURVE('',#28458,#28456,#14724,.T.);
#36147=EDGE_CURVE('',#28457,#28458,#14725,.T.);
#36148=EDGE_CURVE('',#28459,#28457,#14726,.T.);
#36149=EDGE_CURVE('',#28460,#28458,#14727,.T.);
#36150=EDGE_CURVE('',#28459,#28460,#14728,.T.);
#36151=EDGE_CURVE('',#28461,#28459,#14729,.T.);
#36152=EDGE_CURVE('',#28462,#28460,#14730,.T.);
#36153=EDGE_CURVE('',#28461,#28462,#14731,.T.);
#36154=EDGE_CURVE('',#28463,#28461,#14732,.T.);
#36155=EDGE_CURVE('',#28464,#28462,#14733,.T.);
#36156=EDGE_CURVE('',#28463,#28464,#14734,.T.);
#36157=EDGE_CURVE('',#28465,#28463,#14735,.T.);
#36158=EDGE_CURVE('',#28466,#28464,#14736,.T.);
#36159=EDGE_CURVE('',#28465,#28466,#14737,.T.);
#36160=EDGE_CURVE('',#28467,#28465,#14738,.T.);
#36161=EDGE_CURVE('',#28468,#28466,#14739,.T.);
#36162=EDGE_CURVE('',#28467,#28468,#14740,.T.);
#36163=EDGE_CURVE('',#28469,#28467,#14741,.T.);
#36164=EDGE_CURVE('',#28470,#28468,#14742,.T.);
#36165=EDGE_CURVE('',#28469,#28470,#14743,.T.);
#36166=EDGE_CURVE('',#28471,#28469,#14744,.T.);
#36167=EDGE_CURVE('',#28472,#28470,#14745,.T.);
#36168=EDGE_CURVE('',#28471,#28472,#14746,.T.);
#36169=EDGE_CURVE('',#28473,#28471,#14747,.T.);
#36170=EDGE_CURVE('',#28474,#28472,#14748,.T.);
#36171=EDGE_CURVE('',#28473,#28474,#14749,.T.);
#36172=EDGE_CURVE('',#28475,#28473,#14750,.T.);
#36173=EDGE_CURVE('',#28476,#28474,#14751,.T.);
#36174=EDGE_CURVE('',#28475,#28476,#14752,.T.);
#36175=EDGE_CURVE('',#28477,#28475,#14753,.T.);
#36176=EDGE_CURVE('',#28478,#28476,#14754,.T.);
#36177=EDGE_CURVE('',#28477,#28478,#14755,.T.);
#36178=EDGE_CURVE('',#28479,#28477,#14756,.T.);
#36179=EDGE_CURVE('',#28480,#28478,#14757,.T.);
#36180=EDGE_CURVE('',#28479,#28480,#14758,.T.);
#36181=EDGE_CURVE('',#28481,#28479,#14759,.T.);
#36182=EDGE_CURVE('',#28482,#28480,#14760,.T.);
#36183=EDGE_CURVE('',#28481,#28482,#14761,.T.);
#36184=EDGE_CURVE('',#28483,#28481,#14762,.T.);
#36185=EDGE_CURVE('',#28484,#28482,#14763,.T.);
#36186=EDGE_CURVE('',#28483,#28484,#14764,.T.);
#36187=EDGE_CURVE('',#28485,#28483,#14765,.T.);
#36188=EDGE_CURVE('',#28486,#28484,#14766,.T.);
#36189=EDGE_CURVE('',#28485,#28486,#14767,.T.);
#36190=EDGE_CURVE('',#28487,#28485,#14768,.T.);
#36191=EDGE_CURVE('',#28488,#28486,#14769,.T.);
#36192=EDGE_CURVE('',#28487,#28488,#14770,.T.);
#36193=EDGE_CURVE('',#28489,#28487,#14771,.T.);
#36194=EDGE_CURVE('',#28490,#28488,#14772,.T.);
#36195=EDGE_CURVE('',#28489,#28490,#14773,.T.);
#36196=EDGE_CURVE('',#28491,#28489,#14774,.T.);
#36197=EDGE_CURVE('',#28492,#28490,#14775,.T.);
#36198=EDGE_CURVE('',#28491,#28492,#14776,.T.);
#36199=EDGE_CURVE('',#28493,#28491,#14777,.T.);
#36200=EDGE_CURVE('',#28494,#28492,#14778,.T.);
#36201=EDGE_CURVE('',#28493,#28494,#14779,.T.);
#36202=EDGE_CURVE('',#28495,#28493,#14780,.T.);
#36203=EDGE_CURVE('',#28496,#28494,#14781,.T.);
#36204=EDGE_CURVE('',#28495,#28496,#14782,.T.);
#36205=EDGE_CURVE('',#28497,#28495,#14783,.T.);
#36206=EDGE_CURVE('',#28498,#28496,#14784,.T.);
#36207=EDGE_CURVE('',#28497,#28498,#14785,.T.);
#36208=EDGE_CURVE('',#28499,#28497,#14786,.T.);
#36209=EDGE_CURVE('',#28500,#28498,#14787,.T.);
#36210=EDGE_CURVE('',#28499,#28500,#14788,.T.);
#36211=EDGE_CURVE('',#28501,#28499,#14789,.T.);
#36212=EDGE_CURVE('',#28502,#28500,#14790,.T.);
#36213=EDGE_CURVE('',#28501,#28502,#14791,.T.);
#36214=EDGE_CURVE('',#28503,#28501,#14792,.T.);
#36215=EDGE_CURVE('',#28504,#28502,#14793,.T.);
#36216=EDGE_CURVE('',#28503,#28504,#14794,.T.);
#36217=EDGE_CURVE('',#28505,#28503,#14795,.T.);
#36218=EDGE_CURVE('',#28506,#28504,#14796,.T.);
#36219=EDGE_CURVE('',#28505,#28506,#14797,.T.);
#36220=EDGE_CURVE('',#28507,#28505,#14798,.T.);
#36221=EDGE_CURVE('',#28508,#28506,#14799,.T.);
#36222=EDGE_CURVE('',#28507,#28508,#14800,.T.);
#36223=EDGE_CURVE('',#28509,#28507,#14801,.T.);
#36224=EDGE_CURVE('',#28510,#28508,#14802,.T.);
#36225=EDGE_CURVE('',#28509,#28510,#14803,.T.);
#36226=EDGE_CURVE('',#28511,#28509,#14804,.T.);
#36227=EDGE_CURVE('',#28512,#28510,#14805,.T.);
#36228=EDGE_CURVE('',#28511,#28512,#14806,.T.);
#36229=EDGE_CURVE('',#28513,#28511,#14807,.T.);
#36230=EDGE_CURVE('',#28514,#28512,#14808,.T.);
#36231=EDGE_CURVE('',#28513,#28514,#14809,.T.);
#36232=EDGE_CURVE('',#28515,#28513,#14810,.T.);
#36233=EDGE_CURVE('',#28516,#28514,#14811,.T.);
#36234=EDGE_CURVE('',#28515,#28516,#14812,.T.);
#36235=EDGE_CURVE('',#28517,#28515,#14813,.T.);
#36236=EDGE_CURVE('',#28518,#28516,#14814,.T.);
#36237=EDGE_CURVE('',#28517,#28518,#14815,.T.);
#36238=EDGE_CURVE('',#28519,#28517,#14816,.T.);
#36239=EDGE_CURVE('',#28520,#28518,#14817,.T.);
#36240=EDGE_CURVE('',#28519,#28520,#14818,.T.);
#36241=EDGE_CURVE('',#28521,#28519,#14819,.T.);
#36242=EDGE_CURVE('',#28522,#28520,#14820,.T.);
#36243=EDGE_CURVE('',#28521,#28522,#14821,.T.);
#36244=EDGE_CURVE('',#28523,#28521,#14822,.T.);
#36245=EDGE_CURVE('',#28524,#28522,#14823,.T.);
#36246=EDGE_CURVE('',#28523,#28524,#14824,.T.);
#36247=EDGE_CURVE('',#28525,#28523,#14825,.T.);
#36248=EDGE_CURVE('',#28526,#28524,#14826,.T.);
#36249=EDGE_CURVE('',#28525,#28526,#14827,.T.);
#36250=EDGE_CURVE('',#28527,#28525,#14828,.T.);
#36251=EDGE_CURVE('',#28528,#28526,#14829,.T.);
#36252=EDGE_CURVE('',#28527,#28528,#14830,.T.);
#36253=EDGE_CURVE('',#28529,#28527,#14831,.T.);
#36254=EDGE_CURVE('',#28530,#28528,#14832,.T.);
#36255=EDGE_CURVE('',#28529,#28530,#14833,.T.);
#36256=EDGE_CURVE('',#28531,#28529,#14834,.T.);
#36257=EDGE_CURVE('',#28532,#28530,#14835,.T.);
#36258=EDGE_CURVE('',#28531,#28532,#14836,.T.);
#36259=EDGE_CURVE('',#28533,#28531,#14837,.T.);
#36260=EDGE_CURVE('',#28534,#28532,#14838,.T.);
#36261=EDGE_CURVE('',#28533,#28534,#14839,.T.);
#36262=EDGE_CURVE('',#28535,#28533,#14840,.T.);
#36263=EDGE_CURVE('',#28536,#28534,#14841,.T.);
#36264=EDGE_CURVE('',#28535,#28536,#14842,.T.);
#36265=EDGE_CURVE('',#28537,#28535,#14843,.T.);
#36266=EDGE_CURVE('',#28538,#28536,#14844,.T.);
#36267=EDGE_CURVE('',#28537,#28538,#14845,.T.);
#36268=EDGE_CURVE('',#28539,#28537,#14846,.T.);
#36269=EDGE_CURVE('',#28540,#28538,#14847,.T.);
#36270=EDGE_CURVE('',#28539,#28540,#14848,.T.);
#36271=EDGE_CURVE('',#28541,#28539,#14849,.T.);
#36272=EDGE_CURVE('',#28542,#28540,#14850,.T.);
#36273=EDGE_CURVE('',#28541,#28542,#14851,.T.);
#36274=EDGE_CURVE('',#28543,#28541,#14852,.T.);
#36275=EDGE_CURVE('',#28544,#28542,#14853,.T.);
#36276=EDGE_CURVE('',#28543,#28544,#14854,.T.);
#36277=EDGE_CURVE('',#28545,#28543,#14855,.T.);
#36278=EDGE_CURVE('',#28546,#28544,#14856,.T.);
#36279=EDGE_CURVE('',#28545,#28546,#14857,.T.);
#36280=EDGE_CURVE('',#28547,#28545,#14858,.T.);
#36281=EDGE_CURVE('',#28548,#28546,#14859,.T.);
#36282=EDGE_CURVE('',#28547,#28548,#14860,.T.);
#36283=EDGE_CURVE('',#28549,#28547,#14861,.T.);
#36284=EDGE_CURVE('',#28550,#28548,#14862,.T.);
#36285=EDGE_CURVE('',#28549,#28550,#14863,.T.);
#36286=EDGE_CURVE('',#28551,#28549,#14864,.T.);
#36287=EDGE_CURVE('',#28552,#28550,#14865,.T.);
#36288=EDGE_CURVE('',#28551,#28552,#14866,.T.);
#36289=EDGE_CURVE('',#28553,#28551,#14867,.T.);
#36290=EDGE_CURVE('',#28554,#28552,#14868,.T.);
#36291=EDGE_CURVE('',#28553,#28554,#14869,.T.);
#36292=EDGE_CURVE('',#28555,#28553,#14870,.T.);
#36293=EDGE_CURVE('',#28556,#28554,#14871,.T.);
#36294=EDGE_CURVE('',#28555,#28556,#14872,.T.);
#36295=EDGE_CURVE('',#28557,#28555,#14873,.T.);
#36296=EDGE_CURVE('',#28558,#28556,#14874,.T.);
#36297=EDGE_CURVE('',#28557,#28558,#14875,.T.);
#36298=EDGE_CURVE('',#28559,#28557,#14876,.T.);
#36299=EDGE_CURVE('',#28560,#28558,#14877,.T.);
#36300=EDGE_CURVE('',#28559,#28560,#14878,.T.);
#36301=EDGE_CURVE('',#28561,#28559,#14879,.T.);
#36302=EDGE_CURVE('',#28562,#28560,#14880,.T.);
#36303=EDGE_CURVE('',#28561,#28562,#14881,.T.);
#36304=EDGE_CURVE('',#28563,#28561,#14882,.T.);
#36305=EDGE_CURVE('',#28564,#28562,#14883,.T.);
#36306=EDGE_CURVE('',#28563,#28564,#14884,.T.);
#36307=EDGE_CURVE('',#28565,#28563,#14885,.T.);
#36308=EDGE_CURVE('',#28566,#28564,#14886,.T.);
#36309=EDGE_CURVE('',#28565,#28566,#14887,.T.);
#36310=EDGE_CURVE('',#28567,#28565,#14888,.T.);
#36311=EDGE_CURVE('',#28568,#28566,#14889,.T.);
#36312=EDGE_CURVE('',#28567,#28568,#14890,.T.);
#36313=EDGE_CURVE('',#28569,#28567,#14891,.T.);
#36314=EDGE_CURVE('',#28570,#28568,#14892,.T.);
#36315=EDGE_CURVE('',#28569,#28570,#14893,.T.);
#36316=EDGE_CURVE('',#28571,#28569,#14894,.T.);
#36317=EDGE_CURVE('',#28572,#28570,#14895,.T.);
#36318=EDGE_CURVE('',#28571,#28572,#14896,.T.);
#36319=EDGE_CURVE('',#28573,#28571,#14897,.T.);
#36320=EDGE_CURVE('',#28574,#28572,#14898,.T.);
#36321=EDGE_CURVE('',#28573,#28574,#14899,.T.);
#36322=EDGE_CURVE('',#28575,#28573,#14900,.T.);
#36323=EDGE_CURVE('',#28576,#28574,#14901,.T.);
#36324=EDGE_CURVE('',#28575,#28576,#14902,.T.);
#36325=EDGE_CURVE('',#28577,#28575,#14903,.T.);
#36326=EDGE_CURVE('',#28578,#28576,#14904,.T.);
#36327=EDGE_CURVE('',#28577,#28578,#14905,.T.);
#36328=EDGE_CURVE('',#28579,#28577,#14906,.T.);
#36329=EDGE_CURVE('',#28580,#28578,#14907,.T.);
#36330=EDGE_CURVE('',#28579,#28580,#14908,.T.);
#36331=EDGE_CURVE('',#28581,#28579,#14909,.T.);
#36332=EDGE_CURVE('',#28582,#28580,#14910,.T.);
#36333=EDGE_CURVE('',#28581,#28582,#14911,.T.);
#36334=EDGE_CURVE('',#28583,#28581,#14912,.T.);
#36335=EDGE_CURVE('',#28584,#28582,#14913,.T.);
#36336=EDGE_CURVE('',#28583,#28584,#14914,.T.);
#36337=EDGE_CURVE('',#28585,#28583,#14915,.T.);
#36338=EDGE_CURVE('',#28586,#28584,#14916,.T.);
#36339=EDGE_CURVE('',#28585,#28586,#14917,.T.);
#36340=EDGE_CURVE('',#28587,#28585,#14918,.T.);
#36341=EDGE_CURVE('',#28588,#28586,#14919,.T.);
#36342=EDGE_CURVE('',#28587,#28588,#14920,.T.);
#36343=EDGE_CURVE('',#28589,#28587,#14921,.T.);
#36344=EDGE_CURVE('',#28590,#28588,#14922,.T.);
#36345=EDGE_CURVE('',#28589,#28590,#14923,.T.);
#36346=EDGE_CURVE('',#28591,#28589,#14924,.T.);
#36347=EDGE_CURVE('',#28592,#28590,#14925,.T.);
#36348=EDGE_CURVE('',#28591,#28592,#14926,.T.);
#36349=EDGE_CURVE('',#28593,#28591,#14927,.T.);
#36350=EDGE_CURVE('',#28594,#28592,#14928,.T.);
#36351=EDGE_CURVE('',#28593,#28594,#14929,.T.);
#36352=EDGE_CURVE('',#28595,#28593,#14930,.T.);
#36353=EDGE_CURVE('',#28596,#28594,#14931,.T.);
#36354=EDGE_CURVE('',#28595,#28596,#14932,.T.);
#36355=EDGE_CURVE('',#28597,#28595,#14933,.T.);
#36356=EDGE_CURVE('',#28598,#28596,#14934,.T.);
#36357=EDGE_CURVE('',#28597,#28598,#14935,.T.);
#36358=EDGE_CURVE('',#28599,#28597,#14936,.T.);
#36359=EDGE_CURVE('',#28600,#28598,#14937,.T.);
#36360=EDGE_CURVE('',#28599,#28600,#14938,.T.);
#36361=EDGE_CURVE('',#28601,#28599,#14939,.T.);
#36362=EDGE_CURVE('',#28602,#28600,#14940,.T.);
#36363=EDGE_CURVE('',#28601,#28602,#14941,.T.);
#36364=EDGE_CURVE('',#28603,#28601,#14942,.T.);
#36365=EDGE_CURVE('',#28604,#28602,#14943,.T.);
#36366=EDGE_CURVE('',#28603,#28604,#14944,.T.);
#36367=EDGE_CURVE('',#28605,#28603,#14945,.T.);
#36368=EDGE_CURVE('',#28606,#28604,#14946,.T.);
#36369=EDGE_CURVE('',#28605,#28606,#14947,.T.);
#36370=EDGE_CURVE('',#28607,#28605,#14948,.T.);
#36371=EDGE_CURVE('',#28608,#28606,#14949,.T.);
#36372=EDGE_CURVE('',#28607,#28608,#14950,.T.);
#36373=EDGE_CURVE('',#28609,#28607,#14951,.T.);
#36374=EDGE_CURVE('',#28610,#28608,#14952,.T.);
#36375=EDGE_CURVE('',#28609,#28610,#14953,.T.);
#36376=EDGE_CURVE('',#28611,#28609,#14954,.T.);
#36377=EDGE_CURVE('',#28612,#28610,#14955,.T.);
#36378=EDGE_CURVE('',#28611,#28612,#14956,.T.);
#36379=EDGE_CURVE('',#28613,#28611,#14957,.T.);
#36380=EDGE_CURVE('',#28614,#28612,#14958,.T.);
#36381=EDGE_CURVE('',#28613,#28614,#14959,.T.);
#36382=EDGE_CURVE('',#28615,#28613,#14960,.T.);
#36383=EDGE_CURVE('',#28616,#28614,#14961,.T.);
#36384=EDGE_CURVE('',#28615,#28616,#14962,.T.);
#36385=EDGE_CURVE('',#28617,#28615,#14963,.T.);
#36386=EDGE_CURVE('',#28618,#28616,#14964,.T.);
#36387=EDGE_CURVE('',#28617,#28618,#14965,.T.);
#36388=EDGE_CURVE('',#28619,#28617,#14966,.T.);
#36389=EDGE_CURVE('',#28620,#28618,#14967,.T.);
#36390=EDGE_CURVE('',#28619,#28620,#14968,.T.);
#36391=EDGE_CURVE('',#28621,#28619,#14969,.T.);
#36392=EDGE_CURVE('',#28622,#28620,#14970,.T.);
#36393=EDGE_CURVE('',#28621,#28622,#14971,.T.);
#36394=EDGE_CURVE('',#28623,#28621,#14972,.T.);
#36395=EDGE_CURVE('',#28624,#28622,#14973,.T.);
#36396=EDGE_CURVE('',#28623,#28624,#14974,.T.);
#36397=EDGE_CURVE('',#28625,#28623,#14975,.T.);
#36398=EDGE_CURVE('',#28626,#28624,#14976,.T.);
#36399=EDGE_CURVE('',#28625,#28626,#14977,.T.);
#36400=EDGE_CURVE('',#28627,#28625,#14978,.T.);
#36401=EDGE_CURVE('',#28628,#28626,#14979,.T.);
#36402=EDGE_CURVE('',#28627,#28628,#14980,.T.);
#36403=EDGE_CURVE('',#28629,#28627,#14981,.T.);
#36404=EDGE_CURVE('',#28630,#28628,#14982,.T.);
#36405=EDGE_CURVE('',#28629,#28630,#14983,.T.);
#36406=EDGE_CURVE('',#28631,#28629,#14984,.T.);
#36407=EDGE_CURVE('',#28632,#28630,#14985,.T.);
#36408=EDGE_CURVE('',#28631,#28632,#14986,.T.);
#36409=EDGE_CURVE('',#28633,#28631,#14987,.T.);
#36410=EDGE_CURVE('',#28634,#28632,#14988,.T.);
#36411=EDGE_CURVE('',#28633,#28634,#14989,.T.);
#36412=EDGE_CURVE('',#28635,#28633,#14990,.T.);
#36413=EDGE_CURVE('',#28636,#28634,#14991,.T.);
#36414=EDGE_CURVE('',#28635,#28636,#14992,.T.);
#36415=EDGE_CURVE('',#28637,#28635,#14993,.T.);
#36416=EDGE_CURVE('',#28638,#28636,#14994,.T.);
#36417=EDGE_CURVE('',#28637,#28638,#14995,.T.);
#36418=EDGE_CURVE('',#28639,#28637,#14996,.T.);
#36419=EDGE_CURVE('',#28640,#28638,#14997,.T.);
#36420=EDGE_CURVE('',#28639,#28640,#14998,.T.);
#36421=EDGE_CURVE('',#28641,#28639,#14999,.T.);
#36422=EDGE_CURVE('',#28642,#28640,#15000,.T.);
#36423=EDGE_CURVE('',#28641,#28642,#15001,.T.);
#36424=EDGE_CURVE('',#28643,#28641,#15002,.T.);
#36425=EDGE_CURVE('',#28644,#28642,#15003,.T.);
#36426=EDGE_CURVE('',#28643,#28644,#15004,.T.);
#36427=EDGE_CURVE('',#28645,#28643,#15005,.T.);
#36428=EDGE_CURVE('',#28646,#28644,#15006,.T.);
#36429=EDGE_CURVE('',#28645,#28646,#15007,.T.);
#36430=EDGE_CURVE('',#28647,#28645,#15008,.T.);
#36431=EDGE_CURVE('',#28648,#28646,#15009,.T.);
#36432=EDGE_CURVE('',#28647,#28648,#15010,.T.);
#36433=EDGE_CURVE('',#28649,#28647,#15011,.T.);
#36434=EDGE_CURVE('',#28650,#28648,#15012,.T.);
#36435=EDGE_CURVE('',#28649,#28650,#15013,.T.);
#36436=EDGE_CURVE('',#28651,#28649,#15014,.T.);
#36437=EDGE_CURVE('',#28652,#28650,#15015,.T.);
#36438=EDGE_CURVE('',#28651,#28652,#15016,.T.);
#36439=EDGE_CURVE('',#28653,#28651,#15017,.T.);
#36440=EDGE_CURVE('',#28654,#28652,#15018,.T.);
#36441=EDGE_CURVE('',#28653,#28654,#15019,.T.);
#36442=EDGE_CURVE('',#28655,#28653,#15020,.T.);
#36443=EDGE_CURVE('',#28656,#28654,#15021,.T.);
#36444=EDGE_CURVE('',#28655,#28656,#15022,.T.);
#36445=EDGE_CURVE('',#28657,#28655,#15023,.T.);
#36446=EDGE_CURVE('',#28658,#28656,#15024,.T.);
#36447=EDGE_CURVE('',#28657,#28658,#15025,.T.);
#36448=EDGE_CURVE('',#28659,#28657,#15026,.T.);
#36449=EDGE_CURVE('',#28660,#28658,#15027,.T.);
#36450=EDGE_CURVE('',#28659,#28660,#15028,.T.);
#36451=EDGE_CURVE('',#28661,#28659,#15029,.T.);
#36452=EDGE_CURVE('',#28662,#28660,#15030,.T.);
#36453=EDGE_CURVE('',#28661,#28662,#15031,.T.);
#36454=EDGE_CURVE('',#28663,#28661,#15032,.T.);
#36455=EDGE_CURVE('',#28664,#28662,#15033,.T.);
#36456=EDGE_CURVE('',#28663,#28664,#15034,.T.);
#36457=EDGE_CURVE('',#28665,#28663,#15035,.T.);
#36458=EDGE_CURVE('',#28666,#28664,#15036,.T.);
#36459=EDGE_CURVE('',#28665,#28666,#15037,.T.);
#36460=EDGE_CURVE('',#28667,#28665,#15038,.T.);
#36461=EDGE_CURVE('',#28668,#28666,#15039,.T.);
#36462=EDGE_CURVE('',#28667,#28668,#15040,.T.);
#36463=EDGE_CURVE('',#28669,#28667,#15041,.T.);
#36464=EDGE_CURVE('',#28670,#28668,#15042,.T.);
#36465=EDGE_CURVE('',#28669,#28670,#15043,.T.);
#36466=EDGE_CURVE('',#28671,#28669,#15044,.T.);
#36467=EDGE_CURVE('',#28672,#28670,#15045,.T.);
#36468=EDGE_CURVE('',#28671,#28672,#15046,.T.);
#36469=EDGE_CURVE('',#28673,#28671,#15047,.T.);
#36470=EDGE_CURVE('',#28674,#28672,#15048,.T.);
#36471=EDGE_CURVE('',#28673,#28674,#15049,.T.);
#36472=EDGE_CURVE('',#28675,#28673,#15050,.T.);
#36473=EDGE_CURVE('',#28676,#28674,#15051,.T.);
#36474=EDGE_CURVE('',#28675,#28676,#15052,.T.);
#36475=EDGE_CURVE('',#28677,#28675,#15053,.T.);
#36476=EDGE_CURVE('',#28678,#28676,#15054,.T.);
#36477=EDGE_CURVE('',#28677,#28678,#15055,.T.);
#36478=EDGE_CURVE('',#28679,#28677,#15056,.T.);
#36479=EDGE_CURVE('',#28680,#28678,#15057,.T.);
#36480=EDGE_CURVE('',#28679,#28680,#15058,.T.);
#36481=EDGE_CURVE('',#28681,#28679,#15059,.T.);
#36482=EDGE_CURVE('',#28682,#28680,#15060,.T.);
#36483=EDGE_CURVE('',#28681,#28682,#15061,.T.);
#36484=EDGE_CURVE('',#28683,#28681,#15062,.T.);
#36485=EDGE_CURVE('',#28684,#28682,#15063,.T.);
#36486=EDGE_CURVE('',#28683,#28684,#15064,.T.);
#36487=EDGE_CURVE('',#28685,#28683,#15065,.T.);
#36488=EDGE_CURVE('',#28686,#28684,#15066,.T.);
#36489=EDGE_CURVE('',#28685,#28686,#15067,.T.);
#36490=EDGE_CURVE('',#28687,#28685,#15068,.T.);
#36491=EDGE_CURVE('',#28688,#28686,#15069,.T.);
#36492=EDGE_CURVE('',#28687,#28688,#15070,.T.);
#36493=EDGE_CURVE('',#28689,#28687,#15071,.T.);
#36494=EDGE_CURVE('',#28690,#28688,#15072,.T.);
#36495=EDGE_CURVE('',#28689,#28690,#15073,.T.);
#36496=EDGE_CURVE('',#28691,#28689,#15074,.T.);
#36497=EDGE_CURVE('',#28692,#28690,#15075,.T.);
#36498=EDGE_CURVE('',#28691,#28692,#15076,.T.);
#36499=EDGE_CURVE('',#28693,#28691,#15077,.T.);
#36500=EDGE_CURVE('',#28694,#28692,#15078,.T.);
#36501=EDGE_CURVE('',#28693,#28694,#15079,.T.);
#36502=EDGE_CURVE('',#28695,#28693,#15080,.T.);
#36503=EDGE_CURVE('',#28696,#28694,#15081,.T.);
#36504=EDGE_CURVE('',#28695,#28696,#15082,.T.);
#36505=EDGE_CURVE('',#28697,#28695,#15083,.T.);
#36506=EDGE_CURVE('',#28698,#28696,#15084,.T.);
#36507=EDGE_CURVE('',#28697,#28698,#15085,.T.);
#36508=EDGE_CURVE('',#28699,#28697,#15086,.T.);
#36509=EDGE_CURVE('',#28700,#28698,#15087,.T.);
#36510=EDGE_CURVE('',#28699,#28700,#15088,.T.);
#36511=EDGE_CURVE('',#28701,#28699,#15089,.T.);
#36512=EDGE_CURVE('',#28702,#28700,#15090,.T.);
#36513=EDGE_CURVE('',#28701,#28702,#15091,.T.);
#36514=EDGE_CURVE('',#28703,#28701,#15092,.T.);
#36515=EDGE_CURVE('',#28704,#28702,#15093,.T.);
#36516=EDGE_CURVE('',#28703,#28704,#15094,.T.);
#36517=EDGE_CURVE('',#28705,#28703,#15095,.T.);
#36518=EDGE_CURVE('',#28706,#28704,#15096,.T.);
#36519=EDGE_CURVE('',#28705,#28706,#15097,.T.);
#36520=EDGE_CURVE('',#28707,#28705,#15098,.T.);
#36521=EDGE_CURVE('',#28708,#28706,#15099,.T.);
#36522=EDGE_CURVE('',#28707,#28708,#15100,.T.);
#36523=EDGE_CURVE('',#28709,#28707,#15101,.T.);
#36524=EDGE_CURVE('',#28710,#28708,#15102,.T.);
#36525=EDGE_CURVE('',#28709,#28710,#15103,.T.);
#36526=EDGE_CURVE('',#28711,#28709,#15104,.T.);
#36527=EDGE_CURVE('',#28712,#28710,#15105,.T.);
#36528=EDGE_CURVE('',#28711,#28712,#15106,.T.);
#36529=EDGE_CURVE('',#28713,#28711,#15107,.T.);
#36530=EDGE_CURVE('',#28714,#28712,#15108,.T.);
#36531=EDGE_CURVE('',#28713,#28714,#15109,.T.);
#36532=EDGE_CURVE('',#28715,#28713,#15110,.T.);
#36533=EDGE_CURVE('',#28716,#28714,#15111,.T.);
#36534=EDGE_CURVE('',#28715,#28716,#15112,.T.);
#36535=EDGE_CURVE('',#28717,#28715,#15113,.T.);
#36536=EDGE_CURVE('',#28718,#28716,#15114,.T.);
#36537=EDGE_CURVE('',#28717,#28718,#15115,.T.);
#36538=EDGE_CURVE('',#28719,#28717,#15116,.T.);
#36539=EDGE_CURVE('',#28720,#28718,#15117,.T.);
#36540=EDGE_CURVE('',#28719,#28720,#15118,.T.);
#36541=EDGE_CURVE('',#28721,#28719,#15119,.T.);
#36542=EDGE_CURVE('',#28722,#28720,#15120,.T.);
#36543=EDGE_CURVE('',#28721,#28722,#15121,.T.);
#36544=EDGE_CURVE('',#28723,#28721,#15122,.T.);
#36545=EDGE_CURVE('',#28724,#28722,#15123,.T.);
#36546=EDGE_CURVE('',#28723,#28724,#15124,.T.);
#36547=EDGE_CURVE('',#28725,#28723,#15125,.T.);
#36548=EDGE_CURVE('',#28726,#28724,#15126,.T.);
#36549=EDGE_CURVE('',#28725,#28726,#15127,.T.);
#36550=EDGE_CURVE('',#28727,#28725,#15128,.T.);
#36551=EDGE_CURVE('',#28728,#28726,#15129,.T.);
#36552=EDGE_CURVE('',#28727,#28728,#15130,.T.);
#36553=EDGE_CURVE('',#28729,#28727,#15131,.T.);
#36554=EDGE_CURVE('',#28730,#28728,#15132,.T.);
#36555=EDGE_CURVE('',#28729,#28730,#15133,.T.);
#36556=EDGE_CURVE('',#28731,#28729,#15134,.T.);
#36557=EDGE_CURVE('',#28732,#28730,#15135,.T.);
#36558=EDGE_CURVE('',#28731,#28732,#15136,.T.);
#36559=EDGE_CURVE('',#28733,#28731,#15137,.T.);
#36560=EDGE_CURVE('',#28734,#28732,#15138,.T.);
#36561=EDGE_CURVE('',#28733,#28734,#15139,.T.);
#36562=EDGE_CURVE('',#28735,#28733,#15140,.T.);
#36563=EDGE_CURVE('',#28736,#28734,#15141,.T.);
#36564=EDGE_CURVE('',#28735,#28736,#15142,.T.);
#36565=EDGE_CURVE('',#28737,#28735,#15143,.T.);
#36566=EDGE_CURVE('',#28738,#28736,#15144,.T.);
#36567=EDGE_CURVE('',#28737,#28738,#15145,.T.);
#36568=EDGE_CURVE('',#28739,#28737,#15146,.T.);
#36569=EDGE_CURVE('',#28740,#28738,#15147,.T.);
#36570=EDGE_CURVE('',#28739,#28740,#15148,.T.);
#36571=EDGE_CURVE('',#28741,#28739,#15149,.T.);
#36572=EDGE_CURVE('',#28742,#28740,#15150,.T.);
#36573=EDGE_CURVE('',#28741,#28742,#15151,.T.);
#36574=EDGE_CURVE('',#28743,#28741,#15152,.T.);
#36575=EDGE_CURVE('',#28744,#28742,#15153,.T.);
#36576=EDGE_CURVE('',#28743,#28744,#15154,.T.);
#36577=EDGE_CURVE('',#28745,#28743,#15155,.T.);
#36578=EDGE_CURVE('',#28746,#28744,#15156,.T.);
#36579=EDGE_CURVE('',#28745,#28746,#15157,.T.);
#36580=EDGE_CURVE('',#28747,#28745,#15158,.T.);
#36581=EDGE_CURVE('',#28748,#28746,#15159,.T.);
#36582=EDGE_CURVE('',#28747,#28748,#15160,.T.);
#36583=EDGE_CURVE('',#28749,#28747,#15161,.T.);
#36584=EDGE_CURVE('',#28750,#28748,#15162,.T.);
#36585=EDGE_CURVE('',#28749,#28750,#15163,.T.);
#36586=EDGE_CURVE('',#28751,#28749,#15164,.T.);
#36587=EDGE_CURVE('',#28752,#28750,#15165,.T.);
#36588=EDGE_CURVE('',#28751,#28752,#15166,.T.);
#36589=EDGE_CURVE('',#28753,#28751,#15167,.T.);
#36590=EDGE_CURVE('',#28754,#28752,#15168,.T.);
#36591=EDGE_CURVE('',#28753,#28754,#15169,.T.);
#36592=EDGE_CURVE('',#28755,#28753,#15170,.T.);
#36593=EDGE_CURVE('',#28756,#28754,#15171,.T.);
#36594=EDGE_CURVE('',#28755,#28756,#15172,.T.);
#36595=EDGE_CURVE('',#28757,#28755,#15173,.T.);
#36596=EDGE_CURVE('',#28758,#28756,#15174,.T.);
#36597=EDGE_CURVE('',#28757,#28758,#15175,.T.);
#36598=EDGE_CURVE('',#28759,#28757,#15176,.T.);
#36599=EDGE_CURVE('',#28760,#28758,#15177,.T.);
#36600=EDGE_CURVE('',#28759,#28760,#15178,.T.);
#36601=EDGE_CURVE('',#28761,#28759,#15179,.T.);
#36602=EDGE_CURVE('',#28762,#28760,#15180,.T.);
#36603=EDGE_CURVE('',#28761,#28762,#15181,.T.);
#36604=EDGE_CURVE('',#28763,#28761,#15182,.T.);
#36605=EDGE_CURVE('',#28764,#28762,#15183,.T.);
#36606=EDGE_CURVE('',#28763,#28764,#15184,.T.);
#36607=EDGE_CURVE('',#28765,#28763,#15185,.T.);
#36608=EDGE_CURVE('',#28766,#28764,#15186,.T.);
#36609=EDGE_CURVE('',#28765,#28766,#15187,.T.);
#36610=EDGE_CURVE('',#28767,#28765,#15188,.T.);
#36611=EDGE_CURVE('',#28768,#28766,#15189,.T.);
#36612=EDGE_CURVE('',#28767,#28768,#15190,.T.);
#36613=EDGE_CURVE('',#28769,#28767,#15191,.T.);
#36614=EDGE_CURVE('',#28770,#28768,#15192,.T.);
#36615=EDGE_CURVE('',#28769,#28770,#15193,.T.);
#36616=EDGE_CURVE('',#28771,#28769,#15194,.T.);
#36617=EDGE_CURVE('',#28772,#28770,#15195,.T.);
#36618=EDGE_CURVE('',#28771,#28772,#15196,.T.);
#36619=EDGE_CURVE('',#28773,#28771,#15197,.T.);
#36620=EDGE_CURVE('',#28774,#28772,#15198,.T.);
#36621=EDGE_CURVE('',#28773,#28774,#15199,.T.);
#36622=EDGE_CURVE('',#28775,#28773,#15200,.T.);
#36623=EDGE_CURVE('',#28776,#28774,#15201,.T.);
#36624=EDGE_CURVE('',#28775,#28776,#15202,.T.);
#36625=EDGE_CURVE('',#28777,#28775,#15203,.T.);
#36626=EDGE_CURVE('',#28778,#28776,#15204,.T.);
#36627=EDGE_CURVE('',#28777,#28778,#15205,.T.);
#36628=EDGE_CURVE('',#28779,#28777,#15206,.T.);
#36629=EDGE_CURVE('',#28780,#28778,#15207,.T.);
#36630=EDGE_CURVE('',#28779,#28780,#15208,.T.);
#36631=EDGE_CURVE('',#28781,#28779,#15209,.T.);
#36632=EDGE_CURVE('',#28782,#28780,#15210,.T.);
#36633=EDGE_CURVE('',#28781,#28782,#15211,.T.);
#36634=EDGE_CURVE('',#28783,#28781,#15212,.T.);
#36635=EDGE_CURVE('',#28784,#28782,#15213,.T.);
#36636=EDGE_CURVE('',#28783,#28784,#15214,.T.);
#36637=EDGE_CURVE('',#28785,#28783,#15215,.T.);
#36638=EDGE_CURVE('',#28786,#28784,#15216,.T.);
#36639=EDGE_CURVE('',#28785,#28786,#15217,.T.);
#36640=EDGE_CURVE('',#28787,#28785,#15218,.T.);
#36641=EDGE_CURVE('',#28788,#28786,#15219,.T.);
#36642=EDGE_CURVE('',#28787,#28788,#15220,.T.);
#36643=EDGE_CURVE('',#28789,#28787,#15221,.T.);
#36644=EDGE_CURVE('',#28790,#28788,#15222,.T.);
#36645=EDGE_CURVE('',#28789,#28790,#15223,.T.);
#36646=EDGE_CURVE('',#28791,#28789,#15224,.T.);
#36647=EDGE_CURVE('',#28792,#28790,#15225,.T.);
#36648=EDGE_CURVE('',#28791,#28792,#15226,.T.);
#36649=EDGE_CURVE('',#28793,#28791,#15227,.T.);
#36650=EDGE_CURVE('',#28794,#28792,#15228,.T.);
#36651=EDGE_CURVE('',#28793,#28794,#15229,.T.);
#36652=EDGE_CURVE('',#28795,#28793,#15230,.T.);
#36653=EDGE_CURVE('',#28796,#28794,#15231,.T.);
#36654=EDGE_CURVE('',#28795,#28796,#15232,.T.);
#36655=EDGE_CURVE('',#28797,#28795,#15233,.T.);
#36656=EDGE_CURVE('',#28798,#28796,#15234,.T.);
#36657=EDGE_CURVE('',#28797,#28798,#15235,.T.);
#36658=EDGE_CURVE('',#28799,#28797,#15236,.T.);
#36659=EDGE_CURVE('',#28800,#28798,#15237,.T.);
#36660=EDGE_CURVE('',#28799,#28800,#15238,.T.);
#36661=EDGE_CURVE('',#28801,#28799,#15239,.T.);
#36662=EDGE_CURVE('',#28802,#28800,#15240,.T.);
#36663=EDGE_CURVE('',#28801,#28802,#15241,.T.);
#36664=EDGE_CURVE('',#28803,#28801,#15242,.T.);
#36665=EDGE_CURVE('',#28804,#28802,#15243,.T.);
#36666=EDGE_CURVE('',#28803,#28804,#15244,.T.);
#36667=EDGE_CURVE('',#28805,#28803,#15245,.T.);
#36668=EDGE_CURVE('',#28806,#28804,#15246,.T.);
#36669=EDGE_CURVE('',#28805,#28806,#15247,.T.);
#36670=EDGE_CURVE('',#28807,#28805,#15248,.T.);
#36671=EDGE_CURVE('',#28808,#28806,#15249,.T.);
#36672=EDGE_CURVE('',#28807,#28808,#15250,.T.);
#36673=EDGE_CURVE('',#28809,#28807,#15251,.T.);
#36674=EDGE_CURVE('',#28810,#28808,#15252,.T.);
#36675=EDGE_CURVE('',#28809,#28810,#15253,.T.);
#36676=EDGE_CURVE('',#28811,#28809,#15254,.T.);
#36677=EDGE_CURVE('',#28812,#28810,#15255,.T.);
#36678=EDGE_CURVE('',#28811,#28812,#15256,.T.);
#36679=EDGE_CURVE('',#28813,#28811,#15257,.T.);
#36680=EDGE_CURVE('',#28814,#28812,#15258,.T.);
#36681=EDGE_CURVE('',#28813,#28814,#15259,.T.);
#36682=EDGE_CURVE('',#28815,#28813,#15260,.T.);
#36683=EDGE_CURVE('',#28816,#28814,#15261,.T.);
#36684=EDGE_CURVE('',#28815,#28816,#15262,.T.);
#36685=EDGE_CURVE('',#28817,#28815,#15263,.T.);
#36686=EDGE_CURVE('',#28818,#28816,#15264,.T.);
#36687=EDGE_CURVE('',#28817,#28818,#15265,.T.);
#36688=EDGE_CURVE('',#28819,#28817,#15266,.T.);
#36689=EDGE_CURVE('',#28820,#28818,#15267,.T.);
#36690=EDGE_CURVE('',#28819,#28820,#15268,.T.);
#36691=EDGE_CURVE('',#28821,#28819,#15269,.T.);
#36692=EDGE_CURVE('',#28822,#28820,#15270,.T.);
#36693=EDGE_CURVE('',#28821,#28822,#15271,.T.);
#36694=EDGE_CURVE('',#28823,#28821,#15272,.T.);
#36695=EDGE_CURVE('',#28824,#28822,#15273,.T.);
#36696=EDGE_CURVE('',#28823,#28824,#15274,.T.);
#36697=EDGE_CURVE('',#28825,#28823,#15275,.T.);
#36698=EDGE_CURVE('',#28826,#28824,#15276,.T.);
#36699=EDGE_CURVE('',#28825,#28826,#15277,.T.);
#36700=EDGE_CURVE('',#28827,#28825,#15278,.T.);
#36701=EDGE_CURVE('',#28828,#28826,#15279,.T.);
#36702=EDGE_CURVE('',#28827,#28828,#15280,.T.);
#36703=EDGE_CURVE('',#28829,#28827,#15281,.T.);
#36704=EDGE_CURVE('',#28830,#28828,#15282,.T.);
#36705=EDGE_CURVE('',#28829,#28830,#15283,.T.);
#36706=EDGE_CURVE('',#28831,#28829,#15284,.T.);
#36707=EDGE_CURVE('',#28832,#28830,#15285,.T.);
#36708=EDGE_CURVE('',#28831,#28832,#15286,.T.);
#36709=EDGE_CURVE('',#28833,#28831,#15287,.T.);
#36710=EDGE_CURVE('',#28834,#28832,#15288,.T.);
#36711=EDGE_CURVE('',#28833,#28834,#15289,.T.);
#36712=EDGE_CURVE('',#28835,#28833,#15290,.T.);
#36713=EDGE_CURVE('',#28836,#28834,#15291,.T.);
#36714=EDGE_CURVE('',#28835,#28836,#15292,.T.);
#36715=EDGE_CURVE('',#28837,#28835,#15293,.T.);
#36716=EDGE_CURVE('',#28838,#28836,#15294,.T.);
#36717=EDGE_CURVE('',#28837,#28838,#15295,.T.);
#36718=EDGE_CURVE('',#28839,#28837,#15296,.T.);
#36719=EDGE_CURVE('',#28840,#28838,#15297,.T.);
#36720=EDGE_CURVE('',#28839,#28840,#15298,.T.);
#36721=EDGE_CURVE('',#28841,#28839,#15299,.T.);
#36722=EDGE_CURVE('',#28842,#28840,#15300,.T.);
#36723=EDGE_CURVE('',#28841,#28842,#15301,.T.);
#36724=EDGE_CURVE('',#28843,#28841,#15302,.T.);
#36725=EDGE_CURVE('',#28844,#28842,#15303,.T.);
#36726=EDGE_CURVE('',#28843,#28844,#15304,.T.);
#36727=EDGE_CURVE('',#28845,#28843,#15305,.T.);
#36728=EDGE_CURVE('',#28846,#28844,#15306,.T.);
#36729=EDGE_CURVE('',#28845,#28846,#15307,.T.);
#36730=EDGE_CURVE('',#28847,#28845,#15308,.T.);
#36731=EDGE_CURVE('',#28848,#28846,#15309,.T.);
#36732=EDGE_CURVE('',#28847,#28848,#15310,.T.);
#36733=EDGE_CURVE('',#28849,#28847,#15311,.T.);
#36734=EDGE_CURVE('',#28850,#28848,#15312,.T.);
#36735=EDGE_CURVE('',#28849,#28850,#15313,.T.);
#36736=EDGE_CURVE('',#28851,#28849,#15314,.T.);
#36737=EDGE_CURVE('',#28852,#28850,#15315,.T.);
#36738=EDGE_CURVE('',#28851,#28852,#15316,.T.);
#36739=EDGE_CURVE('',#28853,#28851,#15317,.T.);
#36740=EDGE_CURVE('',#28854,#28852,#15318,.T.);
#36741=EDGE_CURVE('',#28853,#28854,#15319,.T.);
#36742=EDGE_CURVE('',#28855,#28853,#15320,.T.);
#36743=EDGE_CURVE('',#28856,#28854,#15321,.T.);
#36744=EDGE_CURVE('',#28855,#28856,#15322,.T.);
#36745=EDGE_CURVE('',#28857,#28855,#15323,.T.);
#36746=EDGE_CURVE('',#28858,#28856,#15324,.T.);
#36747=EDGE_CURVE('',#28857,#28858,#15325,.T.);
#36748=EDGE_CURVE('',#28859,#28857,#15326,.T.);
#36749=EDGE_CURVE('',#28860,#28858,#15327,.T.);
#36750=EDGE_CURVE('',#28859,#28860,#15328,.T.);
#36751=EDGE_CURVE('',#28861,#28859,#15329,.T.);
#36752=EDGE_CURVE('',#28862,#28860,#15330,.T.);
#36753=EDGE_CURVE('',#28861,#28862,#15331,.T.);
#36754=EDGE_CURVE('',#28863,#28861,#15332,.T.);
#36755=EDGE_CURVE('',#28864,#28862,#15333,.T.);
#36756=EDGE_CURVE('',#28863,#28864,#15334,.T.);
#36757=EDGE_CURVE('',#28865,#28863,#15335,.T.);
#36758=EDGE_CURVE('',#28866,#28864,#15336,.T.);
#36759=EDGE_CURVE('',#28865,#28866,#15337,.T.);
#36760=EDGE_CURVE('',#28867,#28865,#15338,.T.);
#36761=EDGE_CURVE('',#28868,#28866,#15339,.T.);
#36762=EDGE_CURVE('',#28867,#28868,#15340,.T.);
#36763=EDGE_CURVE('',#28869,#28867,#15341,.T.);
#36764=EDGE_CURVE('',#28870,#28868,#15342,.T.);
#36765=EDGE_CURVE('',#28869,#28870,#15343,.T.);
#36766=EDGE_CURVE('',#28871,#28869,#15344,.T.);
#36767=EDGE_CURVE('',#28872,#28870,#15345,.T.);
#36768=EDGE_CURVE('',#28871,#28872,#15346,.T.);
#36769=EDGE_CURVE('',#28873,#28871,#15347,.T.);
#36770=EDGE_CURVE('',#28874,#28872,#15348,.T.);
#36771=EDGE_CURVE('',#28873,#28874,#15349,.T.);
#36772=EDGE_CURVE('',#28875,#28873,#15350,.T.);
#36773=EDGE_CURVE('',#28876,#28874,#15351,.T.);
#36774=EDGE_CURVE('',#28875,#28876,#15352,.T.);
#36775=EDGE_CURVE('',#28877,#28875,#15353,.T.);
#36776=EDGE_CURVE('',#28878,#28876,#15354,.T.);
#36777=EDGE_CURVE('',#28877,#28878,#15355,.T.);
#36778=EDGE_CURVE('',#28879,#28877,#15356,.T.);
#36779=EDGE_CURVE('',#28880,#28878,#15357,.T.);
#36780=EDGE_CURVE('',#28879,#28880,#15358,.T.);
#36781=EDGE_CURVE('',#28881,#28879,#15359,.T.);
#36782=EDGE_CURVE('',#28882,#28880,#15360,.T.);
#36783=EDGE_CURVE('',#28881,#28882,#15361,.T.);
#36784=EDGE_CURVE('',#28883,#28881,#15362,.T.);
#36785=EDGE_CURVE('',#28884,#28882,#15363,.T.);
#36786=EDGE_CURVE('',#28883,#28884,#15364,.T.);
#36787=EDGE_CURVE('',#28885,#28883,#15365,.T.);
#36788=EDGE_CURVE('',#28886,#28884,#15366,.T.);
#36789=EDGE_CURVE('',#28885,#28886,#15367,.T.);
#36790=EDGE_CURVE('',#28887,#28885,#15368,.T.);
#36791=EDGE_CURVE('',#28888,#28886,#15369,.T.);
#36792=EDGE_CURVE('',#28887,#28888,#15370,.T.);
#36793=EDGE_CURVE('',#28889,#28887,#15371,.T.);
#36794=EDGE_CURVE('',#28890,#28888,#15372,.T.);
#36795=EDGE_CURVE('',#28889,#28890,#15373,.T.);
#36796=EDGE_CURVE('',#28891,#28889,#15374,.T.);
#36797=EDGE_CURVE('',#28892,#28890,#15375,.T.);
#36798=EDGE_CURVE('',#28891,#28892,#15376,.T.);
#36799=EDGE_CURVE('',#28893,#28891,#15377,.T.);
#36800=EDGE_CURVE('',#28894,#28892,#15378,.T.);
#36801=EDGE_CURVE('',#28893,#28894,#15379,.T.);
#36802=EDGE_CURVE('',#28895,#28893,#15380,.T.);
#36803=EDGE_CURVE('',#28896,#28894,#15381,.T.);
#36804=EDGE_CURVE('',#28895,#28896,#15382,.T.);
#36805=EDGE_CURVE('',#28897,#28895,#15383,.T.);
#36806=EDGE_CURVE('',#28898,#28896,#15384,.T.);
#36807=EDGE_CURVE('',#28897,#28898,#15385,.T.);
#36808=EDGE_CURVE('',#28899,#28897,#15386,.T.);
#36809=EDGE_CURVE('',#28900,#28898,#15387,.T.);
#36810=EDGE_CURVE('',#28899,#28900,#15388,.T.);
#36811=EDGE_CURVE('',#28901,#28899,#15389,.T.);
#36812=EDGE_CURVE('',#28902,#28900,#15390,.T.);
#36813=EDGE_CURVE('',#28901,#28902,#15391,.T.);
#36814=EDGE_CURVE('',#28903,#28901,#15392,.T.);
#36815=EDGE_CURVE('',#28904,#28902,#15393,.T.);
#36816=EDGE_CURVE('',#28903,#28904,#15394,.T.);
#36817=EDGE_CURVE('',#28905,#28903,#15395,.T.);
#36818=EDGE_CURVE('',#28906,#28904,#15396,.T.);
#36819=EDGE_CURVE('',#28905,#28906,#15397,.T.);
#36820=EDGE_CURVE('',#28907,#28905,#15398,.T.);
#36821=EDGE_CURVE('',#28908,#28906,#15399,.T.);
#36822=EDGE_CURVE('',#28907,#28908,#15400,.T.);
#36823=EDGE_CURVE('',#28909,#28907,#15401,.T.);
#36824=EDGE_CURVE('',#28910,#28908,#15402,.T.);
#36825=EDGE_CURVE('',#28909,#28910,#15403,.T.);
#36826=EDGE_CURVE('',#28911,#28909,#15404,.T.);
#36827=EDGE_CURVE('',#28912,#28910,#15405,.T.);
#36828=EDGE_CURVE('',#28911,#28912,#15406,.T.);
#36829=EDGE_CURVE('',#28913,#28911,#15407,.T.);
#36830=EDGE_CURVE('',#28914,#28912,#15408,.T.);
#36831=EDGE_CURVE('',#28913,#28914,#15409,.T.);
#36832=EDGE_CURVE('',#28915,#28913,#15410,.T.);
#36833=EDGE_CURVE('',#28916,#28914,#15411,.T.);
#36834=EDGE_CURVE('',#28915,#28916,#15412,.T.);
#36835=EDGE_CURVE('',#28917,#28915,#15413,.T.);
#36836=EDGE_CURVE('',#28918,#28916,#15414,.T.);
#36837=EDGE_CURVE('',#28917,#28918,#15415,.T.);
#36838=EDGE_CURVE('',#28919,#28917,#15416,.T.);
#36839=EDGE_CURVE('',#28920,#28918,#15417,.T.);
#36840=EDGE_CURVE('',#28919,#28920,#15418,.T.);
#36841=EDGE_CURVE('',#28921,#28919,#15419,.T.);
#36842=EDGE_CURVE('',#28922,#28920,#15420,.T.);
#36843=EDGE_CURVE('',#28921,#28922,#15421,.T.);
#36844=EDGE_CURVE('',#28923,#28921,#15422,.T.);
#36845=EDGE_CURVE('',#28924,#28922,#15423,.T.);
#36846=EDGE_CURVE('',#28923,#28924,#15424,.T.);
#36847=EDGE_CURVE('',#28925,#28923,#15425,.T.);
#36848=EDGE_CURVE('',#28926,#28924,#15426,.T.);
#36849=EDGE_CURVE('',#28925,#28926,#15427,.T.);
#36850=EDGE_CURVE('',#28927,#28925,#15428,.T.);
#36851=EDGE_CURVE('',#28928,#28926,#15429,.T.);
#36852=EDGE_CURVE('',#28927,#28928,#15430,.T.);
#36853=EDGE_CURVE('',#28929,#28927,#15431,.T.);
#36854=EDGE_CURVE('',#28930,#28928,#15432,.T.);
#36855=EDGE_CURVE('',#28929,#28930,#15433,.T.);
#36856=EDGE_CURVE('',#28931,#28929,#15434,.T.);
#36857=EDGE_CURVE('',#28932,#28930,#15435,.T.);
#36858=EDGE_CURVE('',#28931,#28932,#15436,.T.);
#36859=EDGE_CURVE('',#28933,#28931,#15437,.T.);
#36860=EDGE_CURVE('',#28934,#28932,#15438,.T.);
#36861=EDGE_CURVE('',#28933,#28934,#15439,.T.);
#36862=EDGE_CURVE('',#28935,#28933,#15440,.T.);
#36863=EDGE_CURVE('',#28936,#28934,#15441,.T.);
#36864=EDGE_CURVE('',#28935,#28936,#15442,.T.);
#36865=EDGE_CURVE('',#28937,#28935,#15443,.T.);
#36866=EDGE_CURVE('',#28938,#28936,#15444,.T.);
#36867=EDGE_CURVE('',#28937,#28938,#15445,.T.);
#36868=EDGE_CURVE('',#28939,#28937,#15446,.T.);
#36869=EDGE_CURVE('',#28940,#28938,#15447,.T.);
#36870=EDGE_CURVE('',#28939,#28940,#15448,.T.);
#36871=EDGE_CURVE('',#28941,#28939,#15449,.T.);
#36872=EDGE_CURVE('',#28942,#28940,#15450,.T.);
#36873=EDGE_CURVE('',#28941,#28942,#15451,.T.);
#36874=EDGE_CURVE('',#28943,#28941,#15452,.T.);
#36875=EDGE_CURVE('',#28944,#28942,#15453,.T.);
#36876=EDGE_CURVE('',#28943,#28944,#15454,.T.);
#36877=EDGE_CURVE('',#28945,#28943,#15455,.T.);
#36878=EDGE_CURVE('',#28946,#28944,#15456,.T.);
#36879=EDGE_CURVE('',#28945,#28946,#15457,.T.);
#36880=EDGE_CURVE('',#28947,#28945,#15458,.T.);
#36881=EDGE_CURVE('',#28948,#28946,#15459,.T.);
#36882=EDGE_CURVE('',#28947,#28948,#15460,.T.);
#36883=EDGE_CURVE('',#28949,#28947,#15461,.T.);
#36884=EDGE_CURVE('',#28950,#28948,#15462,.T.);
#36885=EDGE_CURVE('',#28949,#28950,#15463,.T.);
#36886=EDGE_CURVE('',#28951,#28949,#15464,.T.);
#36887=EDGE_CURVE('',#28952,#28950,#15465,.T.);
#36888=EDGE_CURVE('',#28951,#28952,#15466,.T.);
#36889=EDGE_CURVE('',#28953,#28951,#15467,.T.);
#36890=EDGE_CURVE('',#28954,#28952,#15468,.T.);
#36891=EDGE_CURVE('',#28953,#28954,#15469,.T.);
#36892=EDGE_CURVE('',#28955,#28953,#15470,.T.);
#36893=EDGE_CURVE('',#28956,#28954,#15471,.T.);
#36894=EDGE_CURVE('',#28955,#28956,#15472,.T.);
#36895=EDGE_CURVE('',#28957,#28955,#15473,.T.);
#36896=EDGE_CURVE('',#28958,#28956,#15474,.T.);
#36897=EDGE_CURVE('',#28957,#28958,#15475,.T.);
#36898=EDGE_CURVE('',#28959,#28957,#15476,.T.);
#36899=EDGE_CURVE('',#28960,#28958,#15477,.T.);
#36900=EDGE_CURVE('',#28959,#28960,#15478,.T.);
#36901=EDGE_CURVE('',#28961,#28959,#15479,.T.);
#36902=EDGE_CURVE('',#28962,#28960,#15480,.T.);
#36903=EDGE_CURVE('',#28961,#28962,#15481,.T.);
#36904=EDGE_CURVE('',#28963,#28961,#15482,.T.);
#36905=EDGE_CURVE('',#28964,#28962,#15483,.T.);
#36906=EDGE_CURVE('',#28963,#28964,#15484,.T.);
#36907=EDGE_CURVE('',#28965,#28963,#15485,.T.);
#36908=EDGE_CURVE('',#28966,#28964,#15486,.T.);
#36909=EDGE_CURVE('',#28965,#28966,#15487,.T.);
#36910=EDGE_CURVE('',#28967,#28965,#15488,.T.);
#36911=EDGE_CURVE('',#28968,#28966,#15489,.T.);
#36912=EDGE_CURVE('',#28967,#28968,#15490,.T.);
#36913=EDGE_CURVE('',#28969,#28967,#15491,.T.);
#36914=EDGE_CURVE('',#28970,#28968,#15492,.T.);
#36915=EDGE_CURVE('',#28969,#28970,#15493,.T.);
#36916=EDGE_CURVE('',#28971,#28969,#15494,.T.);
#36917=EDGE_CURVE('',#28972,#28970,#15495,.T.);
#36918=EDGE_CURVE('',#28971,#28972,#15496,.T.);
#36919=EDGE_CURVE('',#28973,#28971,#15497,.T.);
#36920=EDGE_CURVE('',#28974,#28972,#15498,.T.);
#36921=EDGE_CURVE('',#28973,#28974,#15499,.T.);
#36922=EDGE_CURVE('',#28975,#28973,#15500,.T.);
#36923=EDGE_CURVE('',#28976,#28974,#15501,.T.);
#36924=EDGE_CURVE('',#28975,#28976,#15502,.T.);
#36925=EDGE_CURVE('',#28977,#28975,#15503,.T.);
#36926=EDGE_CURVE('',#28978,#28976,#15504,.T.);
#36927=EDGE_CURVE('',#28977,#28978,#15505,.T.);
#36928=EDGE_CURVE('',#28979,#28977,#15506,.T.);
#36929=EDGE_CURVE('',#28980,#28978,#15507,.T.);
#36930=EDGE_CURVE('',#28979,#28980,#15508,.T.);
#36931=EDGE_CURVE('',#28981,#28979,#15509,.T.);
#36932=EDGE_CURVE('',#28982,#28980,#15510,.T.);
#36933=EDGE_CURVE('',#28981,#28982,#15511,.T.);
#36934=EDGE_CURVE('',#28983,#28981,#15512,.T.);
#36935=EDGE_CURVE('',#28984,#28982,#15513,.T.);
#36936=EDGE_CURVE('',#28983,#28984,#15514,.T.);
#36937=EDGE_CURVE('',#28985,#28983,#15515,.T.);
#36938=EDGE_CURVE('',#28986,#28984,#15516,.T.);
#36939=EDGE_CURVE('',#28985,#28986,#15517,.T.);
#36940=EDGE_CURVE('',#28987,#28985,#15518,.T.);
#36941=EDGE_CURVE('',#28988,#28986,#15519,.T.);
#36942=EDGE_CURVE('',#28987,#28988,#15520,.T.);
#36943=EDGE_CURVE('',#28989,#28987,#15521,.T.);
#36944=EDGE_CURVE('',#28990,#28988,#15522,.T.);
#36945=EDGE_CURVE('',#28989,#28990,#15523,.T.);
#36946=EDGE_CURVE('',#28991,#28989,#15524,.T.);
#36947=EDGE_CURVE('',#28992,#28990,#15525,.T.);
#36948=EDGE_CURVE('',#28991,#28992,#15526,.T.);
#36949=EDGE_CURVE('',#28993,#28991,#15527,.T.);
#36950=EDGE_CURVE('',#28994,#28992,#15528,.T.);
#36951=EDGE_CURVE('',#28993,#28994,#15529,.T.);
#36952=EDGE_CURVE('',#28995,#28993,#15530,.T.);
#36953=EDGE_CURVE('',#28996,#28994,#15531,.T.);
#36954=EDGE_CURVE('',#28995,#28996,#15532,.T.);
#36955=EDGE_CURVE('',#28997,#28995,#15533,.T.);
#36956=EDGE_CURVE('',#28998,#28996,#15534,.T.);
#36957=EDGE_CURVE('',#28997,#28998,#15535,.T.);
#36958=EDGE_CURVE('',#28999,#28997,#15536,.T.);
#36959=EDGE_CURVE('',#29000,#28998,#15537,.T.);
#36960=EDGE_CURVE('',#28999,#29000,#15538,.T.);
#36961=EDGE_CURVE('',#29001,#28999,#15539,.T.);
#36962=EDGE_CURVE('',#29002,#29000,#15540,.T.);
#36963=EDGE_CURVE('',#29001,#29002,#15541,.T.);
#36964=EDGE_CURVE('',#29003,#29001,#15542,.T.);
#36965=EDGE_CURVE('',#29004,#29002,#15543,.T.);
#36966=EDGE_CURVE('',#29003,#29004,#15544,.T.);
#36967=EDGE_CURVE('',#29005,#29003,#15545,.T.);
#36968=EDGE_CURVE('',#29006,#29004,#15546,.T.);
#36969=EDGE_CURVE('',#29005,#29006,#15547,.T.);
#36970=EDGE_CURVE('',#29007,#29005,#15548,.T.);
#36971=EDGE_CURVE('',#29008,#29006,#15549,.T.);
#36972=EDGE_CURVE('',#29007,#29008,#15550,.T.);
#36973=EDGE_CURVE('',#29009,#29007,#15551,.T.);
#36974=EDGE_CURVE('',#29010,#29008,#15552,.T.);
#36975=EDGE_CURVE('',#29009,#29010,#15553,.T.);
#36976=EDGE_CURVE('',#29011,#29009,#15554,.T.);
#36977=EDGE_CURVE('',#29012,#29010,#15555,.T.);
#36978=EDGE_CURVE('',#29011,#29012,#15556,.T.);
#36979=EDGE_CURVE('',#29013,#29011,#15557,.T.);
#36980=EDGE_CURVE('',#29014,#29012,#15558,.T.);
#36981=EDGE_CURVE('',#29013,#29014,#15559,.T.);
#36982=EDGE_CURVE('',#29015,#29013,#15560,.T.);
#36983=EDGE_CURVE('',#29016,#29014,#15561,.T.);
#36984=EDGE_CURVE('',#29015,#29016,#15562,.T.);
#36985=EDGE_CURVE('',#29017,#29015,#15563,.T.);
#36986=EDGE_CURVE('',#29018,#29016,#15564,.T.);
#36987=EDGE_CURVE('',#29017,#29018,#15565,.T.);
#36988=EDGE_CURVE('',#29019,#29017,#15566,.T.);
#36989=EDGE_CURVE('',#29020,#29018,#15567,.T.);
#36990=EDGE_CURVE('',#29019,#29020,#15568,.T.);
#36991=EDGE_CURVE('',#29021,#29019,#15569,.T.);
#36992=EDGE_CURVE('',#29022,#29020,#15570,.T.);
#36993=EDGE_CURVE('',#29021,#29022,#15571,.T.);
#36994=EDGE_CURVE('',#29023,#29021,#15572,.T.);
#36995=EDGE_CURVE('',#29024,#29022,#15573,.T.);
#36996=EDGE_CURVE('',#29023,#29024,#15574,.T.);
#36997=EDGE_CURVE('',#29025,#29023,#15575,.T.);
#36998=EDGE_CURVE('',#29026,#29024,#15576,.T.);
#36999=EDGE_CURVE('',#29025,#29026,#15577,.T.);
#37000=EDGE_CURVE('',#29027,#29025,#15578,.T.);
#37001=EDGE_CURVE('',#29028,#29026,#15579,.T.);
#37002=EDGE_CURVE('',#29027,#29028,#15580,.T.);
#37003=EDGE_CURVE('',#29029,#29027,#15581,.T.);
#37004=EDGE_CURVE('',#29030,#29028,#15582,.T.);
#37005=EDGE_CURVE('',#29029,#29030,#15583,.T.);
#37006=EDGE_CURVE('',#29031,#29029,#15584,.T.);
#37007=EDGE_CURVE('',#29032,#29030,#15585,.T.);
#37008=EDGE_CURVE('',#29031,#29032,#15586,.T.);
#37009=EDGE_CURVE('',#29033,#29031,#15587,.T.);
#37010=EDGE_CURVE('',#29034,#29032,#15588,.T.);
#37011=EDGE_CURVE('',#29033,#29034,#15589,.T.);
#37012=EDGE_CURVE('',#29035,#29033,#15590,.T.);
#37013=EDGE_CURVE('',#29036,#29034,#15591,.T.);
#37014=EDGE_CURVE('',#29035,#29036,#15592,.T.);
#37015=EDGE_CURVE('',#29037,#29035,#15593,.T.);
#37016=EDGE_CURVE('',#29038,#29036,#15594,.T.);
#37017=EDGE_CURVE('',#29037,#29038,#15595,.T.);
#37018=EDGE_CURVE('',#29039,#29037,#15596,.T.);
#37019=EDGE_CURVE('',#29040,#29038,#15597,.T.);
#37020=EDGE_CURVE('',#29039,#29040,#15598,.T.);
#37021=EDGE_CURVE('',#29041,#29039,#15599,.T.);
#37022=EDGE_CURVE('',#29042,#29040,#15600,.T.);
#37023=EDGE_CURVE('',#29041,#29042,#15601,.T.);
#37024=EDGE_CURVE('',#29043,#29041,#15602,.T.);
#37025=EDGE_CURVE('',#29044,#29042,#15603,.T.);
#37026=EDGE_CURVE('',#29043,#29044,#15604,.T.);
#37027=EDGE_CURVE('',#29045,#29043,#15605,.T.);
#37028=EDGE_CURVE('',#29046,#29044,#15606,.T.);
#37029=EDGE_CURVE('',#29045,#29046,#15607,.T.);
#37030=EDGE_CURVE('',#29047,#29045,#15608,.T.);
#37031=EDGE_CURVE('',#29048,#29046,#15609,.T.);
#37032=EDGE_CURVE('',#29047,#29048,#15610,.T.);
#37033=EDGE_CURVE('',#29049,#29047,#15611,.T.);
#37034=EDGE_CURVE('',#29050,#29048,#15612,.T.);
#37035=EDGE_CURVE('',#29049,#29050,#15613,.T.);
#37036=EDGE_CURVE('',#29051,#29049,#15614,.T.);
#37037=EDGE_CURVE('',#29052,#29050,#15615,.T.);
#37038=EDGE_CURVE('',#29051,#29052,#15616,.T.);
#37039=EDGE_CURVE('',#29053,#29051,#15617,.T.);
#37040=EDGE_CURVE('',#29054,#29052,#15618,.T.);
#37041=EDGE_CURVE('',#29053,#29054,#15619,.T.);
#37042=EDGE_CURVE('',#29055,#29053,#15620,.T.);
#37043=EDGE_CURVE('',#29056,#29054,#15621,.T.);
#37044=EDGE_CURVE('',#29055,#29056,#15622,.T.);
#37045=EDGE_CURVE('',#29057,#29055,#15623,.T.);
#37046=EDGE_CURVE('',#29058,#29056,#15624,.T.);
#37047=EDGE_CURVE('',#29057,#29058,#15625,.T.);
#37048=EDGE_CURVE('',#29059,#29057,#15626,.T.);
#37049=EDGE_CURVE('',#29060,#29058,#15627,.T.);
#37050=EDGE_CURVE('',#29059,#29060,#15628,.T.);
#37051=EDGE_CURVE('',#29061,#29059,#15629,.T.);
#37052=EDGE_CURVE('',#29062,#29060,#15630,.T.);
#37053=EDGE_CURVE('',#29061,#29062,#15631,.T.);
#37054=EDGE_CURVE('',#29063,#29061,#15632,.T.);
#37055=EDGE_CURVE('',#29064,#29062,#15633,.T.);
#37056=EDGE_CURVE('',#29063,#29064,#15634,.T.);
#37057=EDGE_CURVE('',#29065,#29063,#15635,.T.);
#37058=EDGE_CURVE('',#29066,#29064,#15636,.T.);
#37059=EDGE_CURVE('',#29065,#29066,#15637,.T.);
#37060=EDGE_CURVE('',#29067,#29065,#15638,.T.);
#37061=EDGE_CURVE('',#29068,#29066,#15639,.T.);
#37062=EDGE_CURVE('',#29067,#29068,#15640,.T.);
#37063=EDGE_CURVE('',#29069,#29067,#15641,.T.);
#37064=EDGE_CURVE('',#29070,#29068,#15642,.T.);
#37065=EDGE_CURVE('',#29069,#29070,#15643,.T.);
#37066=EDGE_CURVE('',#29071,#29069,#15644,.T.);
#37067=EDGE_CURVE('',#29072,#29070,#15645,.T.);
#37068=EDGE_CURVE('',#29071,#29072,#15646,.T.);
#37069=EDGE_CURVE('',#29073,#29071,#15647,.T.);
#37070=EDGE_CURVE('',#29074,#29072,#15648,.T.);
#37071=EDGE_CURVE('',#29073,#29074,#15649,.T.);
#37072=EDGE_CURVE('',#29075,#29073,#15650,.T.);
#37073=EDGE_CURVE('',#29076,#29074,#15651,.T.);
#37074=EDGE_CURVE('',#29075,#29076,#15652,.T.);
#37075=EDGE_CURVE('',#29077,#29075,#15653,.T.);
#37076=EDGE_CURVE('',#29078,#29076,#15654,.T.);
#37077=EDGE_CURVE('',#29077,#29078,#15655,.T.);
#37078=EDGE_CURVE('',#29079,#29077,#15656,.T.);
#37079=EDGE_CURVE('',#29080,#29078,#15657,.T.);
#37080=EDGE_CURVE('',#29079,#29080,#15658,.T.);
#37081=EDGE_CURVE('',#29081,#29079,#15659,.T.);
#37082=EDGE_CURVE('',#29082,#29080,#15660,.T.);
#37083=EDGE_CURVE('',#29081,#29082,#15661,.T.);
#37084=EDGE_CURVE('',#29083,#29081,#15662,.T.);
#37085=EDGE_CURVE('',#29084,#29082,#15663,.T.);
#37086=EDGE_CURVE('',#29083,#29084,#15664,.T.);
#37087=EDGE_CURVE('',#29085,#29083,#15665,.T.);
#37088=EDGE_CURVE('',#29086,#29084,#15666,.T.);
#37089=EDGE_CURVE('',#29085,#29086,#15667,.T.);
#37090=EDGE_CURVE('',#29087,#29085,#15668,.T.);
#37091=EDGE_CURVE('',#29088,#29086,#15669,.T.);
#37092=EDGE_CURVE('',#29087,#29088,#15670,.T.);
#37093=EDGE_CURVE('',#29089,#29087,#15671,.T.);
#37094=EDGE_CURVE('',#29090,#29088,#15672,.T.);
#37095=EDGE_CURVE('',#29089,#29090,#15673,.T.);
#37096=EDGE_CURVE('',#29091,#29089,#15674,.T.);
#37097=EDGE_CURVE('',#29092,#29090,#15675,.T.);
#37098=EDGE_CURVE('',#29091,#29092,#15676,.T.);
#37099=EDGE_CURVE('',#29093,#29091,#15677,.T.);
#37100=EDGE_CURVE('',#29094,#29092,#15678,.T.);
#37101=EDGE_CURVE('',#29093,#29094,#15679,.T.);
#37102=EDGE_CURVE('',#29095,#29093,#15680,.T.);
#37103=EDGE_CURVE('',#29096,#29094,#15681,.T.);
#37104=EDGE_CURVE('',#29095,#29096,#15682,.T.);
#37105=EDGE_CURVE('',#29097,#29095,#15683,.T.);
#37106=EDGE_CURVE('',#29098,#29096,#15684,.T.);
#37107=EDGE_CURVE('',#29097,#29098,#15685,.T.);
#37108=EDGE_CURVE('',#29099,#29097,#15686,.T.);
#37109=EDGE_CURVE('',#29100,#29098,#15687,.T.);
#37110=EDGE_CURVE('',#29099,#29100,#15688,.T.);
#37111=EDGE_CURVE('',#29101,#29099,#15689,.T.);
#37112=EDGE_CURVE('',#29102,#29100,#15690,.T.);
#37113=EDGE_CURVE('',#29101,#29102,#15691,.T.);
#37114=EDGE_CURVE('',#29103,#29101,#15692,.T.);
#37115=EDGE_CURVE('',#29104,#29102,#15693,.T.);
#37116=EDGE_CURVE('',#29103,#29104,#15694,.T.);
#37117=EDGE_CURVE('',#29105,#29103,#15695,.T.);
#37118=EDGE_CURVE('',#29106,#29104,#15696,.T.);
#37119=EDGE_CURVE('',#29105,#29106,#15697,.T.);
#37120=EDGE_CURVE('',#29107,#29105,#15698,.T.);
#37121=EDGE_CURVE('',#29108,#29106,#15699,.T.);
#37122=EDGE_CURVE('',#29107,#29108,#15700,.T.);
#37123=EDGE_CURVE('',#29109,#29107,#15701,.T.);
#37124=EDGE_CURVE('',#29110,#29108,#15702,.T.);
#37125=EDGE_CURVE('',#29109,#29110,#15703,.T.);
#37126=EDGE_CURVE('',#29111,#29109,#15704,.T.);
#37127=EDGE_CURVE('',#29112,#29110,#15705,.T.);
#37128=EDGE_CURVE('',#29111,#29112,#15706,.T.);
#37129=EDGE_CURVE('',#29113,#29111,#15707,.T.);
#37130=EDGE_CURVE('',#29114,#29112,#15708,.T.);
#37131=EDGE_CURVE('',#29113,#29114,#15709,.T.);
#37132=EDGE_CURVE('',#29115,#29113,#15710,.T.);
#37133=EDGE_CURVE('',#29116,#29114,#15711,.T.);
#37134=EDGE_CURVE('',#29115,#29116,#15712,.T.);
#37135=EDGE_CURVE('',#29117,#29115,#15713,.T.);
#37136=EDGE_CURVE('',#29118,#29116,#15714,.T.);
#37137=EDGE_CURVE('',#29117,#29118,#15715,.T.);
#37138=EDGE_CURVE('',#29119,#29117,#15716,.T.);
#37139=EDGE_CURVE('',#29120,#29118,#15717,.T.);
#37140=EDGE_CURVE('',#29119,#29120,#15718,.T.);
#37141=EDGE_CURVE('',#29121,#29119,#15719,.T.);
#37142=EDGE_CURVE('',#29122,#29120,#15720,.T.);
#37143=EDGE_CURVE('',#29121,#29122,#15721,.T.);
#37144=EDGE_CURVE('',#29123,#29121,#15722,.T.);
#37145=EDGE_CURVE('',#29124,#29122,#15723,.T.);
#37146=EDGE_CURVE('',#29123,#29124,#15724,.T.);
#37147=EDGE_CURVE('',#29125,#29123,#15725,.T.);
#37148=EDGE_CURVE('',#29126,#29124,#15726,.T.);
#37149=EDGE_CURVE('',#29125,#29126,#15727,.T.);
#37150=EDGE_CURVE('',#29127,#29125,#15728,.T.);
#37151=EDGE_CURVE('',#29128,#29126,#15729,.T.);
#37152=EDGE_CURVE('',#29127,#29128,#15730,.T.);
#37153=EDGE_CURVE('',#29129,#29127,#15731,.T.);
#37154=EDGE_CURVE('',#29130,#29128,#15732,.T.);
#37155=EDGE_CURVE('',#29129,#29130,#15733,.T.);
#37156=EDGE_CURVE('',#29131,#29129,#15734,.T.);
#37157=EDGE_CURVE('',#29132,#29130,#15735,.T.);
#37158=EDGE_CURVE('',#29131,#29132,#15736,.T.);
#37159=EDGE_CURVE('',#29133,#29131,#15737,.T.);
#37160=EDGE_CURVE('',#29134,#29132,#15738,.T.);
#37161=EDGE_CURVE('',#29133,#29134,#15739,.T.);
#37162=EDGE_CURVE('',#29135,#29133,#15740,.T.);
#37163=EDGE_CURVE('',#29136,#29134,#15741,.T.);
#37164=EDGE_CURVE('',#29135,#29136,#15742,.T.);
#37165=EDGE_CURVE('',#29137,#29135,#15743,.T.);
#37166=EDGE_CURVE('',#29138,#29136,#15744,.T.);
#37167=EDGE_CURVE('',#29137,#29138,#15745,.T.);
#37168=EDGE_CURVE('',#29139,#29137,#15746,.T.);
#37169=EDGE_CURVE('',#29140,#29138,#15747,.T.);
#37170=EDGE_CURVE('',#29139,#29140,#15748,.T.);
#37171=EDGE_CURVE('',#29141,#29139,#15749,.T.);
#37172=EDGE_CURVE('',#29142,#29140,#15750,.T.);
#37173=EDGE_CURVE('',#29141,#29142,#15751,.T.);
#37174=EDGE_CURVE('',#29143,#29141,#15752,.T.);
#37175=EDGE_CURVE('',#29144,#29142,#15753,.T.);
#37176=EDGE_CURVE('',#29143,#29144,#15754,.T.);
#37177=EDGE_CURVE('',#29145,#29143,#15755,.T.);
#37178=EDGE_CURVE('',#29146,#29144,#15756,.T.);
#37179=EDGE_CURVE('',#29145,#29146,#15757,.T.);
#37180=EDGE_CURVE('',#29147,#29145,#15758,.T.);
#37181=EDGE_CURVE('',#29148,#29146,#15759,.T.);
#37182=EDGE_CURVE('',#29147,#29148,#15760,.T.);
#37183=EDGE_CURVE('',#29149,#29147,#15761,.T.);
#37184=EDGE_CURVE('',#29150,#29148,#15762,.T.);
#37185=EDGE_CURVE('',#29149,#29150,#15763,.T.);
#37186=EDGE_CURVE('',#29151,#29149,#15764,.T.);
#37187=EDGE_CURVE('',#29152,#29150,#15765,.T.);
#37188=EDGE_CURVE('',#29151,#29152,#15766,.T.);
#37189=EDGE_CURVE('',#29153,#29151,#15767,.T.);
#37190=EDGE_CURVE('',#29154,#29152,#15768,.T.);
#37191=EDGE_CURVE('',#29153,#29154,#15769,.T.);
#37192=EDGE_CURVE('',#29155,#29153,#15770,.T.);
#37193=EDGE_CURVE('',#29156,#29154,#15771,.T.);
#37194=EDGE_CURVE('',#29155,#29156,#15772,.T.);
#37195=EDGE_CURVE('',#29157,#29155,#15773,.T.);
#37196=EDGE_CURVE('',#29158,#29156,#15774,.T.);
#37197=EDGE_CURVE('',#29157,#29158,#15775,.T.);
#37198=EDGE_CURVE('',#29159,#29157,#15776,.T.);
#37199=EDGE_CURVE('',#29160,#29158,#15777,.T.);
#37200=EDGE_CURVE('',#29159,#29160,#15778,.T.);
#37201=EDGE_CURVE('',#29161,#29159,#15779,.T.);
#37202=EDGE_CURVE('',#29162,#29160,#15780,.T.);
#37203=EDGE_CURVE('',#29161,#29162,#15781,.T.);
#37204=EDGE_CURVE('',#29163,#29161,#15782,.T.);
#37205=EDGE_CURVE('',#29164,#29162,#15783,.T.);
#37206=EDGE_CURVE('',#29163,#29164,#15784,.T.);
#37207=EDGE_CURVE('',#29165,#29163,#15785,.T.);
#37208=EDGE_CURVE('',#29166,#29164,#15786,.T.);
#37209=EDGE_CURVE('',#29165,#29166,#15787,.T.);
#37210=EDGE_CURVE('',#29167,#29165,#15788,.T.);
#37211=EDGE_CURVE('',#29168,#29166,#15789,.T.);
#37212=EDGE_CURVE('',#29167,#29168,#15790,.T.);
#37213=EDGE_CURVE('',#29169,#29167,#15791,.T.);
#37214=EDGE_CURVE('',#29170,#29168,#15792,.T.);
#37215=EDGE_CURVE('',#29169,#29170,#15793,.T.);
#37216=EDGE_CURVE('',#29171,#29169,#15794,.T.);
#37217=EDGE_CURVE('',#29172,#29170,#15795,.T.);
#37218=EDGE_CURVE('',#29171,#29172,#15796,.T.);
#37219=EDGE_CURVE('',#29173,#29171,#15797,.T.);
#37220=EDGE_CURVE('',#29174,#29172,#15798,.T.);
#37221=EDGE_CURVE('',#29173,#29174,#15799,.T.);
#37222=EDGE_CURVE('',#29175,#29173,#15800,.T.);
#37223=EDGE_CURVE('',#29176,#29174,#15801,.T.);
#37224=EDGE_CURVE('',#29175,#29176,#15802,.T.);
#37225=EDGE_CURVE('',#29177,#29175,#15803,.T.);
#37226=EDGE_CURVE('',#29178,#29176,#15804,.T.);
#37227=EDGE_CURVE('',#29177,#29178,#15805,.T.);
#37228=EDGE_CURVE('',#29179,#29177,#15806,.T.);
#37229=EDGE_CURVE('',#29180,#29178,#15807,.T.);
#37230=EDGE_CURVE('',#29179,#29180,#15808,.T.);
#37231=EDGE_CURVE('',#29181,#29179,#15809,.T.);
#37232=EDGE_CURVE('',#29182,#29180,#15810,.T.);
#37233=EDGE_CURVE('',#29181,#29182,#15811,.T.);
#37234=EDGE_CURVE('',#29183,#29181,#15812,.T.);
#37235=EDGE_CURVE('',#29184,#29182,#15813,.T.);
#37236=EDGE_CURVE('',#29183,#29184,#15814,.T.);
#37237=EDGE_CURVE('',#29185,#29183,#15815,.T.);
#37238=EDGE_CURVE('',#29186,#29184,#15816,.T.);
#37239=EDGE_CURVE('',#29185,#29186,#15817,.T.);
#37240=EDGE_CURVE('',#29187,#29185,#15818,.T.);
#37241=EDGE_CURVE('',#29188,#29186,#15819,.T.);
#37242=EDGE_CURVE('',#29187,#29188,#15820,.T.);
#37243=EDGE_CURVE('',#29189,#29187,#15821,.T.);
#37244=EDGE_CURVE('',#29190,#29188,#15822,.T.);
#37245=EDGE_CURVE('',#29189,#29190,#15823,.T.);
#37246=EDGE_CURVE('',#29191,#29189,#15824,.T.);
#37247=EDGE_CURVE('',#29192,#29190,#15825,.T.);
#37248=EDGE_CURVE('',#29191,#29192,#15826,.T.);
#37249=EDGE_CURVE('',#29193,#29191,#15827,.T.);
#37250=EDGE_CURVE('',#29194,#29192,#15828,.T.);
#37251=EDGE_CURVE('',#29193,#29194,#15829,.T.);
#37252=EDGE_CURVE('',#29195,#29193,#15830,.T.);
#37253=EDGE_CURVE('',#29196,#29194,#15831,.T.);
#37254=EDGE_CURVE('',#29195,#29196,#15832,.T.);
#37255=EDGE_CURVE('',#29197,#29195,#15833,.T.);
#37256=EDGE_CURVE('',#29198,#29196,#15834,.T.);
#37257=EDGE_CURVE('',#29197,#29198,#15835,.T.);
#37258=EDGE_CURVE('',#29199,#29197,#15836,.T.);
#37259=EDGE_CURVE('',#29200,#29198,#15837,.T.);
#37260=EDGE_CURVE('',#29199,#29200,#15838,.T.);
#37261=EDGE_CURVE('',#29201,#29199,#15839,.T.);
#37262=EDGE_CURVE('',#29202,#29200,#15840,.T.);
#37263=EDGE_CURVE('',#29201,#29202,#15841,.T.);
#37264=EDGE_CURVE('',#29203,#29201,#15842,.T.);
#37265=EDGE_CURVE('',#29204,#29202,#15843,.T.);
#37266=EDGE_CURVE('',#29203,#29204,#15844,.T.);
#37267=EDGE_CURVE('',#29205,#29203,#15845,.T.);
#37268=EDGE_CURVE('',#29206,#29204,#15846,.T.);
#37269=EDGE_CURVE('',#29205,#29206,#15847,.T.);
#37270=EDGE_CURVE('',#29207,#29205,#15848,.T.);
#37271=EDGE_CURVE('',#29208,#29206,#15849,.T.);
#37272=EDGE_CURVE('',#29207,#29208,#15850,.T.);
#37273=EDGE_CURVE('',#29209,#29207,#15851,.T.);
#37274=EDGE_CURVE('',#29210,#29208,#15852,.T.);
#37275=EDGE_CURVE('',#29209,#29210,#15853,.T.);
#37276=EDGE_CURVE('',#29211,#29209,#15854,.T.);
#37277=EDGE_CURVE('',#29212,#29210,#15855,.T.);
#37278=EDGE_CURVE('',#29211,#29212,#15856,.T.);
#37279=EDGE_CURVE('',#29213,#29211,#15857,.T.);
#37280=EDGE_CURVE('',#29214,#29212,#15858,.T.);
#37281=EDGE_CURVE('',#29213,#29214,#15859,.T.);
#37282=EDGE_CURVE('',#29215,#29213,#15860,.T.);
#37283=EDGE_CURVE('',#29216,#29214,#15861,.T.);
#37284=EDGE_CURVE('',#29215,#29216,#15862,.T.);
#37285=EDGE_CURVE('',#29217,#29215,#15863,.T.);
#37286=EDGE_CURVE('',#29218,#29216,#15864,.T.);
#37287=EDGE_CURVE('',#29217,#29218,#15865,.T.);
#37288=EDGE_CURVE('',#29219,#29217,#15866,.T.);
#37289=EDGE_CURVE('',#29220,#29218,#15867,.T.);
#37290=EDGE_CURVE('',#29219,#29220,#15868,.T.);
#37291=EDGE_CURVE('',#29221,#29219,#15869,.T.);
#37292=EDGE_CURVE('',#29222,#29220,#15870,.T.);
#37293=EDGE_CURVE('',#29221,#29222,#15871,.T.);
#37294=EDGE_CURVE('',#29223,#29221,#15872,.T.);
#37295=EDGE_CURVE('',#29224,#29222,#15873,.T.);
#37296=EDGE_CURVE('',#29223,#29224,#15874,.T.);
#37297=EDGE_CURVE('',#29225,#29223,#15875,.T.);
#37298=EDGE_CURVE('',#29226,#29224,#15876,.T.);
#37299=EDGE_CURVE('',#29225,#29226,#15877,.T.);
#37300=EDGE_CURVE('',#29227,#29225,#15878,.T.);
#37301=EDGE_CURVE('',#29228,#29226,#15879,.T.);
#37302=EDGE_CURVE('',#29227,#29228,#15880,.T.);
#37303=EDGE_CURVE('',#29229,#29227,#15881,.T.);
#37304=EDGE_CURVE('',#29230,#29228,#15882,.T.);
#37305=EDGE_CURVE('',#29229,#29230,#15883,.T.);
#37306=EDGE_CURVE('',#29231,#29229,#15884,.T.);
#37307=EDGE_CURVE('',#29232,#29230,#15885,.T.);
#37308=EDGE_CURVE('',#29231,#29232,#15886,.T.);
#37309=EDGE_CURVE('',#29233,#29231,#15887,.T.);
#37310=EDGE_CURVE('',#29234,#29232,#15888,.T.);
#37311=EDGE_CURVE('',#29233,#29234,#15889,.T.);
#37312=EDGE_CURVE('',#29235,#29233,#15890,.T.);
#37313=EDGE_CURVE('',#29236,#29234,#15891,.T.);
#37314=EDGE_CURVE('',#29235,#29236,#15892,.T.);
#37315=EDGE_CURVE('',#29237,#29235,#15893,.T.);
#37316=EDGE_CURVE('',#29238,#29236,#15894,.T.);
#37317=EDGE_CURVE('',#29237,#29238,#15895,.T.);
#37318=EDGE_CURVE('',#29239,#29237,#15896,.T.);
#37319=EDGE_CURVE('',#29240,#29238,#15897,.T.);
#37320=EDGE_CURVE('',#29239,#29240,#15898,.T.);
#37321=EDGE_CURVE('',#29241,#29239,#15899,.T.);
#37322=EDGE_CURVE('',#29242,#29240,#15900,.T.);
#37323=EDGE_CURVE('',#29241,#29242,#15901,.T.);
#37324=EDGE_CURVE('',#29243,#29241,#15902,.T.);
#37325=EDGE_CURVE('',#29244,#29242,#15903,.T.);
#37326=EDGE_CURVE('',#29243,#29244,#15904,.T.);
#37327=EDGE_CURVE('',#29245,#29243,#15905,.T.);
#37328=EDGE_CURVE('',#29246,#29244,#15906,.T.);
#37329=EDGE_CURVE('',#29245,#29246,#15907,.T.);
#37330=EDGE_CURVE('',#29247,#29245,#15908,.T.);
#37331=EDGE_CURVE('',#29248,#29246,#15909,.T.);
#37332=EDGE_CURVE('',#29247,#29248,#15910,.T.);
#37333=EDGE_CURVE('',#29249,#29247,#15911,.T.);
#37334=EDGE_CURVE('',#29250,#29248,#15912,.T.);
#37335=EDGE_CURVE('',#29249,#29250,#15913,.T.);
#37336=EDGE_CURVE('',#29251,#29249,#15914,.T.);
#37337=EDGE_CURVE('',#29252,#29250,#15915,.T.);
#37338=EDGE_CURVE('',#29251,#29252,#15916,.T.);
#37339=EDGE_CURVE('',#29253,#29251,#15917,.T.);
#37340=EDGE_CURVE('',#29254,#29252,#15918,.T.);
#37341=EDGE_CURVE('',#29253,#29254,#15919,.T.);
#37342=EDGE_CURVE('',#29255,#29253,#15920,.T.);
#37343=EDGE_CURVE('',#29256,#29254,#15921,.T.);
#37344=EDGE_CURVE('',#29255,#29256,#15922,.T.);
#37345=EDGE_CURVE('',#29257,#29255,#15923,.T.);
#37346=EDGE_CURVE('',#29258,#29256,#15924,.T.);
#37347=EDGE_CURVE('',#29257,#29258,#15925,.T.);
#37348=EDGE_CURVE('',#29259,#29257,#15926,.T.);
#37349=EDGE_CURVE('',#29260,#29258,#15927,.T.);
#37350=EDGE_CURVE('',#29259,#29260,#15928,.T.);
#37351=EDGE_CURVE('',#29261,#29259,#15929,.T.);
#37352=EDGE_CURVE('',#29262,#29260,#15930,.T.);
#37353=EDGE_CURVE('',#29261,#29262,#15931,.T.);
#37354=EDGE_CURVE('',#29263,#29261,#15932,.T.);
#37355=EDGE_CURVE('',#29264,#29262,#15933,.T.);
#37356=EDGE_CURVE('',#29263,#29264,#15934,.T.);
#37357=EDGE_CURVE('',#29265,#29263,#15935,.T.);
#37358=EDGE_CURVE('',#29266,#29264,#15936,.T.);
#37359=EDGE_CURVE('',#29265,#29266,#15937,.T.);
#37360=EDGE_CURVE('',#29267,#29265,#15938,.T.);
#37361=EDGE_CURVE('',#29268,#29266,#15939,.T.);
#37362=EDGE_CURVE('',#29267,#29268,#15940,.T.);
#37363=EDGE_CURVE('',#29269,#29267,#15941,.T.);
#37364=EDGE_CURVE('',#29270,#29268,#15942,.T.);
#37365=EDGE_CURVE('',#29269,#29270,#15943,.T.);
#37366=EDGE_CURVE('',#29271,#29269,#15944,.T.);
#37367=EDGE_CURVE('',#29272,#29270,#15945,.T.);
#37368=EDGE_CURVE('',#29271,#29272,#15946,.T.);
#37369=EDGE_CURVE('',#29273,#29271,#15947,.T.);
#37370=EDGE_CURVE('',#29274,#29272,#15948,.T.);
#37371=EDGE_CURVE('',#29273,#29274,#15949,.T.);
#37372=EDGE_CURVE('',#29275,#29273,#15950,.T.);
#37373=EDGE_CURVE('',#29276,#29274,#15951,.T.);
#37374=EDGE_CURVE('',#29275,#29276,#15952,.T.);
#37375=EDGE_CURVE('',#29277,#29275,#15953,.T.);
#37376=EDGE_CURVE('',#29278,#29276,#15954,.T.);
#37377=EDGE_CURVE('',#29277,#29278,#15955,.T.);
#37378=EDGE_CURVE('',#29279,#29277,#15956,.T.);
#37379=EDGE_CURVE('',#29280,#29278,#15957,.T.);
#37380=EDGE_CURVE('',#29279,#29280,#15958,.T.);
#37381=EDGE_CURVE('',#29281,#29279,#15959,.T.);
#37382=EDGE_CURVE('',#29282,#29280,#15960,.T.);
#37383=EDGE_CURVE('',#29281,#29282,#15961,.T.);
#37384=EDGE_CURVE('',#29283,#29281,#15962,.T.);
#37385=EDGE_CURVE('',#29284,#29282,#15963,.T.);
#37386=EDGE_CURVE('',#29283,#29284,#15964,.T.);
#37387=EDGE_CURVE('',#29285,#29283,#15965,.T.);
#37388=EDGE_CURVE('',#29286,#29284,#15966,.T.);
#37389=EDGE_CURVE('',#29285,#29286,#15967,.T.);
#37390=EDGE_CURVE('',#29287,#29285,#15968,.T.);
#37391=EDGE_CURVE('',#29288,#29286,#15969,.T.);
#37392=EDGE_CURVE('',#29287,#29288,#15970,.T.);
#37393=EDGE_CURVE('',#29289,#29287,#15971,.T.);
#37394=EDGE_CURVE('',#29290,#29288,#15972,.T.);
#37395=EDGE_CURVE('',#29289,#29290,#15973,.T.);
#37396=EDGE_CURVE('',#29291,#29289,#15974,.T.);
#37397=EDGE_CURVE('',#29292,#29290,#15975,.T.);
#37398=EDGE_CURVE('',#29291,#29292,#15976,.T.);
#37399=EDGE_CURVE('',#29293,#29291,#15977,.T.);
#37400=EDGE_CURVE('',#29294,#29292,#15978,.T.);
#37401=EDGE_CURVE('',#29293,#29294,#15979,.T.);
#37402=EDGE_CURVE('',#29295,#29293,#15980,.T.);
#37403=EDGE_CURVE('',#29296,#29294,#15981,.T.);
#37404=EDGE_CURVE('',#29295,#29296,#15982,.T.);
#37405=EDGE_CURVE('',#29297,#29295,#15983,.T.);
#37406=EDGE_CURVE('',#29298,#29296,#15984,.T.);
#37407=EDGE_CURVE('',#29297,#29298,#15985,.T.);
#37408=EDGE_CURVE('',#29299,#29297,#15986,.T.);
#37409=EDGE_CURVE('',#29300,#29298,#15987,.T.);
#37410=EDGE_CURVE('',#29299,#29300,#15988,.T.);
#37411=EDGE_CURVE('',#29301,#29299,#15989,.T.);
#37412=EDGE_CURVE('',#29302,#29300,#15990,.T.);
#37413=EDGE_CURVE('',#29301,#29302,#15991,.T.);
#37414=EDGE_CURVE('',#29303,#29301,#15992,.T.);
#37415=EDGE_CURVE('',#29304,#29302,#15993,.T.);
#37416=EDGE_CURVE('',#29303,#29304,#15994,.T.);
#37417=EDGE_CURVE('',#29305,#29303,#15995,.T.);
#37418=EDGE_CURVE('',#29306,#29304,#15996,.T.);
#37419=EDGE_CURVE('',#29305,#29306,#15997,.T.);
#37420=EDGE_CURVE('',#29307,#29305,#15998,.T.);
#37421=EDGE_CURVE('',#29308,#29306,#15999,.T.);
#37422=EDGE_CURVE('',#29307,#29308,#16000,.T.);
#37423=EDGE_CURVE('',#29309,#29307,#16001,.T.);
#37424=EDGE_CURVE('',#29310,#29308,#16002,.T.);
#37425=EDGE_CURVE('',#29309,#29310,#16003,.T.);
#37426=EDGE_CURVE('',#29311,#29309,#16004,.T.);
#37427=EDGE_CURVE('',#29312,#29310,#16005,.T.);
#37428=EDGE_CURVE('',#29311,#29312,#16006,.T.);
#37429=EDGE_CURVE('',#29313,#29311,#16007,.T.);
#37430=EDGE_CURVE('',#29314,#29312,#16008,.T.);
#37431=EDGE_CURVE('',#29313,#29314,#16009,.T.);
#37432=EDGE_CURVE('',#29315,#29313,#16010,.T.);
#37433=EDGE_CURVE('',#29316,#29314,#16011,.T.);
#37434=EDGE_CURVE('',#29315,#29316,#16012,.T.);
#37435=EDGE_CURVE('',#29317,#29315,#16013,.T.);
#37436=EDGE_CURVE('',#29318,#29316,#16014,.T.);
#37437=EDGE_CURVE('',#29317,#29318,#16015,.T.);
#37438=EDGE_CURVE('',#29319,#29317,#16016,.T.);
#37439=EDGE_CURVE('',#29320,#29318,#16017,.T.);
#37440=EDGE_CURVE('',#29319,#29320,#16018,.T.);
#37441=EDGE_CURVE('',#29321,#29319,#16019,.T.);
#37442=EDGE_CURVE('',#29322,#29320,#16020,.T.);
#37443=EDGE_CURVE('',#29321,#29322,#16021,.T.);
#37444=EDGE_CURVE('',#29323,#29321,#16022,.T.);
#37445=EDGE_CURVE('',#29324,#29322,#16023,.T.);
#37446=EDGE_CURVE('',#29323,#29324,#16024,.T.);
#37447=EDGE_CURVE('',#29325,#29323,#16025,.T.);
#37448=EDGE_CURVE('',#29326,#29324,#16026,.T.);
#37449=EDGE_CURVE('',#29325,#29326,#16027,.T.);
#37450=EDGE_CURVE('',#29327,#29325,#16028,.T.);
#37451=EDGE_CURVE('',#29328,#29326,#16029,.T.);
#37452=EDGE_CURVE('',#29327,#29328,#16030,.T.);
#37453=EDGE_CURVE('',#29329,#29327,#16031,.T.);
#37454=EDGE_CURVE('',#29330,#29328,#16032,.T.);
#37455=EDGE_CURVE('',#29329,#29330,#16033,.T.);
#37456=EDGE_CURVE('',#29331,#29329,#16034,.T.);
#37457=EDGE_CURVE('',#29332,#29330,#16035,.T.);
#37458=EDGE_CURVE('',#29331,#29332,#16036,.T.);
#37459=EDGE_CURVE('',#29333,#29331,#16037,.T.);
#37460=EDGE_CURVE('',#29334,#29332,#16038,.T.);
#37461=EDGE_CURVE('',#29333,#29334,#16039,.T.);
#37462=EDGE_CURVE('',#29335,#29333,#16040,.T.);
#37463=EDGE_CURVE('',#29336,#29334,#16041,.T.);
#37464=EDGE_CURVE('',#29335,#29336,#16042,.T.);
#37465=EDGE_CURVE('',#29337,#29335,#16043,.T.);
#37466=EDGE_CURVE('',#29338,#29336,#16044,.T.);
#37467=EDGE_CURVE('',#29337,#29338,#16045,.T.);
#37468=EDGE_CURVE('',#29339,#29337,#16046,.T.);
#37469=EDGE_CURVE('',#29340,#29338,#16047,.T.);
#37470=EDGE_CURVE('',#29339,#29340,#16048,.T.);
#37471=EDGE_CURVE('',#29341,#29339,#16049,.T.);
#37472=EDGE_CURVE('',#29342,#29340,#16050,.T.);
#37473=EDGE_CURVE('',#29341,#29342,#16051,.T.);
#37474=EDGE_CURVE('',#29343,#29341,#16052,.T.);
#37475=EDGE_CURVE('',#29344,#29342,#16053,.T.);
#37476=EDGE_CURVE('',#29343,#29344,#16054,.T.);
#37477=EDGE_CURVE('',#29345,#29343,#16055,.T.);
#37478=EDGE_CURVE('',#29346,#29344,#16056,.T.);
#37479=EDGE_CURVE('',#29345,#29346,#16057,.T.);
#37480=EDGE_CURVE('',#29347,#29345,#16058,.T.);
#37481=EDGE_CURVE('',#29348,#29346,#16059,.T.);
#37482=EDGE_CURVE('',#29347,#29348,#16060,.T.);
#37483=EDGE_CURVE('',#29349,#29347,#16061,.T.);
#37484=EDGE_CURVE('',#29350,#29348,#16062,.T.);
#37485=EDGE_CURVE('',#29349,#29350,#16063,.T.);
#37486=EDGE_CURVE('',#29351,#29349,#16064,.T.);
#37487=EDGE_CURVE('',#29352,#29350,#16065,.T.);
#37488=EDGE_CURVE('',#29351,#29352,#16066,.T.);
#37489=EDGE_CURVE('',#29353,#29351,#16067,.T.);
#37490=EDGE_CURVE('',#29354,#29352,#16068,.T.);
#37491=EDGE_CURVE('',#29353,#29354,#16069,.T.);
#37492=EDGE_CURVE('',#29355,#29353,#16070,.T.);
#37493=EDGE_CURVE('',#29356,#29354,#16071,.T.);
#37494=EDGE_CURVE('',#29355,#29356,#16072,.T.);
#37495=EDGE_CURVE('',#29357,#29355,#16073,.T.);
#37496=EDGE_CURVE('',#29358,#29356,#16074,.T.);
#37497=EDGE_CURVE('',#29357,#29358,#16075,.T.);
#37498=EDGE_CURVE('',#29359,#29357,#16076,.T.);
#37499=EDGE_CURVE('',#29360,#29358,#16077,.T.);
#37500=EDGE_CURVE('',#29359,#29360,#16078,.T.);
#37501=EDGE_CURVE('',#29361,#29359,#16079,.T.);
#37502=EDGE_CURVE('',#29362,#29360,#16080,.T.);
#37503=EDGE_CURVE('',#29361,#29362,#16081,.T.);
#37504=EDGE_CURVE('',#29363,#29361,#16082,.T.);
#37505=EDGE_CURVE('',#29364,#29362,#16083,.T.);
#37506=EDGE_CURVE('',#29363,#29364,#16084,.T.);
#37507=EDGE_CURVE('',#29365,#29363,#16085,.T.);
#37508=EDGE_CURVE('',#29366,#29364,#16086,.T.);
#37509=EDGE_CURVE('',#29365,#29366,#16087,.T.);
#37510=EDGE_CURVE('',#29367,#29365,#16088,.T.);
#37511=EDGE_CURVE('',#29368,#29366,#16089,.T.);
#37512=EDGE_CURVE('',#29367,#29368,#16090,.T.);
#37513=EDGE_CURVE('',#29369,#29367,#16091,.T.);
#37514=EDGE_CURVE('',#29370,#29368,#16092,.T.);
#37515=EDGE_CURVE('',#29369,#29370,#16093,.T.);
#37516=EDGE_CURVE('',#29371,#29369,#16094,.T.);
#37517=EDGE_CURVE('',#29372,#29370,#16095,.T.);
#37518=EDGE_CURVE('',#29371,#29372,#16096,.T.);
#37519=EDGE_CURVE('',#29373,#29371,#16097,.T.);
#37520=EDGE_CURVE('',#29374,#29372,#16098,.T.);
#37521=EDGE_CURVE('',#29373,#29374,#16099,.T.);
#37522=EDGE_CURVE('',#29375,#29373,#16100,.T.);
#37523=EDGE_CURVE('',#29376,#29374,#16101,.T.);
#37524=EDGE_CURVE('',#29375,#29376,#16102,.T.);
#37525=EDGE_CURVE('',#29377,#29375,#16103,.T.);
#37526=EDGE_CURVE('',#29378,#29376,#16104,.T.);
#37527=EDGE_CURVE('',#29377,#29378,#16105,.T.);
#37528=EDGE_CURVE('',#29379,#29377,#16106,.T.);
#37529=EDGE_CURVE('',#29380,#29378,#16107,.T.);
#37530=EDGE_CURVE('',#29379,#29380,#16108,.T.);
#37531=EDGE_CURVE('',#29381,#29379,#16109,.T.);
#37532=EDGE_CURVE('',#29382,#29380,#16110,.T.);
#37533=EDGE_CURVE('',#29381,#29382,#16111,.T.);
#37534=EDGE_CURVE('',#29383,#29381,#16112,.T.);
#37535=EDGE_CURVE('',#29384,#29382,#16113,.T.);
#37536=EDGE_CURVE('',#29383,#29384,#16114,.T.);
#37537=EDGE_CURVE('',#29385,#29383,#16115,.T.);
#37538=EDGE_CURVE('',#29386,#29384,#16116,.T.);
#37539=EDGE_CURVE('',#29385,#29386,#16117,.T.);
#37540=EDGE_CURVE('',#29387,#29385,#16118,.T.);
#37541=EDGE_CURVE('',#29388,#29386,#16119,.T.);
#37542=EDGE_CURVE('',#29387,#29388,#16120,.T.);
#37543=EDGE_CURVE('',#29389,#29387,#16121,.T.);
#37544=EDGE_CURVE('',#29390,#29388,#16122,.T.);
#37545=EDGE_CURVE('',#29389,#29390,#16123,.T.);
#37546=EDGE_CURVE('',#29391,#29389,#16124,.T.);
#37547=EDGE_CURVE('',#29392,#29390,#16125,.T.);
#37548=EDGE_CURVE('',#29391,#29392,#16126,.T.);
#37549=EDGE_CURVE('',#29393,#29391,#16127,.T.);
#37550=EDGE_CURVE('',#29394,#29392,#16128,.T.);
#37551=EDGE_CURVE('',#29393,#29394,#16129,.T.);
#37552=EDGE_CURVE('',#29395,#29393,#16130,.T.);
#37553=EDGE_CURVE('',#29396,#29394,#16131,.T.);
#37554=EDGE_CURVE('',#29395,#29396,#16132,.T.);
#37555=EDGE_CURVE('',#29397,#29395,#16133,.T.);
#37556=EDGE_CURVE('',#29398,#29396,#16134,.T.);
#37557=EDGE_CURVE('',#29397,#29398,#16135,.T.);
#37558=EDGE_CURVE('',#29399,#29397,#16136,.T.);
#37559=EDGE_CURVE('',#29400,#29398,#16137,.T.);
#37560=EDGE_CURVE('',#29399,#29400,#16138,.T.);
#37561=EDGE_CURVE('',#29401,#29399,#16139,.T.);
#37562=EDGE_CURVE('',#29402,#29400,#16140,.T.);
#37563=EDGE_CURVE('',#29401,#29402,#16141,.T.);
#37564=EDGE_CURVE('',#29403,#29401,#16142,.T.);
#37565=EDGE_CURVE('',#29404,#29402,#16143,.T.);
#37566=EDGE_CURVE('',#29403,#29404,#16144,.T.);
#37567=EDGE_CURVE('',#29405,#29403,#16145,.T.);
#37568=EDGE_CURVE('',#29406,#29404,#16146,.T.);
#37569=EDGE_CURVE('',#29405,#29406,#16147,.T.);
#37570=EDGE_CURVE('',#29407,#29405,#16148,.T.);
#37571=EDGE_CURVE('',#29408,#29406,#16149,.T.);
#37572=EDGE_CURVE('',#29407,#29408,#16150,.T.);
#37573=EDGE_CURVE('',#29409,#29407,#16151,.T.);
#37574=EDGE_CURVE('',#29410,#29408,#16152,.T.);
#37575=EDGE_CURVE('',#29409,#29410,#16153,.T.);
#37576=EDGE_CURVE('',#29411,#29409,#16154,.T.);
#37577=EDGE_CURVE('',#29412,#29410,#16155,.T.);
#37578=EDGE_CURVE('',#29411,#29412,#16156,.T.);
#37579=EDGE_CURVE('',#28395,#29411,#16157,.T.);
#37580=EDGE_CURVE('',#28396,#29412,#16158,.T.);
#37581=EDGE_CURVE('',#28403,#28411,#16159,.T.);
#37582=EDGE_CURVE('',#28402,#28416,#16160,.T.);
#37583=EDGE_CURVE('',#29413,#29414,#1254,.T.);
#37584=EDGE_CURVE('',#29414,#29415,#16161,.T.);
#37585=EDGE_CURVE('',#29415,#29416,#1255,.T.);
#37586=EDGE_CURVE('',#29416,#29413,#16162,.T.);
#37587=EDGE_CURVE('',#29414,#29417,#1256,.T.);
#37588=EDGE_CURVE('',#29418,#29417,#16163,.T.);
#37589=EDGE_CURVE('',#29415,#29418,#1257,.T.);
#37590=EDGE_CURVE('',#29417,#29419,#1258,.T.);
#37591=EDGE_CURVE('',#29419,#29420,#16164,.T.);
#37592=EDGE_CURVE('',#29420,#29418,#1259,.T.);
#37593=EDGE_CURVE('',#29421,#29419,#16165,.T.);
#37594=EDGE_CURVE('',#29421,#29422,#16166,.T.);
#37595=EDGE_CURVE('',#29423,#29422,#16167,.T.);
#37596=EDGE_CURVE('',#29424,#29423,#16168,.T.);
#37597=EDGE_CURVE('',#29420,#29424,#16169,.T.);
#37598=EDGE_CURVE('',#29425,#29424,#1260,.T.);
#37599=EDGE_CURVE('',#29423,#29426,#601,.F.);
#37600=EDGE_CURVE('',#29426,#29425,#16170,.T.);
#37601=EDGE_CURVE('',#29422,#29427,#16171,.T.);
#37602=EDGE_CURVE('',#29428,#29421,#16172,.T.);
#37603=EDGE_CURVE('',#29427,#29428,#16173,.T.);
#37604=EDGE_CURVE('',#29426,#29429,#16174,.T.);
#37605=EDGE_CURVE('',#29429,#29430,#16175,.T.);
#37606=EDGE_CURVE('',#29430,#29431,#16176,.T.);
#37607=EDGE_CURVE('',#29432,#29431,#16177,.T.);
#37608=EDGE_CURVE('',#29433,#29432,#16178,.T.);
#37609=EDGE_CURVE('',#29425,#29433,#16179,.T.);
#37610=EDGE_CURVE('',#29434,#29433,#1261,.T.);
#37611=EDGE_CURVE('',#29432,#29435,#1262,.T.);
#37612=EDGE_CURVE('',#29435,#29434,#16180,.T.);
#37613=EDGE_CURVE('',#29431,#29436,#16181,.T.);
#37614=EDGE_CURVE('',#29436,#29437,#16182,.T.);
#37615=EDGE_CURVE('',#29428,#29437,#1263,.T.);
#37616=EDGE_CURVE('',#29413,#29435,#16183,.T.);
#37617=EDGE_CURVE('',#29438,#29438,#1264,.T.);
#37618=EDGE_CURVE('',#29439,#29427,#602,.T.);
#37619=EDGE_CURVE('',#29437,#29439,#16184,.T.);
#37620=EDGE_CURVE('',#29430,#29440,#16185,.T.);
#37621=EDGE_CURVE('',#29441,#29440,#16186,.T.);
#37622=EDGE_CURVE('',#29442,#29441,#16187,.T.);
#37623=EDGE_CURVE('',#29436,#29442,#16188,.T.);
#37624=EDGE_CURVE('',#29429,#29443,#16189,.T.);
#37625=EDGE_CURVE('',#29440,#29443,#16190,.T.);
#37626=EDGE_CURVE('',#29444,#29439,#16191,.T.);
#37627=EDGE_CURVE('',#29444,#29445,#16192,.T.);
#37628=EDGE_CURVE('',#29443,#29445,#16193,.T.);
#37629=EDGE_CURVE('',#29442,#29444,#16194,.T.);
#37630=EDGE_CURVE('',#29445,#29441,#16195,.T.);
#37631=EDGE_CURVE('',#29438,#29446,#16196,.T.);
#37632=EDGE_CURVE('',#29446,#29446,#1265,.T.);
#37633=EDGE_CURVE('',#29434,#29416,#16197,.T.);
#37634=EDGE_CURVE('',#29447,#29448,#16198,.T.);
#37635=EDGE_CURVE('',#29449,#29447,#16199,.T.);
#37636=EDGE_CURVE('',#29449,#29450,#16200,.T.);
#37637=EDGE_CURVE('',#29450,#29448,#16201,.T.);
#37638=EDGE_CURVE('',#29448,#29451,#16202,.T.);
#37639=EDGE_CURVE('',#29452,#29450,#16203,.T.);
#37640=EDGE_CURVE('',#29451,#29452,#16204,.T.);
#37641=EDGE_CURVE('',#29453,#29449,#16205,.T.);
#37642=EDGE_CURVE('',#29453,#29452,#16206,.T.);
#37643=EDGE_CURVE('',#29451,#29454,#16207,.T.);
#37644=EDGE_CURVE('',#29454,#29453,#16208,.T.);
#37645=EDGE_CURVE('',#29455,#29456,#16209,.T.);
#37646=EDGE_CURVE('',#29457,#29455,#16210,.T.);
#37647=EDGE_CURVE('',#29457,#29458,#16211,.T.);
#37648=EDGE_CURVE('',#29458,#29456,#16212,.T.);
#37649=EDGE_CURVE('',#29456,#29459,#16213,.T.);
#37650=EDGE_CURVE('',#29460,#29458,#16214,.T.);
#37651=EDGE_CURVE('',#29459,#29460,#16215,.T.);
#37652=EDGE_CURVE('',#29461,#29457,#16216,.T.);
#37653=EDGE_CURVE('',#29461,#29460,#16217,.T.);
#37654=EDGE_CURVE('',#29459,#29462,#16218,.T.);
#37655=EDGE_CURVE('',#29462,#29461,#16219,.T.);
#37656=EDGE_CURVE('',#29463,#29464,#16220,.T.);
#37657=EDGE_CURVE('',#29465,#29463,#16221,.T.);
#37658=EDGE_CURVE('',#29465,#29466,#16222,.T.);
#37659=EDGE_CURVE('',#29466,#29464,#16223,.T.);
#37660=EDGE_CURVE('',#29464,#29467,#16224,.T.);
#37661=EDGE_CURVE('',#29468,#29466,#16225,.T.);
#37662=EDGE_CURVE('',#29467,#29468,#16226,.T.);
#37663=EDGE_CURVE('',#29469,#29465,#16227,.T.);
#37664=EDGE_CURVE('',#29469,#29468,#16228,.T.);
#37665=EDGE_CURVE('',#29467,#29470,#16229,.T.);
#37666=EDGE_CURVE('',#29470,#29469,#16230,.T.);
#37667=EDGE_CURVE('',#29471,#29472,#16231,.T.);
#37668=EDGE_CURVE('',#29473,#29471,#16232,.T.);
#37669=EDGE_CURVE('',#29473,#29474,#16233,.T.);
#37670=EDGE_CURVE('',#29474,#29472,#16234,.T.);
#37671=EDGE_CURVE('',#29472,#29475,#16235,.T.);
#37672=EDGE_CURVE('',#29476,#29474,#16236,.T.);
#37673=EDGE_CURVE('',#29475,#29476,#16237,.T.);
#37674=EDGE_CURVE('',#29477,#29473,#16238,.T.);
#37675=EDGE_CURVE('',#29477,#29476,#16239,.T.);
#37676=EDGE_CURVE('',#29475,#29478,#16240,.T.);
#37677=EDGE_CURVE('',#29478,#29477,#16241,.T.);
#37678=EDGE_CURVE('',#29479,#29480,#16242,.T.);
#37679=EDGE_CURVE('',#29481,#29479,#16243,.T.);
#37680=EDGE_CURVE('',#29481,#29482,#16244,.T.);
#37681=EDGE_CURVE('',#29482,#29480,#16245,.T.);
#37682=EDGE_CURVE('',#29480,#29483,#16246,.T.);
#37683=EDGE_CURVE('',#29484,#29482,#16247,.T.);
#37684=EDGE_CURVE('',#29483,#29484,#16248,.T.);
#37685=EDGE_CURVE('',#29485,#29481,#16249,.T.);
#37686=EDGE_CURVE('',#29485,#29484,#16250,.T.);
#37687=EDGE_CURVE('',#29483,#29486,#16251,.T.);
#37688=EDGE_CURVE('',#29486,#29485,#16252,.T.);
#37689=EDGE_CURVE('',#29487,#29488,#16253,.T.);
#37690=EDGE_CURVE('',#29489,#29487,#16254,.T.);
#37691=EDGE_CURVE('',#29489,#29490,#16255,.T.);
#37692=EDGE_CURVE('',#29490,#29488,#16256,.T.);
#37693=EDGE_CURVE('',#29488,#29491,#16257,.T.);
#37694=EDGE_CURVE('',#29492,#29490,#16258,.T.);
#37695=EDGE_CURVE('',#29491,#29492,#16259,.T.);
#37696=EDGE_CURVE('',#29493,#29489,#16260,.T.);
#37697=EDGE_CURVE('',#29493,#29492,#16261,.T.);
#37698=EDGE_CURVE('',#29491,#29494,#16262,.T.);
#37699=EDGE_CURVE('',#29494,#29493,#16263,.T.);
#37700=EDGE_CURVE('',#29495,#29496,#16264,.T.);
#37701=EDGE_CURVE('',#29497,#29495,#16265,.T.);
#37702=EDGE_CURVE('',#29497,#29498,#16266,.T.);
#37703=EDGE_CURVE('',#29498,#29496,#16267,.T.);
#37704=EDGE_CURVE('',#29496,#29499,#16268,.T.);
#37705=EDGE_CURVE('',#29500,#29498,#16269,.T.);
#37706=EDGE_CURVE('',#29499,#29500,#16270,.T.);
#37707=EDGE_CURVE('',#29501,#29497,#16271,.T.);
#37708=EDGE_CURVE('',#29501,#29500,#16272,.T.);
#37709=EDGE_CURVE('',#29499,#29502,#16273,.T.);
#37710=EDGE_CURVE('',#29502,#29501,#16274,.T.);
#37711=EDGE_CURVE('',#29503,#29504,#16275,.T.);
#37712=EDGE_CURVE('',#29505,#29503,#16276,.T.);
#37713=EDGE_CURVE('',#29505,#29506,#16277,.T.);
#37714=EDGE_CURVE('',#29506,#29504,#16278,.T.);
#37715=EDGE_CURVE('',#29504,#29507,#16279,.T.);
#37716=EDGE_CURVE('',#29508,#29506,#16280,.T.);
#37717=EDGE_CURVE('',#29507,#29508,#16281,.T.);
#37718=EDGE_CURVE('',#29509,#29505,#16282,.T.);
#37719=EDGE_CURVE('',#29509,#29508,#16283,.T.);
#37720=EDGE_CURVE('',#29507,#29510,#16284,.T.);
#37721=EDGE_CURVE('',#29510,#29509,#16285,.T.);
#37722=EDGE_CURVE('',#29511,#29512,#371,.T.);
#37723=EDGE_CURVE('',#29511,#29513,#16286,.T.);
#37724=EDGE_CURVE('',#29514,#29513,#16287,.T.);
#37725=EDGE_CURVE('',#29512,#29514,#16288,.T.);
#37726=EDGE_CURVE('',#29515,#29516,#372,.T.);
#37727=EDGE_CURVE('',#29517,#29515,#16289,.T.);
#37728=EDGE_CURVE('',#29518,#29517,#16290,.T.);
#37729=EDGE_CURVE('',#29518,#29516,#16291,.T.);
#37730=EDGE_CURVE('',#29516,#29511,#1266,.T.);
#37731=EDGE_CURVE('',#29513,#29518,#16292,.T.);
#37732=EDGE_CURVE('',#29519,#29520,#16293,.T.);
#37733=EDGE_CURVE('',#29521,#29519,#16294,.T.);
#37734=EDGE_CURVE('',#29521,#29522,#16295,.T.);
#37735=EDGE_CURVE('',#29522,#29520,#16296,.T.);
#37736=EDGE_CURVE('',#29520,#29523,#16297,.T.);
#37737=EDGE_CURVE('',#29524,#29522,#16298,.T.);
#37738=EDGE_CURVE('',#29523,#29524,#16299,.T.);
#37739=EDGE_CURVE('',#29525,#29521,#16300,.T.);
#37740=EDGE_CURVE('',#29525,#29524,#16301,.T.);
#37741=EDGE_CURVE('',#29523,#29526,#16302,.T.);
#37742=EDGE_CURVE('',#29526,#29525,#16303,.T.);
#37743=EDGE_CURVE('',#29527,#29528,#16304,.T.);
#37744=EDGE_CURVE('',#29529,#29527,#16305,.T.);
#37745=EDGE_CURVE('',#29529,#29530,#16306,.T.);
#37746=EDGE_CURVE('',#29530,#29528,#16307,.T.);
#37747=EDGE_CURVE('',#29528,#29531,#16308,.T.);
#37748=EDGE_CURVE('',#29532,#29530,#16309,.T.);
#37749=EDGE_CURVE('',#29531,#29532,#16310,.T.);
#37750=EDGE_CURVE('',#29533,#29529,#16311,.T.);
#37751=EDGE_CURVE('',#29533,#29532,#16312,.T.);
#37752=EDGE_CURVE('',#29531,#29534,#16313,.T.);
#37753=EDGE_CURVE('',#29534,#29533,#16314,.T.);
#37754=EDGE_CURVE('',#29535,#29536,#16315,.T.);
#37755=EDGE_CURVE('',#29537,#29535,#16316,.T.);
#37756=EDGE_CURVE('',#29537,#29538,#16317,.T.);
#37757=EDGE_CURVE('',#29538,#29536,#16318,.T.);
#37758=EDGE_CURVE('',#29536,#29539,#16319,.T.);
#37759=EDGE_CURVE('',#29540,#29538,#16320,.T.);
#37760=EDGE_CURVE('',#29539,#29540,#16321,.T.);
#37761=EDGE_CURVE('',#29541,#29537,#16322,.T.);
#37762=EDGE_CURVE('',#29541,#29540,#16323,.T.);
#37763=EDGE_CURVE('',#29539,#29542,#16324,.T.);
#37764=EDGE_CURVE('',#29542,#29541,#16325,.T.);
#37765=EDGE_CURVE('',#29543,#29544,#16326,.T.);
#37766=EDGE_CURVE('',#29545,#29543,#16327,.T.);
#37767=EDGE_CURVE('',#29545,#29546,#16328,.T.);
#37768=EDGE_CURVE('',#29546,#29544,#16329,.T.);
#37769=EDGE_CURVE('',#29544,#29547,#16330,.T.);
#37770=EDGE_CURVE('',#29548,#29546,#16331,.T.);
#37771=EDGE_CURVE('',#29547,#29548,#16332,.T.);
#37772=EDGE_CURVE('',#29549,#29545,#16333,.T.);
#37773=EDGE_CURVE('',#29549,#29548,#16334,.T.);
#37774=EDGE_CURVE('',#29547,#29550,#16335,.T.);
#37775=EDGE_CURVE('',#29550,#29549,#16336,.T.);
#37776=EDGE_CURVE('',#29551,#29552,#16337,.T.);
#37777=EDGE_CURVE('',#29553,#29551,#16338,.T.);
#37778=EDGE_CURVE('',#29553,#29554,#16339,.T.);
#37779=EDGE_CURVE('',#29554,#29552,#16340,.T.);
#37780=EDGE_CURVE('',#29552,#29555,#16341,.T.);
#37781=EDGE_CURVE('',#29556,#29554,#16342,.T.);
#37782=EDGE_CURVE('',#29555,#29556,#16343,.T.);
#37783=EDGE_CURVE('',#29557,#29553,#16344,.T.);
#37784=EDGE_CURVE('',#29557,#29556,#16345,.T.);
#37785=EDGE_CURVE('',#29555,#29558,#16346,.T.);
#37786=EDGE_CURVE('',#29558,#29557,#16347,.T.);
#37787=EDGE_CURVE('',#29559,#29560,#16348,.T.);
#37788=EDGE_CURVE('',#29561,#29559,#16349,.T.);
#37789=EDGE_CURVE('',#29561,#29562,#16350,.T.);
#37790=EDGE_CURVE('',#29562,#29560,#16351,.T.);
#37791=EDGE_CURVE('',#29560,#29563,#16352,.T.);
#37792=EDGE_CURVE('',#29564,#29562,#16353,.T.);
#37793=EDGE_CURVE('',#29563,#29564,#16354,.T.);
#37794=EDGE_CURVE('',#29565,#29561,#16355,.T.);
#37795=EDGE_CURVE('',#29565,#29564,#16356,.T.);
#37796=EDGE_CURVE('',#29563,#29566,#16357,.T.);
#37797=EDGE_CURVE('',#29566,#29565,#16358,.T.);
#37798=EDGE_CURVE('',#29567,#29568,#16359,.T.);
#37799=EDGE_CURVE('',#29569,#29567,#16360,.T.);
#37800=EDGE_CURVE('',#29569,#29570,#16361,.T.);
#37801=EDGE_CURVE('',#29570,#29568,#16362,.T.);
#37802=EDGE_CURVE('',#29568,#29571,#16363,.T.);
#37803=EDGE_CURVE('',#29572,#29570,#16364,.T.);
#37804=EDGE_CURVE('',#29571,#29572,#16365,.T.);
#37805=EDGE_CURVE('',#29573,#29569,#16366,.T.);
#37806=EDGE_CURVE('',#29573,#29572,#16367,.T.);
#37807=EDGE_CURVE('',#29571,#29574,#16368,.T.);
#37808=EDGE_CURVE('',#29574,#29573,#16369,.T.);
#37809=EDGE_CURVE('',#29575,#29576,#373,.T.);
#37810=EDGE_CURVE('',#29575,#29577,#16370,.T.);
#37811=EDGE_CURVE('',#29578,#29577,#16371,.T.);
#37812=EDGE_CURVE('',#29576,#29578,#16372,.T.);
#37813=EDGE_CURVE('',#29579,#29580,#374,.T.);
#37814=EDGE_CURVE('',#29581,#29579,#16373,.T.);
#37815=EDGE_CURVE('',#29582,#29581,#16374,.T.);
#37816=EDGE_CURVE('',#29582,#29580,#16375,.T.);
#37817=EDGE_CURVE('',#29580,#29575,#1267,.T.);
#37818=EDGE_CURVE('',#29577,#29582,#16376,.T.);
#37819=EDGE_CURVE('',#29578,#29583,#16377,.T.);
#37820=EDGE_CURVE('',#29583,#29576,#1268,.T.);
#37821=EDGE_CURVE('',#29515,#29584,#1269,.T.);
#37822=EDGE_CURVE('',#29584,#29517,#16378,.T.);
#37823=EDGE_CURVE('',#29567,#29454,#16379,.T.);
#37824=EDGE_CURVE('',#29455,#29574,#16380,.T.);
#37825=EDGE_CURVE('',#29559,#29462,#16381,.T.);
#37826=EDGE_CURVE('',#29463,#29566,#16382,.T.);
#37827=EDGE_CURVE('',#29551,#29470,#16383,.T.);
#37828=EDGE_CURVE('',#29471,#29558,#16384,.T.);
#37829=EDGE_CURVE('',#29479,#29478,#16385,.T.);
#37830=EDGE_CURVE('',#29543,#29486,#16386,.T.);
#37831=EDGE_CURVE('',#29487,#29550,#16387,.T.);
#37832=EDGE_CURVE('',#29535,#29494,#16388,.T.);
#37833=EDGE_CURVE('',#29495,#29542,#16389,.T.);
#37834=EDGE_CURVE('',#29527,#29502,#16390,.T.);
#37835=EDGE_CURVE('',#29503,#29534,#16391,.T.);
#37836=EDGE_CURVE('',#29519,#29510,#16392,.T.);
#37837=EDGE_CURVE('',#29514,#29526,#16393,.T.);
#37838=EDGE_CURVE('',#29584,#29585,#375,.T.);
#37839=EDGE_CURVE('',#29586,#29585,#16394,.T.);
#37840=EDGE_CURVE('',#29587,#29586,#16395,.T.);
#37841=EDGE_CURVE('',#29587,#29588,#16396,.T.);
#37842=EDGE_CURVE('',#29588,#29589,#16397,.T.);
#37843=EDGE_CURVE('',#29590,#29589,#16398,.T.);
#37844=EDGE_CURVE('',#29590,#29583,#376,.T.);
#37845=EDGE_CURVE('',#29447,#29581,#16399,.T.);
#37846=EDGE_CURVE('',#29591,#29591,#1270,.T.);
#37847=EDGE_CURVE('',#29591,#29592,#16400,.T.);
#37848=EDGE_CURVE('',#29592,#29592,#1271,.T.);
#37849=EDGE_CURVE('',#29592,#29593,#16401,.T.);
#37850=EDGE_CURVE('',#29579,#29593,#1272,.T.);
#37851=EDGE_CURVE('',#29594,#29590,#1273,.T.);
#37852=EDGE_CURVE('',#29595,#29594,#377,.T.);
#37853=EDGE_CURVE('',#29593,#29595,#1274,.T.);
#37854=EDGE_CURVE('',#29595,#29596,#16402,.T.);
#37855=EDGE_CURVE('',#29596,#29512,#1275,.T.);
#37856=EDGE_CURVE('',#29589,#29597,#16403,.T.);
#37857=EDGE_CURVE('',#29597,#29598,#1276,.T.);
#37858=EDGE_CURVE('',#29598,#29594,#16404,.T.);
#37859=EDGE_CURVE('',#29599,#29599,#1277,.T.);
#37860=EDGE_CURVE('',#29599,#29600,#16405,.T.);
#37861=EDGE_CURVE('',#29600,#29600,#1278,.T.);
#37862=EDGE_CURVE('',#29600,#29601,#16406,.T.);
#37863=EDGE_CURVE('',#29585,#29601,#1279,.T.);
#37864=EDGE_CURVE('',#29602,#29596,#378,.T.);
#37865=EDGE_CURVE('',#29601,#29602,#1280,.T.);
#37866=EDGE_CURVE('',#29602,#29603,#16407,.T.);
#37867=EDGE_CURVE('',#29603,#29604,#1281,.T.);
#37868=EDGE_CURVE('',#29604,#29586,#16408,.T.);
#37869=EDGE_CURVE('',#29605,#29606,#1282,.T.);
#37870=EDGE_CURVE('',#29606,#29604,#16409,.T.);
#37871=EDGE_CURVE('',#29605,#29603,#16410,.T.);
#37872=EDGE_CURVE('',#29607,#29598,#16411,.T.);
#37873=EDGE_CURVE('',#29607,#29605,#16412,.T.);
#37874=EDGE_CURVE('',#29608,#29607,#1283,.T.);
#37875=EDGE_CURVE('',#29608,#29597,#16413,.T.);
#37876=EDGE_CURVE('',#29588,#29608,#16414,.T.);
#37877=EDGE_CURVE('',#29606,#29587,#16415,.T.);
#37878=EDGE_CURVE('',#29609,#29610,#16416,.T.);
#37879=EDGE_CURVE('',#29609,#29611,#24350,.T.);
#37880=EDGE_CURVE('',#29612,#29611,#1284,.T.);
#37881=EDGE_CURVE('',#29612,#29610,#24351,.T.);
#37882=EDGE_CURVE('',#29613,#29614,#16417,.T.);
#37883=EDGE_CURVE('',#29613,#29609,#24352,.T.);
#37884=EDGE_CURVE('',#29610,#29614,#24353,.T.);
#37885=EDGE_CURVE('',#29615,#29616,#16418,.T.);
#37886=EDGE_CURVE('',#29615,#29613,#24354,.T.);
#37887=EDGE_CURVE('',#29614,#29616,#24355,.T.);
#37888=EDGE_CURVE('',#29617,#29618,#16419,.T.);
#37889=EDGE_CURVE('',#29617,#29615,#24356,.T.);
#37890=EDGE_CURVE('',#29616,#29618,#24357,.T.);
#37891=EDGE_CURVE('',#29619,#29620,#16420,.T.);
#37892=EDGE_CURVE('',#29619,#29617,#24358,.T.);
#37893=EDGE_CURVE('',#29618,#29620,#24359,.T.);
#37894=EDGE_CURVE('',#29621,#29622,#16421,.T.);
#37895=EDGE_CURVE('',#29621,#29619,#24360,.T.);
#37896=EDGE_CURVE('',#29620,#29622,#24361,.T.);
#37897=EDGE_CURVE('',#29623,#29624,#16422,.T.);
#37898=EDGE_CURVE('',#29623,#29621,#24362,.T.);
#37899=EDGE_CURVE('',#29622,#29624,#24363,.T.);
#37900=EDGE_CURVE('',#29625,#29626,#16423,.T.);
#37901=EDGE_CURVE('',#29625,#29623,#24364,.T.);
#37902=EDGE_CURVE('',#29624,#29626,#24365,.T.);
#37903=EDGE_CURVE('',#29627,#29628,#16424,.T.);
#37904=EDGE_CURVE('',#29627,#29625,#24366,.T.);
#37905=EDGE_CURVE('',#29626,#29628,#24367,.T.);
#37906=EDGE_CURVE('',#29629,#29630,#16425,.T.);
#37907=EDGE_CURVE('',#29629,#29627,#24368,.T.);
#37908=EDGE_CURVE('',#29628,#29630,#24369,.T.);
#37909=EDGE_CURVE('',#29631,#29632,#16426,.T.);
#37910=EDGE_CURVE('',#29631,#29629,#24370,.T.);
#37911=EDGE_CURVE('',#29630,#29632,#24371,.T.);
#37912=EDGE_CURVE('',#29633,#29634,#16427,.T.);
#37913=EDGE_CURVE('',#29633,#29635,#24372,.T.);
#37914=EDGE_CURVE('',#29636,#29635,#1285,.T.);
#37915=EDGE_CURVE('',#29634,#29636,#24373,.T.);
#37916=EDGE_CURVE('',#29637,#29638,#16428,.T.);
#37917=EDGE_CURVE('',#29637,#29633,#24374,.T.);
#37918=EDGE_CURVE('',#29638,#29634,#24375,.T.);
#37919=EDGE_CURVE('',#29639,#29640,#16429,.T.);
#37920=EDGE_CURVE('',#29639,#29637,#24376,.T.);
#37921=EDGE_CURVE('',#29640,#29638,#24377,.T.);
#37922=EDGE_CURVE('',#29641,#29642,#16430,.T.);
#37923=EDGE_CURVE('',#29641,#29639,#24378,.T.);
#37924=EDGE_CURVE('',#29642,#29640,#24379,.T.);
#37925=EDGE_CURVE('',#29643,#29644,#16431,.T.);
#37926=EDGE_CURVE('',#29643,#29641,#24380,.T.);
#37927=EDGE_CURVE('',#29644,#29642,#24381,.T.);
#37928=EDGE_CURVE('',#29645,#29646,#16432,.T.);
#37929=EDGE_CURVE('',#29645,#29643,#24382,.T.);
#37930=EDGE_CURVE('',#29646,#29644,#24383,.T.);
#37931=EDGE_CURVE('',#29647,#29648,#16433,.T.);
#37932=EDGE_CURVE('',#29647,#29645,#24384,.T.);
#37933=EDGE_CURVE('',#29648,#29646,#24385,.T.);
#37934=EDGE_CURVE('',#29649,#29650,#16434,.T.);
#37935=EDGE_CURVE('',#29649,#29647,#24386,.T.);
#37936=EDGE_CURVE('',#29650,#29648,#24387,.T.);
#37937=EDGE_CURVE('',#29651,#29652,#16435,.T.);
#37938=EDGE_CURVE('',#29651,#29649,#24388,.T.);
#37939=EDGE_CURVE('',#29652,#29650,#24389,.T.);
#37940=EDGE_CURVE('',#29653,#29654,#16436,.T.);
#37941=EDGE_CURVE('',#29653,#29651,#24390,.T.);
#37942=EDGE_CURVE('',#29654,#29652,#24391,.T.);
#37943=EDGE_CURVE('',#29635,#29655,#24392,.T.);
#37944=EDGE_CURVE('',#29656,#29655,#1286,.F.);
#37945=EDGE_CURVE('',#29657,#29656,#1287,.F.);
#37946=EDGE_CURVE('',#29657,#29636,#24393,.T.);
#37947=EDGE_CURVE('',#29632,#29657,#24394,.T.);
#37948=EDGE_CURVE('',#29658,#29612,#24395,.T.);
#37949=EDGE_CURVE('',#29658,#29654,#24396,.T.);
#37950=EDGE_CURVE('',#29611,#29659,#1288,.T.);
#37951=EDGE_CURVE('',#29611,#29660,#24397,.T.);
#37952=EDGE_CURVE('',#29660,#29658,#1289,.T.);
#37953=EDGE_CURVE('',#29659,#29612,#1290,.T.);
#37954=EDGE_CURVE('',#29660,#29653,#24398,.T.);
#37955=EDGE_CURVE('',#29655,#29631,#24399,.T.);
#37956=EDGE_CURVE('',#29661,#29661,#1291,.T.);
#37957=EDGE_CURVE('',#29661,#29659,#1292,.T.);
#37958=EDGE_CURVE('',#29662,#29662,#1293,.T.);
#37959=EDGE_CURVE('',#29655,#29657,#1294,.F.);
#37960=EDGE_CURVE('',#29663,#29664,#16437,.T.);
#37961=EDGE_CURVE('',#29663,#29665,#16438,.T.);
#37962=EDGE_CURVE('',#29666,#29665,#16439,.T.);
#37963=EDGE_CURVE('',#29667,#29666,#379,.T.);
#37964=EDGE_CURVE('',#29668,#29667,#16440,.T.);
#37965=EDGE_CURVE('',#29664,#29668,#380,.T.);
#37966=EDGE_CURVE('',#29669,#29670,#16441,.T.);
#37967=EDGE_CURVE('',#29671,#29669,#381,.T.);
#37968=EDGE_CURVE('',#29672,#29671,#16442,.T.);
#37969=EDGE_CURVE('',#29673,#29672,#382,.T.);
#37970=EDGE_CURVE('',#29674,#29673,#16443,.T.);
#37971=EDGE_CURVE('',#29674,#29670,#16444,.T.);
#37972=EDGE_CURVE('',#29670,#29663,#1295,.T.);
#37973=EDGE_CURVE('',#29675,#29674,#1296,.T.);
#37974=EDGE_CURVE('',#29665,#29675,#1297,.T.);
#37975=EDGE_CURVE('',#29673,#29669,#1298,.T.);
#37976=EDGE_CURVE('',#29672,#29671,#1299,.T.);
#37977=EDGE_CURVE('',#29668,#29667,#1300,.T.);
#37978=EDGE_CURVE('',#29664,#29666,#1301,.T.);
#37979=EDGE_CURVE('',#29662,#29675,#16445,.T.);
#37980=EDGE_CURVE('',#29676,#29676,#1302,.T.);
#37981=EDGE_CURVE('',#29676,#29656,#16446,.T.);
#37982=EDGE_CURVE('',#29677,#29678,#16447,.T.);
#37983=EDGE_CURVE('',#29677,#29679,#24400,.T.);
#37984=EDGE_CURVE('',#29679,#29680,#1303,.T.);
#37985=EDGE_CURVE('',#29680,#29678,#24401,.T.);
#37986=EDGE_CURVE('',#29681,#29682,#16448,.T.);
#37987=EDGE_CURVE('',#29681,#29677,#24402,.T.);
#37988=EDGE_CURVE('',#29678,#29682,#24403,.T.);
#37989=EDGE_CURVE('',#29683,#29684,#16449,.T.);
#37990=EDGE_CURVE('',#29683,#29681,#24404,.T.);
#37991=EDGE_CURVE('',#29682,#29684,#24405,.T.);
#37992=EDGE_CURVE('',#29685,#29686,#16450,.T.);
#37993=EDGE_CURVE('',#29685,#29683,#24406,.T.);
#37994=EDGE_CURVE('',#29684,#29686,#24407,.T.);
#37995=EDGE_CURVE('',#29687,#29688,#16451,.T.);
#37996=EDGE_CURVE('',#29687,#29685,#24408,.T.);
#37997=EDGE_CURVE('',#29686,#29688,#24409,.T.);
#37998=EDGE_CURVE('',#29689,#29690,#16452,.T.);
#37999=EDGE_CURVE('',#29689,#29691,#24410,.T.);
#38000=EDGE_CURVE('',#29692,#29691,#1304,.T.);
#38001=EDGE_CURVE('',#29690,#29692,#24411,.T.);
#38002=EDGE_CURVE('',#29693,#29694,#16453,.T.);
#38003=EDGE_CURVE('',#29693,#29689,#24412,.T.);
#38004=EDGE_CURVE('',#29694,#29690,#24413,.T.);
#38005=EDGE_CURVE('',#29695,#29696,#16454,.T.);
#38006=EDGE_CURVE('',#29695,#29693,#24414,.T.);
#38007=EDGE_CURVE('',#29696,#29694,#24415,.T.);
#38008=EDGE_CURVE('',#29697,#29698,#16455,.T.);
#38009=EDGE_CURVE('',#29697,#29695,#24416,.T.);
#38010=EDGE_CURVE('',#29698,#29696,#24417,.T.);
#38011=EDGE_CURVE('',#29691,#29699,#24418,.T.);
#38012=EDGE_CURVE('',#29700,#29699,#1305,.F.);
#38013=EDGE_CURVE('',#29701,#29700,#1306,.F.);
#38014=EDGE_CURVE('',#29701,#29692,#24419,.T.);
#38015=EDGE_CURVE('',#29688,#29701,#24420,.T.);
#38016=EDGE_CURVE('',#29702,#29680,#24421,.T.);
#38017=EDGE_CURVE('',#29702,#29698,#24422,.T.);
#38018=EDGE_CURVE('',#29680,#29703,#1307,.T.);
#38019=EDGE_CURVE('',#29703,#29679,#1308,.T.);
#38020=EDGE_CURVE('',#29679,#29704,#24423,.T.);
#38021=EDGE_CURVE('',#29704,#29702,#1309,.T.);
#38022=EDGE_CURVE('',#29704,#29697,#24424,.T.);
#38023=EDGE_CURVE('',#29699,#29687,#24425,.T.);
#38024=EDGE_CURVE('',#29705,#29705,#1310,.T.);
#38025=EDGE_CURVE('',#29705,#29706,#16456,.T.);
#38026=EDGE_CURVE('',#29707,#29706,#383,.T.);
#38027=EDGE_CURVE('',#29707,#29708,#1311,.T.);
#38028=EDGE_CURVE('',#29709,#29708,#384,.T.);
#38029=EDGE_CURVE('',#29710,#29709,#385,.T.);
#38030=EDGE_CURVE('',#29710,#29711,#1312,.T.);
#38031=EDGE_CURVE('',#29712,#29711,#386,.T.);
#38032=EDGE_CURVE('',#29713,#29712,#387,.T.);
#38033=EDGE_CURVE('',#29713,#29714,#1313,.T.);
#38034=EDGE_CURVE('',#29715,#29714,#388,.T.);
#38035=EDGE_CURVE('',#29716,#29715,#389,.T.);
#38036=EDGE_CURVE('',#29716,#29717,#1314,.T.);
#38037=EDGE_CURVE('',#29718,#29717,#390,.T.);
#38038=EDGE_CURVE('',#29719,#29718,#391,.T.);
#38039=EDGE_CURVE('',#29719,#29720,#1315,.T.);
#38040=EDGE_CURVE('',#29721,#29720,#392,.T.);
#38041=EDGE_CURVE('',#29722,#29721,#393,.T.);
#38042=EDGE_CURVE('',#29722,#29723,#1316,.T.);
#38043=EDGE_CURVE('',#29706,#29723,#394,.T.);
#38044=EDGE_CURVE('',#29711,#29724,#16457,.T.);
#38045=EDGE_CURVE('',#29725,#29710,#16458,.T.);
#38046=EDGE_CURVE('',#29724,#29725,#1317,.T.);
#38047=EDGE_CURVE('',#29714,#29726,#16459,.T.);
#38048=EDGE_CURVE('',#29727,#29713,#16460,.T.);
#38049=EDGE_CURVE('',#29726,#29727,#1318,.T.);
#38050=EDGE_CURVE('',#29728,#29707,#16461,.T.);
#38051=EDGE_CURVE('',#29729,#29728,#1319,.T.);
#38052=EDGE_CURVE('',#29708,#29729,#16462,.T.);
#38053=EDGE_CURVE('',#29717,#29730,#16463,.T.);
#38054=EDGE_CURVE('',#29731,#29716,#16464,.T.);
#38055=EDGE_CURVE('',#29730,#29731,#1320,.T.);
#38056=EDGE_CURVE('',#29732,#29722,#16465,.T.);
#38057=EDGE_CURVE('',#29733,#29732,#1321,.T.);
#38058=EDGE_CURVE('',#29723,#29733,#16466,.T.);
#38059=EDGE_CURVE('',#29734,#29719,#16467,.T.);
#38060=EDGE_CURVE('',#29735,#29734,#1322,.T.);
#38061=EDGE_CURVE('',#29720,#29735,#16468,.T.);
#38062=EDGE_CURVE('',#29731,#29730,#16469,.T.);
#38063=EDGE_CURVE('',#29715,#29736,#16470,.T.);
#38064=EDGE_CURVE('',#29736,#29737,#16471,.T.);
#38065=EDGE_CURVE('',#29718,#29737,#16472,.T.);
#38066=EDGE_CURVE('',#29727,#29726,#16473,.T.);
#38067=EDGE_CURVE('',#29712,#29738,#16474,.T.);
#38068=EDGE_CURVE('',#29738,#29736,#16475,.T.);
#38069=EDGE_CURVE('',#29725,#29724,#16476,.T.);
#38070=EDGE_CURVE('',#29709,#29739,#16477,.T.);
#38071=EDGE_CURVE('',#29739,#29738,#16478,.T.);
#38072=EDGE_CURVE('',#29728,#29729,#16479,.T.);
#38073=EDGE_CURVE('',#29732,#29733,#16480,.T.);
#38074=EDGE_CURVE('',#29734,#29735,#16481,.T.);
#38075=EDGE_CURVE('',#29740,#29739,#16482,.T.);
#38076=EDGE_CURVE('',#29740,#29739,#1323,.T.);
#38077=EDGE_CURVE('',#29739,#29738,#1324,.T.);
#38078=EDGE_CURVE('',#29738,#29736,#1325,.T.);
#38079=EDGE_CURVE('',#29736,#29737,#1326,.T.);
#38080=EDGE_CURVE('',#29737,#29741,#16483,.T.);
#38081=EDGE_CURVE('',#29737,#29741,#1327,.T.);
#38082=EDGE_CURVE('',#29741,#29740,#16484,.T.);
#38083=EDGE_CURVE('',#29741,#29740,#1328,.T.);
#38084=EDGE_CURVE('',#29740,#29742,#16485,.T.);
#38085=EDGE_CURVE('',#29706,#29740,#16486,.T.);
#38086=EDGE_CURVE('',#29721,#29741,#16487,.T.);
#38087=EDGE_CURVE('',#29743,#29743,#1329,.T.);
#38088=EDGE_CURVE('',#29703,#29743,#16488,.T.);
#38089=EDGE_CURVE('',#29699,#29701,#1330,.F.);
#38090=EDGE_CURVE('',#29744,#29744,#1331,.T.);
#38091=EDGE_CURVE('',#29744,#29700,#16489,.T.);
#38092=EDGE_CURVE('',#29745,#29746,#16490,.T.);
#38093=EDGE_CURVE('',#29745,#29747,#24426,.T.);
#38094=EDGE_CURVE('',#29747,#29748,#1332,.T.);
#38095=EDGE_CURVE('',#29748,#29746,#24427,.T.);
#38096=EDGE_CURVE('',#29749,#29750,#16491,.T.);
#38097=EDGE_CURVE('',#29749,#29745,#24428,.T.);
#38098=EDGE_CURVE('',#29746,#29750,#24429,.T.);
#38099=EDGE_CURVE('',#29751,#29752,#16492,.T.);
#38100=EDGE_CURVE('',#29751,#29749,#24430,.T.);
#38101=EDGE_CURVE('',#29750,#29752,#24431,.T.);
#38102=EDGE_CURVE('',#29753,#29754,#16493,.T.);
#38103=EDGE_CURVE('',#29755,#29753,#1333,.F.);
#38104=EDGE_CURVE('',#29755,#29751,#24432,.T.);
#38105=EDGE_CURVE('',#29752,#29754,#24433,.T.);
#38106=EDGE_CURVE('',#29756,#29757,#16494,.T.);
#38107=EDGE_CURVE('',#29756,#29758,#24434,.T.);
#38108=EDGE_CURVE('',#29759,#29758,#1334,.T.);
#38109=EDGE_CURVE('',#29757,#29759,#24435,.T.);
#38110=EDGE_CURVE('',#29760,#29761,#16495,.T.);
#38111=EDGE_CURVE('',#29760,#29756,#24436,.T.);
#38112=EDGE_CURVE('',#29761,#29757,#24437,.T.);
#38113=EDGE_CURVE('',#29762,#29763,#16496,.T.);
#38114=EDGE_CURVE('',#29762,#29760,#24438,.T.);
#38115=EDGE_CURVE('',#29763,#29761,#24439,.T.);
#38116=EDGE_CURVE('',#29758,#29755,#24440,.T.);
#38117=EDGE_CURVE('',#29764,#29755,#1335,.F.);
#38118=EDGE_CURVE('',#29764,#29759,#24441,.T.);
#38119=EDGE_CURVE('',#29754,#29764,#24442,.T.);
#38120=EDGE_CURVE('',#29765,#29748,#24443,.T.);
#38121=EDGE_CURVE('',#29765,#29763,#24444,.T.);
#38122=EDGE_CURVE('',#29748,#29766,#1336,.T.);
#38123=EDGE_CURVE('',#29766,#29747,#1337,.T.);
#38124=EDGE_CURVE('',#29747,#29767,#24445,.T.);
#38125=EDGE_CURVE('',#29767,#29765,#1338,.T.);
#38126=EDGE_CURVE('',#29767,#29762,#24446,.T.);
#38127=EDGE_CURVE('',#29768,#29768,#1339,.T.);
#38128=EDGE_CURVE('',#29768,#29769,#16497,.T.);
#38129=EDGE_CURVE('',#29770,#29769,#395,.T.);
#38130=EDGE_CURVE('',#29770,#29771,#1340,.T.);
#38131=EDGE_CURVE('',#29772,#29771,#396,.T.);
#38132=EDGE_CURVE('',#29773,#29772,#397,.T.);
#38133=EDGE_CURVE('',#29773,#29774,#1341,.T.);
#38134=EDGE_CURVE('',#29775,#29774,#398,.T.);
#38135=EDGE_CURVE('',#29776,#29775,#399,.T.);
#38136=EDGE_CURVE('',#29776,#29777,#1342,.T.);
#38137=EDGE_CURVE('',#29778,#29777,#400,.T.);
#38138=EDGE_CURVE('',#29779,#29778,#401,.T.);
#38139=EDGE_CURVE('',#29779,#29780,#1343,.T.);
#38140=EDGE_CURVE('',#29781,#29780,#402,.T.);
#38141=EDGE_CURVE('',#29782,#29781,#403,.T.);
#38142=EDGE_CURVE('',#29782,#29783,#1344,.T.);
#38143=EDGE_CURVE('',#29784,#29783,#404,.T.);
#38144=EDGE_CURVE('',#29785,#29784,#405,.T.);
#38145=EDGE_CURVE('',#29785,#29786,#1345,.T.);
#38146=EDGE_CURVE('',#29769,#29786,#406,.T.);
#38147=EDGE_CURVE('',#29774,#29787,#16498,.T.);
#38148=EDGE_CURVE('',#29788,#29773,#16499,.T.);
#38149=EDGE_CURVE('',#29787,#29788,#1346,.T.);
#38150=EDGE_CURVE('',#29777,#29789,#16500,.T.);
#38151=EDGE_CURVE('',#29790,#29776,#16501,.T.);
#38152=EDGE_CURVE('',#29789,#29790,#1347,.T.);
#38153=EDGE_CURVE('',#29791,#29770,#16502,.T.);
#38154=EDGE_CURVE('',#29792,#29791,#1348,.T.);
#38155=EDGE_CURVE('',#29771,#29792,#16503,.T.);
#38156=EDGE_CURVE('',#29780,#29793,#16504,.T.);
#38157=EDGE_CURVE('',#29794,#29779,#16505,.T.);
#38158=EDGE_CURVE('',#29793,#29794,#1349,.T.);
#38159=EDGE_CURVE('',#29795,#29785,#16506,.T.);
#38160=EDGE_CURVE('',#29796,#29795,#1350,.T.);
#38161=EDGE_CURVE('',#29786,#29796,#16507,.T.);
#38162=EDGE_CURVE('',#29797,#29782,#16508,.T.);
#38163=EDGE_CURVE('',#29798,#29797,#1351,.T.);
#38164=EDGE_CURVE('',#29783,#29798,#16509,.T.);
#38165=EDGE_CURVE('',#29794,#29793,#16510,.T.);
#38166=EDGE_CURVE('',#29778,#29799,#16511,.T.);
#38167=EDGE_CURVE('',#29799,#29800,#16512,.T.);
#38168=EDGE_CURVE('',#29781,#29800,#16513,.T.);
#38169=EDGE_CURVE('',#29790,#29789,#16514,.T.);
#38170=EDGE_CURVE('',#29775,#29801,#16515,.T.);
#38171=EDGE_CURVE('',#29801,#29799,#16516,.T.);
#38172=EDGE_CURVE('',#29788,#29787,#16517,.T.);
#38173=EDGE_CURVE('',#29772,#29802,#16518,.T.);
#38174=EDGE_CURVE('',#29802,#29801,#16519,.T.);
#38175=EDGE_CURVE('',#29791,#29792,#16520,.T.);
#38176=EDGE_CURVE('',#29795,#29796,#16521,.T.);
#38177=EDGE_CURVE('',#29797,#29798,#16522,.T.);
#38178=EDGE_CURVE('',#29803,#29802,#16523,.T.);
#38179=EDGE_CURVE('',#29803,#29802,#1352,.T.);
#38180=EDGE_CURVE('',#29802,#29801,#1353,.T.);
#38181=EDGE_CURVE('',#29801,#29799,#1354,.T.);
#38182=EDGE_CURVE('',#29799,#29800,#1355,.T.);
#38183=EDGE_CURVE('',#29800,#29804,#16524,.T.);
#38184=EDGE_CURVE('',#29800,#29804,#1356,.T.);
#38185=EDGE_CURVE('',#29804,#29803,#16525,.T.);
#38186=EDGE_CURVE('',#29804,#29803,#1357,.T.);
#38187=EDGE_CURVE('',#29803,#29805,#16526,.T.);
#38188=EDGE_CURVE('',#29769,#29803,#16527,.T.);
#38189=EDGE_CURVE('',#29784,#29804,#16528,.T.);
#38190=EDGE_CURVE('',#29806,#29806,#1358,.T.);
#38191=EDGE_CURVE('',#29766,#29806,#16529,.T.);
#38192=EDGE_CURVE('',#29753,#29764,#1359,.F.);
#38193=EDGE_CURVE('',#29807,#29807,#1360,.T.);
#38194=EDGE_CURVE('',#29807,#29753,#16530,.T.);
#38195=EDGE_CURVE('',#29808,#29809,#16531,.T.);
#38196=EDGE_CURVE('',#29808,#29810,#24447,.T.);
#38197=EDGE_CURVE('',#29810,#29811,#1361,.T.);
#38198=EDGE_CURVE('',#29811,#29809,#24448,.T.);
#38199=EDGE_CURVE('',#29812,#29813,#16532,.T.);
#38200=EDGE_CURVE('',#29812,#29808,#24449,.T.);
#38201=EDGE_CURVE('',#29809,#29813,#24450,.T.);
#38202=EDGE_CURVE('',#29814,#29815,#16533,.T.);
#38203=EDGE_CURVE('',#29814,#29812,#24451,.T.);
#38204=EDGE_CURVE('',#29813,#29815,#24452,.T.);
#38205=EDGE_CURVE('',#29816,#29817,#16534,.T.);
#38206=EDGE_CURVE('',#29816,#29814,#24453,.T.);
#38207=EDGE_CURVE('',#29815,#29817,#24454,.T.);
#38208=EDGE_CURVE('',#29818,#29819,#16535,.T.);
#38209=EDGE_CURVE('',#29818,#29816,#24455,.T.);
#38210=EDGE_CURVE('',#29817,#29819,#24456,.T.);
#38211=EDGE_CURVE('',#29820,#29821,#16536,.T.);
#38212=EDGE_CURVE('',#29820,#29818,#24457,.T.);
#38213=EDGE_CURVE('',#29819,#29821,#24458,.T.);
#38214=EDGE_CURVE('',#29822,#29823,#16537,.T.);
#38215=EDGE_CURVE('',#29822,#29820,#24459,.T.);
#38216=EDGE_CURVE('',#29821,#29823,#24460,.T.);
#38217=EDGE_CURVE('',#29824,#29825,#16538,.T.);
#38218=EDGE_CURVE('',#29824,#29822,#24461,.T.);
#38219=EDGE_CURVE('',#29823,#29825,#24462,.T.);
#38220=EDGE_CURVE('',#29826,#29827,#16539,.T.);
#38221=EDGE_CURVE('',#29826,#29824,#24463,.T.);
#38222=EDGE_CURVE('',#29825,#29827,#24464,.T.);
#38223=EDGE_CURVE('',#29828,#29829,#16540,.T.);
#38224=EDGE_CURVE('',#29828,#29826,#24465,.T.);
#38225=EDGE_CURVE('',#29827,#29829,#24466,.T.);
#38226=EDGE_CURVE('',#29830,#29831,#16541,.T.);
#38227=EDGE_CURVE('',#29830,#29828,#24467,.T.);
#38228=EDGE_CURVE('',#29829,#29831,#24468,.T.);
#38229=EDGE_CURVE('',#29832,#29833,#16542,.T.);
#38230=EDGE_CURVE('',#29832,#29834,#24469,.T.);
#38231=EDGE_CURVE('',#29835,#29834,#1362,.T.);
#38232=EDGE_CURVE('',#29833,#29835,#24470,.T.);
#38233=EDGE_CURVE('',#29836,#29837,#16543,.T.);
#38234=EDGE_CURVE('',#29836,#29832,#24471,.T.);
#38235=EDGE_CURVE('',#29837,#29833,#24472,.T.);
#38236=EDGE_CURVE('',#29838,#29839,#16544,.T.);
#38237=EDGE_CURVE('',#29838,#29836,#24473,.T.);
#38238=EDGE_CURVE('',#29839,#29837,#24474,.T.);
#38239=EDGE_CURVE('',#29840,#29841,#16545,.T.);
#38240=EDGE_CURVE('',#29840,#29838,#24475,.T.);
#38241=EDGE_CURVE('',#29841,#29839,#24476,.T.);
#38242=EDGE_CURVE('',#29842,#29843,#16546,.T.);
#38243=EDGE_CURVE('',#29842,#29840,#24477,.T.);
#38244=EDGE_CURVE('',#29843,#29841,#24478,.T.);
#38245=EDGE_CURVE('',#29844,#29845,#16547,.T.);
#38246=EDGE_CURVE('',#29844,#29842,#24479,.T.);
#38247=EDGE_CURVE('',#29845,#29843,#24480,.T.);
#38248=EDGE_CURVE('',#29846,#29847,#16548,.T.);
#38249=EDGE_CURVE('',#29846,#29844,#24481,.T.);
#38250=EDGE_CURVE('',#29847,#29845,#24482,.T.);
#38251=EDGE_CURVE('',#29848,#29849,#16549,.T.);
#38252=EDGE_CURVE('',#29848,#29846,#24483,.T.);
#38253=EDGE_CURVE('',#29849,#29847,#24484,.T.);
#38254=EDGE_CURVE('',#29850,#29851,#16550,.T.);
#38255=EDGE_CURVE('',#29850,#29848,#24485,.T.);
#38256=EDGE_CURVE('',#29851,#29849,#24486,.T.);
#38257=EDGE_CURVE('',#29852,#29853,#16551,.T.);
#38258=EDGE_CURVE('',#29852,#29850,#24487,.T.);
#38259=EDGE_CURVE('',#29853,#29851,#24488,.T.);
#38260=EDGE_CURVE('',#29834,#29854,#24489,.T.);
#38261=EDGE_CURVE('',#29855,#29854,#1363,.F.);
#38262=EDGE_CURVE('',#29856,#29855,#1364,.F.);
#38263=EDGE_CURVE('',#29856,#29835,#24490,.T.);
#38264=EDGE_CURVE('',#29831,#29856,#24491,.T.);
#38265=EDGE_CURVE('',#29857,#29811,#24492,.T.);
#38266=EDGE_CURVE('',#29857,#29853,#24493,.T.);
#38267=EDGE_CURVE('',#29811,#29858,#1365,.T.);
#38268=EDGE_CURVE('',#29858,#29810,#1366,.T.);
#38269=EDGE_CURVE('',#29810,#29859,#24494,.T.);
#38270=EDGE_CURVE('',#29859,#29857,#1367,.T.);
#38271=EDGE_CURVE('',#29859,#29852,#24495,.T.);
#38272=EDGE_CURVE('',#29854,#29830,#24496,.T.);
#38273=EDGE_CURVE('',#29860,#29860,#1368,.T.);
#38274=EDGE_CURVE('',#29860,#29861,#16552,.T.);
#38275=EDGE_CURVE('',#29862,#29861,#407,.T.);
#38276=EDGE_CURVE('',#29862,#29863,#1369,.T.);
#38277=EDGE_CURVE('',#29864,#29863,#408,.T.);
#38278=EDGE_CURVE('',#29865,#29864,#409,.T.);
#38279=EDGE_CURVE('',#29865,#29866,#1370,.T.);
#38280=EDGE_CURVE('',#29867,#29866,#410,.T.);
#38281=EDGE_CURVE('',#29868,#29867,#411,.T.);
#38282=EDGE_CURVE('',#29868,#29869,#1371,.T.);
#38283=EDGE_CURVE('',#29870,#29869,#412,.T.);
#38284=EDGE_CURVE('',#29871,#29870,#413,.T.);
#38285=EDGE_CURVE('',#29871,#29872,#1372,.T.);
#38286=EDGE_CURVE('',#29873,#29872,#414,.T.);
#38287=EDGE_CURVE('',#29874,#29873,#415,.T.);
#38288=EDGE_CURVE('',#29874,#29875,#1373,.T.);
#38289=EDGE_CURVE('',#29876,#29875,#416,.T.);
#38290=EDGE_CURVE('',#29877,#29876,#417,.T.);
#38291=EDGE_CURVE('',#29877,#29878,#1374,.T.);
#38292=EDGE_CURVE('',#29861,#29878,#418,.T.);
#38293=EDGE_CURVE('',#29869,#29879,#16553,.T.);
#38294=EDGE_CURVE('',#29880,#29868,#16554,.T.);
#38295=EDGE_CURVE('',#29879,#29880,#1375,.T.);
#38296=EDGE_CURVE('',#29872,#29881,#16555,.T.);
#38297=EDGE_CURVE('',#29882,#29871,#16556,.T.);
#38298=EDGE_CURVE('',#29881,#29882,#1376,.T.);
#38299=EDGE_CURVE('',#29883,#29865,#16557,.T.);
#38300=EDGE_CURVE('',#29884,#29883,#1377,.T.);
#38301=EDGE_CURVE('',#29866,#29884,#16558,.T.);
#38302=EDGE_CURVE('',#29875,#29885,#16559,.T.);
#38303=EDGE_CURVE('',#29886,#29874,#16560,.T.);
#38304=EDGE_CURVE('',#29885,#29886,#1378,.T.);
#38305=EDGE_CURVE('',#29887,#29862,#16561,.T.);
#38306=EDGE_CURVE('',#29888,#29887,#1379,.T.);
#38307=EDGE_CURVE('',#29863,#29888,#16562,.T.);
#38308=EDGE_CURVE('',#29889,#29877,#16563,.T.);
#38309=EDGE_CURVE('',#29890,#29889,#1380,.T.);
#38310=EDGE_CURVE('',#29878,#29890,#16564,.T.);
#38311=EDGE_CURVE('',#29886,#29885,#16565,.T.);
#38312=EDGE_CURVE('',#29873,#29891,#16566,.T.);
#38313=EDGE_CURVE('',#29891,#29892,#16567,.T.);
#38314=EDGE_CURVE('',#29876,#29892,#16568,.T.);
#38315=EDGE_CURVE('',#29882,#29881,#16569,.T.);
#38316=EDGE_CURVE('',#29870,#29893,#16570,.T.);
#38317=EDGE_CURVE('',#29893,#29891,#16571,.T.);
#38318=EDGE_CURVE('',#29880,#29879,#16572,.T.);
#38319=EDGE_CURVE('',#29867,#29894,#16573,.T.);
#38320=EDGE_CURVE('',#29894,#29893,#16574,.T.);
#38321=EDGE_CURVE('',#29883,#29884,#16575,.T.);
#38322=EDGE_CURVE('',#29887,#29888,#16576,.T.);
#38323=EDGE_CURVE('',#29889,#29890,#16577,.T.);
#38324=EDGE_CURVE('',#29895,#29894,#16578,.T.);
#38325=EDGE_CURVE('',#29895,#29894,#1381,.T.);
#38326=EDGE_CURVE('',#29894,#29893,#1382,.T.);
#38327=EDGE_CURVE('',#29893,#29891,#1383,.T.);
#38328=EDGE_CURVE('',#29891,#29892,#1384,.T.);
#38329=EDGE_CURVE('',#29892,#29896,#16579,.T.);
#38330=EDGE_CURVE('',#29892,#29896,#1385,.T.);
#38331=EDGE_CURVE('',#29896,#29895,#16580,.T.);
#38332=EDGE_CURVE('',#29896,#29895,#1386,.T.);
#38333=EDGE_CURVE('',#29896,#29897,#16581,.T.);
#38334=EDGE_CURVE('',#29864,#29895,#16582,.T.);
#38335=EDGE_CURVE('',#29861,#29896,#16583,.T.);
#38336=EDGE_CURVE('',#29898,#29898,#1387,.T.);
#38337=EDGE_CURVE('',#29858,#29898,#16584,.T.);
#38338=EDGE_CURVE('',#29854,#29856,#1388,.F.);
#38339=EDGE_CURVE('',#29899,#29899,#1389,.T.);
#38340=EDGE_CURVE('',#29899,#29855,#16585,.T.);
#38341=EDGE_CURVE('',#29900,#29901,#16586,.T.);
#38342=EDGE_CURVE('',#29900,#29902,#24497,.T.);
#38343=EDGE_CURVE('',#29902,#29903,#1390,.T.);
#38344=EDGE_CURVE('',#29903,#29901,#24498,.T.);
#38345=EDGE_CURVE('',#29904,#29905,#16587,.T.);
#38346=EDGE_CURVE('',#29904,#29900,#24499,.T.);
#38347=EDGE_CURVE('',#29901,#29905,#24500,.T.);
#38348=EDGE_CURVE('',#29906,#29907,#16588,.T.);
#38349=EDGE_CURVE('',#29906,#29904,#24501,.T.);
#38350=EDGE_CURVE('',#29905,#29907,#24502,.T.);
#38351=EDGE_CURVE('',#29908,#29909,#16589,.T.);
#38352=EDGE_CURVE('',#29908,#29906,#24503,.T.);
#38353=EDGE_CURVE('',#29907,#29909,#24504,.T.);
#38354=EDGE_CURVE('',#29910,#29911,#16590,.T.);
#38355=EDGE_CURVE('',#29910,#29908,#24505,.T.);
#38356=EDGE_CURVE('',#29909,#29911,#24506,.T.);
#38357=EDGE_CURVE('',#29912,#29913,#16591,.T.);
#38358=EDGE_CURVE('',#29912,#29910,#24507,.T.);
#38359=EDGE_CURVE('',#29911,#29913,#24508,.T.);
#38360=EDGE_CURVE('',#29914,#29915,#16592,.T.);
#38361=EDGE_CURVE('',#29914,#29916,#24509,.T.);
#38362=EDGE_CURVE('',#29915,#29916,#1391,.T.);
#38363=EDGE_CURVE('',#29917,#29918,#16593,.T.);
#38364=EDGE_CURVE('',#29917,#29914,#24510,.T.);
#38365=EDGE_CURVE('',#29919,#29915,#1392,.T.);
#38366=EDGE_CURVE('',#29918,#29919,#24511,.T.);
#38367=EDGE_CURVE('',#29920,#29921,#16594,.T.);
#38368=EDGE_CURVE('',#29920,#29917,#24512,.T.);
#38369=EDGE_CURVE('',#29921,#29918,#24513,.T.);
#38370=EDGE_CURVE('',#29922,#29923,#16595,.T.);
#38371=EDGE_CURVE('',#29922,#29920,#24514,.T.);
#38372=EDGE_CURVE('',#29923,#29921,#24515,.T.);
#38373=EDGE_CURVE('',#29924,#29925,#16596,.T.);
#38374=EDGE_CURVE('',#29924,#29922,#24516,.T.);
#38375=EDGE_CURVE('',#29925,#29923,#24517,.T.);
#38376=EDGE_CURVE('',#29926,#29927,#16597,.T.);
#38377=EDGE_CURVE('',#29926,#29924,#24518,.T.);
#38378=EDGE_CURVE('',#29927,#29925,#24519,.T.);
#38379=EDGE_CURVE('',#29916,#29928,#24520,.T.);
#38380=EDGE_CURVE('',#29929,#29928,#1393,.F.);
#38381=EDGE_CURVE('',#29930,#29929,#1394,.F.);
#38382=EDGE_CURVE('',#29930,#29919,#24521,.T.);
#38383=EDGE_CURVE('',#29913,#29930,#24522,.T.);
#38384=EDGE_CURVE('',#29931,#29903,#24523,.T.);
#38385=EDGE_CURVE('',#29931,#29927,#24524,.T.);
#38386=EDGE_CURVE('',#29903,#29932,#1395,.T.);
#38387=EDGE_CURVE('',#29932,#29902,#1396,.T.);
#38388=EDGE_CURVE('',#29902,#29933,#24525,.T.);
#38389=EDGE_CURVE('',#29933,#29931,#1397,.T.);
#38390=EDGE_CURVE('',#29933,#29926,#24526,.T.);
#38391=EDGE_CURVE('',#29928,#29912,#24527,.T.);
#38392=EDGE_CURVE('',#29934,#29934,#1398,.T.);
#38393=EDGE_CURVE('',#29934,#29935,#16598,.T.);
#38394=EDGE_CURVE('',#29936,#29935,#419,.T.);
#38395=EDGE_CURVE('',#29936,#29937,#1399,.T.);
#38396=EDGE_CURVE('',#29938,#29937,#420,.T.);
#38397=EDGE_CURVE('',#29939,#29938,#421,.T.);
#38398=EDGE_CURVE('',#29939,#29940,#1400,.T.);
#38399=EDGE_CURVE('',#29941,#29940,#422,.T.);
#38400=EDGE_CURVE('',#29942,#29941,#423,.T.);
#38401=EDGE_CURVE('',#29942,#29943,#1401,.T.);
#38402=EDGE_CURVE('',#29944,#29943,#424,.T.);
#38403=EDGE_CURVE('',#29945,#29944,#425,.T.);
#38404=EDGE_CURVE('',#29945,#29946,#1402,.T.);
#38405=EDGE_CURVE('',#29947,#29946,#426,.T.);
#38406=EDGE_CURVE('',#29948,#29947,#427,.T.);
#38407=EDGE_CURVE('',#29948,#29949,#1403,.T.);
#38408=EDGE_CURVE('',#29950,#29949,#428,.T.);
#38409=EDGE_CURVE('',#29951,#29950,#429,.T.);
#38410=EDGE_CURVE('',#29951,#29952,#1404,.T.);
#38411=EDGE_CURVE('',#29935,#29952,#430,.T.);
#38412=EDGE_CURVE('',#29940,#29953,#16599,.T.);
#38413=EDGE_CURVE('',#29954,#29939,#16600,.T.);
#38414=EDGE_CURVE('',#29953,#29954,#1405,.T.);
#38415=EDGE_CURVE('',#29943,#29955,#16601,.T.);
#38416=EDGE_CURVE('',#29956,#29942,#16602,.T.);
#38417=EDGE_CURVE('',#29955,#29956,#1406,.T.);
#38418=EDGE_CURVE('',#29957,#29936,#16603,.T.);
#38419=EDGE_CURVE('',#29958,#29957,#1407,.T.);
#38420=EDGE_CURVE('',#29937,#29958,#16604,.T.);
#38421=EDGE_CURVE('',#29946,#29959,#16605,.T.);
#38422=EDGE_CURVE('',#29960,#29945,#16606,.T.);
#38423=EDGE_CURVE('',#29959,#29960,#1408,.T.);
#38424=EDGE_CURVE('',#29961,#29951,#16607,.T.);
#38425=EDGE_CURVE('',#29962,#29961,#1409,.T.);
#38426=EDGE_CURVE('',#29952,#29962,#16608,.T.);
#38427=EDGE_CURVE('',#29963,#29948,#16609,.T.);
#38428=EDGE_CURVE('',#29964,#29963,#1410,.T.);
#38429=EDGE_CURVE('',#29949,#29964,#16610,.T.);
#38430=EDGE_CURVE('',#29960,#29959,#16611,.T.);
#38431=EDGE_CURVE('',#29944,#29965,#16612,.T.);
#38432=EDGE_CURVE('',#29965,#29966,#16613,.T.);
#38433=EDGE_CURVE('',#29947,#29966,#16614,.T.);
#38434=EDGE_CURVE('',#29956,#29955,#16615,.T.);
#38435=EDGE_CURVE('',#29941,#29967,#16616,.T.);
#38436=EDGE_CURVE('',#29967,#29965,#16617,.T.);
#38437=EDGE_CURVE('',#29954,#29953,#16618,.T.);
#38438=EDGE_CURVE('',#29938,#29968,#16619,.T.);
#38439=EDGE_CURVE('',#29968,#29967,#16620,.T.);
#38440=EDGE_CURVE('',#29957,#29958,#16621,.T.);
#38441=EDGE_CURVE('',#29961,#29962,#16622,.T.);
#38442=EDGE_CURVE('',#29963,#29964,#16623,.T.);
#38443=EDGE_CURVE('',#29969,#29968,#16624,.T.);
#38444=EDGE_CURVE('',#29969,#29968,#1411,.T.);
#38445=EDGE_CURVE('',#29968,#29967,#1412,.T.);
#38446=EDGE_CURVE('',#29967,#29965,#1413,.T.);
#38447=EDGE_CURVE('',#29965,#29966,#1414,.T.);
#38448=EDGE_CURVE('',#29966,#29970,#16625,.T.);
#38449=EDGE_CURVE('',#29966,#29970,#1415,.T.);
#38450=EDGE_CURVE('',#29970,#29969,#16626,.T.);
#38451=EDGE_CURVE('',#29970,#29969,#1416,.T.);
#38452=EDGE_CURVE('',#29969,#29971,#16627,.T.);
#38453=EDGE_CURVE('',#29935,#29969,#16628,.T.);
#38454=EDGE_CURVE('',#29950,#29970,#16629,.T.);
#38455=EDGE_CURVE('',#29972,#29972,#1417,.T.);
#38456=EDGE_CURVE('',#29932,#29972,#16630,.T.);
#38457=EDGE_CURVE('',#29928,#29930,#1418,.F.);
#38458=EDGE_CURVE('',#29973,#29973,#1419,.T.);
#38459=EDGE_CURVE('',#29973,#29929,#16631,.T.);
#38460=EDGE_CURVE('',#29974,#29975,#16632,.T.);
#38461=EDGE_CURVE('',#29974,#29976,#24528,.T.);
#38462=EDGE_CURVE('',#29976,#29977,#1420,.T.);
#38463=EDGE_CURVE('',#29977,#29975,#24529,.T.);
#38464=EDGE_CURVE('',#29978,#29979,#16633,.T.);
#38465=EDGE_CURVE('',#29978,#29974,#24530,.T.);
#38466=EDGE_CURVE('',#29975,#29979,#24531,.T.);
#38467=EDGE_CURVE('',#29980,#29981,#16634,.T.);
#38468=EDGE_CURVE('',#29980,#29978,#24532,.T.);
#38469=EDGE_CURVE('',#29979,#29981,#24533,.T.);
#38470=EDGE_CURVE('',#29982,#29983,#16635,.T.);
#38471=EDGE_CURVE('',#29982,#29980,#24534,.T.);
#38472=EDGE_CURVE('',#29981,#29983,#24535,.T.);
#38473=EDGE_CURVE('',#29984,#29985,#16636,.T.);
#38474=EDGE_CURVE('',#29984,#29982,#24536,.T.);
#38475=EDGE_CURVE('',#29983,#29985,#24537,.T.);
#38476=EDGE_CURVE('',#29986,#29987,#16637,.T.);
#38477=EDGE_CURVE('',#29986,#29984,#24538,.T.);
#38478=EDGE_CURVE('',#29985,#29987,#24539,.T.);
#38479=EDGE_CURVE('',#29988,#29989,#16638,.T.);
#38480=EDGE_CURVE('',#29988,#29986,#24540,.T.);
#38481=EDGE_CURVE('',#29987,#29989,#24541,.T.);
#38482=EDGE_CURVE('',#29990,#29991,#16639,.T.);
#38483=EDGE_CURVE('',#29992,#29990,#1421,.T.);
#38484=EDGE_CURVE('',#29992,#29988,#24542,.T.);
#38485=EDGE_CURVE('',#29989,#29991,#24543,.T.);
#38486=EDGE_CURVE('',#29993,#29994,#16640,.T.);
#38487=EDGE_CURVE('',#29993,#29995,#24544,.T.);
#38488=EDGE_CURVE('',#29996,#29995,#1422,.T.);
#38489=EDGE_CURVE('',#29994,#29996,#24545,.T.);
#38490=EDGE_CURVE('',#29997,#29998,#16641,.T.);
#38491=EDGE_CURVE('',#29997,#29993,#24546,.T.);
#38492=EDGE_CURVE('',#29998,#29994,#24547,.T.);
#38493=EDGE_CURVE('',#29999,#30000,#16642,.T.);
#38494=EDGE_CURVE('',#29999,#29997,#24548,.T.);
#38495=EDGE_CURVE('',#30000,#29998,#24549,.T.);
#38496=EDGE_CURVE('',#30001,#30002,#16643,.T.);
#38497=EDGE_CURVE('',#30001,#29999,#24550,.T.);
#38498=EDGE_CURVE('',#30002,#30000,#24551,.T.);
#38499=EDGE_CURVE('',#30003,#30004,#16644,.T.);
#38500=EDGE_CURVE('',#30003,#30001,#24552,.T.);
#38501=EDGE_CURVE('',#30004,#30002,#24553,.T.);
#38502=EDGE_CURVE('',#30005,#30006,#16645,.T.);
#38503=EDGE_CURVE('',#30005,#30003,#24554,.T.);
#38504=EDGE_CURVE('',#30006,#30004,#24555,.T.);
#38505=EDGE_CURVE('',#30007,#30008,#16646,.T.);
#38506=EDGE_CURVE('',#30007,#30005,#24556,.T.);
#38507=EDGE_CURVE('',#30008,#30006,#24557,.T.);
#38508=EDGE_CURVE('',#29995,#29992,#24558,.T.);
#38509=EDGE_CURVE('',#30009,#29992,#1423,.T.);
#38510=EDGE_CURVE('',#30009,#29996,#24559,.T.);
#38511=EDGE_CURVE('',#29991,#30009,#24560,.T.);
#38512=EDGE_CURVE('',#30010,#29977,#24561,.T.);
#38513=EDGE_CURVE('',#30010,#30008,#24562,.T.);
#38514=EDGE_CURVE('',#29977,#30011,#1424,.T.);
#38515=EDGE_CURVE('',#30011,#29976,#1425,.T.);
#38516=EDGE_CURVE('',#29976,#30012,#24563,.T.);
#38517=EDGE_CURVE('',#30012,#30010,#1426,.T.);
#38518=EDGE_CURVE('',#30012,#30007,#24564,.T.);
#38519=EDGE_CURVE('',#30013,#30014,#16647,.T.);
#38520=EDGE_CURVE('',#30013,#30015,#16648,.T.);
#38521=EDGE_CURVE('',#30015,#30016,#16649,.T.);
#38522=EDGE_CURVE('',#30014,#30016,#16650,.T.);
#38523=EDGE_CURVE('',#30017,#30013,#16651,.T.);
#38524=EDGE_CURVE('',#30017,#30018,#16652,.T.);
#38525=EDGE_CURVE('',#30018,#30015,#16653,.T.);
#38526=EDGE_CURVE('',#30019,#30017,#16654,.T.);
#38527=EDGE_CURVE('',#30019,#30020,#16655,.T.);
#38528=EDGE_CURVE('',#30020,#30018,#16656,.T.);
#38529=EDGE_CURVE('',#30021,#30019,#16657,.T.);
#38530=EDGE_CURVE('',#30021,#30022,#16658,.T.);
#38531=EDGE_CURVE('',#30022,#30020,#16659,.T.);
#38532=EDGE_CURVE('',#30023,#30021,#16660,.T.);
#38533=EDGE_CURVE('',#30023,#30024,#16661,.T.);
#38534=EDGE_CURVE('',#30024,#30022,#16662,.T.);
#38535=EDGE_CURVE('',#30014,#30023,#16663,.T.);
#38536=EDGE_CURVE('',#30016,#30024,#16664,.T.);
#38537=EDGE_CURVE('',#30025,#30025,#1427,.T.);
#38538=EDGE_CURVE('',#30011,#30025,#16665,.T.);
#38539=EDGE_CURVE('',#29990,#30009,#1428,.T.);
#38540=EDGE_CURVE('',#30026,#30026,#1429,.T.);
#38541=EDGE_CURVE('',#30026,#29990,#16666,.T.);
#38542=EDGE_CURVE('',#30027,#30028,#16667,.T.);
#38543=EDGE_CURVE('',#30027,#30029,#24565,.T.);
#38544=EDGE_CURVE('',#30030,#30029,#1430,.T.);
#38545=EDGE_CURVE('',#30030,#30028,#24566,.T.);
#38546=EDGE_CURVE('',#30031,#30032,#16668,.T.);
#38547=EDGE_CURVE('',#30031,#30027,#24567,.T.);
#38548=EDGE_CURVE('',#30028,#30032,#24568,.T.);
#38549=EDGE_CURVE('',#30033,#30034,#16669,.T.);
#38550=EDGE_CURVE('',#30033,#30031,#24569,.T.);
#38551=EDGE_CURVE('',#30032,#30034,#24570,.T.);
#38552=EDGE_CURVE('',#30035,#30036,#16670,.T.);
#38553=EDGE_CURVE('',#30035,#30033,#24571,.T.);
#38554=EDGE_CURVE('',#30034,#30036,#24572,.T.);
#38555=EDGE_CURVE('',#30037,#30038,#16671,.T.);
#38556=EDGE_CURVE('',#30037,#30035,#24573,.T.);
#38557=EDGE_CURVE('',#30036,#30038,#24574,.T.);
#38558=EDGE_CURVE('',#30039,#30040,#16672,.T.);
#38559=EDGE_CURVE('',#30039,#30037,#24575,.T.);
#38560=EDGE_CURVE('',#30038,#30040,#24576,.T.);
#38561=EDGE_CURVE('',#30041,#30042,#16673,.T.);
#38562=EDGE_CURVE('',#30041,#30039,#24577,.T.);
#38563=EDGE_CURVE('',#30040,#30042,#24578,.T.);
#38564=EDGE_CURVE('',#30043,#30044,#16674,.T.);
#38565=EDGE_CURVE('',#30043,#30041,#24579,.T.);
#38566=EDGE_CURVE('',#30042,#30044,#24580,.T.);
#38567=EDGE_CURVE('',#30045,#30046,#16675,.T.);
#38568=EDGE_CURVE('',#30045,#30043,#24581,.T.);
#38569=EDGE_CURVE('',#30044,#30046,#24582,.T.);
#38570=EDGE_CURVE('',#30047,#30048,#16676,.T.);
#38571=EDGE_CURVE('',#30047,#30045,#24583,.T.);
#38572=EDGE_CURVE('',#30046,#30048,#24584,.T.);
#38573=EDGE_CURVE('',#30049,#30050,#16677,.T.);
#38574=EDGE_CURVE('',#30049,#30047,#24585,.T.);
#38575=EDGE_CURVE('',#30048,#30050,#24586,.T.);
#38576=EDGE_CURVE('',#30051,#30052,#16678,.T.);
#38577=EDGE_CURVE('',#30051,#30049,#24587,.T.);
#38578=EDGE_CURVE('',#30050,#30052,#24588,.T.);
#38579=EDGE_CURVE('',#30053,#30054,#16679,.T.);
#38580=EDGE_CURVE('',#30053,#30051,#24589,.T.);
#38581=EDGE_CURVE('',#30052,#30054,#24590,.T.);
#38582=EDGE_CURVE('',#30055,#30056,#16680,.T.);
#38583=EDGE_CURVE('',#30055,#30057,#24591,.T.);
#38584=EDGE_CURVE('',#30058,#30057,#1431,.T.);
#38585=EDGE_CURVE('',#30056,#30058,#24592,.T.);
#38586=EDGE_CURVE('',#30059,#30060,#16681,.T.);
#38587=EDGE_CURVE('',#30059,#30055,#24593,.T.);
#38588=EDGE_CURVE('',#30060,#30056,#24594,.T.);
#38589=EDGE_CURVE('',#30061,#30062,#16682,.T.);
#38590=EDGE_CURVE('',#30061,#30059,#24595,.T.);
#38591=EDGE_CURVE('',#30062,#30060,#24596,.T.);
#38592=EDGE_CURVE('',#30063,#30064,#16683,.T.);
#38593=EDGE_CURVE('',#30063,#30061,#24597,.T.);
#38594=EDGE_CURVE('',#30064,#30062,#24598,.T.);
#38595=EDGE_CURVE('',#30065,#30066,#16684,.T.);
#38596=EDGE_CURVE('',#30065,#30063,#24599,.T.);
#38597=EDGE_CURVE('',#30066,#30064,#24600,.T.);
#38598=EDGE_CURVE('',#30067,#30068,#16685,.T.);
#38599=EDGE_CURVE('',#30067,#30065,#24601,.T.);
#38600=EDGE_CURVE('',#30068,#30066,#24602,.T.);
#38601=EDGE_CURVE('',#30069,#30070,#16686,.T.);
#38602=EDGE_CURVE('',#30069,#30067,#24603,.T.);
#38603=EDGE_CURVE('',#30070,#30068,#24604,.T.);
#38604=EDGE_CURVE('',#30071,#30072,#16687,.T.);
#38605=EDGE_CURVE('',#30071,#30069,#24605,.T.);
#38606=EDGE_CURVE('',#30072,#30070,#24606,.T.);
#38607=EDGE_CURVE('',#30073,#30074,#16688,.T.);
#38608=EDGE_CURVE('',#30073,#30071,#24607,.T.);
#38609=EDGE_CURVE('',#30074,#30072,#24608,.T.);
#38610=EDGE_CURVE('',#30075,#30076,#16689,.T.);
#38611=EDGE_CURVE('',#30075,#30073,#24609,.T.);
#38612=EDGE_CURVE('',#30076,#30074,#24610,.T.);
#38613=EDGE_CURVE('',#30077,#30078,#16690,.T.);
#38614=EDGE_CURVE('',#30077,#30075,#24611,.T.);
#38615=EDGE_CURVE('',#30078,#30076,#24612,.T.);
#38616=EDGE_CURVE('',#30079,#30080,#16691,.T.);
#38617=EDGE_CURVE('',#30079,#30077,#24613,.T.);
#38618=EDGE_CURVE('',#30080,#30078,#24614,.T.);
#38619=EDGE_CURVE('',#30057,#30081,#24615,.T.);
#38620=EDGE_CURVE('',#30082,#30081,#1432,.T.);
#38621=EDGE_CURVE('',#30083,#30082,#1433,.T.);
#38622=EDGE_CURVE('',#30083,#30058,#24616,.T.);
#38623=EDGE_CURVE('',#30054,#30083,#24617,.T.);
#38624=EDGE_CURVE('',#30084,#30030,#24618,.T.);
#38625=EDGE_CURVE('',#30084,#30080,#24619,.T.);
#38626=EDGE_CURVE('',#30029,#30085,#1434,.T.);
#38627=EDGE_CURVE('',#30029,#30086,#24620,.T.);
#38628=EDGE_CURVE('',#30086,#30084,#1435,.T.);
#38629=EDGE_CURVE('',#30085,#30030,#1436,.T.);
#38630=EDGE_CURVE('',#30086,#30079,#24621,.T.);
#38631=EDGE_CURVE('',#30081,#30053,#24622,.T.);
#38632=EDGE_CURVE('',#30085,#30087,#1437,.T.);
#38633=EDGE_CURVE('',#30087,#30087,#1438,.T.);
#38634=EDGE_CURVE('',#30081,#30083,#1439,.T.);
#38635=EDGE_CURVE('',#30088,#30088,#1440,.T.);
#38636=EDGE_CURVE('',#30082,#30089,#16692,.T.);
#38637=EDGE_CURVE('',#30089,#30089,#1441,.T.);
#38638=EDGE_CURVE('',#30090,#30091,#431,.T.);
#38639=EDGE_CURVE('',#30090,#30092,#16693,.T.);
#38640=EDGE_CURVE('',#30092,#30093,#16694,.T.);
#38641=EDGE_CURVE('',#30091,#30093,#16695,.T.);
#38642=EDGE_CURVE('',#30093,#30094,#1442,.T.);
#38643=EDGE_CURVE('',#30094,#30092,#16696,.T.);
#38644=EDGE_CURVE('',#30095,#30090,#432,.T.);
#38645=EDGE_CURVE('',#30094,#30095,#16697,.T.);
#38646=EDGE_CURVE('',#30096,#30095,#1443,.T.);
#38647=EDGE_CURVE('',#30096,#30097,#16698,.T.);
#38648=EDGE_CURVE('',#30097,#30098,#1444,.T.);
#38649=EDGE_CURVE('',#30098,#30099,#16699,.T.);
#38650=EDGE_CURVE('',#30100,#30099,#1445,.T.);
#38651=EDGE_CURVE('',#30100,#30101,#16700,.T.);
#38652=EDGE_CURVE('',#30101,#30102,#1446,.T.);
#38653=EDGE_CURVE('',#30102,#30103,#16701,.T.);
#38654=EDGE_CURVE('',#30104,#30103,#1447,.T.);
#38655=EDGE_CURVE('',#30104,#30105,#16702,.T.);
#38656=EDGE_CURVE('',#30105,#30106,#1448,.T.);
#38657=EDGE_CURVE('',#30106,#30107,#16703,.T.);
#38658=EDGE_CURVE('',#30108,#30107,#1449,.T.);
#38659=EDGE_CURVE('',#30108,#30109,#16704,.T.);
#38660=EDGE_CURVE('',#30109,#30110,#1450,.T.);
#38661=EDGE_CURVE('',#30110,#30111,#16705,.T.);
#38662=EDGE_CURVE('',#30112,#30111,#1451,.T.);
#38663=EDGE_CURVE('',#30112,#30113,#16706,.T.);
#38664=EDGE_CURVE('',#30113,#30114,#1452,.T.);
#38665=EDGE_CURVE('',#30114,#30115,#16707,.T.);
#38666=EDGE_CURVE('',#30116,#30115,#1453,.T.);
#38667=EDGE_CURVE('',#30116,#30117,#16708,.T.);
#38668=EDGE_CURVE('',#30117,#30118,#1454,.T.);
#38669=EDGE_CURVE('',#30118,#30119,#16709,.T.);
#38670=EDGE_CURVE('',#30120,#30119,#1455,.T.);
#38671=EDGE_CURVE('',#30120,#30121,#16710,.T.);
#38672=EDGE_CURVE('',#30121,#30122,#1456,.T.);
#38673=EDGE_CURVE('',#30122,#30123,#16711,.T.);
#38674=EDGE_CURVE('',#30124,#30123,#1457,.T.);
#38675=EDGE_CURVE('',#30124,#30125,#16712,.T.);
#38676=EDGE_CURVE('',#30125,#30126,#1458,.T.);
#38677=EDGE_CURVE('',#30126,#30127,#16713,.T.);
#38678=EDGE_CURVE('',#30128,#30127,#1459,.T.);
#38679=EDGE_CURVE('',#30128,#30129,#16714,.T.);
#38680=EDGE_CURVE('',#30129,#30130,#1460,.T.);
#38681=EDGE_CURVE('',#30130,#30131,#16715,.T.);
#38682=EDGE_CURVE('',#30132,#30131,#1461,.T.);
#38683=EDGE_CURVE('',#30132,#30133,#16716,.T.);
#38684=EDGE_CURVE('',#30133,#30134,#1462,.T.);
#38685=EDGE_CURVE('',#30134,#30135,#16717,.T.);
#38686=EDGE_CURVE('',#30136,#30135,#1463,.T.);
#38687=EDGE_CURVE('',#30136,#30137,#16718,.T.);
#38688=EDGE_CURVE('',#30137,#30138,#1464,.T.);
#38689=EDGE_CURVE('',#30138,#30139,#16719,.T.);
#38690=EDGE_CURVE('',#30140,#30139,#1465,.T.);
#38691=EDGE_CURVE('',#30140,#30141,#16720,.T.);
#38692=EDGE_CURVE('',#30141,#30142,#1466,.T.);
#38693=EDGE_CURVE('',#30142,#30143,#16721,.T.);
#38694=EDGE_CURVE('',#30144,#30143,#1467,.T.);
#38695=EDGE_CURVE('',#30144,#30145,#16722,.T.);
#38696=EDGE_CURVE('',#30145,#30146,#1468,.T.);
#38697=EDGE_CURVE('',#30146,#30147,#16723,.T.);
#38698=EDGE_CURVE('',#30148,#30147,#1469,.T.);
#38699=EDGE_CURVE('',#30148,#30149,#16724,.T.);
#38700=EDGE_CURVE('',#30149,#30150,#1470,.T.);
#38701=EDGE_CURVE('',#30150,#30151,#16725,.T.);
#38702=EDGE_CURVE('',#30152,#30151,#1471,.T.);
#38703=EDGE_CURVE('',#30152,#30153,#16726,.T.);
#38704=EDGE_CURVE('',#30153,#30154,#1472,.T.);
#38705=EDGE_CURVE('',#30154,#30155,#16727,.T.);
#38706=EDGE_CURVE('',#30156,#30155,#1473,.T.);
#38707=EDGE_CURVE('',#30156,#30157,#16728,.T.);
#38708=EDGE_CURVE('',#30157,#30158,#1474,.T.);
#38709=EDGE_CURVE('',#30158,#30159,#16729,.T.);
#38710=EDGE_CURVE('',#30160,#30159,#1475,.T.);
#38711=EDGE_CURVE('',#30160,#30161,#16730,.T.);
#38712=EDGE_CURVE('',#30161,#30162,#1476,.T.);
#38713=EDGE_CURVE('',#30162,#30163,#16731,.T.);
#38714=EDGE_CURVE('',#30164,#30163,#1477,.T.);
#38715=EDGE_CURVE('',#30164,#30165,#16732,.T.);
#38716=EDGE_CURVE('',#30165,#30166,#1478,.T.);
#38717=EDGE_CURVE('',#30166,#30167,#16733,.T.);
#38718=EDGE_CURVE('',#30168,#30167,#1479,.T.);
#38719=EDGE_CURVE('',#30168,#30169,#16734,.T.);
#38720=EDGE_CURVE('',#30169,#30170,#1480,.T.);
#38721=EDGE_CURVE('',#30170,#30171,#16735,.T.);
#38722=EDGE_CURVE('',#30172,#30171,#1481,.T.);
#38723=EDGE_CURVE('',#30171,#30172,#1482,.T.);
#38724=EDGE_CURVE('',#30170,#30173,#1483,.T.);
#38725=EDGE_CURVE('',#30173,#30174,#16736,.T.);
#38726=EDGE_CURVE('',#30175,#30174,#1484,.T.);
#38727=EDGE_CURVE('',#30175,#30176,#16737,.T.);
#38728=EDGE_CURVE('',#30176,#30177,#1485,.T.);
#38729=EDGE_CURVE('',#30177,#30178,#16738,.T.);
#38730=EDGE_CURVE('',#30179,#30178,#1486,.T.);
#38731=EDGE_CURVE('',#30179,#30180,#16739,.T.);
#38732=EDGE_CURVE('',#30180,#30181,#1487,.T.);
#38733=EDGE_CURVE('',#30181,#30182,#16740,.T.);
#38734=EDGE_CURVE('',#30183,#30182,#1488,.T.);
#38735=EDGE_CURVE('',#30183,#30184,#16741,.T.);
#38736=EDGE_CURVE('',#30184,#30185,#1489,.T.);
#38737=EDGE_CURVE('',#30185,#30186,#16742,.T.);
#38738=EDGE_CURVE('',#30187,#30186,#1490,.T.);
#38739=EDGE_CURVE('',#30187,#30188,#16743,.T.);
#38740=EDGE_CURVE('',#30188,#30189,#1491,.T.);
#38741=EDGE_CURVE('',#30189,#30190,#16744,.T.);
#38742=EDGE_CURVE('',#30191,#30190,#1492,.T.);
#38743=EDGE_CURVE('',#30191,#30192,#16745,.T.);
#38744=EDGE_CURVE('',#30192,#30193,#1493,.T.);
#38745=EDGE_CURVE('',#30193,#30194,#16746,.T.);
#38746=EDGE_CURVE('',#30195,#30194,#1494,.T.);
#38747=EDGE_CURVE('',#30195,#30196,#16747,.T.);
#38748=EDGE_CURVE('',#30196,#30197,#1495,.T.);
#38749=EDGE_CURVE('',#30197,#30198,#16748,.T.);
#38750=EDGE_CURVE('',#30199,#30198,#1496,.T.);
#38751=EDGE_CURVE('',#30199,#30200,#16749,.T.);
#38752=EDGE_CURVE('',#30200,#30201,#1497,.T.);
#38753=EDGE_CURVE('',#30201,#30202,#16750,.T.);
#38754=EDGE_CURVE('',#30203,#30202,#1498,.T.);
#38755=EDGE_CURVE('',#30203,#30204,#16751,.T.);
#38756=EDGE_CURVE('',#30204,#30205,#1499,.T.);
#38757=EDGE_CURVE('',#30205,#30206,#16752,.T.);
#38758=EDGE_CURVE('',#30207,#30206,#1500,.T.);
#38759=EDGE_CURVE('',#30207,#30208,#16753,.T.);
#38760=EDGE_CURVE('',#30208,#30209,#1501,.T.);
#38761=EDGE_CURVE('',#30209,#30210,#16754,.T.);
#38762=EDGE_CURVE('',#30211,#30210,#1502,.T.);
#38763=EDGE_CURVE('',#30211,#30212,#16755,.T.);
#38764=EDGE_CURVE('',#30212,#30213,#1503,.T.);
#38765=EDGE_CURVE('',#30213,#30214,#16756,.T.);
#38766=EDGE_CURVE('',#30215,#30214,#1504,.T.);
#38767=EDGE_CURVE('',#30215,#30216,#16757,.T.);
#38768=EDGE_CURVE('',#30216,#30217,#1505,.T.);
#38769=EDGE_CURVE('',#30217,#30218,#16758,.T.);
#38770=EDGE_CURVE('',#30219,#30218,#1506,.T.);
#38771=EDGE_CURVE('',#30219,#30220,#16759,.T.);
#38772=EDGE_CURVE('',#30220,#30221,#1507,.T.);
#38773=EDGE_CURVE('',#30221,#30222,#16760,.T.);
#38774=EDGE_CURVE('',#30223,#30222,#1508,.T.);
#38775=EDGE_CURVE('',#30223,#30224,#16761,.T.);
#38776=EDGE_CURVE('',#30224,#30225,#1509,.T.);
#38777=EDGE_CURVE('',#30225,#30226,#16762,.T.);
#38778=EDGE_CURVE('',#30227,#30226,#1510,.T.);
#38779=EDGE_CURVE('',#30227,#30228,#16763,.T.);
#38780=EDGE_CURVE('',#30228,#30229,#1511,.T.);
#38781=EDGE_CURVE('',#30229,#30230,#16764,.T.);
#38782=EDGE_CURVE('',#30231,#30230,#1512,.T.);
#38783=EDGE_CURVE('',#30231,#30232,#16765,.T.);
#38784=EDGE_CURVE('',#30232,#30233,#1513,.T.);
#38785=EDGE_CURVE('',#30233,#30234,#16766,.T.);
#38786=EDGE_CURVE('',#30235,#30234,#1514,.T.);
#38787=EDGE_CURVE('',#30235,#30236,#16767,.T.);
#38788=EDGE_CURVE('',#30236,#30237,#1515,.T.);
#38789=EDGE_CURVE('',#30237,#30238,#16768,.T.);
#38790=EDGE_CURVE('',#30091,#30238,#1516,.T.);
#38791=EDGE_CURVE('',#30239,#30235,#433,.T.);
#38792=EDGE_CURVE('',#30239,#30240,#16769,.T.);
#38793=EDGE_CURVE('',#30240,#30236,#16770,.T.);
#38794=EDGE_CURVE('',#30237,#30240,#16771,.T.);
#38795=EDGE_CURVE('',#30238,#30239,#434,.T.);
#38796=EDGE_CURVE('',#30241,#30231,#435,.T.);
#38797=EDGE_CURVE('',#30241,#30242,#16772,.T.);
#38798=EDGE_CURVE('',#30242,#30232,#16773,.T.);
#38799=EDGE_CURVE('',#30233,#30242,#16774,.T.);
#38800=EDGE_CURVE('',#30234,#30241,#436,.T.);
#38801=EDGE_CURVE('',#30243,#30227,#437,.T.);
#38802=EDGE_CURVE('',#30243,#30244,#16775,.T.);
#38803=EDGE_CURVE('',#30244,#30228,#16776,.T.);
#38804=EDGE_CURVE('',#30229,#30244,#16777,.T.);
#38805=EDGE_CURVE('',#30230,#30243,#438,.T.);
#38806=EDGE_CURVE('',#30245,#30223,#439,.T.);
#38807=EDGE_CURVE('',#30245,#30246,#16778,.T.);
#38808=EDGE_CURVE('',#30246,#30224,#16779,.T.);
#38809=EDGE_CURVE('',#30225,#30246,#16780,.T.);
#38810=EDGE_CURVE('',#30226,#30245,#440,.T.);
#38811=EDGE_CURVE('',#30247,#30219,#441,.T.);
#38812=EDGE_CURVE('',#30247,#30248,#16781,.T.);
#38813=EDGE_CURVE('',#30248,#30220,#16782,.T.);
#38814=EDGE_CURVE('',#30221,#30248,#16783,.T.);
#38815=EDGE_CURVE('',#30222,#30247,#442,.T.);
#38816=EDGE_CURVE('',#30249,#30215,#443,.T.);
#38817=EDGE_CURVE('',#30249,#30250,#16784,.T.);
#38818=EDGE_CURVE('',#30250,#30216,#16785,.T.);
#38819=EDGE_CURVE('',#30217,#30250,#16786,.T.);
#38820=EDGE_CURVE('',#30218,#30249,#444,.T.);
#38821=EDGE_CURVE('',#30251,#30211,#445,.T.);
#38822=EDGE_CURVE('',#30251,#30252,#16787,.T.);
#38823=EDGE_CURVE('',#30252,#30212,#16788,.T.);
#38824=EDGE_CURVE('',#30213,#30252,#16789,.T.);
#38825=EDGE_CURVE('',#30214,#30251,#446,.T.);
#38826=EDGE_CURVE('',#30253,#30207,#447,.T.);
#38827=EDGE_CURVE('',#30253,#30254,#16790,.T.);
#38828=EDGE_CURVE('',#30254,#30208,#16791,.T.);
#38829=EDGE_CURVE('',#30209,#30254,#16792,.T.);
#38830=EDGE_CURVE('',#30210,#30253,#448,.T.);
#38831=EDGE_CURVE('',#30255,#30203,#449,.T.);
#38832=EDGE_CURVE('',#30255,#30256,#16793,.T.);
#38833=EDGE_CURVE('',#30256,#30204,#16794,.T.);
#38834=EDGE_CURVE('',#30205,#30256,#16795,.T.);
#38835=EDGE_CURVE('',#30206,#30255,#450,.T.);
#38836=EDGE_CURVE('',#30257,#30199,#451,.T.);
#38837=EDGE_CURVE('',#30257,#30258,#16796,.T.);
#38838=EDGE_CURVE('',#30258,#30200,#16797,.T.);
#38839=EDGE_CURVE('',#30201,#30258,#16798,.T.);
#38840=EDGE_CURVE('',#30202,#30257,#452,.T.);
#38841=EDGE_CURVE('',#30259,#30195,#453,.T.);
#38842=EDGE_CURVE('',#30259,#30260,#16799,.T.);
#38843=EDGE_CURVE('',#30260,#30196,#16800,.T.);
#38844=EDGE_CURVE('',#30197,#30260,#16801,.T.);
#38845=EDGE_CURVE('',#30198,#30259,#454,.T.);
#38846=EDGE_CURVE('',#30261,#30191,#455,.T.);
#38847=EDGE_CURVE('',#30261,#30262,#16802,.T.);
#38848=EDGE_CURVE('',#30262,#30192,#16803,.T.);
#38849=EDGE_CURVE('',#30193,#30262,#16804,.T.);
#38850=EDGE_CURVE('',#30194,#30261,#456,.T.);
#38851=EDGE_CURVE('',#30263,#30187,#457,.T.);
#38852=EDGE_CURVE('',#30263,#30264,#16805,.T.);
#38853=EDGE_CURVE('',#30264,#30188,#16806,.T.);
#38854=EDGE_CURVE('',#30189,#30264,#16807,.T.);
#38855=EDGE_CURVE('',#30190,#30263,#458,.T.);
#38856=EDGE_CURVE('',#30265,#30183,#459,.T.);
#38857=EDGE_CURVE('',#30265,#30266,#16808,.T.);
#38858=EDGE_CURVE('',#30266,#30184,#16809,.T.);
#38859=EDGE_CURVE('',#30185,#30266,#16810,.T.);
#38860=EDGE_CURVE('',#30186,#30265,#460,.T.);
#38861=EDGE_CURVE('',#30267,#30179,#461,.T.);
#38862=EDGE_CURVE('',#30267,#30268,#16811,.T.);
#38863=EDGE_CURVE('',#30268,#30180,#16812,.T.);
#38864=EDGE_CURVE('',#30181,#30268,#16813,.T.);
#38865=EDGE_CURVE('',#30182,#30267,#462,.T.);
#38866=EDGE_CURVE('',#30269,#30175,#463,.T.);
#38867=EDGE_CURVE('',#30269,#30270,#16814,.T.);
#38868=EDGE_CURVE('',#30270,#30176,#16815,.T.);
#38869=EDGE_CURVE('',#30177,#30270,#16816,.T.);
#38870=EDGE_CURVE('',#30178,#30269,#464,.T.);
#38871=EDGE_CURVE('',#30271,#30168,#465,.T.);
#38872=EDGE_CURVE('',#30271,#30272,#16817,.T.);
#38873=EDGE_CURVE('',#30272,#30169,#16818,.T.);
#38874=EDGE_CURVE('',#30173,#30272,#16819,.T.);
#38875=EDGE_CURVE('',#30174,#30271,#466,.T.);
#38876=EDGE_CURVE('',#30273,#30164,#467,.T.);
#38877=EDGE_CURVE('',#30273,#30274,#16820,.T.);
#38878=EDGE_CURVE('',#30274,#30165,#16821,.T.);
#38879=EDGE_CURVE('',#30166,#30274,#16822,.T.);
#38880=EDGE_CURVE('',#30167,#30273,#468,.T.);
#38881=EDGE_CURVE('',#30275,#30160,#469,.T.);
#38882=EDGE_CURVE('',#30275,#30276,#16823,.T.);
#38883=EDGE_CURVE('',#30276,#30161,#16824,.T.);
#38884=EDGE_CURVE('',#30162,#30276,#16825,.T.);
#38885=EDGE_CURVE('',#30163,#30275,#470,.T.);
#38886=EDGE_CURVE('',#30277,#30156,#471,.T.);
#38887=EDGE_CURVE('',#30277,#30278,#16826,.T.);
#38888=EDGE_CURVE('',#30278,#30157,#16827,.T.);
#38889=EDGE_CURVE('',#30158,#30278,#16828,.T.);
#38890=EDGE_CURVE('',#30159,#30277,#472,.T.);
#38891=EDGE_CURVE('',#30279,#30152,#473,.T.);
#38892=EDGE_CURVE('',#30279,#30280,#16829,.T.);
#38893=EDGE_CURVE('',#30280,#30153,#16830,.T.);
#38894=EDGE_CURVE('',#30154,#30280,#16831,.T.);
#38895=EDGE_CURVE('',#30155,#30279,#474,.T.);
#38896=EDGE_CURVE('',#30281,#30148,#475,.T.);
#38897=EDGE_CURVE('',#30281,#30282,#16832,.T.);
#38898=EDGE_CURVE('',#30282,#30149,#16833,.T.);
#38899=EDGE_CURVE('',#30150,#30282,#16834,.T.);
#38900=EDGE_CURVE('',#30151,#30281,#476,.T.);
#38901=EDGE_CURVE('',#30283,#30144,#477,.T.);
#38902=EDGE_CURVE('',#30283,#30284,#16835,.T.);
#38903=EDGE_CURVE('',#30284,#30145,#16836,.T.);
#38904=EDGE_CURVE('',#30146,#30284,#16837,.T.);
#38905=EDGE_CURVE('',#30147,#30283,#478,.T.);
#38906=EDGE_CURVE('',#30285,#30140,#479,.T.);
#38907=EDGE_CURVE('',#30285,#30286,#16838,.T.);
#38908=EDGE_CURVE('',#30286,#30141,#16839,.T.);
#38909=EDGE_CURVE('',#30142,#30286,#16840,.T.);
#38910=EDGE_CURVE('',#30143,#30285,#480,.T.);
#38911=EDGE_CURVE('',#30287,#30136,#481,.T.);
#38912=EDGE_CURVE('',#30287,#30288,#16841,.T.);
#38913=EDGE_CURVE('',#30288,#30137,#16842,.T.);
#38914=EDGE_CURVE('',#30138,#30288,#16843,.T.);
#38915=EDGE_CURVE('',#30139,#30287,#482,.T.);
#38916=EDGE_CURVE('',#30289,#30132,#483,.T.);
#38917=EDGE_CURVE('',#30289,#30290,#16844,.T.);
#38918=EDGE_CURVE('',#30290,#30133,#16845,.T.);
#38919=EDGE_CURVE('',#30134,#30290,#16846,.T.);
#38920=EDGE_CURVE('',#30135,#30289,#484,.T.);
#38921=EDGE_CURVE('',#30291,#30128,#485,.T.);
#38922=EDGE_CURVE('',#30291,#30292,#16847,.T.);
#38923=EDGE_CURVE('',#30292,#30129,#16848,.T.);
#38924=EDGE_CURVE('',#30130,#30292,#16849,.T.);
#38925=EDGE_CURVE('',#30131,#30291,#486,.T.);
#38926=EDGE_CURVE('',#30293,#30124,#487,.T.);
#38927=EDGE_CURVE('',#30293,#30294,#16850,.T.);
#38928=EDGE_CURVE('',#30294,#30125,#16851,.T.);
#38929=EDGE_CURVE('',#30126,#30294,#16852,.T.);
#38930=EDGE_CURVE('',#30127,#30293,#488,.T.);
#38931=EDGE_CURVE('',#30295,#30120,#489,.T.);
#38932=EDGE_CURVE('',#30295,#30296,#16853,.T.);
#38933=EDGE_CURVE('',#30296,#30121,#16854,.T.);
#38934=EDGE_CURVE('',#30122,#30296,#16855,.T.);
#38935=EDGE_CURVE('',#30123,#30295,#490,.T.);
#38936=EDGE_CURVE('',#30297,#30116,#491,.T.);
#38937=EDGE_CURVE('',#30297,#30298,#16856,.T.);
#38938=EDGE_CURVE('',#30298,#30117,#16857,.T.);
#38939=EDGE_CURVE('',#30118,#30298,#16858,.T.);
#38940=EDGE_CURVE('',#30119,#30297,#492,.T.);
#38941=EDGE_CURVE('',#30299,#30112,#493,.T.);
#38942=EDGE_CURVE('',#30299,#30300,#16859,.T.);
#38943=EDGE_CURVE('',#30300,#30113,#16860,.T.);
#38944=EDGE_CURVE('',#30114,#30300,#16861,.T.);
#38945=EDGE_CURVE('',#30115,#30299,#494,.T.);
#38946=EDGE_CURVE('',#30301,#30108,#495,.T.);
#38947=EDGE_CURVE('',#30301,#30302,#16862,.T.);
#38948=EDGE_CURVE('',#30302,#30109,#16863,.T.);
#38949=EDGE_CURVE('',#30110,#30302,#16864,.T.);
#38950=EDGE_CURVE('',#30111,#30301,#496,.T.);
#38951=EDGE_CURVE('',#30303,#30104,#497,.T.);
#38952=EDGE_CURVE('',#30303,#30304,#16865,.T.);
#38953=EDGE_CURVE('',#30304,#30105,#16866,.T.);
#38954=EDGE_CURVE('',#30106,#30304,#16867,.T.);
#38955=EDGE_CURVE('',#30107,#30303,#498,.T.);
#38956=EDGE_CURVE('',#30305,#30100,#499,.T.);
#38957=EDGE_CURVE('',#30305,#30306,#16868,.T.);
#38958=EDGE_CURVE('',#30306,#30101,#16869,.T.);
#38959=EDGE_CURVE('',#30102,#30306,#16870,.T.);
#38960=EDGE_CURVE('',#30103,#30305,#500,.T.);
#38961=EDGE_CURVE('',#30307,#30096,#501,.T.);
#38962=EDGE_CURVE('',#30307,#30308,#16871,.T.);
#38963=EDGE_CURVE('',#30308,#30097,#16872,.T.);
#38964=EDGE_CURVE('',#30098,#30308,#16873,.T.);
#38965=EDGE_CURVE('',#30099,#30307,#502,.T.);
#38966=EDGE_CURVE('',#30172,#30088,#1517,.T.);
#38967=EDGE_CURVE('',#30309,#30309,#1518,.T.);
#38968=EDGE_CURVE('',#30309,#30271,#16874,.T.);
#38969=EDGE_CURVE('',#30310,#30310,#1519,.T.);
#38970=EDGE_CURVE('',#30310,#30311,#16875,.T.);
#38971=EDGE_CURVE('',#30312,#30311,#503,.T.);
#38972=EDGE_CURVE('',#30312,#30313,#1520,.T.);
#38973=EDGE_CURVE('',#30314,#30313,#504,.T.);
#38974=EDGE_CURVE('',#30315,#30314,#505,.T.);
#38975=EDGE_CURVE('',#30315,#30316,#1521,.T.);
#38976=EDGE_CURVE('',#30317,#30316,#506,.T.);
#38977=EDGE_CURVE('',#30318,#30317,#507,.T.);
#38978=EDGE_CURVE('',#30318,#30319,#1522,.T.);
#38979=EDGE_CURVE('',#30320,#30319,#508,.T.);
#38980=EDGE_CURVE('',#30321,#30320,#509,.T.);
#38981=EDGE_CURVE('',#30321,#30322,#1523,.T.);
#38982=EDGE_CURVE('',#30323,#30322,#510,.T.);
#38983=EDGE_CURVE('',#30324,#30323,#511,.T.);
#38984=EDGE_CURVE('',#30324,#30325,#1524,.T.);
#38985=EDGE_CURVE('',#30326,#30325,#512,.T.);
#38986=EDGE_CURVE('',#30327,#30326,#513,.T.);
#38987=EDGE_CURVE('',#30327,#30328,#1525,.T.);
#38988=EDGE_CURVE('',#30311,#30328,#514,.T.);
#38989=EDGE_CURVE('',#30316,#30329,#16876,.T.);
#38990=EDGE_CURVE('',#30330,#30315,#16877,.T.);
#38991=EDGE_CURVE('',#30329,#30330,#1526,.T.);
#38992=EDGE_CURVE('',#30319,#30331,#16878,.T.);
#38993=EDGE_CURVE('',#30332,#30318,#16879,.T.);
#38994=EDGE_CURVE('',#30331,#30332,#1527,.T.);
#38995=EDGE_CURVE('',#30333,#30312,#16880,.T.);
#38996=EDGE_CURVE('',#30334,#30333,#1528,.T.);
#38997=EDGE_CURVE('',#30313,#30334,#16881,.T.);
#38998=EDGE_CURVE('',#30322,#30335,#16882,.T.);
#38999=EDGE_CURVE('',#30336,#30321,#16883,.T.);
#39000=EDGE_CURVE('',#30335,#30336,#1529,.T.);
#39001=EDGE_CURVE('',#30337,#30327,#16884,.T.);
#39002=EDGE_CURVE('',#30338,#30337,#1530,.T.);
#39003=EDGE_CURVE('',#30328,#30338,#16885,.T.);
#39004=EDGE_CURVE('',#30339,#30324,#16886,.T.);
#39005=EDGE_CURVE('',#30340,#30339,#1531,.T.);
#39006=EDGE_CURVE('',#30325,#30340,#16887,.T.);
#39007=EDGE_CURVE('',#30336,#30335,#16888,.T.);
#39008=EDGE_CURVE('',#30320,#30341,#16889,.T.);
#39009=EDGE_CURVE('',#30341,#30342,#16890,.T.);
#39010=EDGE_CURVE('',#30323,#30342,#16891,.T.);
#39011=EDGE_CURVE('',#30332,#30331,#16892,.T.);
#39012=EDGE_CURVE('',#30317,#30343,#16893,.T.);
#39013=EDGE_CURVE('',#30343,#30341,#16894,.T.);
#39014=EDGE_CURVE('',#30330,#30329,#16895,.T.);
#39015=EDGE_CURVE('',#30314,#30344,#16896,.T.);
#39016=EDGE_CURVE('',#30344,#30343,#16897,.T.);
#39017=EDGE_CURVE('',#30333,#30334,#16898,.T.);
#39018=EDGE_CURVE('',#30337,#30338,#16899,.T.);
#39019=EDGE_CURVE('',#30339,#30340,#16900,.T.);
#39020=EDGE_CURVE('',#30345,#30344,#16901,.T.);
#39021=EDGE_CURVE('',#30345,#30344,#1532,.T.);
#39022=EDGE_CURVE('',#30344,#30343,#1533,.T.);
#39023=EDGE_CURVE('',#30343,#30341,#1534,.T.);
#39024=EDGE_CURVE('',#30341,#30342,#1535,.T.);
#39025=EDGE_CURVE('',#30342,#30346,#16902,.T.);
#39026=EDGE_CURVE('',#30342,#30346,#1536,.T.);
#39027=EDGE_CURVE('',#30346,#30345,#16903,.T.);
#39028=EDGE_CURVE('',#30346,#30345,#1537,.T.);
#39029=EDGE_CURVE('',#30345,#30347,#16904,.T.);
#39030=EDGE_CURVE('',#30311,#30345,#16905,.T.);
#39031=EDGE_CURVE('',#30326,#30346,#16906,.T.);
#39032=EDGE_CURVE('',#30348,#30348,#1538,.T.);
#39033=EDGE_CURVE('',#30349,#30349,#1539,.T.);
#39034=EDGE_CURVE('',#30349,#30348,#16907,.T.);
#39035=EDGE_CURVE('',#30350,#30350,#1540,.T.);
#39036=EDGE_CURVE('',#30350,#30349,#16908,.T.);
#39037=EDGE_CURVE('',#30351,#30351,#1541,.T.);
#39038=EDGE_CURVE('',#30351,#30350,#16909,.T.);
#39039=ORIENTED_EDGE('',*,*,#30352,.F.);
#39040=ORIENTED_EDGE('',*,*,#30353,.T.);
#39041=ORIENTED_EDGE('',*,*,#30354,.T.);
#39042=ORIENTED_EDGE('',*,*,#30355,.F.);
#39043=ORIENTED_EDGE('',*,*,#30356,.F.);
#39044=ORIENTED_EDGE('',*,*,#30357,.T.);
#39045=ORIENTED_EDGE('',*,*,#30358,.T.);
#39046=ORIENTED_EDGE('',*,*,#30353,.F.);
#39047=ORIENTED_EDGE('',*,*,#30359,.F.);
#39048=ORIENTED_EDGE('',*,*,#30360,.T.);
#39049=ORIENTED_EDGE('',*,*,#30361,.T.);
#39050=ORIENTED_EDGE('',*,*,#30357,.F.);
#39051=ORIENTED_EDGE('',*,*,#30362,.F.);
#39052=ORIENTED_EDGE('',*,*,#30363,.T.);
#39053=ORIENTED_EDGE('',*,*,#30364,.T.);
#39054=ORIENTED_EDGE('',*,*,#30360,.F.);
#39055=ORIENTED_EDGE('',*,*,#30365,.F.);
#39056=ORIENTED_EDGE('',*,*,#30366,.T.);
#39057=ORIENTED_EDGE('',*,*,#30367,.T.);
#39058=ORIENTED_EDGE('',*,*,#30363,.F.);
#39059=ORIENTED_EDGE('',*,*,#30368,.F.);
#39060=ORIENTED_EDGE('',*,*,#30369,.T.);
#39061=ORIENTED_EDGE('',*,*,#30370,.T.);
#39062=ORIENTED_EDGE('',*,*,#30366,.F.);
#39063=ORIENTED_EDGE('',*,*,#30371,.F.);
#39064=ORIENTED_EDGE('',*,*,#30372,.T.);
#39065=ORIENTED_EDGE('',*,*,#30373,.T.);
#39066=ORIENTED_EDGE('',*,*,#30369,.F.);
#39067=ORIENTED_EDGE('',*,*,#30374,.F.);
#39068=ORIENTED_EDGE('',*,*,#30355,.T.);
#39069=ORIENTED_EDGE('',*,*,#30375,.T.);
#39070=ORIENTED_EDGE('',*,*,#30372,.F.);
#39071=ORIENTED_EDGE('',*,*,#30376,.F.);
#39072=ORIENTED_EDGE('',*,*,#30377,.T.);
#39073=ORIENTED_EDGE('',*,*,#30378,.T.);
#39074=ORIENTED_EDGE('',*,*,#30379,.F.);
#39075=ORIENTED_EDGE('',*,*,#30380,.F.);
#39076=ORIENTED_EDGE('',*,*,#30381,.T.);
#39077=ORIENTED_EDGE('',*,*,#30382,.T.);
#39078=ORIENTED_EDGE('',*,*,#30377,.F.);
#39079=ORIENTED_EDGE('',*,*,#30383,.F.);
#39080=ORIENTED_EDGE('',*,*,#30384,.T.);
#39081=ORIENTED_EDGE('',*,*,#30385,.T.);
#39082=ORIENTED_EDGE('',*,*,#30381,.F.);
#39083=ORIENTED_EDGE('',*,*,#30386,.F.);
#39084=ORIENTED_EDGE('',*,*,#30387,.T.);
#39085=ORIENTED_EDGE('',*,*,#30388,.T.);
#39086=ORIENTED_EDGE('',*,*,#30384,.F.);
#39087=ORIENTED_EDGE('',*,*,#30389,.F.);
#39088=ORIENTED_EDGE('',*,*,#30390,.T.);
#39089=ORIENTED_EDGE('',*,*,#30391,.T.);
#39090=ORIENTED_EDGE('',*,*,#30387,.F.);
#39091=ORIENTED_EDGE('',*,*,#30392,.F.);
#39092=ORIENTED_EDGE('',*,*,#30393,.T.);
#39093=ORIENTED_EDGE('',*,*,#30394,.T.);
#39094=ORIENTED_EDGE('',*,*,#30390,.F.);
#39095=ORIENTED_EDGE('',*,*,#30395,.F.);
#39096=ORIENTED_EDGE('',*,*,#30396,.T.);
#39097=ORIENTED_EDGE('',*,*,#30397,.T.);
#39098=ORIENTED_EDGE('',*,*,#30393,.F.);
#39099=ORIENTED_EDGE('',*,*,#30398,.F.);
#39100=ORIENTED_EDGE('',*,*,#30399,.T.);
#39101=ORIENTED_EDGE('',*,*,#30400,.T.);
#39102=ORIENTED_EDGE('',*,*,#30396,.F.);
#39103=ORIENTED_EDGE('',*,*,#30401,.F.);
#39104=ORIENTED_EDGE('',*,*,#30402,.T.);
#39105=ORIENTED_EDGE('',*,*,#30403,.T.);
#39106=ORIENTED_EDGE('',*,*,#30399,.F.);
#39107=ORIENTED_EDGE('',*,*,#30404,.F.);
#39108=ORIENTED_EDGE('',*,*,#30405,.T.);
#39109=ORIENTED_EDGE('',*,*,#30406,.T.);
#39110=ORIENTED_EDGE('',*,*,#30402,.F.);
#39111=ORIENTED_EDGE('',*,*,#30407,.F.);
#39112=ORIENTED_EDGE('',*,*,#30408,.T.);
#39113=ORIENTED_EDGE('',*,*,#30409,.T.);
#39114=ORIENTED_EDGE('',*,*,#30405,.F.);
#39115=ORIENTED_EDGE('',*,*,#30410,.F.);
#39116=ORIENTED_EDGE('',*,*,#30379,.T.);
#39117=ORIENTED_EDGE('',*,*,#30411,.T.);
#39118=ORIENTED_EDGE('',*,*,#30408,.F.);
#39119=ORIENTED_EDGE('',*,*,#30411,.F.);
#39120=ORIENTED_EDGE('',*,*,#30378,.F.);
#39121=ORIENTED_EDGE('',*,*,#30382,.F.);
#39122=ORIENTED_EDGE('',*,*,#30385,.F.);
#39123=ORIENTED_EDGE('',*,*,#30388,.F.);
#39124=ORIENTED_EDGE('',*,*,#30391,.F.);
#39125=ORIENTED_EDGE('',*,*,#30394,.F.);
#39126=ORIENTED_EDGE('',*,*,#30397,.F.);
#39127=ORIENTED_EDGE('',*,*,#30400,.F.);
#39128=ORIENTED_EDGE('',*,*,#30403,.F.);
#39129=ORIENTED_EDGE('',*,*,#30406,.F.);
#39130=ORIENTED_EDGE('',*,*,#30409,.F.);
#39131=ORIENTED_EDGE('',*,*,#30375,.F.);
#39132=ORIENTED_EDGE('',*,*,#30354,.F.);
#39133=ORIENTED_EDGE('',*,*,#30358,.F.);
#39134=ORIENTED_EDGE('',*,*,#30361,.F.);
#39135=ORIENTED_EDGE('',*,*,#30364,.F.);
#39136=ORIENTED_EDGE('',*,*,#30367,.F.);
#39137=ORIENTED_EDGE('',*,*,#30370,.F.);
#39138=ORIENTED_EDGE('',*,*,#30373,.F.);
#39139=ORIENTED_EDGE('',*,*,#30412,.F.);
#39140=ORIENTED_EDGE('',*,*,#30413,.T.);
#39141=ORIENTED_EDGE('',*,*,#30414,.T.);
#39142=ORIENTED_EDGE('',*,*,#30415,.F.);
#39143=ORIENTED_EDGE('',*,*,#30416,.F.);
#39144=ORIENTED_EDGE('',*,*,#30417,.T.);
#39145=ORIENTED_EDGE('',*,*,#30418,.T.);
#39146=ORIENTED_EDGE('',*,*,#30413,.F.);
#39147=ORIENTED_EDGE('',*,*,#30419,.F.);
#39148=ORIENTED_EDGE('',*,*,#30420,.T.);
#39149=ORIENTED_EDGE('',*,*,#30421,.T.);
#39150=ORIENTED_EDGE('',*,*,#30417,.F.);
#39151=ORIENTED_EDGE('',*,*,#30422,.F.);
#39152=ORIENTED_EDGE('',*,*,#30423,.T.);
#39153=ORIENTED_EDGE('',*,*,#30424,.T.);
#39154=ORIENTED_EDGE('',*,*,#30420,.F.);
#39155=ORIENTED_EDGE('',*,*,#30425,.F.);
#39156=ORIENTED_EDGE('',*,*,#30426,.T.);
#39157=ORIENTED_EDGE('',*,*,#30427,.T.);
#39158=ORIENTED_EDGE('',*,*,#30423,.F.);
#39159=ORIENTED_EDGE('',*,*,#30428,.F.);
#39160=ORIENTED_EDGE('',*,*,#30429,.T.);
#39161=ORIENTED_EDGE('',*,*,#30430,.T.);
#39162=ORIENTED_EDGE('',*,*,#30426,.F.);
#39163=ORIENTED_EDGE('',*,*,#30431,.F.);
#39164=ORIENTED_EDGE('',*,*,#30432,.T.);
#39165=ORIENTED_EDGE('',*,*,#30433,.T.);
#39166=ORIENTED_EDGE('',*,*,#30429,.F.);
#39167=ORIENTED_EDGE('',*,*,#30434,.F.);
#39168=ORIENTED_EDGE('',*,*,#30415,.T.);
#39169=ORIENTED_EDGE('',*,*,#30435,.T.);
#39170=ORIENTED_EDGE('',*,*,#30432,.F.);
#39171=ORIENTED_EDGE('',*,*,#30436,.F.);
#39172=ORIENTED_EDGE('',*,*,#30437,.T.);
#39173=ORIENTED_EDGE('',*,*,#30438,.T.);
#39174=ORIENTED_EDGE('',*,*,#30439,.F.);
#39175=ORIENTED_EDGE('',*,*,#30440,.F.);
#39176=ORIENTED_EDGE('',*,*,#30441,.T.);
#39177=ORIENTED_EDGE('',*,*,#30442,.T.);
#39178=ORIENTED_EDGE('',*,*,#30437,.F.);
#39179=ORIENTED_EDGE('',*,*,#30443,.F.);
#39180=ORIENTED_EDGE('',*,*,#30444,.T.);
#39181=ORIENTED_EDGE('',*,*,#30445,.T.);
#39182=ORIENTED_EDGE('',*,*,#30441,.F.);
#39183=ORIENTED_EDGE('',*,*,#30446,.F.);
#39184=ORIENTED_EDGE('',*,*,#30447,.T.);
#39185=ORIENTED_EDGE('',*,*,#30448,.T.);
#39186=ORIENTED_EDGE('',*,*,#30444,.F.);
#39187=ORIENTED_EDGE('',*,*,#30449,.F.);
#39188=ORIENTED_EDGE('',*,*,#30450,.T.);
#39189=ORIENTED_EDGE('',*,*,#30451,.T.);
#39190=ORIENTED_EDGE('',*,*,#30447,.F.);
#39191=ORIENTED_EDGE('',*,*,#30452,.F.);
#39192=ORIENTED_EDGE('',*,*,#30453,.T.);
#39193=ORIENTED_EDGE('',*,*,#30454,.T.);
#39194=ORIENTED_EDGE('',*,*,#30450,.F.);
#39195=ORIENTED_EDGE('',*,*,#30455,.F.);
#39196=ORIENTED_EDGE('',*,*,#30456,.T.);
#39197=ORIENTED_EDGE('',*,*,#30457,.T.);
#39198=ORIENTED_EDGE('',*,*,#30453,.F.);
#39199=ORIENTED_EDGE('',*,*,#30458,.F.);
#39200=ORIENTED_EDGE('',*,*,#30459,.T.);
#39201=ORIENTED_EDGE('',*,*,#30460,.T.);
#39202=ORIENTED_EDGE('',*,*,#30456,.F.);
#39203=ORIENTED_EDGE('',*,*,#30461,.F.);
#39204=ORIENTED_EDGE('',*,*,#30462,.T.);
#39205=ORIENTED_EDGE('',*,*,#30463,.T.);
#39206=ORIENTED_EDGE('',*,*,#30459,.F.);
#39207=ORIENTED_EDGE('',*,*,#30464,.F.);
#39208=ORIENTED_EDGE('',*,*,#30465,.T.);
#39209=ORIENTED_EDGE('',*,*,#30466,.T.);
#39210=ORIENTED_EDGE('',*,*,#30462,.F.);
#39211=ORIENTED_EDGE('',*,*,#30467,.F.);
#39212=ORIENTED_EDGE('',*,*,#30468,.T.);
#39213=ORIENTED_EDGE('',*,*,#30469,.T.);
#39214=ORIENTED_EDGE('',*,*,#30465,.F.);
#39215=ORIENTED_EDGE('',*,*,#30470,.F.);
#39216=ORIENTED_EDGE('',*,*,#30471,.T.);
#39217=ORIENTED_EDGE('',*,*,#30472,.T.);
#39218=ORIENTED_EDGE('',*,*,#30468,.F.);
#39219=ORIENTED_EDGE('',*,*,#30473,.F.);
#39220=ORIENTED_EDGE('',*,*,#30474,.T.);
#39221=ORIENTED_EDGE('',*,*,#30475,.T.);
#39222=ORIENTED_EDGE('',*,*,#30471,.F.);
#39223=ORIENTED_EDGE('',*,*,#30476,.F.);
#39224=ORIENTED_EDGE('',*,*,#30477,.T.);
#39225=ORIENTED_EDGE('',*,*,#30478,.T.);
#39226=ORIENTED_EDGE('',*,*,#30474,.F.);
#39227=ORIENTED_EDGE('',*,*,#30479,.F.);
#39228=ORIENTED_EDGE('',*,*,#30480,.T.);
#39229=ORIENTED_EDGE('',*,*,#30481,.T.);
#39230=ORIENTED_EDGE('',*,*,#30477,.F.);
#39231=ORIENTED_EDGE('',*,*,#30482,.F.);
#39232=ORIENTED_EDGE('',*,*,#30483,.T.);
#39233=ORIENTED_EDGE('',*,*,#30484,.T.);
#39234=ORIENTED_EDGE('',*,*,#30480,.F.);
#39235=ORIENTED_EDGE('',*,*,#30485,.F.);
#39236=ORIENTED_EDGE('',*,*,#30486,.T.);
#39237=ORIENTED_EDGE('',*,*,#30487,.T.);
#39238=ORIENTED_EDGE('',*,*,#30483,.F.);
#39239=ORIENTED_EDGE('',*,*,#30488,.F.);
#39240=ORIENTED_EDGE('',*,*,#30489,.T.);
#39241=ORIENTED_EDGE('',*,*,#30490,.T.);
#39242=ORIENTED_EDGE('',*,*,#30486,.F.);
#39243=ORIENTED_EDGE('',*,*,#30491,.F.);
#39244=ORIENTED_EDGE('',*,*,#30492,.T.);
#39245=ORIENTED_EDGE('',*,*,#30493,.T.);
#39246=ORIENTED_EDGE('',*,*,#30489,.F.);
#39247=ORIENTED_EDGE('',*,*,#30494,.F.);
#39248=ORIENTED_EDGE('',*,*,#30495,.T.);
#39249=ORIENTED_EDGE('',*,*,#30496,.T.);
#39250=ORIENTED_EDGE('',*,*,#30492,.F.);
#39251=ORIENTED_EDGE('',*,*,#30497,.F.);
#39252=ORIENTED_EDGE('',*,*,#30498,.T.);
#39253=ORIENTED_EDGE('',*,*,#30499,.T.);
#39254=ORIENTED_EDGE('',*,*,#30495,.F.);
#39255=ORIENTED_EDGE('',*,*,#30500,.F.);
#39256=ORIENTED_EDGE('',*,*,#30439,.T.);
#39257=ORIENTED_EDGE('',*,*,#30501,.T.);
#39258=ORIENTED_EDGE('',*,*,#30498,.F.);
#39259=ORIENTED_EDGE('',*,*,#30501,.F.);
#39260=ORIENTED_EDGE('',*,*,#30438,.F.);
#39261=ORIENTED_EDGE('',*,*,#30442,.F.);
#39262=ORIENTED_EDGE('',*,*,#30445,.F.);
#39263=ORIENTED_EDGE('',*,*,#30448,.F.);
#39264=ORIENTED_EDGE('',*,*,#30451,.F.);
#39265=ORIENTED_EDGE('',*,*,#30454,.F.);
#39266=ORIENTED_EDGE('',*,*,#30457,.F.);
#39267=ORIENTED_EDGE('',*,*,#30460,.F.);
#39268=ORIENTED_EDGE('',*,*,#30463,.F.);
#39269=ORIENTED_EDGE('',*,*,#30466,.F.);
#39270=ORIENTED_EDGE('',*,*,#30469,.F.);
#39271=ORIENTED_EDGE('',*,*,#30472,.F.);
#39272=ORIENTED_EDGE('',*,*,#30475,.F.);
#39273=ORIENTED_EDGE('',*,*,#30478,.F.);
#39274=ORIENTED_EDGE('',*,*,#30481,.F.);
#39275=ORIENTED_EDGE('',*,*,#30484,.F.);
#39276=ORIENTED_EDGE('',*,*,#30487,.F.);
#39277=ORIENTED_EDGE('',*,*,#30490,.F.);
#39278=ORIENTED_EDGE('',*,*,#30493,.F.);
#39279=ORIENTED_EDGE('',*,*,#30496,.F.);
#39280=ORIENTED_EDGE('',*,*,#30499,.F.);
#39281=ORIENTED_EDGE('',*,*,#30435,.F.);
#39282=ORIENTED_EDGE('',*,*,#30414,.F.);
#39283=ORIENTED_EDGE('',*,*,#30418,.F.);
#39284=ORIENTED_EDGE('',*,*,#30421,.F.);
#39285=ORIENTED_EDGE('',*,*,#30424,.F.);
#39286=ORIENTED_EDGE('',*,*,#30427,.F.);
#39287=ORIENTED_EDGE('',*,*,#30430,.F.);
#39288=ORIENTED_EDGE('',*,*,#30433,.F.);
#39289=ORIENTED_EDGE('',*,*,#30412,.T.);
#39290=ORIENTED_EDGE('',*,*,#30434,.T.);
#39291=ORIENTED_EDGE('',*,*,#30431,.T.);
#39292=ORIENTED_EDGE('',*,*,#30428,.T.);
#39293=ORIENTED_EDGE('',*,*,#30425,.T.);
#39294=ORIENTED_EDGE('',*,*,#30422,.T.);
#39295=ORIENTED_EDGE('',*,*,#30419,.T.);
#39296=ORIENTED_EDGE('',*,*,#30416,.T.);
#39297=ORIENTED_EDGE('',*,*,#30352,.T.);
#39298=ORIENTED_EDGE('',*,*,#30374,.T.);
#39299=ORIENTED_EDGE('',*,*,#30371,.T.);
#39300=ORIENTED_EDGE('',*,*,#30368,.T.);
#39301=ORIENTED_EDGE('',*,*,#30365,.T.);
#39302=ORIENTED_EDGE('',*,*,#30362,.T.);
#39303=ORIENTED_EDGE('',*,*,#30359,.T.);
#39304=ORIENTED_EDGE('',*,*,#30356,.T.);
#39305=ORIENTED_EDGE('',*,*,#30502,.F.);
#39306=ORIENTED_EDGE('',*,*,#30503,.T.);
#39307=ORIENTED_EDGE('',*,*,#30504,.T.);
#39308=ORIENTED_EDGE('',*,*,#30505,.F.);
#39309=ORIENTED_EDGE('',*,*,#30506,.F.);
#39310=ORIENTED_EDGE('',*,*,#30507,.T.);
#39311=ORIENTED_EDGE('',*,*,#30508,.T.);
#39312=ORIENTED_EDGE('',*,*,#30503,.F.);
#39313=ORIENTED_EDGE('',*,*,#30509,.F.);
#39314=ORIENTED_EDGE('',*,*,#30510,.T.);
#39315=ORIENTED_EDGE('',*,*,#30511,.T.);
#39316=ORIENTED_EDGE('',*,*,#30507,.F.);
#39317=ORIENTED_EDGE('',*,*,#30512,.F.);
#39318=ORIENTED_EDGE('',*,*,#30513,.T.);
#39319=ORIENTED_EDGE('',*,*,#30514,.T.);
#39320=ORIENTED_EDGE('',*,*,#30510,.F.);
#39321=ORIENTED_EDGE('',*,*,#30515,.F.);
#39322=ORIENTED_EDGE('',*,*,#30516,.T.);
#39323=ORIENTED_EDGE('',*,*,#30517,.T.);
#39324=ORIENTED_EDGE('',*,*,#30513,.F.);
#39325=ORIENTED_EDGE('',*,*,#30518,.F.);
#39326=ORIENTED_EDGE('',*,*,#30519,.T.);
#39327=ORIENTED_EDGE('',*,*,#30520,.T.);
#39328=ORIENTED_EDGE('',*,*,#30516,.F.);
#39329=ORIENTED_EDGE('',*,*,#30521,.F.);
#39330=ORIENTED_EDGE('',*,*,#30522,.T.);
#39331=ORIENTED_EDGE('',*,*,#30523,.T.);
#39332=ORIENTED_EDGE('',*,*,#30519,.F.);
#39333=ORIENTED_EDGE('',*,*,#30524,.F.);
#39334=ORIENTED_EDGE('',*,*,#30505,.T.);
#39335=ORIENTED_EDGE('',*,*,#30525,.T.);
#39336=ORIENTED_EDGE('',*,*,#30522,.F.);
#39337=ORIENTED_EDGE('',*,*,#30526,.F.);
#39338=ORIENTED_EDGE('',*,*,#30527,.T.);
#39339=ORIENTED_EDGE('',*,*,#30528,.T.);
#39340=ORIENTED_EDGE('',*,*,#30529,.F.);
#39341=ORIENTED_EDGE('',*,*,#30530,.F.);
#39342=ORIENTED_EDGE('',*,*,#30531,.T.);
#39343=ORIENTED_EDGE('',*,*,#30532,.T.);
#39344=ORIENTED_EDGE('',*,*,#30527,.F.);
#39345=ORIENTED_EDGE('',*,*,#30533,.F.);
#39346=ORIENTED_EDGE('',*,*,#30534,.T.);
#39347=ORIENTED_EDGE('',*,*,#30535,.T.);
#39348=ORIENTED_EDGE('',*,*,#30531,.F.);
#39349=ORIENTED_EDGE('',*,*,#30536,.F.);
#39350=ORIENTED_EDGE('',*,*,#30537,.T.);
#39351=ORIENTED_EDGE('',*,*,#30538,.T.);
#39352=ORIENTED_EDGE('',*,*,#30534,.F.);
#39353=ORIENTED_EDGE('',*,*,#30539,.F.);
#39354=ORIENTED_EDGE('',*,*,#30540,.T.);
#39355=ORIENTED_EDGE('',*,*,#30541,.T.);
#39356=ORIENTED_EDGE('',*,*,#30537,.F.);
#39357=ORIENTED_EDGE('',*,*,#30542,.F.);
#39358=ORIENTED_EDGE('',*,*,#30543,.T.);
#39359=ORIENTED_EDGE('',*,*,#30544,.T.);
#39360=ORIENTED_EDGE('',*,*,#30540,.F.);
#39361=ORIENTED_EDGE('',*,*,#30545,.F.);
#39362=ORIENTED_EDGE('',*,*,#30546,.T.);
#39363=ORIENTED_EDGE('',*,*,#30547,.T.);
#39364=ORIENTED_EDGE('',*,*,#30543,.F.);
#39365=ORIENTED_EDGE('',*,*,#30548,.F.);
#39366=ORIENTED_EDGE('',*,*,#30549,.T.);
#39367=ORIENTED_EDGE('',*,*,#30550,.T.);
#39368=ORIENTED_EDGE('',*,*,#30546,.F.);
#39369=ORIENTED_EDGE('',*,*,#30551,.F.);
#39370=ORIENTED_EDGE('',*,*,#30552,.T.);
#39371=ORIENTED_EDGE('',*,*,#30553,.T.);
#39372=ORIENTED_EDGE('',*,*,#30549,.F.);
#39373=ORIENTED_EDGE('',*,*,#30554,.F.);
#39374=ORIENTED_EDGE('',*,*,#30555,.T.);
#39375=ORIENTED_EDGE('',*,*,#30556,.T.);
#39376=ORIENTED_EDGE('',*,*,#30552,.F.);
#39377=ORIENTED_EDGE('',*,*,#30557,.F.);
#39378=ORIENTED_EDGE('',*,*,#30558,.T.);
#39379=ORIENTED_EDGE('',*,*,#30559,.T.);
#39380=ORIENTED_EDGE('',*,*,#30555,.F.);
#39381=ORIENTED_EDGE('',*,*,#30560,.F.);
#39382=ORIENTED_EDGE('',*,*,#30529,.T.);
#39383=ORIENTED_EDGE('',*,*,#30561,.T.);
#39384=ORIENTED_EDGE('',*,*,#30558,.F.);
#39385=ORIENTED_EDGE('',*,*,#30561,.F.);
#39386=ORIENTED_EDGE('',*,*,#30528,.F.);
#39387=ORIENTED_EDGE('',*,*,#30532,.F.);
#39388=ORIENTED_EDGE('',*,*,#30535,.F.);
#39389=ORIENTED_EDGE('',*,*,#30538,.F.);
#39390=ORIENTED_EDGE('',*,*,#30541,.F.);
#39391=ORIENTED_EDGE('',*,*,#30544,.F.);
#39392=ORIENTED_EDGE('',*,*,#30547,.F.);
#39393=ORIENTED_EDGE('',*,*,#30550,.F.);
#39394=ORIENTED_EDGE('',*,*,#30553,.F.);
#39395=ORIENTED_EDGE('',*,*,#30556,.F.);
#39396=ORIENTED_EDGE('',*,*,#30559,.F.);
#39397=ORIENTED_EDGE('',*,*,#30525,.F.);
#39398=ORIENTED_EDGE('',*,*,#30504,.F.);
#39399=ORIENTED_EDGE('',*,*,#30508,.F.);
#39400=ORIENTED_EDGE('',*,*,#30511,.F.);
#39401=ORIENTED_EDGE('',*,*,#30514,.F.);
#39402=ORIENTED_EDGE('',*,*,#30517,.F.);
#39403=ORIENTED_EDGE('',*,*,#30520,.F.);
#39404=ORIENTED_EDGE('',*,*,#30523,.F.);
#39405=ORIENTED_EDGE('',*,*,#30562,.F.);
#39406=ORIENTED_EDGE('',*,*,#30563,.T.);
#39407=ORIENTED_EDGE('',*,*,#30564,.T.);
#39408=ORIENTED_EDGE('',*,*,#30565,.F.);
#39409=ORIENTED_EDGE('',*,*,#30566,.F.);
#39410=ORIENTED_EDGE('',*,*,#30567,.T.);
#39411=ORIENTED_EDGE('',*,*,#30568,.T.);
#39412=ORIENTED_EDGE('',*,*,#30563,.F.);
#39413=ORIENTED_EDGE('',*,*,#30569,.F.);
#39414=ORIENTED_EDGE('',*,*,#30570,.T.);
#39415=ORIENTED_EDGE('',*,*,#30571,.T.);
#39416=ORIENTED_EDGE('',*,*,#30567,.F.);
#39417=ORIENTED_EDGE('',*,*,#30572,.F.);
#39418=ORIENTED_EDGE('',*,*,#30573,.T.);
#39419=ORIENTED_EDGE('',*,*,#30574,.T.);
#39420=ORIENTED_EDGE('',*,*,#30570,.F.);
#39421=ORIENTED_EDGE('',*,*,#30575,.F.);
#39422=ORIENTED_EDGE('',*,*,#30576,.T.);
#39423=ORIENTED_EDGE('',*,*,#30577,.T.);
#39424=ORIENTED_EDGE('',*,*,#30573,.F.);
#39425=ORIENTED_EDGE('',*,*,#30578,.F.);
#39426=ORIENTED_EDGE('',*,*,#30579,.T.);
#39427=ORIENTED_EDGE('',*,*,#30580,.T.);
#39428=ORIENTED_EDGE('',*,*,#30576,.F.);
#39429=ORIENTED_EDGE('',*,*,#30581,.F.);
#39430=ORIENTED_EDGE('',*,*,#30582,.T.);
#39431=ORIENTED_EDGE('',*,*,#30583,.T.);
#39432=ORIENTED_EDGE('',*,*,#30579,.F.);
#39433=ORIENTED_EDGE('',*,*,#30584,.F.);
#39434=ORIENTED_EDGE('',*,*,#30565,.T.);
#39435=ORIENTED_EDGE('',*,*,#30585,.T.);
#39436=ORIENTED_EDGE('',*,*,#30582,.F.);
#39437=ORIENTED_EDGE('',*,*,#30586,.F.);
#39438=ORIENTED_EDGE('',*,*,#30587,.T.);
#39439=ORIENTED_EDGE('',*,*,#30588,.T.);
#39440=ORIENTED_EDGE('',*,*,#30589,.F.);
#39441=ORIENTED_EDGE('',*,*,#30590,.F.);
#39442=ORIENTED_EDGE('',*,*,#30591,.T.);
#39443=ORIENTED_EDGE('',*,*,#30592,.T.);
#39444=ORIENTED_EDGE('',*,*,#30587,.F.);
#39445=ORIENTED_EDGE('',*,*,#30593,.F.);
#39446=ORIENTED_EDGE('',*,*,#30594,.T.);
#39447=ORIENTED_EDGE('',*,*,#30595,.T.);
#39448=ORIENTED_EDGE('',*,*,#30591,.F.);
#39449=ORIENTED_EDGE('',*,*,#30596,.F.);
#39450=ORIENTED_EDGE('',*,*,#30597,.T.);
#39451=ORIENTED_EDGE('',*,*,#30598,.T.);
#39452=ORIENTED_EDGE('',*,*,#30594,.F.);
#39453=ORIENTED_EDGE('',*,*,#30599,.F.);
#39454=ORIENTED_EDGE('',*,*,#30600,.T.);
#39455=ORIENTED_EDGE('',*,*,#30601,.T.);
#39456=ORIENTED_EDGE('',*,*,#30597,.F.);
#39457=ORIENTED_EDGE('',*,*,#30602,.F.);
#39458=ORIENTED_EDGE('',*,*,#30603,.T.);
#39459=ORIENTED_EDGE('',*,*,#30604,.T.);
#39460=ORIENTED_EDGE('',*,*,#30600,.F.);
#39461=ORIENTED_EDGE('',*,*,#30605,.F.);
#39462=ORIENTED_EDGE('',*,*,#30606,.T.);
#39463=ORIENTED_EDGE('',*,*,#30607,.T.);
#39464=ORIENTED_EDGE('',*,*,#30603,.F.);
#39465=ORIENTED_EDGE('',*,*,#30608,.F.);
#39466=ORIENTED_EDGE('',*,*,#30609,.T.);
#39467=ORIENTED_EDGE('',*,*,#30610,.T.);
#39468=ORIENTED_EDGE('',*,*,#30606,.F.);
#39469=ORIENTED_EDGE('',*,*,#30611,.F.);
#39470=ORIENTED_EDGE('',*,*,#30589,.T.);
#39471=ORIENTED_EDGE('',*,*,#30612,.T.);
#39472=ORIENTED_EDGE('',*,*,#30609,.F.);
#39473=ORIENTED_EDGE('',*,*,#30613,.F.);
#39474=ORIENTED_EDGE('',*,*,#30614,.T.);
#39475=ORIENTED_EDGE('',*,*,#30615,.T.);
#39476=ORIENTED_EDGE('',*,*,#30616,.F.);
#39477=ORIENTED_EDGE('',*,*,#30617,.F.);
#39478=ORIENTED_EDGE('',*,*,#30618,.T.);
#39479=ORIENTED_EDGE('',*,*,#30619,.T.);
#39480=ORIENTED_EDGE('',*,*,#30614,.F.);
#39481=ORIENTED_EDGE('',*,*,#30620,.F.);
#39482=ORIENTED_EDGE('',*,*,#30621,.T.);
#39483=ORIENTED_EDGE('',*,*,#30622,.T.);
#39484=ORIENTED_EDGE('',*,*,#30618,.F.);
#39485=ORIENTED_EDGE('',*,*,#30623,.F.);
#39486=ORIENTED_EDGE('',*,*,#30624,.T.);
#39487=ORIENTED_EDGE('',*,*,#30625,.T.);
#39488=ORIENTED_EDGE('',*,*,#30621,.F.);
#39489=ORIENTED_EDGE('',*,*,#30626,.F.);
#39490=ORIENTED_EDGE('',*,*,#30627,.T.);
#39491=ORIENTED_EDGE('',*,*,#30628,.T.);
#39492=ORIENTED_EDGE('',*,*,#30624,.F.);
#39493=ORIENTED_EDGE('',*,*,#30629,.F.);
#39494=ORIENTED_EDGE('',*,*,#30630,.T.);
#39495=ORIENTED_EDGE('',*,*,#30631,.T.);
#39496=ORIENTED_EDGE('',*,*,#30627,.F.);
#39497=ORIENTED_EDGE('',*,*,#30632,.F.);
#39498=ORIENTED_EDGE('',*,*,#30633,.T.);
#39499=ORIENTED_EDGE('',*,*,#30634,.T.);
#39500=ORIENTED_EDGE('',*,*,#30630,.F.);
#39501=ORIENTED_EDGE('',*,*,#30635,.F.);
#39502=ORIENTED_EDGE('',*,*,#30636,.T.);
#39503=ORIENTED_EDGE('',*,*,#30637,.T.);
#39504=ORIENTED_EDGE('',*,*,#30633,.F.);
#39505=ORIENTED_EDGE('',*,*,#30638,.F.);
#39506=ORIENTED_EDGE('',*,*,#30639,.T.);
#39507=ORIENTED_EDGE('',*,*,#30640,.T.);
#39508=ORIENTED_EDGE('',*,*,#30636,.F.);
#39509=ORIENTED_EDGE('',*,*,#30641,.F.);
#39510=ORIENTED_EDGE('',*,*,#30642,.T.);
#39511=ORIENTED_EDGE('',*,*,#30643,.T.);
#39512=ORIENTED_EDGE('',*,*,#30639,.F.);
#39513=ORIENTED_EDGE('',*,*,#30644,.F.);
#39514=ORIENTED_EDGE('',*,*,#30645,.T.);
#39515=ORIENTED_EDGE('',*,*,#30646,.T.);
#39516=ORIENTED_EDGE('',*,*,#30642,.F.);
#39517=ORIENTED_EDGE('',*,*,#30647,.F.);
#39518=ORIENTED_EDGE('',*,*,#30648,.T.);
#39519=ORIENTED_EDGE('',*,*,#30649,.T.);
#39520=ORIENTED_EDGE('',*,*,#30645,.F.);
#39521=ORIENTED_EDGE('',*,*,#30650,.F.);
#39522=ORIENTED_EDGE('',*,*,#30651,.T.);
#39523=ORIENTED_EDGE('',*,*,#30652,.T.);
#39524=ORIENTED_EDGE('',*,*,#30648,.F.);
#39525=ORIENTED_EDGE('',*,*,#30653,.F.);
#39526=ORIENTED_EDGE('',*,*,#30654,.T.);
#39527=ORIENTED_EDGE('',*,*,#30655,.T.);
#39528=ORIENTED_EDGE('',*,*,#30651,.F.);
#39529=ORIENTED_EDGE('',*,*,#30656,.F.);
#39530=ORIENTED_EDGE('',*,*,#30657,.T.);
#39531=ORIENTED_EDGE('',*,*,#30658,.T.);
#39532=ORIENTED_EDGE('',*,*,#30654,.F.);
#39533=ORIENTED_EDGE('',*,*,#30659,.F.);
#39534=ORIENTED_EDGE('',*,*,#30616,.T.);
#39535=ORIENTED_EDGE('',*,*,#30660,.T.);
#39536=ORIENTED_EDGE('',*,*,#30657,.F.);
#39537=ORIENTED_EDGE('',*,*,#30660,.F.);
#39538=ORIENTED_EDGE('',*,*,#30615,.F.);
#39539=ORIENTED_EDGE('',*,*,#30619,.F.);
#39540=ORIENTED_EDGE('',*,*,#30622,.F.);
#39541=ORIENTED_EDGE('',*,*,#30625,.F.);
#39542=ORIENTED_EDGE('',*,*,#30628,.F.);
#39543=ORIENTED_EDGE('',*,*,#30631,.F.);
#39544=ORIENTED_EDGE('',*,*,#30634,.F.);
#39545=ORIENTED_EDGE('',*,*,#30637,.F.);
#39546=ORIENTED_EDGE('',*,*,#30640,.F.);
#39547=ORIENTED_EDGE('',*,*,#30643,.F.);
#39548=ORIENTED_EDGE('',*,*,#30646,.F.);
#39549=ORIENTED_EDGE('',*,*,#30649,.F.);
#39550=ORIENTED_EDGE('',*,*,#30652,.F.);
#39551=ORIENTED_EDGE('',*,*,#30655,.F.);
#39552=ORIENTED_EDGE('',*,*,#30658,.F.);
#39553=ORIENTED_EDGE('',*,*,#30612,.F.);
#39554=ORIENTED_EDGE('',*,*,#30588,.F.);
#39555=ORIENTED_EDGE('',*,*,#30592,.F.);
#39556=ORIENTED_EDGE('',*,*,#30595,.F.);
#39557=ORIENTED_EDGE('',*,*,#30598,.F.);
#39558=ORIENTED_EDGE('',*,*,#30601,.F.);
#39559=ORIENTED_EDGE('',*,*,#30604,.F.);
#39560=ORIENTED_EDGE('',*,*,#30607,.F.);
#39561=ORIENTED_EDGE('',*,*,#30610,.F.);
#39562=ORIENTED_EDGE('',*,*,#30585,.F.);
#39563=ORIENTED_EDGE('',*,*,#30564,.F.);
#39564=ORIENTED_EDGE('',*,*,#30568,.F.);
#39565=ORIENTED_EDGE('',*,*,#30571,.F.);
#39566=ORIENTED_EDGE('',*,*,#30574,.F.);
#39567=ORIENTED_EDGE('',*,*,#30577,.F.);
#39568=ORIENTED_EDGE('',*,*,#30580,.F.);
#39569=ORIENTED_EDGE('',*,*,#30583,.F.);
#39570=ORIENTED_EDGE('',*,*,#30586,.T.);
#39571=ORIENTED_EDGE('',*,*,#30611,.T.);
#39572=ORIENTED_EDGE('',*,*,#30608,.T.);
#39573=ORIENTED_EDGE('',*,*,#30605,.T.);
#39574=ORIENTED_EDGE('',*,*,#30602,.T.);
#39575=ORIENTED_EDGE('',*,*,#30599,.T.);
#39576=ORIENTED_EDGE('',*,*,#30596,.T.);
#39577=ORIENTED_EDGE('',*,*,#30593,.T.);
#39578=ORIENTED_EDGE('',*,*,#30590,.T.);
#39579=ORIENTED_EDGE('',*,*,#30562,.T.);
#39580=ORIENTED_EDGE('',*,*,#30584,.T.);
#39581=ORIENTED_EDGE('',*,*,#30581,.T.);
#39582=ORIENTED_EDGE('',*,*,#30578,.T.);
#39583=ORIENTED_EDGE('',*,*,#30575,.T.);
#39584=ORIENTED_EDGE('',*,*,#30572,.T.);
#39585=ORIENTED_EDGE('',*,*,#30569,.T.);
#39586=ORIENTED_EDGE('',*,*,#30566,.T.);
#39587=ORIENTED_EDGE('',*,*,#30502,.T.);
#39588=ORIENTED_EDGE('',*,*,#30524,.T.);
#39589=ORIENTED_EDGE('',*,*,#30521,.T.);
#39590=ORIENTED_EDGE('',*,*,#30518,.T.);
#39591=ORIENTED_EDGE('',*,*,#30515,.T.);
#39592=ORIENTED_EDGE('',*,*,#30512,.T.);
#39593=ORIENTED_EDGE('',*,*,#30509,.T.);
#39594=ORIENTED_EDGE('',*,*,#30506,.T.);
#39595=ORIENTED_EDGE('',*,*,#30661,.F.);
#39596=ORIENTED_EDGE('',*,*,#30662,.T.);
#39597=ORIENTED_EDGE('',*,*,#30663,.T.);
#39598=ORIENTED_EDGE('',*,*,#30664,.F.);
#39599=ORIENTED_EDGE('',*,*,#30665,.F.);
#39600=ORIENTED_EDGE('',*,*,#30666,.T.);
#39601=ORIENTED_EDGE('',*,*,#30667,.T.);
#39602=ORIENTED_EDGE('',*,*,#30662,.F.);
#39603=ORIENTED_EDGE('',*,*,#30668,.F.);
#39604=ORIENTED_EDGE('',*,*,#30669,.T.);
#39605=ORIENTED_EDGE('',*,*,#30670,.T.);
#39606=ORIENTED_EDGE('',*,*,#30666,.F.);
#39607=ORIENTED_EDGE('',*,*,#30671,.F.);
#39608=ORIENTED_EDGE('',*,*,#30672,.T.);
#39609=ORIENTED_EDGE('',*,*,#30673,.T.);
#39610=ORIENTED_EDGE('',*,*,#30669,.F.);
#39611=ORIENTED_EDGE('',*,*,#30674,.F.);
#39612=ORIENTED_EDGE('',*,*,#30675,.T.);
#39613=ORIENTED_EDGE('',*,*,#30676,.T.);
#39614=ORIENTED_EDGE('',*,*,#30672,.F.);
#39615=ORIENTED_EDGE('',*,*,#30677,.F.);
#39616=ORIENTED_EDGE('',*,*,#30678,.T.);
#39617=ORIENTED_EDGE('',*,*,#30679,.T.);
#39618=ORIENTED_EDGE('',*,*,#30675,.F.);
#39619=ORIENTED_EDGE('',*,*,#30680,.F.);
#39620=ORIENTED_EDGE('',*,*,#30681,.T.);
#39621=ORIENTED_EDGE('',*,*,#30682,.T.);
#39622=ORIENTED_EDGE('',*,*,#30678,.F.);
#39623=ORIENTED_EDGE('',*,*,#30683,.F.);
#39624=ORIENTED_EDGE('',*,*,#30664,.T.);
#39625=ORIENTED_EDGE('',*,*,#30684,.T.);
#39626=ORIENTED_EDGE('',*,*,#30681,.F.);
#39627=ORIENTED_EDGE('',*,*,#30685,.F.);
#39628=ORIENTED_EDGE('',*,*,#30686,.T.);
#39629=ORIENTED_EDGE('',*,*,#30687,.T.);
#39630=ORIENTED_EDGE('',*,*,#30688,.F.);
#39631=ORIENTED_EDGE('',*,*,#30689,.F.);
#39632=ORIENTED_EDGE('',*,*,#30690,.T.);
#39633=ORIENTED_EDGE('',*,*,#30691,.T.);
#39634=ORIENTED_EDGE('',*,*,#30686,.F.);
#39635=ORIENTED_EDGE('',*,*,#30692,.F.);
#39636=ORIENTED_EDGE('',*,*,#30693,.T.);
#39637=ORIENTED_EDGE('',*,*,#30694,.T.);
#39638=ORIENTED_EDGE('',*,*,#30690,.F.);
#39639=ORIENTED_EDGE('',*,*,#30695,.F.);
#39640=ORIENTED_EDGE('',*,*,#30696,.T.);
#39641=ORIENTED_EDGE('',*,*,#30697,.T.);
#39642=ORIENTED_EDGE('',*,*,#30693,.F.);
#39643=ORIENTED_EDGE('',*,*,#30698,.F.);
#39644=ORIENTED_EDGE('',*,*,#30699,.T.);
#39645=ORIENTED_EDGE('',*,*,#30700,.T.);
#39646=ORIENTED_EDGE('',*,*,#30696,.F.);
#39647=ORIENTED_EDGE('',*,*,#30701,.F.);
#39648=ORIENTED_EDGE('',*,*,#30702,.T.);
#39649=ORIENTED_EDGE('',*,*,#30703,.T.);
#39650=ORIENTED_EDGE('',*,*,#30699,.F.);
#39651=ORIENTED_EDGE('',*,*,#30704,.F.);
#39652=ORIENTED_EDGE('',*,*,#30705,.T.);
#39653=ORIENTED_EDGE('',*,*,#30706,.T.);
#39654=ORIENTED_EDGE('',*,*,#30702,.F.);
#39655=ORIENTED_EDGE('',*,*,#30707,.F.);
#39656=ORIENTED_EDGE('',*,*,#30708,.T.);
#39657=ORIENTED_EDGE('',*,*,#30709,.T.);
#39658=ORIENTED_EDGE('',*,*,#30705,.F.);
#39659=ORIENTED_EDGE('',*,*,#30710,.F.);
#39660=ORIENTED_EDGE('',*,*,#30711,.T.);
#39661=ORIENTED_EDGE('',*,*,#30712,.T.);
#39662=ORIENTED_EDGE('',*,*,#30708,.F.);
#39663=ORIENTED_EDGE('',*,*,#30713,.F.);
#39664=ORIENTED_EDGE('',*,*,#30714,.T.);
#39665=ORIENTED_EDGE('',*,*,#30715,.T.);
#39666=ORIENTED_EDGE('',*,*,#30711,.F.);
#39667=ORIENTED_EDGE('',*,*,#30716,.F.);
#39668=ORIENTED_EDGE('',*,*,#30717,.T.);
#39669=ORIENTED_EDGE('',*,*,#30718,.T.);
#39670=ORIENTED_EDGE('',*,*,#30714,.F.);
#39671=ORIENTED_EDGE('',*,*,#30719,.F.);
#39672=ORIENTED_EDGE('',*,*,#30688,.T.);
#39673=ORIENTED_EDGE('',*,*,#30720,.T.);
#39674=ORIENTED_EDGE('',*,*,#30717,.F.);
#39675=ORIENTED_EDGE('',*,*,#30720,.F.);
#39676=ORIENTED_EDGE('',*,*,#30687,.F.);
#39677=ORIENTED_EDGE('',*,*,#30691,.F.);
#39678=ORIENTED_EDGE('',*,*,#30694,.F.);
#39679=ORIENTED_EDGE('',*,*,#30697,.F.);
#39680=ORIENTED_EDGE('',*,*,#30700,.F.);
#39681=ORIENTED_EDGE('',*,*,#30703,.F.);
#39682=ORIENTED_EDGE('',*,*,#30706,.F.);
#39683=ORIENTED_EDGE('',*,*,#30709,.F.);
#39684=ORIENTED_EDGE('',*,*,#30712,.F.);
#39685=ORIENTED_EDGE('',*,*,#30715,.F.);
#39686=ORIENTED_EDGE('',*,*,#30718,.F.);
#39687=ORIENTED_EDGE('',*,*,#30684,.F.);
#39688=ORIENTED_EDGE('',*,*,#30663,.F.);
#39689=ORIENTED_EDGE('',*,*,#30667,.F.);
#39690=ORIENTED_EDGE('',*,*,#30670,.F.);
#39691=ORIENTED_EDGE('',*,*,#30673,.F.);
#39692=ORIENTED_EDGE('',*,*,#30676,.F.);
#39693=ORIENTED_EDGE('',*,*,#30679,.F.);
#39694=ORIENTED_EDGE('',*,*,#30682,.F.);
#39695=ORIENTED_EDGE('',*,*,#30721,.F.);
#39696=ORIENTED_EDGE('',*,*,#30722,.T.);
#39697=ORIENTED_EDGE('',*,*,#30723,.T.);
#39698=ORIENTED_EDGE('',*,*,#30724,.F.);
#39699=ORIENTED_EDGE('',*,*,#30725,.F.);
#39700=ORIENTED_EDGE('',*,*,#30726,.T.);
#39701=ORIENTED_EDGE('',*,*,#30727,.T.);
#39702=ORIENTED_EDGE('',*,*,#30722,.F.);
#39703=ORIENTED_EDGE('',*,*,#30728,.F.);
#39704=ORIENTED_EDGE('',*,*,#30729,.T.);
#39705=ORIENTED_EDGE('',*,*,#30730,.T.);
#39706=ORIENTED_EDGE('',*,*,#30726,.F.);
#39707=ORIENTED_EDGE('',*,*,#30731,.F.);
#39708=ORIENTED_EDGE('',*,*,#30732,.T.);
#39709=ORIENTED_EDGE('',*,*,#30733,.T.);
#39710=ORIENTED_EDGE('',*,*,#30729,.F.);
#39711=ORIENTED_EDGE('',*,*,#30734,.F.);
#39712=ORIENTED_EDGE('',*,*,#30735,.T.);
#39713=ORIENTED_EDGE('',*,*,#30736,.T.);
#39714=ORIENTED_EDGE('',*,*,#30732,.F.);
#39715=ORIENTED_EDGE('',*,*,#30737,.F.);
#39716=ORIENTED_EDGE('',*,*,#30738,.T.);
#39717=ORIENTED_EDGE('',*,*,#30739,.T.);
#39718=ORIENTED_EDGE('',*,*,#30735,.F.);
#39719=ORIENTED_EDGE('',*,*,#30740,.F.);
#39720=ORIENTED_EDGE('',*,*,#30741,.T.);
#39721=ORIENTED_EDGE('',*,*,#30742,.T.);
#39722=ORIENTED_EDGE('',*,*,#30738,.F.);
#39723=ORIENTED_EDGE('',*,*,#30743,.F.);
#39724=ORIENTED_EDGE('',*,*,#30744,.T.);
#39725=ORIENTED_EDGE('',*,*,#30745,.T.);
#39726=ORIENTED_EDGE('',*,*,#30741,.F.);
#39727=ORIENTED_EDGE('',*,*,#30746,.F.);
#39728=ORIENTED_EDGE('',*,*,#30747,.T.);
#39729=ORIENTED_EDGE('',*,*,#30748,.T.);
#39730=ORIENTED_EDGE('',*,*,#30744,.F.);
#39731=ORIENTED_EDGE('',*,*,#30749,.F.);
#39732=ORIENTED_EDGE('',*,*,#30750,.T.);
#39733=ORIENTED_EDGE('',*,*,#30751,.T.);
#39734=ORIENTED_EDGE('',*,*,#30747,.F.);
#39735=ORIENTED_EDGE('',*,*,#30752,.F.);
#39736=ORIENTED_EDGE('',*,*,#30724,.T.);
#39737=ORIENTED_EDGE('',*,*,#30753,.T.);
#39738=ORIENTED_EDGE('',*,*,#30750,.F.);
#39739=ORIENTED_EDGE('',*,*,#30753,.F.);
#39740=ORIENTED_EDGE('',*,*,#30723,.F.);
#39741=ORIENTED_EDGE('',*,*,#30727,.F.);
#39742=ORIENTED_EDGE('',*,*,#30730,.F.);
#39743=ORIENTED_EDGE('',*,*,#30733,.F.);
#39744=ORIENTED_EDGE('',*,*,#30736,.F.);
#39745=ORIENTED_EDGE('',*,*,#30739,.F.);
#39746=ORIENTED_EDGE('',*,*,#30742,.F.);
#39747=ORIENTED_EDGE('',*,*,#30745,.F.);
#39748=ORIENTED_EDGE('',*,*,#30748,.F.);
#39749=ORIENTED_EDGE('',*,*,#30751,.F.);
#39750=ORIENTED_EDGE('',*,*,#30661,.T.);
#39751=ORIENTED_EDGE('',*,*,#30683,.T.);
#39752=ORIENTED_EDGE('',*,*,#30680,.T.);
#39753=ORIENTED_EDGE('',*,*,#30677,.T.);
#39754=ORIENTED_EDGE('',*,*,#30674,.T.);
#39755=ORIENTED_EDGE('',*,*,#30671,.T.);
#39756=ORIENTED_EDGE('',*,*,#30668,.T.);
#39757=ORIENTED_EDGE('',*,*,#30665,.T.);
#39758=ORIENTED_EDGE('',*,*,#30754,.F.);
#39759=ORIENTED_EDGE('',*,*,#30755,.T.);
#39760=ORIENTED_EDGE('',*,*,#30756,.T.);
#39761=ORIENTED_EDGE('',*,*,#30757,.F.);
#39762=ORIENTED_EDGE('',*,*,#30758,.F.);
#39763=ORIENTED_EDGE('',*,*,#30759,.T.);
#39764=ORIENTED_EDGE('',*,*,#30760,.T.);
#39765=ORIENTED_EDGE('',*,*,#30755,.F.);
#39766=ORIENTED_EDGE('',*,*,#30761,.F.);
#39767=ORIENTED_EDGE('',*,*,#30762,.T.);
#39768=ORIENTED_EDGE('',*,*,#30763,.T.);
#39769=ORIENTED_EDGE('',*,*,#30759,.F.);
#39770=ORIENTED_EDGE('',*,*,#30764,.F.);
#39771=ORIENTED_EDGE('',*,*,#30765,.T.);
#39772=ORIENTED_EDGE('',*,*,#30766,.T.);
#39773=ORIENTED_EDGE('',*,*,#30762,.F.);
#39774=ORIENTED_EDGE('',*,*,#30767,.F.);
#39775=ORIENTED_EDGE('',*,*,#30768,.T.);
#39776=ORIENTED_EDGE('',*,*,#30769,.T.);
#39777=ORIENTED_EDGE('',*,*,#30765,.F.);
#39778=ORIENTED_EDGE('',*,*,#30770,.F.);
#39779=ORIENTED_EDGE('',*,*,#30771,.T.);
#39780=ORIENTED_EDGE('',*,*,#30772,.T.);
#39781=ORIENTED_EDGE('',*,*,#30768,.F.);
#39782=ORIENTED_EDGE('',*,*,#30773,.F.);
#39783=ORIENTED_EDGE('',*,*,#30774,.T.);
#39784=ORIENTED_EDGE('',*,*,#30775,.T.);
#39785=ORIENTED_EDGE('',*,*,#30771,.F.);
#39786=ORIENTED_EDGE('',*,*,#30776,.F.);
#39787=ORIENTED_EDGE('',*,*,#30757,.T.);
#39788=ORIENTED_EDGE('',*,*,#30777,.T.);
#39789=ORIENTED_EDGE('',*,*,#30774,.F.);
#39790=ORIENTED_EDGE('',*,*,#30778,.F.);
#39791=ORIENTED_EDGE('',*,*,#30779,.T.);
#39792=ORIENTED_EDGE('',*,*,#30780,.T.);
#39793=ORIENTED_EDGE('',*,*,#30781,.F.);
#39794=ORIENTED_EDGE('',*,*,#30782,.F.);
#39795=ORIENTED_EDGE('',*,*,#30783,.T.);
#39796=ORIENTED_EDGE('',*,*,#30784,.T.);
#39797=ORIENTED_EDGE('',*,*,#30779,.F.);
#39798=ORIENTED_EDGE('',*,*,#30785,.F.);
#39799=ORIENTED_EDGE('',*,*,#30786,.T.);
#39800=ORIENTED_EDGE('',*,*,#30787,.T.);
#39801=ORIENTED_EDGE('',*,*,#30783,.F.);
#39802=ORIENTED_EDGE('',*,*,#30788,.F.);
#39803=ORIENTED_EDGE('',*,*,#30789,.T.);
#39804=ORIENTED_EDGE('',*,*,#30790,.T.);
#39805=ORIENTED_EDGE('',*,*,#30786,.F.);
#39806=ORIENTED_EDGE('',*,*,#30791,.F.);
#39807=ORIENTED_EDGE('',*,*,#30792,.T.);
#39808=ORIENTED_EDGE('',*,*,#30793,.T.);
#39809=ORIENTED_EDGE('',*,*,#30789,.F.);
#39810=ORIENTED_EDGE('',*,*,#30794,.F.);
#39811=ORIENTED_EDGE('',*,*,#30795,.T.);
#39812=ORIENTED_EDGE('',*,*,#30796,.T.);
#39813=ORIENTED_EDGE('',*,*,#30792,.F.);
#39814=ORIENTED_EDGE('',*,*,#30797,.F.);
#39815=ORIENTED_EDGE('',*,*,#30798,.T.);
#39816=ORIENTED_EDGE('',*,*,#30799,.T.);
#39817=ORIENTED_EDGE('',*,*,#30795,.F.);
#39818=ORIENTED_EDGE('',*,*,#30800,.F.);
#39819=ORIENTED_EDGE('',*,*,#30801,.T.);
#39820=ORIENTED_EDGE('',*,*,#30802,.T.);
#39821=ORIENTED_EDGE('',*,*,#30798,.F.);
#39822=ORIENTED_EDGE('',*,*,#30803,.F.);
#39823=ORIENTED_EDGE('',*,*,#30804,.T.);
#39824=ORIENTED_EDGE('',*,*,#30805,.T.);
#39825=ORIENTED_EDGE('',*,*,#30801,.F.);
#39826=ORIENTED_EDGE('',*,*,#30806,.F.);
#39827=ORIENTED_EDGE('',*,*,#30807,.T.);
#39828=ORIENTED_EDGE('',*,*,#30808,.T.);
#39829=ORIENTED_EDGE('',*,*,#30804,.F.);
#39830=ORIENTED_EDGE('',*,*,#30809,.F.);
#39831=ORIENTED_EDGE('',*,*,#30810,.T.);
#39832=ORIENTED_EDGE('',*,*,#30811,.T.);
#39833=ORIENTED_EDGE('',*,*,#30807,.F.);
#39834=ORIENTED_EDGE('',*,*,#30812,.F.);
#39835=ORIENTED_EDGE('',*,*,#30781,.T.);
#39836=ORIENTED_EDGE('',*,*,#30813,.T.);
#39837=ORIENTED_EDGE('',*,*,#30810,.F.);
#39838=ORIENTED_EDGE('',*,*,#30813,.F.);
#39839=ORIENTED_EDGE('',*,*,#30780,.F.);
#39840=ORIENTED_EDGE('',*,*,#30784,.F.);
#39841=ORIENTED_EDGE('',*,*,#30787,.F.);
#39842=ORIENTED_EDGE('',*,*,#30790,.F.);
#39843=ORIENTED_EDGE('',*,*,#30793,.F.);
#39844=ORIENTED_EDGE('',*,*,#30796,.F.);
#39845=ORIENTED_EDGE('',*,*,#30799,.F.);
#39846=ORIENTED_EDGE('',*,*,#30802,.F.);
#39847=ORIENTED_EDGE('',*,*,#30805,.F.);
#39848=ORIENTED_EDGE('',*,*,#30808,.F.);
#39849=ORIENTED_EDGE('',*,*,#30811,.F.);
#39850=ORIENTED_EDGE('',*,*,#30777,.F.);
#39851=ORIENTED_EDGE('',*,*,#30756,.F.);
#39852=ORIENTED_EDGE('',*,*,#30760,.F.);
#39853=ORIENTED_EDGE('',*,*,#30763,.F.);
#39854=ORIENTED_EDGE('',*,*,#30766,.F.);
#39855=ORIENTED_EDGE('',*,*,#30769,.F.);
#39856=ORIENTED_EDGE('',*,*,#30772,.F.);
#39857=ORIENTED_EDGE('',*,*,#30775,.F.);
#39858=ORIENTED_EDGE('',*,*,#30814,.F.);
#39859=ORIENTED_EDGE('',*,*,#30815,.T.);
#39860=ORIENTED_EDGE('',*,*,#30816,.T.);
#39861=ORIENTED_EDGE('',*,*,#30817,.F.);
#39862=ORIENTED_EDGE('',*,*,#30818,.F.);
#39863=ORIENTED_EDGE('',*,*,#30819,.T.);
#39864=ORIENTED_EDGE('',*,*,#30820,.T.);
#39865=ORIENTED_EDGE('',*,*,#30815,.F.);
#39866=ORIENTED_EDGE('',*,*,#30821,.F.);
#39867=ORIENTED_EDGE('',*,*,#30822,.T.);
#39868=ORIENTED_EDGE('',*,*,#30823,.T.);
#39869=ORIENTED_EDGE('',*,*,#30819,.F.);
#39870=ORIENTED_EDGE('',*,*,#30824,.F.);
#39871=ORIENTED_EDGE('',*,*,#30825,.T.);
#39872=ORIENTED_EDGE('',*,*,#30826,.T.);
#39873=ORIENTED_EDGE('',*,*,#30822,.F.);
#39874=ORIENTED_EDGE('',*,*,#30827,.F.);
#39875=ORIENTED_EDGE('',*,*,#30828,.T.);
#39876=ORIENTED_EDGE('',*,*,#30829,.T.);
#39877=ORIENTED_EDGE('',*,*,#30825,.F.);
#39878=ORIENTED_EDGE('',*,*,#30830,.F.);
#39879=ORIENTED_EDGE('',*,*,#30831,.T.);
#39880=ORIENTED_EDGE('',*,*,#30832,.T.);
#39881=ORIENTED_EDGE('',*,*,#30828,.F.);
#39882=ORIENTED_EDGE('',*,*,#30833,.F.);
#39883=ORIENTED_EDGE('',*,*,#30834,.T.);
#39884=ORIENTED_EDGE('',*,*,#30835,.T.);
#39885=ORIENTED_EDGE('',*,*,#30831,.F.);
#39886=ORIENTED_EDGE('',*,*,#30836,.F.);
#39887=ORIENTED_EDGE('',*,*,#30837,.T.);
#39888=ORIENTED_EDGE('',*,*,#30838,.T.);
#39889=ORIENTED_EDGE('',*,*,#30834,.F.);
#39890=ORIENTED_EDGE('',*,*,#30839,.F.);
#39891=ORIENTED_EDGE('',*,*,#30817,.T.);
#39892=ORIENTED_EDGE('',*,*,#30840,.T.);
#39893=ORIENTED_EDGE('',*,*,#30837,.F.);
#39894=ORIENTED_EDGE('',*,*,#30841,.F.);
#39895=ORIENTED_EDGE('',*,*,#30842,.T.);
#39896=ORIENTED_EDGE('',*,*,#30843,.T.);
#39897=ORIENTED_EDGE('',*,*,#30844,.F.);
#39898=ORIENTED_EDGE('',*,*,#30845,.F.);
#39899=ORIENTED_EDGE('',*,*,#30846,.T.);
#39900=ORIENTED_EDGE('',*,*,#30847,.T.);
#39901=ORIENTED_EDGE('',*,*,#30842,.F.);
#39902=ORIENTED_EDGE('',*,*,#30848,.F.);
#39903=ORIENTED_EDGE('',*,*,#30849,.T.);
#39904=ORIENTED_EDGE('',*,*,#30850,.T.);
#39905=ORIENTED_EDGE('',*,*,#30846,.F.);
#39906=ORIENTED_EDGE('',*,*,#30851,.F.);
#39907=ORIENTED_EDGE('',*,*,#30852,.T.);
#39908=ORIENTED_EDGE('',*,*,#30853,.T.);
#39909=ORIENTED_EDGE('',*,*,#30849,.F.);
#39910=ORIENTED_EDGE('',*,*,#30854,.F.);
#39911=ORIENTED_EDGE('',*,*,#30855,.T.);
#39912=ORIENTED_EDGE('',*,*,#30856,.T.);
#39913=ORIENTED_EDGE('',*,*,#30852,.F.);
#39914=ORIENTED_EDGE('',*,*,#30857,.F.);
#39915=ORIENTED_EDGE('',*,*,#30858,.T.);
#39916=ORIENTED_EDGE('',*,*,#30859,.T.);
#39917=ORIENTED_EDGE('',*,*,#30855,.F.);
#39918=ORIENTED_EDGE('',*,*,#30860,.F.);
#39919=ORIENTED_EDGE('',*,*,#30861,.T.);
#39920=ORIENTED_EDGE('',*,*,#30862,.T.);
#39921=ORIENTED_EDGE('',*,*,#30858,.F.);
#39922=ORIENTED_EDGE('',*,*,#30863,.F.);
#39923=ORIENTED_EDGE('',*,*,#30864,.T.);
#39924=ORIENTED_EDGE('',*,*,#30865,.T.);
#39925=ORIENTED_EDGE('',*,*,#30861,.F.);
#39926=ORIENTED_EDGE('',*,*,#30866,.F.);
#39927=ORIENTED_EDGE('',*,*,#30867,.T.);
#39928=ORIENTED_EDGE('',*,*,#30868,.T.);
#39929=ORIENTED_EDGE('',*,*,#30864,.F.);
#39930=ORIENTED_EDGE('',*,*,#30869,.F.);
#39931=ORIENTED_EDGE('',*,*,#30870,.T.);
#39932=ORIENTED_EDGE('',*,*,#30871,.T.);
#39933=ORIENTED_EDGE('',*,*,#30867,.F.);
#39934=ORIENTED_EDGE('',*,*,#30872,.F.);
#39935=ORIENTED_EDGE('',*,*,#30873,.T.);
#39936=ORIENTED_EDGE('',*,*,#30874,.T.);
#39937=ORIENTED_EDGE('',*,*,#30870,.F.);
#39938=ORIENTED_EDGE('',*,*,#30875,.F.);
#39939=ORIENTED_EDGE('',*,*,#30876,.T.);
#39940=ORIENTED_EDGE('',*,*,#30877,.T.);
#39941=ORIENTED_EDGE('',*,*,#30873,.F.);
#39942=ORIENTED_EDGE('',*,*,#30878,.F.);
#39943=ORIENTED_EDGE('',*,*,#30879,.T.);
#39944=ORIENTED_EDGE('',*,*,#30880,.T.);
#39945=ORIENTED_EDGE('',*,*,#30876,.F.);
#39946=ORIENTED_EDGE('',*,*,#30881,.F.);
#39947=ORIENTED_EDGE('',*,*,#30882,.T.);
#39948=ORIENTED_EDGE('',*,*,#30883,.T.);
#39949=ORIENTED_EDGE('',*,*,#30879,.F.);
#39950=ORIENTED_EDGE('',*,*,#30884,.F.);
#39951=ORIENTED_EDGE('',*,*,#30885,.T.);
#39952=ORIENTED_EDGE('',*,*,#30886,.T.);
#39953=ORIENTED_EDGE('',*,*,#30882,.F.);
#39954=ORIENTED_EDGE('',*,*,#30887,.F.);
#39955=ORIENTED_EDGE('',*,*,#30888,.T.);
#39956=ORIENTED_EDGE('',*,*,#30889,.T.);
#39957=ORIENTED_EDGE('',*,*,#30885,.F.);
#39958=ORIENTED_EDGE('',*,*,#30890,.F.);
#39959=ORIENTED_EDGE('',*,*,#30891,.T.);
#39960=ORIENTED_EDGE('',*,*,#30892,.T.);
#39961=ORIENTED_EDGE('',*,*,#30888,.F.);
#39962=ORIENTED_EDGE('',*,*,#30893,.F.);
#39963=ORIENTED_EDGE('',*,*,#30894,.T.);
#39964=ORIENTED_EDGE('',*,*,#30895,.T.);
#39965=ORIENTED_EDGE('',*,*,#30891,.F.);
#39966=ORIENTED_EDGE('',*,*,#30896,.F.);
#39967=ORIENTED_EDGE('',*,*,#30844,.T.);
#39968=ORIENTED_EDGE('',*,*,#30897,.T.);
#39969=ORIENTED_EDGE('',*,*,#30894,.F.);
#39970=ORIENTED_EDGE('',*,*,#30897,.F.);
#39971=ORIENTED_EDGE('',*,*,#30843,.F.);
#39972=ORIENTED_EDGE('',*,*,#30847,.F.);
#39973=ORIENTED_EDGE('',*,*,#30850,.F.);
#39974=ORIENTED_EDGE('',*,*,#30853,.F.);
#39975=ORIENTED_EDGE('',*,*,#30856,.F.);
#39976=ORIENTED_EDGE('',*,*,#30859,.F.);
#39977=ORIENTED_EDGE('',*,*,#30862,.F.);
#39978=ORIENTED_EDGE('',*,*,#30865,.F.);
#39979=ORIENTED_EDGE('',*,*,#30868,.F.);
#39980=ORIENTED_EDGE('',*,*,#30871,.F.);
#39981=ORIENTED_EDGE('',*,*,#30874,.F.);
#39982=ORIENTED_EDGE('',*,*,#30877,.F.);
#39983=ORIENTED_EDGE('',*,*,#30880,.F.);
#39984=ORIENTED_EDGE('',*,*,#30883,.F.);
#39985=ORIENTED_EDGE('',*,*,#30886,.F.);
#39986=ORIENTED_EDGE('',*,*,#30889,.F.);
#39987=ORIENTED_EDGE('',*,*,#30892,.F.);
#39988=ORIENTED_EDGE('',*,*,#30895,.F.);
#39989=ORIENTED_EDGE('',*,*,#30840,.F.);
#39990=ORIENTED_EDGE('',*,*,#30816,.F.);
#39991=ORIENTED_EDGE('',*,*,#30820,.F.);
#39992=ORIENTED_EDGE('',*,*,#30823,.F.);
#39993=ORIENTED_EDGE('',*,*,#30826,.F.);
#39994=ORIENTED_EDGE('',*,*,#30829,.F.);
#39995=ORIENTED_EDGE('',*,*,#30832,.F.);
#39996=ORIENTED_EDGE('',*,*,#30835,.F.);
#39997=ORIENTED_EDGE('',*,*,#30838,.F.);
#39998=ORIENTED_EDGE('',*,*,#30814,.T.);
#39999=ORIENTED_EDGE('',*,*,#30839,.T.);
#40000=ORIENTED_EDGE('',*,*,#30836,.T.);
#40001=ORIENTED_EDGE('',*,*,#30833,.T.);
#40002=ORIENTED_EDGE('',*,*,#30830,.T.);
#40003=ORIENTED_EDGE('',*,*,#30827,.T.);
#40004=ORIENTED_EDGE('',*,*,#30824,.T.);
#40005=ORIENTED_EDGE('',*,*,#30821,.T.);
#40006=ORIENTED_EDGE('',*,*,#30818,.T.);
#40007=ORIENTED_EDGE('',*,*,#30754,.T.);
#40008=ORIENTED_EDGE('',*,*,#30776,.T.);
#40009=ORIENTED_EDGE('',*,*,#30773,.T.);
#40010=ORIENTED_EDGE('',*,*,#30770,.T.);
#40011=ORIENTED_EDGE('',*,*,#30767,.T.);
#40012=ORIENTED_EDGE('',*,*,#30764,.T.);
#40013=ORIENTED_EDGE('',*,*,#30761,.T.);
#40014=ORIENTED_EDGE('',*,*,#30758,.T.);
#40015=ORIENTED_EDGE('',*,*,#30898,.F.);
#40016=ORIENTED_EDGE('',*,*,#30899,.T.);
#40017=ORIENTED_EDGE('',*,*,#30900,.T.);
#40018=ORIENTED_EDGE('',*,*,#30901,.F.);
#40019=ORIENTED_EDGE('',*,*,#30902,.F.);
#40020=ORIENTED_EDGE('',*,*,#30903,.T.);
#40021=ORIENTED_EDGE('',*,*,#30904,.T.);
#40022=ORIENTED_EDGE('',*,*,#30899,.F.);
#40023=ORIENTED_EDGE('',*,*,#30905,.F.);
#40024=ORIENTED_EDGE('',*,*,#30906,.T.);
#40025=ORIENTED_EDGE('',*,*,#30907,.T.);
#40026=ORIENTED_EDGE('',*,*,#30903,.F.);
#40027=ORIENTED_EDGE('',*,*,#30908,.F.);
#40028=ORIENTED_EDGE('',*,*,#30909,.T.);
#40029=ORIENTED_EDGE('',*,*,#30910,.T.);
#40030=ORIENTED_EDGE('',*,*,#30906,.F.);
#40031=ORIENTED_EDGE('',*,*,#30911,.F.);
#40032=ORIENTED_EDGE('',*,*,#30912,.T.);
#40033=ORIENTED_EDGE('',*,*,#30913,.T.);
#40034=ORIENTED_EDGE('',*,*,#30909,.F.);
#40035=ORIENTED_EDGE('',*,*,#30914,.F.);
#40036=ORIENTED_EDGE('',*,*,#30915,.T.);
#40037=ORIENTED_EDGE('',*,*,#30916,.T.);
#40038=ORIENTED_EDGE('',*,*,#30912,.F.);
#40039=ORIENTED_EDGE('',*,*,#30917,.F.);
#40040=ORIENTED_EDGE('',*,*,#30918,.T.);
#40041=ORIENTED_EDGE('',*,*,#30919,.T.);
#40042=ORIENTED_EDGE('',*,*,#30915,.F.);
#40043=ORIENTED_EDGE('',*,*,#30920,.F.);
#40044=ORIENTED_EDGE('',*,*,#30901,.T.);
#40045=ORIENTED_EDGE('',*,*,#30921,.T.);
#40046=ORIENTED_EDGE('',*,*,#30918,.F.);
#40047=ORIENTED_EDGE('',*,*,#30922,.F.);
#40048=ORIENTED_EDGE('',*,*,#30923,.T.);
#40049=ORIENTED_EDGE('',*,*,#30924,.T.);
#40050=ORIENTED_EDGE('',*,*,#30925,.F.);
#40051=ORIENTED_EDGE('',*,*,#30926,.F.);
#40052=ORIENTED_EDGE('',*,*,#30927,.T.);
#40053=ORIENTED_EDGE('',*,*,#30928,.T.);
#40054=ORIENTED_EDGE('',*,*,#30923,.F.);
#40055=ORIENTED_EDGE('',*,*,#30929,.F.);
#40056=ORIENTED_EDGE('',*,*,#30930,.T.);
#40057=ORIENTED_EDGE('',*,*,#30931,.T.);
#40058=ORIENTED_EDGE('',*,*,#30927,.F.);
#40059=ORIENTED_EDGE('',*,*,#30932,.F.);
#40060=ORIENTED_EDGE('',*,*,#30933,.T.);
#40061=ORIENTED_EDGE('',*,*,#30934,.T.);
#40062=ORIENTED_EDGE('',*,*,#30930,.F.);
#40063=ORIENTED_EDGE('',*,*,#30935,.F.);
#40064=ORIENTED_EDGE('',*,*,#30936,.T.);
#40065=ORIENTED_EDGE('',*,*,#30937,.T.);
#40066=ORIENTED_EDGE('',*,*,#30933,.F.);
#40067=ORIENTED_EDGE('',*,*,#30938,.F.);
#40068=ORIENTED_EDGE('',*,*,#30939,.T.);
#40069=ORIENTED_EDGE('',*,*,#30940,.T.);
#40070=ORIENTED_EDGE('',*,*,#30936,.F.);
#40071=ORIENTED_EDGE('',*,*,#30941,.F.);
#40072=ORIENTED_EDGE('',*,*,#30942,.T.);
#40073=ORIENTED_EDGE('',*,*,#30943,.T.);
#40074=ORIENTED_EDGE('',*,*,#30939,.F.);
#40075=ORIENTED_EDGE('',*,*,#30944,.F.);
#40076=ORIENTED_EDGE('',*,*,#30945,.T.);
#40077=ORIENTED_EDGE('',*,*,#30946,.T.);
#40078=ORIENTED_EDGE('',*,*,#30942,.F.);
#40079=ORIENTED_EDGE('',*,*,#30947,.F.);
#40080=ORIENTED_EDGE('',*,*,#30948,.T.);
#40081=ORIENTED_EDGE('',*,*,#30949,.T.);
#40082=ORIENTED_EDGE('',*,*,#30945,.F.);
#40083=ORIENTED_EDGE('',*,*,#30950,.F.);
#40084=ORIENTED_EDGE('',*,*,#30951,.T.);
#40085=ORIENTED_EDGE('',*,*,#30952,.T.);
#40086=ORIENTED_EDGE('',*,*,#30948,.F.);
#40087=ORIENTED_EDGE('',*,*,#30953,.F.);
#40088=ORIENTED_EDGE('',*,*,#30954,.T.);
#40089=ORIENTED_EDGE('',*,*,#30955,.T.);
#40090=ORIENTED_EDGE('',*,*,#30951,.F.);
#40091=ORIENTED_EDGE('',*,*,#30956,.F.);
#40092=ORIENTED_EDGE('',*,*,#30925,.T.);
#40093=ORIENTED_EDGE('',*,*,#30957,.T.);
#40094=ORIENTED_EDGE('',*,*,#30954,.F.);
#40095=ORIENTED_EDGE('',*,*,#30957,.F.);
#40096=ORIENTED_EDGE('',*,*,#30924,.F.);
#40097=ORIENTED_EDGE('',*,*,#30928,.F.);
#40098=ORIENTED_EDGE('',*,*,#30931,.F.);
#40099=ORIENTED_EDGE('',*,*,#30934,.F.);
#40100=ORIENTED_EDGE('',*,*,#30937,.F.);
#40101=ORIENTED_EDGE('',*,*,#30940,.F.);
#40102=ORIENTED_EDGE('',*,*,#30943,.F.);
#40103=ORIENTED_EDGE('',*,*,#30946,.F.);
#40104=ORIENTED_EDGE('',*,*,#30949,.F.);
#40105=ORIENTED_EDGE('',*,*,#30952,.F.);
#40106=ORIENTED_EDGE('',*,*,#30955,.F.);
#40107=ORIENTED_EDGE('',*,*,#30921,.F.);
#40108=ORIENTED_EDGE('',*,*,#30900,.F.);
#40109=ORIENTED_EDGE('',*,*,#30904,.F.);
#40110=ORIENTED_EDGE('',*,*,#30907,.F.);
#40111=ORIENTED_EDGE('',*,*,#30910,.F.);
#40112=ORIENTED_EDGE('',*,*,#30913,.F.);
#40113=ORIENTED_EDGE('',*,*,#30916,.F.);
#40114=ORIENTED_EDGE('',*,*,#30919,.F.);
#40115=ORIENTED_EDGE('',*,*,#30958,.F.);
#40116=ORIENTED_EDGE('',*,*,#30959,.T.);
#40117=ORIENTED_EDGE('',*,*,#30960,.T.);
#40118=ORIENTED_EDGE('',*,*,#30961,.F.);
#40119=ORIENTED_EDGE('',*,*,#30962,.F.);
#40120=ORIENTED_EDGE('',*,*,#30963,.T.);
#40121=ORIENTED_EDGE('',*,*,#30964,.T.);
#40122=ORIENTED_EDGE('',*,*,#30959,.F.);
#40123=ORIENTED_EDGE('',*,*,#30965,.F.);
#40124=ORIENTED_EDGE('',*,*,#30966,.T.);
#40125=ORIENTED_EDGE('',*,*,#30967,.T.);
#40126=ORIENTED_EDGE('',*,*,#30963,.F.);
#40127=ORIENTED_EDGE('',*,*,#30968,.F.);
#40128=ORIENTED_EDGE('',*,*,#30969,.T.);
#40129=ORIENTED_EDGE('',*,*,#30970,.T.);
#40130=ORIENTED_EDGE('',*,*,#30966,.F.);
#40131=ORIENTED_EDGE('',*,*,#30971,.F.);
#40132=ORIENTED_EDGE('',*,*,#30972,.T.);
#40133=ORIENTED_EDGE('',*,*,#30973,.T.);
#40134=ORIENTED_EDGE('',*,*,#30969,.F.);
#40135=ORIENTED_EDGE('',*,*,#30974,.F.);
#40136=ORIENTED_EDGE('',*,*,#30975,.T.);
#40137=ORIENTED_EDGE('',*,*,#30976,.T.);
#40138=ORIENTED_EDGE('',*,*,#30972,.F.);
#40139=ORIENTED_EDGE('',*,*,#30977,.F.);
#40140=ORIENTED_EDGE('',*,*,#30978,.T.);
#40141=ORIENTED_EDGE('',*,*,#30979,.T.);
#40142=ORIENTED_EDGE('',*,*,#30975,.F.);
#40143=ORIENTED_EDGE('',*,*,#30980,.F.);
#40144=ORIENTED_EDGE('',*,*,#30981,.T.);
#40145=ORIENTED_EDGE('',*,*,#30982,.T.);
#40146=ORIENTED_EDGE('',*,*,#30978,.F.);
#40147=ORIENTED_EDGE('',*,*,#30983,.F.);
#40148=ORIENTED_EDGE('',*,*,#30984,.T.);
#40149=ORIENTED_EDGE('',*,*,#30985,.T.);
#40150=ORIENTED_EDGE('',*,*,#30981,.F.);
#40151=ORIENTED_EDGE('',*,*,#30986,.F.);
#40152=ORIENTED_EDGE('',*,*,#30987,.T.);
#40153=ORIENTED_EDGE('',*,*,#30988,.T.);
#40154=ORIENTED_EDGE('',*,*,#30984,.F.);
#40155=ORIENTED_EDGE('',*,*,#30989,.F.);
#40156=ORIENTED_EDGE('',*,*,#30990,.T.);
#40157=ORIENTED_EDGE('',*,*,#30991,.T.);
#40158=ORIENTED_EDGE('',*,*,#30987,.F.);
#40159=ORIENTED_EDGE('',*,*,#30992,.F.);
#40160=ORIENTED_EDGE('',*,*,#30993,.T.);
#40161=ORIENTED_EDGE('',*,*,#30994,.T.);
#40162=ORIENTED_EDGE('',*,*,#30990,.F.);
#40163=ORIENTED_EDGE('',*,*,#30995,.F.);
#40164=ORIENTED_EDGE('',*,*,#30996,.T.);
#40165=ORIENTED_EDGE('',*,*,#30997,.T.);
#40166=ORIENTED_EDGE('',*,*,#30993,.F.);
#40167=ORIENTED_EDGE('',*,*,#30998,.F.);
#40168=ORIENTED_EDGE('',*,*,#30999,.T.);
#40169=ORIENTED_EDGE('',*,*,#31000,.T.);
#40170=ORIENTED_EDGE('',*,*,#30996,.F.);
#40171=ORIENTED_EDGE('',*,*,#31001,.F.);
#40172=ORIENTED_EDGE('',*,*,#31002,.T.);
#40173=ORIENTED_EDGE('',*,*,#31003,.T.);
#40174=ORIENTED_EDGE('',*,*,#30999,.F.);
#40175=ORIENTED_EDGE('',*,*,#31004,.F.);
#40176=ORIENTED_EDGE('',*,*,#31005,.T.);
#40177=ORIENTED_EDGE('',*,*,#31006,.T.);
#40178=ORIENTED_EDGE('',*,*,#31002,.F.);
#40179=ORIENTED_EDGE('',*,*,#31007,.F.);
#40180=ORIENTED_EDGE('',*,*,#31008,.T.);
#40181=ORIENTED_EDGE('',*,*,#31009,.T.);
#40182=ORIENTED_EDGE('',*,*,#31005,.F.);
#40183=ORIENTED_EDGE('',*,*,#31010,.F.);
#40184=ORIENTED_EDGE('',*,*,#31011,.T.);
#40185=ORIENTED_EDGE('',*,*,#31012,.T.);
#40186=ORIENTED_EDGE('',*,*,#31008,.F.);
#40187=ORIENTED_EDGE('',*,*,#31013,.F.);
#40188=ORIENTED_EDGE('',*,*,#31014,.T.);
#40189=ORIENTED_EDGE('',*,*,#31015,.T.);
#40190=ORIENTED_EDGE('',*,*,#31011,.F.);
#40191=ORIENTED_EDGE('',*,*,#31016,.F.);
#40192=ORIENTED_EDGE('',*,*,#31017,.T.);
#40193=ORIENTED_EDGE('',*,*,#31018,.T.);
#40194=ORIENTED_EDGE('',*,*,#31014,.F.);
#40195=ORIENTED_EDGE('',*,*,#31019,.F.);
#40196=ORIENTED_EDGE('',*,*,#31020,.T.);
#40197=ORIENTED_EDGE('',*,*,#31021,.T.);
#40198=ORIENTED_EDGE('',*,*,#31017,.F.);
#40199=ORIENTED_EDGE('',*,*,#31022,.F.);
#40200=ORIENTED_EDGE('',*,*,#30961,.T.);
#40201=ORIENTED_EDGE('',*,*,#31023,.T.);
#40202=ORIENTED_EDGE('',*,*,#31020,.F.);
#40203=ORIENTED_EDGE('',*,*,#31023,.F.);
#40204=ORIENTED_EDGE('',*,*,#30960,.F.);
#40205=ORIENTED_EDGE('',*,*,#30964,.F.);
#40206=ORIENTED_EDGE('',*,*,#30967,.F.);
#40207=ORIENTED_EDGE('',*,*,#30970,.F.);
#40208=ORIENTED_EDGE('',*,*,#30973,.F.);
#40209=ORIENTED_EDGE('',*,*,#30976,.F.);
#40210=ORIENTED_EDGE('',*,*,#30979,.F.);
#40211=ORIENTED_EDGE('',*,*,#30982,.F.);
#40212=ORIENTED_EDGE('',*,*,#30985,.F.);
#40213=ORIENTED_EDGE('',*,*,#30988,.F.);
#40214=ORIENTED_EDGE('',*,*,#30991,.F.);
#40215=ORIENTED_EDGE('',*,*,#30994,.F.);
#40216=ORIENTED_EDGE('',*,*,#30997,.F.);
#40217=ORIENTED_EDGE('',*,*,#31000,.F.);
#40218=ORIENTED_EDGE('',*,*,#31003,.F.);
#40219=ORIENTED_EDGE('',*,*,#31006,.F.);
#40220=ORIENTED_EDGE('',*,*,#31009,.F.);
#40221=ORIENTED_EDGE('',*,*,#31012,.F.);
#40222=ORIENTED_EDGE('',*,*,#31015,.F.);
#40223=ORIENTED_EDGE('',*,*,#31018,.F.);
#40224=ORIENTED_EDGE('',*,*,#31021,.F.);
#40225=ORIENTED_EDGE('',*,*,#30898,.T.);
#40226=ORIENTED_EDGE('',*,*,#30920,.T.);
#40227=ORIENTED_EDGE('',*,*,#30917,.T.);
#40228=ORIENTED_EDGE('',*,*,#30914,.T.);
#40229=ORIENTED_EDGE('',*,*,#30911,.T.);
#40230=ORIENTED_EDGE('',*,*,#30908,.T.);
#40231=ORIENTED_EDGE('',*,*,#30905,.T.);
#40232=ORIENTED_EDGE('',*,*,#30902,.T.);
#40233=ORIENTED_EDGE('',*,*,#31024,.F.);
#40234=ORIENTED_EDGE('',*,*,#31025,.T.);
#40235=ORIENTED_EDGE('',*,*,#31026,.T.);
#40236=ORIENTED_EDGE('',*,*,#31027,.F.);
#40237=ORIENTED_EDGE('',*,*,#31028,.F.);
#40238=ORIENTED_EDGE('',*,*,#31029,.T.);
#40239=ORIENTED_EDGE('',*,*,#31030,.T.);
#40240=ORIENTED_EDGE('',*,*,#31025,.F.);
#40241=ORIENTED_EDGE('',*,*,#31031,.F.);
#40242=ORIENTED_EDGE('',*,*,#31032,.T.);
#40243=ORIENTED_EDGE('',*,*,#31033,.T.);
#40244=ORIENTED_EDGE('',*,*,#31029,.F.);
#40245=ORIENTED_EDGE('',*,*,#31034,.F.);
#40246=ORIENTED_EDGE('',*,*,#31035,.T.);
#40247=ORIENTED_EDGE('',*,*,#31036,.T.);
#40248=ORIENTED_EDGE('',*,*,#31032,.F.);
#40249=ORIENTED_EDGE('',*,*,#31037,.F.);
#40250=ORIENTED_EDGE('',*,*,#31038,.T.);
#40251=ORIENTED_EDGE('',*,*,#31039,.T.);
#40252=ORIENTED_EDGE('',*,*,#31035,.F.);
#40253=ORIENTED_EDGE('',*,*,#31040,.F.);
#40254=ORIENTED_EDGE('',*,*,#31041,.T.);
#40255=ORIENTED_EDGE('',*,*,#31042,.T.);
#40256=ORIENTED_EDGE('',*,*,#31038,.F.);
#40257=ORIENTED_EDGE('',*,*,#31043,.F.);
#40258=ORIENTED_EDGE('',*,*,#31044,.T.);
#40259=ORIENTED_EDGE('',*,*,#31045,.T.);
#40260=ORIENTED_EDGE('',*,*,#31041,.F.);
#40261=ORIENTED_EDGE('',*,*,#31046,.F.);
#40262=ORIENTED_EDGE('',*,*,#31027,.T.);
#40263=ORIENTED_EDGE('',*,*,#31047,.T.);
#40264=ORIENTED_EDGE('',*,*,#31044,.F.);
#40265=ORIENTED_EDGE('',*,*,#31048,.F.);
#40266=ORIENTED_EDGE('',*,*,#31049,.T.);
#40267=ORIENTED_EDGE('',*,*,#31050,.T.);
#40268=ORIENTED_EDGE('',*,*,#31051,.F.);
#40269=ORIENTED_EDGE('',*,*,#31052,.F.);
#40270=ORIENTED_EDGE('',*,*,#31053,.T.);
#40271=ORIENTED_EDGE('',*,*,#31054,.T.);
#40272=ORIENTED_EDGE('',*,*,#31049,.F.);
#40273=ORIENTED_EDGE('',*,*,#31055,.F.);
#40274=ORIENTED_EDGE('',*,*,#31056,.T.);
#40275=ORIENTED_EDGE('',*,*,#31057,.T.);
#40276=ORIENTED_EDGE('',*,*,#31053,.F.);
#40277=ORIENTED_EDGE('',*,*,#31058,.F.);
#40278=ORIENTED_EDGE('',*,*,#31059,.T.);
#40279=ORIENTED_EDGE('',*,*,#31060,.T.);
#40280=ORIENTED_EDGE('',*,*,#31056,.F.);
#40281=ORIENTED_EDGE('',*,*,#31061,.F.);
#40282=ORIENTED_EDGE('',*,*,#31062,.T.);
#40283=ORIENTED_EDGE('',*,*,#31063,.T.);
#40284=ORIENTED_EDGE('',*,*,#31059,.F.);
#40285=ORIENTED_EDGE('',*,*,#31064,.F.);
#40286=ORIENTED_EDGE('',*,*,#31065,.T.);
#40287=ORIENTED_EDGE('',*,*,#31066,.T.);
#40288=ORIENTED_EDGE('',*,*,#31062,.F.);
#40289=ORIENTED_EDGE('',*,*,#31067,.F.);
#40290=ORIENTED_EDGE('',*,*,#31068,.T.);
#40291=ORIENTED_EDGE('',*,*,#31069,.T.);
#40292=ORIENTED_EDGE('',*,*,#31065,.F.);
#40293=ORIENTED_EDGE('',*,*,#31070,.F.);
#40294=ORIENTED_EDGE('',*,*,#31071,.T.);
#40295=ORIENTED_EDGE('',*,*,#31072,.T.);
#40296=ORIENTED_EDGE('',*,*,#31068,.F.);
#40297=ORIENTED_EDGE('',*,*,#31073,.F.);
#40298=ORIENTED_EDGE('',*,*,#31074,.T.);
#40299=ORIENTED_EDGE('',*,*,#31075,.T.);
#40300=ORIENTED_EDGE('',*,*,#31071,.F.);
#40301=ORIENTED_EDGE('',*,*,#31076,.F.);
#40302=ORIENTED_EDGE('',*,*,#31077,.T.);
#40303=ORIENTED_EDGE('',*,*,#31078,.T.);
#40304=ORIENTED_EDGE('',*,*,#31074,.F.);
#40305=ORIENTED_EDGE('',*,*,#31079,.F.);
#40306=ORIENTED_EDGE('',*,*,#31080,.T.);
#40307=ORIENTED_EDGE('',*,*,#31081,.T.);
#40308=ORIENTED_EDGE('',*,*,#31077,.F.);
#40309=ORIENTED_EDGE('',*,*,#31082,.F.);
#40310=ORIENTED_EDGE('',*,*,#31051,.T.);
#40311=ORIENTED_EDGE('',*,*,#31083,.T.);
#40312=ORIENTED_EDGE('',*,*,#31080,.F.);
#40313=ORIENTED_EDGE('',*,*,#31083,.F.);
#40314=ORIENTED_EDGE('',*,*,#31050,.F.);
#40315=ORIENTED_EDGE('',*,*,#31054,.F.);
#40316=ORIENTED_EDGE('',*,*,#31057,.F.);
#40317=ORIENTED_EDGE('',*,*,#31060,.F.);
#40318=ORIENTED_EDGE('',*,*,#31063,.F.);
#40319=ORIENTED_EDGE('',*,*,#31066,.F.);
#40320=ORIENTED_EDGE('',*,*,#31069,.F.);
#40321=ORIENTED_EDGE('',*,*,#31072,.F.);
#40322=ORIENTED_EDGE('',*,*,#31075,.F.);
#40323=ORIENTED_EDGE('',*,*,#31078,.F.);
#40324=ORIENTED_EDGE('',*,*,#31081,.F.);
#40325=ORIENTED_EDGE('',*,*,#31047,.F.);
#40326=ORIENTED_EDGE('',*,*,#31026,.F.);
#40327=ORIENTED_EDGE('',*,*,#31030,.F.);
#40328=ORIENTED_EDGE('',*,*,#31033,.F.);
#40329=ORIENTED_EDGE('',*,*,#31036,.F.);
#40330=ORIENTED_EDGE('',*,*,#31039,.F.);
#40331=ORIENTED_EDGE('',*,*,#31042,.F.);
#40332=ORIENTED_EDGE('',*,*,#31045,.F.);
#40333=ORIENTED_EDGE('',*,*,#31084,.F.);
#40334=ORIENTED_EDGE('',*,*,#31085,.T.);
#40335=ORIENTED_EDGE('',*,*,#31086,.T.);
#40336=ORIENTED_EDGE('',*,*,#31087,.F.);
#40337=ORIENTED_EDGE('',*,*,#31088,.F.);
#40338=ORIENTED_EDGE('',*,*,#31089,.T.);
#40339=ORIENTED_EDGE('',*,*,#31090,.T.);
#40340=ORIENTED_EDGE('',*,*,#31085,.F.);
#40341=ORIENTED_EDGE('',*,*,#31091,.F.);
#40342=ORIENTED_EDGE('',*,*,#31087,.T.);
#40343=ORIENTED_EDGE('',*,*,#31092,.T.);
#40344=ORIENTED_EDGE('',*,*,#31089,.F.);
#40345=ORIENTED_EDGE('',*,*,#31093,.F.);
#40346=ORIENTED_EDGE('',*,*,#31094,.T.);
#40347=ORIENTED_EDGE('',*,*,#31095,.T.);
#40348=ORIENTED_EDGE('',*,*,#31096,.F.);
#40349=ORIENTED_EDGE('',*,*,#31097,.F.);
#40350=ORIENTED_EDGE('',*,*,#31098,.T.);
#40351=ORIENTED_EDGE('',*,*,#31099,.T.);
#40352=ORIENTED_EDGE('',*,*,#31094,.F.);
#40353=ORIENTED_EDGE('',*,*,#31100,.F.);
#40354=ORIENTED_EDGE('',*,*,#31101,.T.);
#40355=ORIENTED_EDGE('',*,*,#31102,.T.);
#40356=ORIENTED_EDGE('',*,*,#31098,.F.);
#40357=ORIENTED_EDGE('',*,*,#31103,.F.);
#40358=ORIENTED_EDGE('',*,*,#31104,.T.);
#40359=ORIENTED_EDGE('',*,*,#31105,.T.);
#40360=ORIENTED_EDGE('',*,*,#31101,.F.);
#40361=ORIENTED_EDGE('',*,*,#31106,.F.);
#40362=ORIENTED_EDGE('',*,*,#31107,.T.);
#40363=ORIENTED_EDGE('',*,*,#31108,.T.);
#40364=ORIENTED_EDGE('',*,*,#31104,.F.);
#40365=ORIENTED_EDGE('',*,*,#31109,.F.);
#40366=ORIENTED_EDGE('',*,*,#31110,.T.);
#40367=ORIENTED_EDGE('',*,*,#31111,.T.);
#40368=ORIENTED_EDGE('',*,*,#31107,.F.);
#40369=ORIENTED_EDGE('',*,*,#31112,.F.);
#40370=ORIENTED_EDGE('',*,*,#31113,.T.);
#40371=ORIENTED_EDGE('',*,*,#31114,.T.);
#40372=ORIENTED_EDGE('',*,*,#31110,.F.);
#40373=ORIENTED_EDGE('',*,*,#31115,.F.);
#40374=ORIENTED_EDGE('',*,*,#31116,.T.);
#40375=ORIENTED_EDGE('',*,*,#31117,.T.);
#40376=ORIENTED_EDGE('',*,*,#31113,.F.);
#40377=ORIENTED_EDGE('',*,*,#31118,.F.);
#40378=ORIENTED_EDGE('',*,*,#31119,.T.);
#40379=ORIENTED_EDGE('',*,*,#31120,.T.);
#40380=ORIENTED_EDGE('',*,*,#31116,.F.);
#40381=ORIENTED_EDGE('',*,*,#31121,.F.);
#40382=ORIENTED_EDGE('',*,*,#31122,.T.);
#40383=ORIENTED_EDGE('',*,*,#31123,.T.);
#40384=ORIENTED_EDGE('',*,*,#31119,.F.);
#40385=ORIENTED_EDGE('',*,*,#31124,.F.);
#40386=ORIENTED_EDGE('',*,*,#31096,.T.);
#40387=ORIENTED_EDGE('',*,*,#31125,.T.);
#40388=ORIENTED_EDGE('',*,*,#31122,.F.);
#40389=ORIENTED_EDGE('',*,*,#31125,.F.);
#40390=ORIENTED_EDGE('',*,*,#31095,.F.);
#40391=ORIENTED_EDGE('',*,*,#31099,.F.);
#40392=ORIENTED_EDGE('',*,*,#31102,.F.);
#40393=ORIENTED_EDGE('',*,*,#31105,.F.);
#40394=ORIENTED_EDGE('',*,*,#31108,.F.);
#40395=ORIENTED_EDGE('',*,*,#31111,.F.);
#40396=ORIENTED_EDGE('',*,*,#31114,.F.);
#40397=ORIENTED_EDGE('',*,*,#31117,.F.);
#40398=ORIENTED_EDGE('',*,*,#31120,.F.);
#40399=ORIENTED_EDGE('',*,*,#31123,.F.);
#40400=ORIENTED_EDGE('',*,*,#31092,.F.);
#40401=ORIENTED_EDGE('',*,*,#31086,.F.);
#40402=ORIENTED_EDGE('',*,*,#31090,.F.);
#40403=ORIENTED_EDGE('',*,*,#31084,.T.);
#40404=ORIENTED_EDGE('',*,*,#31091,.T.);
#40405=ORIENTED_EDGE('',*,*,#31088,.T.);
#40406=ORIENTED_EDGE('',*,*,#31024,.T.);
#40407=ORIENTED_EDGE('',*,*,#31046,.T.);
#40408=ORIENTED_EDGE('',*,*,#31043,.T.);
#40409=ORIENTED_EDGE('',*,*,#31040,.T.);
#40410=ORIENTED_EDGE('',*,*,#31037,.T.);
#40411=ORIENTED_EDGE('',*,*,#31034,.T.);
#40412=ORIENTED_EDGE('',*,*,#31031,.T.);
#40413=ORIENTED_EDGE('',*,*,#31028,.T.);
#40414=ORIENTED_EDGE('',*,*,#31126,.F.);
#40415=ORIENTED_EDGE('',*,*,#31127,.T.);
#40416=ORIENTED_EDGE('',*,*,#31128,.T.);
#40417=ORIENTED_EDGE('',*,*,#31129,.F.);
#40418=ORIENTED_EDGE('',*,*,#31130,.F.);
#40419=ORIENTED_EDGE('',*,*,#31131,.T.);
#40420=ORIENTED_EDGE('',*,*,#31132,.T.);
#40421=ORIENTED_EDGE('',*,*,#31127,.F.);
#40422=ORIENTED_EDGE('',*,*,#31133,.F.);
#40423=ORIENTED_EDGE('',*,*,#31134,.T.);
#40424=ORIENTED_EDGE('',*,*,#31135,.T.);
#40425=ORIENTED_EDGE('',*,*,#31131,.F.);
#40426=ORIENTED_EDGE('',*,*,#31136,.F.);
#40427=ORIENTED_EDGE('',*,*,#31137,.T.);
#40428=ORIENTED_EDGE('',*,*,#31138,.T.);
#40429=ORIENTED_EDGE('',*,*,#31134,.F.);
#40430=ORIENTED_EDGE('',*,*,#31139,.F.);
#40431=ORIENTED_EDGE('',*,*,#31140,.T.);
#40432=ORIENTED_EDGE('',*,*,#31141,.T.);
#40433=ORIENTED_EDGE('',*,*,#31137,.F.);
#40434=ORIENTED_EDGE('',*,*,#31142,.F.);
#40435=ORIENTED_EDGE('',*,*,#31143,.T.);
#40436=ORIENTED_EDGE('',*,*,#31144,.T.);
#40437=ORIENTED_EDGE('',*,*,#31140,.F.);
#40438=ORIENTED_EDGE('',*,*,#31145,.F.);
#40439=ORIENTED_EDGE('',*,*,#31146,.T.);
#40440=ORIENTED_EDGE('',*,*,#31147,.T.);
#40441=ORIENTED_EDGE('',*,*,#31143,.F.);
#40442=ORIENTED_EDGE('',*,*,#31148,.F.);
#40443=ORIENTED_EDGE('',*,*,#31129,.T.);
#40444=ORIENTED_EDGE('',*,*,#31149,.T.);
#40445=ORIENTED_EDGE('',*,*,#31146,.F.);
#40446=ORIENTED_EDGE('',*,*,#31150,.F.);
#40447=ORIENTED_EDGE('',*,*,#31151,.T.);
#40448=ORIENTED_EDGE('',*,*,#31152,.T.);
#40449=ORIENTED_EDGE('',*,*,#31153,.F.);
#40450=ORIENTED_EDGE('',*,*,#31154,.F.);
#40451=ORIENTED_EDGE('',*,*,#31155,.T.);
#40452=ORIENTED_EDGE('',*,*,#31156,.T.);
#40453=ORIENTED_EDGE('',*,*,#31151,.F.);
#40454=ORIENTED_EDGE('',*,*,#31157,.F.);
#40455=ORIENTED_EDGE('',*,*,#31158,.T.);
#40456=ORIENTED_EDGE('',*,*,#31159,.T.);
#40457=ORIENTED_EDGE('',*,*,#31155,.F.);
#40458=ORIENTED_EDGE('',*,*,#31160,.F.);
#40459=ORIENTED_EDGE('',*,*,#31161,.T.);
#40460=ORIENTED_EDGE('',*,*,#31162,.T.);
#40461=ORIENTED_EDGE('',*,*,#31158,.F.);
#40462=ORIENTED_EDGE('',*,*,#31163,.F.);
#40463=ORIENTED_EDGE('',*,*,#31164,.T.);
#40464=ORIENTED_EDGE('',*,*,#31165,.T.);
#40465=ORIENTED_EDGE('',*,*,#31161,.F.);
#40466=ORIENTED_EDGE('',*,*,#31166,.F.);
#40467=ORIENTED_EDGE('',*,*,#31167,.T.);
#40468=ORIENTED_EDGE('',*,*,#31168,.T.);
#40469=ORIENTED_EDGE('',*,*,#31164,.F.);
#40470=ORIENTED_EDGE('',*,*,#31169,.F.);
#40471=ORIENTED_EDGE('',*,*,#31170,.T.);
#40472=ORIENTED_EDGE('',*,*,#31171,.T.);
#40473=ORIENTED_EDGE('',*,*,#31167,.F.);
#40474=ORIENTED_EDGE('',*,*,#31172,.F.);
#40475=ORIENTED_EDGE('',*,*,#31173,.T.);
#40476=ORIENTED_EDGE('',*,*,#31174,.T.);
#40477=ORIENTED_EDGE('',*,*,#31170,.F.);
#40478=ORIENTED_EDGE('',*,*,#31175,.F.);
#40479=ORIENTED_EDGE('',*,*,#31176,.T.);
#40480=ORIENTED_EDGE('',*,*,#31177,.T.);
#40481=ORIENTED_EDGE('',*,*,#31173,.F.);
#40482=ORIENTED_EDGE('',*,*,#31178,.F.);
#40483=ORIENTED_EDGE('',*,*,#31179,.T.);
#40484=ORIENTED_EDGE('',*,*,#31180,.T.);
#40485=ORIENTED_EDGE('',*,*,#31176,.F.);
#40486=ORIENTED_EDGE('',*,*,#31181,.F.);
#40487=ORIENTED_EDGE('',*,*,#31182,.T.);
#40488=ORIENTED_EDGE('',*,*,#31183,.T.);
#40489=ORIENTED_EDGE('',*,*,#31179,.F.);
#40490=ORIENTED_EDGE('',*,*,#31184,.F.);
#40491=ORIENTED_EDGE('',*,*,#31153,.T.);
#40492=ORIENTED_EDGE('',*,*,#31185,.T.);
#40493=ORIENTED_EDGE('',*,*,#31182,.F.);
#40494=ORIENTED_EDGE('',*,*,#31185,.F.);
#40495=ORIENTED_EDGE('',*,*,#31152,.F.);
#40496=ORIENTED_EDGE('',*,*,#31156,.F.);
#40497=ORIENTED_EDGE('',*,*,#31159,.F.);
#40498=ORIENTED_EDGE('',*,*,#31162,.F.);
#40499=ORIENTED_EDGE('',*,*,#31165,.F.);
#40500=ORIENTED_EDGE('',*,*,#31168,.F.);
#40501=ORIENTED_EDGE('',*,*,#31171,.F.);
#40502=ORIENTED_EDGE('',*,*,#31174,.F.);
#40503=ORIENTED_EDGE('',*,*,#31177,.F.);
#40504=ORIENTED_EDGE('',*,*,#31180,.F.);
#40505=ORIENTED_EDGE('',*,*,#31183,.F.);
#40506=ORIENTED_EDGE('',*,*,#31149,.F.);
#40507=ORIENTED_EDGE('',*,*,#31128,.F.);
#40508=ORIENTED_EDGE('',*,*,#31132,.F.);
#40509=ORIENTED_EDGE('',*,*,#31135,.F.);
#40510=ORIENTED_EDGE('',*,*,#31138,.F.);
#40511=ORIENTED_EDGE('',*,*,#31141,.F.);
#40512=ORIENTED_EDGE('',*,*,#31144,.F.);
#40513=ORIENTED_EDGE('',*,*,#31147,.F.);
#40514=ORIENTED_EDGE('',*,*,#31186,.F.);
#40515=ORIENTED_EDGE('',*,*,#31187,.T.);
#40516=ORIENTED_EDGE('',*,*,#31188,.T.);
#40517=ORIENTED_EDGE('',*,*,#31189,.F.);
#40518=ORIENTED_EDGE('',*,*,#31190,.F.);
#40519=ORIENTED_EDGE('',*,*,#31191,.T.);
#40520=ORIENTED_EDGE('',*,*,#31192,.T.);
#40521=ORIENTED_EDGE('',*,*,#31187,.F.);
#40522=ORIENTED_EDGE('',*,*,#31193,.F.);
#40523=ORIENTED_EDGE('',*,*,#31194,.T.);
#40524=ORIENTED_EDGE('',*,*,#31195,.T.);
#40525=ORIENTED_EDGE('',*,*,#31191,.F.);
#40526=ORIENTED_EDGE('',*,*,#31196,.F.);
#40527=ORIENTED_EDGE('',*,*,#31197,.T.);
#40528=ORIENTED_EDGE('',*,*,#31198,.T.);
#40529=ORIENTED_EDGE('',*,*,#31194,.F.);
#40530=ORIENTED_EDGE('',*,*,#31199,.F.);
#40531=ORIENTED_EDGE('',*,*,#31200,.T.);
#40532=ORIENTED_EDGE('',*,*,#31201,.T.);
#40533=ORIENTED_EDGE('',*,*,#31197,.F.);
#40534=ORIENTED_EDGE('',*,*,#31202,.F.);
#40535=ORIENTED_EDGE('',*,*,#31203,.T.);
#40536=ORIENTED_EDGE('',*,*,#31204,.T.);
#40537=ORIENTED_EDGE('',*,*,#31200,.F.);
#40538=ORIENTED_EDGE('',*,*,#31205,.F.);
#40539=ORIENTED_EDGE('',*,*,#31206,.T.);
#40540=ORIENTED_EDGE('',*,*,#31207,.T.);
#40541=ORIENTED_EDGE('',*,*,#31203,.F.);
#40542=ORIENTED_EDGE('',*,*,#31208,.F.);
#40543=ORIENTED_EDGE('',*,*,#31209,.T.);
#40544=ORIENTED_EDGE('',*,*,#31210,.T.);
#40545=ORIENTED_EDGE('',*,*,#31206,.F.);
#40546=ORIENTED_EDGE('',*,*,#31211,.F.);
#40547=ORIENTED_EDGE('',*,*,#31212,.T.);
#40548=ORIENTED_EDGE('',*,*,#31213,.T.);
#40549=ORIENTED_EDGE('',*,*,#31209,.F.);
#40550=ORIENTED_EDGE('',*,*,#31214,.F.);
#40551=ORIENTED_EDGE('',*,*,#31215,.T.);
#40552=ORIENTED_EDGE('',*,*,#31216,.T.);
#40553=ORIENTED_EDGE('',*,*,#31212,.F.);
#40554=ORIENTED_EDGE('',*,*,#31217,.F.);
#40555=ORIENTED_EDGE('',*,*,#31218,.T.);
#40556=ORIENTED_EDGE('',*,*,#31219,.T.);
#40557=ORIENTED_EDGE('',*,*,#31215,.F.);
#40558=ORIENTED_EDGE('',*,*,#31220,.F.);
#40559=ORIENTED_EDGE('',*,*,#31221,.T.);
#40560=ORIENTED_EDGE('',*,*,#31222,.T.);
#40561=ORIENTED_EDGE('',*,*,#31218,.F.);
#40562=ORIENTED_EDGE('',*,*,#31223,.F.);
#40563=ORIENTED_EDGE('',*,*,#31224,.T.);
#40564=ORIENTED_EDGE('',*,*,#31225,.T.);
#40565=ORIENTED_EDGE('',*,*,#31221,.F.);
#40566=ORIENTED_EDGE('',*,*,#31226,.F.);
#40567=ORIENTED_EDGE('',*,*,#31227,.T.);
#40568=ORIENTED_EDGE('',*,*,#31228,.T.);
#40569=ORIENTED_EDGE('',*,*,#31224,.F.);
#40570=ORIENTED_EDGE('',*,*,#31229,.F.);
#40571=ORIENTED_EDGE('',*,*,#31230,.T.);
#40572=ORIENTED_EDGE('',*,*,#31231,.T.);
#40573=ORIENTED_EDGE('',*,*,#31227,.F.);
#40574=ORIENTED_EDGE('',*,*,#31232,.F.);
#40575=ORIENTED_EDGE('',*,*,#31233,.T.);
#40576=ORIENTED_EDGE('',*,*,#31234,.T.);
#40577=ORIENTED_EDGE('',*,*,#31230,.F.);
#40578=ORIENTED_EDGE('',*,*,#31235,.F.);
#40579=ORIENTED_EDGE('',*,*,#31236,.T.);
#40580=ORIENTED_EDGE('',*,*,#31237,.T.);
#40581=ORIENTED_EDGE('',*,*,#31233,.F.);
#40582=ORIENTED_EDGE('',*,*,#31238,.F.);
#40583=ORIENTED_EDGE('',*,*,#31239,.T.);
#40584=ORIENTED_EDGE('',*,*,#31240,.T.);
#40585=ORIENTED_EDGE('',*,*,#31236,.F.);
#40586=ORIENTED_EDGE('',*,*,#31241,.F.);
#40587=ORIENTED_EDGE('',*,*,#31242,.T.);
#40588=ORIENTED_EDGE('',*,*,#31243,.T.);
#40589=ORIENTED_EDGE('',*,*,#31239,.F.);
#40590=ORIENTED_EDGE('',*,*,#31244,.F.);
#40591=ORIENTED_EDGE('',*,*,#31245,.T.);
#40592=ORIENTED_EDGE('',*,*,#31246,.T.);
#40593=ORIENTED_EDGE('',*,*,#31242,.F.);
#40594=ORIENTED_EDGE('',*,*,#31247,.F.);
#40595=ORIENTED_EDGE('',*,*,#31248,.T.);
#40596=ORIENTED_EDGE('',*,*,#31249,.T.);
#40597=ORIENTED_EDGE('',*,*,#31245,.F.);
#40598=ORIENTED_EDGE('',*,*,#31250,.F.);
#40599=ORIENTED_EDGE('',*,*,#31251,.T.);
#40600=ORIENTED_EDGE('',*,*,#31252,.T.);
#40601=ORIENTED_EDGE('',*,*,#31248,.F.);
#40602=ORIENTED_EDGE('',*,*,#31253,.F.);
#40603=ORIENTED_EDGE('',*,*,#31254,.T.);
#40604=ORIENTED_EDGE('',*,*,#31255,.T.);
#40605=ORIENTED_EDGE('',*,*,#31251,.F.);
#40606=ORIENTED_EDGE('',*,*,#31256,.F.);
#40607=ORIENTED_EDGE('',*,*,#31257,.T.);
#40608=ORIENTED_EDGE('',*,*,#31258,.T.);
#40609=ORIENTED_EDGE('',*,*,#31254,.F.);
#40610=ORIENTED_EDGE('',*,*,#31259,.F.);
#40611=ORIENTED_EDGE('',*,*,#31260,.T.);
#40612=ORIENTED_EDGE('',*,*,#31261,.T.);
#40613=ORIENTED_EDGE('',*,*,#31257,.F.);
#40614=ORIENTED_EDGE('',*,*,#31262,.F.);
#40615=ORIENTED_EDGE('',*,*,#31263,.T.);
#40616=ORIENTED_EDGE('',*,*,#31264,.T.);
#40617=ORIENTED_EDGE('',*,*,#31260,.F.);
#40618=ORIENTED_EDGE('',*,*,#31265,.F.);
#40619=ORIENTED_EDGE('',*,*,#31266,.T.);
#40620=ORIENTED_EDGE('',*,*,#31267,.T.);
#40621=ORIENTED_EDGE('',*,*,#31263,.F.);
#40622=ORIENTED_EDGE('',*,*,#31268,.F.);
#40623=ORIENTED_EDGE('',*,*,#31269,.T.);
#40624=ORIENTED_EDGE('',*,*,#31270,.T.);
#40625=ORIENTED_EDGE('',*,*,#31266,.F.);
#40626=ORIENTED_EDGE('',*,*,#31271,.F.);
#40627=ORIENTED_EDGE('',*,*,#31272,.T.);
#40628=ORIENTED_EDGE('',*,*,#31273,.T.);
#40629=ORIENTED_EDGE('',*,*,#31269,.F.);
#40630=ORIENTED_EDGE('',*,*,#31274,.F.);
#40631=ORIENTED_EDGE('',*,*,#31189,.T.);
#40632=ORIENTED_EDGE('',*,*,#31275,.T.);
#40633=ORIENTED_EDGE('',*,*,#31272,.F.);
#40634=ORIENTED_EDGE('',*,*,#31275,.F.);
#40635=ORIENTED_EDGE('',*,*,#31188,.F.);
#40636=ORIENTED_EDGE('',*,*,#31192,.F.);
#40637=ORIENTED_EDGE('',*,*,#31195,.F.);
#40638=ORIENTED_EDGE('',*,*,#31198,.F.);
#40639=ORIENTED_EDGE('',*,*,#31201,.F.);
#40640=ORIENTED_EDGE('',*,*,#31204,.F.);
#40641=ORIENTED_EDGE('',*,*,#31207,.F.);
#40642=ORIENTED_EDGE('',*,*,#31210,.F.);
#40643=ORIENTED_EDGE('',*,*,#31213,.F.);
#40644=ORIENTED_EDGE('',*,*,#31216,.F.);
#40645=ORIENTED_EDGE('',*,*,#31219,.F.);
#40646=ORIENTED_EDGE('',*,*,#31222,.F.);
#40647=ORIENTED_EDGE('',*,*,#31225,.F.);
#40648=ORIENTED_EDGE('',*,*,#31228,.F.);
#40649=ORIENTED_EDGE('',*,*,#31231,.F.);
#40650=ORIENTED_EDGE('',*,*,#31234,.F.);
#40651=ORIENTED_EDGE('',*,*,#31237,.F.);
#40652=ORIENTED_EDGE('',*,*,#31240,.F.);
#40653=ORIENTED_EDGE('',*,*,#31243,.F.);
#40654=ORIENTED_EDGE('',*,*,#31246,.F.);
#40655=ORIENTED_EDGE('',*,*,#31249,.F.);
#40656=ORIENTED_EDGE('',*,*,#31252,.F.);
#40657=ORIENTED_EDGE('',*,*,#31255,.F.);
#40658=ORIENTED_EDGE('',*,*,#31258,.F.);
#40659=ORIENTED_EDGE('',*,*,#31261,.F.);
#40660=ORIENTED_EDGE('',*,*,#31264,.F.);
#40661=ORIENTED_EDGE('',*,*,#31267,.F.);
#40662=ORIENTED_EDGE('',*,*,#31270,.F.);
#40663=ORIENTED_EDGE('',*,*,#31273,.F.);
#40664=ORIENTED_EDGE('',*,*,#31126,.T.);
#40665=ORIENTED_EDGE('',*,*,#31148,.T.);
#40666=ORIENTED_EDGE('',*,*,#31145,.T.);
#40667=ORIENTED_EDGE('',*,*,#31142,.T.);
#40668=ORIENTED_EDGE('',*,*,#31139,.T.);
#40669=ORIENTED_EDGE('',*,*,#31136,.T.);
#40670=ORIENTED_EDGE('',*,*,#31133,.T.);
#40671=ORIENTED_EDGE('',*,*,#31130,.T.);
#40672=ORIENTED_EDGE('',*,*,#31276,.F.);
#40673=ORIENTED_EDGE('',*,*,#31277,.T.);
#40674=ORIENTED_EDGE('',*,*,#31278,.T.);
#40675=ORIENTED_EDGE('',*,*,#31279,.F.);
#40676=ORIENTED_EDGE('',*,*,#31280,.F.);
#40677=ORIENTED_EDGE('',*,*,#31281,.T.);
#40678=ORIENTED_EDGE('',*,*,#31282,.T.);
#40679=ORIENTED_EDGE('',*,*,#31277,.F.);
#40680=ORIENTED_EDGE('',*,*,#31283,.F.);
#40681=ORIENTED_EDGE('',*,*,#31284,.T.);
#40682=ORIENTED_EDGE('',*,*,#31285,.T.);
#40683=ORIENTED_EDGE('',*,*,#31281,.F.);
#40684=ORIENTED_EDGE('',*,*,#31286,.F.);
#40685=ORIENTED_EDGE('',*,*,#31287,.T.);
#40686=ORIENTED_EDGE('',*,*,#31288,.T.);
#40687=ORIENTED_EDGE('',*,*,#31284,.F.);
#40688=ORIENTED_EDGE('',*,*,#31289,.F.);
#40689=ORIENTED_EDGE('',*,*,#31290,.T.);
#40690=ORIENTED_EDGE('',*,*,#31291,.T.);
#40691=ORIENTED_EDGE('',*,*,#31287,.F.);
#40692=ORIENTED_EDGE('',*,*,#31292,.F.);
#40693=ORIENTED_EDGE('',*,*,#31293,.T.);
#40694=ORIENTED_EDGE('',*,*,#31294,.T.);
#40695=ORIENTED_EDGE('',*,*,#31290,.F.);
#40696=ORIENTED_EDGE('',*,*,#31295,.F.);
#40697=ORIENTED_EDGE('',*,*,#31296,.T.);
#40698=ORIENTED_EDGE('',*,*,#31297,.T.);
#40699=ORIENTED_EDGE('',*,*,#31293,.F.);
#40700=ORIENTED_EDGE('',*,*,#31298,.F.);
#40701=ORIENTED_EDGE('',*,*,#31279,.T.);
#40702=ORIENTED_EDGE('',*,*,#31299,.T.);
#40703=ORIENTED_EDGE('',*,*,#31296,.F.);
#40704=ORIENTED_EDGE('',*,*,#31300,.F.);
#40705=ORIENTED_EDGE('',*,*,#31301,.T.);
#40706=ORIENTED_EDGE('',*,*,#31302,.T.);
#40707=ORIENTED_EDGE('',*,*,#31303,.F.);
#40708=ORIENTED_EDGE('',*,*,#31304,.F.);
#40709=ORIENTED_EDGE('',*,*,#31305,.T.);
#40710=ORIENTED_EDGE('',*,*,#31306,.T.);
#40711=ORIENTED_EDGE('',*,*,#31301,.F.);
#40712=ORIENTED_EDGE('',*,*,#31307,.F.);
#40713=ORIENTED_EDGE('',*,*,#31308,.T.);
#40714=ORIENTED_EDGE('',*,*,#31309,.T.);
#40715=ORIENTED_EDGE('',*,*,#31305,.F.);
#40716=ORIENTED_EDGE('',*,*,#31310,.F.);
#40717=ORIENTED_EDGE('',*,*,#31311,.T.);
#40718=ORIENTED_EDGE('',*,*,#31312,.T.);
#40719=ORIENTED_EDGE('',*,*,#31308,.F.);
#40720=ORIENTED_EDGE('',*,*,#31313,.F.);
#40721=ORIENTED_EDGE('',*,*,#31314,.T.);
#40722=ORIENTED_EDGE('',*,*,#31315,.T.);
#40723=ORIENTED_EDGE('',*,*,#31311,.F.);
#40724=ORIENTED_EDGE('',*,*,#31316,.F.);
#40725=ORIENTED_EDGE('',*,*,#31317,.T.);
#40726=ORIENTED_EDGE('',*,*,#31318,.T.);
#40727=ORIENTED_EDGE('',*,*,#31314,.F.);
#40728=ORIENTED_EDGE('',*,*,#31319,.F.);
#40729=ORIENTED_EDGE('',*,*,#31320,.T.);
#40730=ORIENTED_EDGE('',*,*,#31321,.T.);
#40731=ORIENTED_EDGE('',*,*,#31317,.F.);
#40732=ORIENTED_EDGE('',*,*,#31322,.F.);
#40733=ORIENTED_EDGE('',*,*,#31323,.T.);
#40734=ORIENTED_EDGE('',*,*,#31324,.T.);
#40735=ORIENTED_EDGE('',*,*,#31320,.F.);
#40736=ORIENTED_EDGE('',*,*,#31325,.F.);
#40737=ORIENTED_EDGE('',*,*,#31326,.T.);
#40738=ORIENTED_EDGE('',*,*,#31327,.T.);
#40739=ORIENTED_EDGE('',*,*,#31323,.F.);
#40740=ORIENTED_EDGE('',*,*,#31328,.F.);
#40741=ORIENTED_EDGE('',*,*,#31329,.T.);
#40742=ORIENTED_EDGE('',*,*,#31330,.T.);
#40743=ORIENTED_EDGE('',*,*,#31326,.F.);
#40744=ORIENTED_EDGE('',*,*,#31331,.F.);
#40745=ORIENTED_EDGE('',*,*,#31332,.T.);
#40746=ORIENTED_EDGE('',*,*,#31333,.T.);
#40747=ORIENTED_EDGE('',*,*,#31329,.F.);
#40748=ORIENTED_EDGE('',*,*,#31334,.F.);
#40749=ORIENTED_EDGE('',*,*,#31303,.T.);
#40750=ORIENTED_EDGE('',*,*,#31335,.T.);
#40751=ORIENTED_EDGE('',*,*,#31332,.F.);
#40752=ORIENTED_EDGE('',*,*,#31335,.F.);
#40753=ORIENTED_EDGE('',*,*,#31302,.F.);
#40754=ORIENTED_EDGE('',*,*,#31306,.F.);
#40755=ORIENTED_EDGE('',*,*,#31309,.F.);
#40756=ORIENTED_EDGE('',*,*,#31312,.F.);
#40757=ORIENTED_EDGE('',*,*,#31315,.F.);
#40758=ORIENTED_EDGE('',*,*,#31318,.F.);
#40759=ORIENTED_EDGE('',*,*,#31321,.F.);
#40760=ORIENTED_EDGE('',*,*,#31324,.F.);
#40761=ORIENTED_EDGE('',*,*,#31327,.F.);
#40762=ORIENTED_EDGE('',*,*,#31330,.F.);
#40763=ORIENTED_EDGE('',*,*,#31333,.F.);
#40764=ORIENTED_EDGE('',*,*,#31299,.F.);
#40765=ORIENTED_EDGE('',*,*,#31278,.F.);
#40766=ORIENTED_EDGE('',*,*,#31282,.F.);
#40767=ORIENTED_EDGE('',*,*,#31285,.F.);
#40768=ORIENTED_EDGE('',*,*,#31288,.F.);
#40769=ORIENTED_EDGE('',*,*,#31291,.F.);
#40770=ORIENTED_EDGE('',*,*,#31294,.F.);
#40771=ORIENTED_EDGE('',*,*,#31297,.F.);
#40772=ORIENTED_EDGE('',*,*,#31336,.F.);
#40773=ORIENTED_EDGE('',*,*,#31337,.T.);
#40774=ORIENTED_EDGE('',*,*,#31338,.T.);
#40775=ORIENTED_EDGE('',*,*,#31339,.F.);
#40776=ORIENTED_EDGE('',*,*,#31340,.F.);
#40777=ORIENTED_EDGE('',*,*,#31341,.T.);
#40778=ORIENTED_EDGE('',*,*,#31342,.T.);
#40779=ORIENTED_EDGE('',*,*,#31337,.F.);
#40780=ORIENTED_EDGE('',*,*,#31343,.F.);
#40781=ORIENTED_EDGE('',*,*,#31344,.T.);
#40782=ORIENTED_EDGE('',*,*,#31345,.T.);
#40783=ORIENTED_EDGE('',*,*,#31341,.F.);
#40784=ORIENTED_EDGE('',*,*,#31346,.F.);
#40785=ORIENTED_EDGE('',*,*,#31347,.T.);
#40786=ORIENTED_EDGE('',*,*,#31348,.T.);
#40787=ORIENTED_EDGE('',*,*,#31344,.F.);
#40788=ORIENTED_EDGE('',*,*,#31349,.F.);
#40789=ORIENTED_EDGE('',*,*,#31350,.T.);
#40790=ORIENTED_EDGE('',*,*,#31351,.T.);
#40791=ORIENTED_EDGE('',*,*,#31347,.F.);
#40792=ORIENTED_EDGE('',*,*,#31352,.F.);
#40793=ORIENTED_EDGE('',*,*,#31353,.T.);
#40794=ORIENTED_EDGE('',*,*,#31354,.T.);
#40795=ORIENTED_EDGE('',*,*,#31350,.F.);
#40796=ORIENTED_EDGE('',*,*,#31355,.F.);
#40797=ORIENTED_EDGE('',*,*,#31356,.T.);
#40798=ORIENTED_EDGE('',*,*,#31357,.T.);
#40799=ORIENTED_EDGE('',*,*,#31353,.F.);
#40800=ORIENTED_EDGE('',*,*,#31358,.F.);
#40801=ORIENTED_EDGE('',*,*,#31359,.T.);
#40802=ORIENTED_EDGE('',*,*,#31360,.T.);
#40803=ORIENTED_EDGE('',*,*,#31356,.F.);
#40804=ORIENTED_EDGE('',*,*,#31361,.F.);
#40805=ORIENTED_EDGE('',*,*,#31362,.T.);
#40806=ORIENTED_EDGE('',*,*,#31363,.T.);
#40807=ORIENTED_EDGE('',*,*,#31359,.F.);
#40808=ORIENTED_EDGE('',*,*,#31364,.F.);
#40809=ORIENTED_EDGE('',*,*,#31365,.T.);
#40810=ORIENTED_EDGE('',*,*,#31366,.T.);
#40811=ORIENTED_EDGE('',*,*,#31362,.F.);
#40812=ORIENTED_EDGE('',*,*,#31367,.F.);
#40813=ORIENTED_EDGE('',*,*,#31368,.T.);
#40814=ORIENTED_EDGE('',*,*,#31369,.T.);
#40815=ORIENTED_EDGE('',*,*,#31365,.F.);
#40816=ORIENTED_EDGE('',*,*,#31370,.F.);
#40817=ORIENTED_EDGE('',*,*,#31371,.T.);
#40818=ORIENTED_EDGE('',*,*,#31372,.T.);
#40819=ORIENTED_EDGE('',*,*,#31368,.F.);
#40820=ORIENTED_EDGE('',*,*,#31373,.F.);
#40821=ORIENTED_EDGE('',*,*,#31374,.T.);
#40822=ORIENTED_EDGE('',*,*,#31375,.T.);
#40823=ORIENTED_EDGE('',*,*,#31371,.F.);
#40824=ORIENTED_EDGE('',*,*,#31376,.F.);
#40825=ORIENTED_EDGE('',*,*,#31377,.T.);
#40826=ORIENTED_EDGE('',*,*,#31378,.T.);
#40827=ORIENTED_EDGE('',*,*,#31374,.F.);
#40828=ORIENTED_EDGE('',*,*,#31379,.F.);
#40829=ORIENTED_EDGE('',*,*,#31380,.T.);
#40830=ORIENTED_EDGE('',*,*,#31381,.T.);
#40831=ORIENTED_EDGE('',*,*,#31377,.F.);
#40832=ORIENTED_EDGE('',*,*,#31382,.F.);
#40833=ORIENTED_EDGE('',*,*,#31383,.T.);
#40834=ORIENTED_EDGE('',*,*,#31384,.T.);
#40835=ORIENTED_EDGE('',*,*,#31380,.F.);
#40836=ORIENTED_EDGE('',*,*,#31385,.F.);
#40837=ORIENTED_EDGE('',*,*,#31386,.T.);
#40838=ORIENTED_EDGE('',*,*,#31387,.T.);
#40839=ORIENTED_EDGE('',*,*,#31383,.F.);
#40840=ORIENTED_EDGE('',*,*,#31388,.F.);
#40841=ORIENTED_EDGE('',*,*,#31389,.T.);
#40842=ORIENTED_EDGE('',*,*,#31390,.T.);
#40843=ORIENTED_EDGE('',*,*,#31386,.F.);
#40844=ORIENTED_EDGE('',*,*,#31391,.F.);
#40845=ORIENTED_EDGE('',*,*,#31392,.T.);
#40846=ORIENTED_EDGE('',*,*,#31393,.T.);
#40847=ORIENTED_EDGE('',*,*,#31389,.F.);
#40848=ORIENTED_EDGE('',*,*,#31394,.F.);
#40849=ORIENTED_EDGE('',*,*,#31395,.T.);
#40850=ORIENTED_EDGE('',*,*,#31396,.T.);
#40851=ORIENTED_EDGE('',*,*,#31392,.F.);
#40852=ORIENTED_EDGE('',*,*,#31397,.F.);
#40853=ORIENTED_EDGE('',*,*,#31398,.T.);
#40854=ORIENTED_EDGE('',*,*,#31399,.T.);
#40855=ORIENTED_EDGE('',*,*,#31395,.F.);
#40856=ORIENTED_EDGE('',*,*,#31400,.F.);
#40857=ORIENTED_EDGE('',*,*,#31339,.T.);
#40858=ORIENTED_EDGE('',*,*,#31401,.T.);
#40859=ORIENTED_EDGE('',*,*,#31398,.F.);
#40860=ORIENTED_EDGE('',*,*,#31401,.F.);
#40861=ORIENTED_EDGE('',*,*,#31338,.F.);
#40862=ORIENTED_EDGE('',*,*,#31342,.F.);
#40863=ORIENTED_EDGE('',*,*,#31345,.F.);
#40864=ORIENTED_EDGE('',*,*,#31348,.F.);
#40865=ORIENTED_EDGE('',*,*,#31351,.F.);
#40866=ORIENTED_EDGE('',*,*,#31354,.F.);
#40867=ORIENTED_EDGE('',*,*,#31357,.F.);
#40868=ORIENTED_EDGE('',*,*,#31360,.F.);
#40869=ORIENTED_EDGE('',*,*,#31363,.F.);
#40870=ORIENTED_EDGE('',*,*,#31366,.F.);
#40871=ORIENTED_EDGE('',*,*,#31369,.F.);
#40872=ORIENTED_EDGE('',*,*,#31372,.F.);
#40873=ORIENTED_EDGE('',*,*,#31375,.F.);
#40874=ORIENTED_EDGE('',*,*,#31378,.F.);
#40875=ORIENTED_EDGE('',*,*,#31381,.F.);
#40876=ORIENTED_EDGE('',*,*,#31384,.F.);
#40877=ORIENTED_EDGE('',*,*,#31387,.F.);
#40878=ORIENTED_EDGE('',*,*,#31390,.F.);
#40879=ORIENTED_EDGE('',*,*,#31393,.F.);
#40880=ORIENTED_EDGE('',*,*,#31396,.F.);
#40881=ORIENTED_EDGE('',*,*,#31399,.F.);
#40882=ORIENTED_EDGE('',*,*,#31276,.T.);
#40883=ORIENTED_EDGE('',*,*,#31298,.T.);
#40884=ORIENTED_EDGE('',*,*,#31295,.T.);
#40885=ORIENTED_EDGE('',*,*,#31292,.T.);
#40886=ORIENTED_EDGE('',*,*,#31289,.T.);
#40887=ORIENTED_EDGE('',*,*,#31286,.T.);
#40888=ORIENTED_EDGE('',*,*,#31283,.T.);
#40889=ORIENTED_EDGE('',*,*,#31280,.T.);
#40890=ORIENTED_EDGE('',*,*,#31402,.F.);
#40891=ORIENTED_EDGE('',*,*,#31403,.T.);
#40892=ORIENTED_EDGE('',*,*,#31404,.T.);
#40893=ORIENTED_EDGE('',*,*,#31405,.F.);
#40894=ORIENTED_EDGE('',*,*,#31406,.F.);
#40895=ORIENTED_EDGE('',*,*,#31407,.T.);
#40896=ORIENTED_EDGE('',*,*,#31408,.T.);
#40897=ORIENTED_EDGE('',*,*,#31403,.F.);
#40898=ORIENTED_EDGE('',*,*,#31409,.F.);
#40899=ORIENTED_EDGE('',*,*,#31410,.T.);
#40900=ORIENTED_EDGE('',*,*,#31411,.T.);
#40901=ORIENTED_EDGE('',*,*,#31407,.F.);
#40902=ORIENTED_EDGE('',*,*,#31412,.F.);
#40903=ORIENTED_EDGE('',*,*,#31413,.T.);
#40904=ORIENTED_EDGE('',*,*,#31414,.T.);
#40905=ORIENTED_EDGE('',*,*,#31410,.F.);
#40906=ORIENTED_EDGE('',*,*,#31415,.F.);
#40907=ORIENTED_EDGE('',*,*,#31416,.T.);
#40908=ORIENTED_EDGE('',*,*,#31417,.T.);
#40909=ORIENTED_EDGE('',*,*,#31413,.F.);
#40910=ORIENTED_EDGE('',*,*,#31418,.F.);
#40911=ORIENTED_EDGE('',*,*,#31419,.T.);
#40912=ORIENTED_EDGE('',*,*,#31420,.T.);
#40913=ORIENTED_EDGE('',*,*,#31416,.F.);
#40914=ORIENTED_EDGE('',*,*,#31421,.F.);
#40915=ORIENTED_EDGE('',*,*,#31422,.T.);
#40916=ORIENTED_EDGE('',*,*,#31423,.T.);
#40917=ORIENTED_EDGE('',*,*,#31419,.F.);
#40918=ORIENTED_EDGE('',*,*,#31424,.F.);
#40919=ORIENTED_EDGE('',*,*,#31405,.T.);
#40920=ORIENTED_EDGE('',*,*,#31425,.T.);
#40921=ORIENTED_EDGE('',*,*,#31422,.F.);
#40922=ORIENTED_EDGE('',*,*,#31426,.F.);
#40923=ORIENTED_EDGE('',*,*,#31427,.T.);
#40924=ORIENTED_EDGE('',*,*,#31428,.T.);
#40925=ORIENTED_EDGE('',*,*,#31429,.F.);
#40926=ORIENTED_EDGE('',*,*,#31430,.F.);
#40927=ORIENTED_EDGE('',*,*,#31431,.T.);
#40928=ORIENTED_EDGE('',*,*,#31432,.T.);
#40929=ORIENTED_EDGE('',*,*,#31427,.F.);
#40930=ORIENTED_EDGE('',*,*,#31433,.F.);
#40931=ORIENTED_EDGE('',*,*,#31434,.T.);
#40932=ORIENTED_EDGE('',*,*,#31435,.T.);
#40933=ORIENTED_EDGE('',*,*,#31431,.F.);
#40934=ORIENTED_EDGE('',*,*,#31436,.F.);
#40935=ORIENTED_EDGE('',*,*,#31437,.T.);
#40936=ORIENTED_EDGE('',*,*,#31438,.T.);
#40937=ORIENTED_EDGE('',*,*,#31434,.F.);
#40938=ORIENTED_EDGE('',*,*,#31439,.F.);
#40939=ORIENTED_EDGE('',*,*,#31440,.T.);
#40940=ORIENTED_EDGE('',*,*,#31441,.T.);
#40941=ORIENTED_EDGE('',*,*,#31437,.F.);
#40942=ORIENTED_EDGE('',*,*,#31442,.F.);
#40943=ORIENTED_EDGE('',*,*,#31443,.T.);
#40944=ORIENTED_EDGE('',*,*,#31444,.T.);
#40945=ORIENTED_EDGE('',*,*,#31440,.F.);
#40946=ORIENTED_EDGE('',*,*,#31445,.F.);
#40947=ORIENTED_EDGE('',*,*,#31446,.T.);
#40948=ORIENTED_EDGE('',*,*,#31447,.T.);
#40949=ORIENTED_EDGE('',*,*,#31443,.F.);
#40950=ORIENTED_EDGE('',*,*,#31448,.F.);
#40951=ORIENTED_EDGE('',*,*,#31449,.T.);
#40952=ORIENTED_EDGE('',*,*,#31450,.T.);
#40953=ORIENTED_EDGE('',*,*,#31446,.F.);
#40954=ORIENTED_EDGE('',*,*,#31451,.F.);
#40955=ORIENTED_EDGE('',*,*,#31452,.T.);
#40956=ORIENTED_EDGE('',*,*,#31453,.T.);
#40957=ORIENTED_EDGE('',*,*,#31449,.F.);
#40958=ORIENTED_EDGE('',*,*,#31454,.F.);
#40959=ORIENTED_EDGE('',*,*,#31455,.T.);
#40960=ORIENTED_EDGE('',*,*,#31456,.T.);
#40961=ORIENTED_EDGE('',*,*,#31452,.F.);
#40962=ORIENTED_EDGE('',*,*,#31457,.F.);
#40963=ORIENTED_EDGE('',*,*,#31458,.T.);
#40964=ORIENTED_EDGE('',*,*,#31459,.T.);
#40965=ORIENTED_EDGE('',*,*,#31455,.F.);
#40966=ORIENTED_EDGE('',*,*,#31460,.F.);
#40967=ORIENTED_EDGE('',*,*,#31429,.T.);
#40968=ORIENTED_EDGE('',*,*,#31461,.T.);
#40969=ORIENTED_EDGE('',*,*,#31458,.F.);
#40970=ORIENTED_EDGE('',*,*,#31461,.F.);
#40971=ORIENTED_EDGE('',*,*,#31428,.F.);
#40972=ORIENTED_EDGE('',*,*,#31432,.F.);
#40973=ORIENTED_EDGE('',*,*,#31435,.F.);
#40974=ORIENTED_EDGE('',*,*,#31438,.F.);
#40975=ORIENTED_EDGE('',*,*,#31441,.F.);
#40976=ORIENTED_EDGE('',*,*,#31444,.F.);
#40977=ORIENTED_EDGE('',*,*,#31447,.F.);
#40978=ORIENTED_EDGE('',*,*,#31450,.F.);
#40979=ORIENTED_EDGE('',*,*,#31453,.F.);
#40980=ORIENTED_EDGE('',*,*,#31456,.F.);
#40981=ORIENTED_EDGE('',*,*,#31459,.F.);
#40982=ORIENTED_EDGE('',*,*,#31425,.F.);
#40983=ORIENTED_EDGE('',*,*,#31404,.F.);
#40984=ORIENTED_EDGE('',*,*,#31408,.F.);
#40985=ORIENTED_EDGE('',*,*,#31411,.F.);
#40986=ORIENTED_EDGE('',*,*,#31414,.F.);
#40987=ORIENTED_EDGE('',*,*,#31417,.F.);
#40988=ORIENTED_EDGE('',*,*,#31420,.F.);
#40989=ORIENTED_EDGE('',*,*,#31423,.F.);
#40990=ORIENTED_EDGE('',*,*,#31462,.F.);
#40991=ORIENTED_EDGE('',*,*,#31463,.T.);
#40992=ORIENTED_EDGE('',*,*,#31464,.T.);
#40993=ORIENTED_EDGE('',*,*,#31465,.F.);
#40994=ORIENTED_EDGE('',*,*,#31466,.F.);
#40995=ORIENTED_EDGE('',*,*,#31467,.T.);
#40996=ORIENTED_EDGE('',*,*,#31468,.T.);
#40997=ORIENTED_EDGE('',*,*,#31463,.F.);
#40998=ORIENTED_EDGE('',*,*,#31469,.F.);
#40999=ORIENTED_EDGE('',*,*,#31470,.T.);
#41000=ORIENTED_EDGE('',*,*,#31471,.T.);
#41001=ORIENTED_EDGE('',*,*,#31467,.F.);
#41002=ORIENTED_EDGE('',*,*,#31472,.F.);
#41003=ORIENTED_EDGE('',*,*,#31473,.T.);
#41004=ORIENTED_EDGE('',*,*,#31474,.T.);
#41005=ORIENTED_EDGE('',*,*,#31470,.F.);
#41006=ORIENTED_EDGE('',*,*,#31475,.F.);
#41007=ORIENTED_EDGE('',*,*,#31476,.T.);
#41008=ORIENTED_EDGE('',*,*,#31477,.T.);
#41009=ORIENTED_EDGE('',*,*,#31473,.F.);
#41010=ORIENTED_EDGE('',*,*,#31478,.F.);
#41011=ORIENTED_EDGE('',*,*,#31479,.T.);
#41012=ORIENTED_EDGE('',*,*,#31480,.T.);
#41013=ORIENTED_EDGE('',*,*,#31476,.F.);
#41014=ORIENTED_EDGE('',*,*,#31481,.F.);
#41015=ORIENTED_EDGE('',*,*,#31482,.T.);
#41016=ORIENTED_EDGE('',*,*,#31483,.T.);
#41017=ORIENTED_EDGE('',*,*,#31479,.F.);
#41018=ORIENTED_EDGE('',*,*,#31484,.F.);
#41019=ORIENTED_EDGE('',*,*,#31485,.T.);
#41020=ORIENTED_EDGE('',*,*,#31486,.T.);
#41021=ORIENTED_EDGE('',*,*,#31482,.F.);
#41022=ORIENTED_EDGE('',*,*,#31487,.F.);
#41023=ORIENTED_EDGE('',*,*,#31465,.T.);
#41024=ORIENTED_EDGE('',*,*,#31488,.T.);
#41025=ORIENTED_EDGE('',*,*,#31485,.F.);
#41026=ORIENTED_EDGE('',*,*,#31488,.F.);
#41027=ORIENTED_EDGE('',*,*,#31464,.F.);
#41028=ORIENTED_EDGE('',*,*,#31468,.F.);
#41029=ORIENTED_EDGE('',*,*,#31471,.F.);
#41030=ORIENTED_EDGE('',*,*,#31474,.F.);
#41031=ORIENTED_EDGE('',*,*,#31477,.F.);
#41032=ORIENTED_EDGE('',*,*,#31480,.F.);
#41033=ORIENTED_EDGE('',*,*,#31483,.F.);
#41034=ORIENTED_EDGE('',*,*,#31486,.F.);
#41035=ORIENTED_EDGE('',*,*,#31402,.T.);
#41036=ORIENTED_EDGE('',*,*,#31424,.T.);
#41037=ORIENTED_EDGE('',*,*,#31421,.T.);
#41038=ORIENTED_EDGE('',*,*,#31418,.T.);
#41039=ORIENTED_EDGE('',*,*,#31415,.T.);
#41040=ORIENTED_EDGE('',*,*,#31412,.T.);
#41041=ORIENTED_EDGE('',*,*,#31409,.T.);
#41042=ORIENTED_EDGE('',*,*,#31406,.T.);
#41043=ORIENTED_EDGE('',*,*,#31489,.F.);
#41044=ORIENTED_EDGE('',*,*,#31490,.T.);
#41045=ORIENTED_EDGE('',*,*,#31491,.T.);
#41046=ORIENTED_EDGE('',*,*,#31492,.F.);
#41047=ORIENTED_EDGE('',*,*,#31493,.F.);
#41048=ORIENTED_EDGE('',*,*,#31494,.T.);
#41049=ORIENTED_EDGE('',*,*,#31495,.T.);
#41050=ORIENTED_EDGE('',*,*,#31490,.F.);
#41051=ORIENTED_EDGE('',*,*,#31496,.F.);
#41052=ORIENTED_EDGE('',*,*,#31497,.T.);
#41053=ORIENTED_EDGE('',*,*,#31498,.T.);
#41054=ORIENTED_EDGE('',*,*,#31494,.F.);
#41055=ORIENTED_EDGE('',*,*,#31499,.F.);
#41056=ORIENTED_EDGE('',*,*,#31500,.T.);
#41057=ORIENTED_EDGE('',*,*,#31501,.T.);
#41058=ORIENTED_EDGE('',*,*,#31497,.F.);
#41059=ORIENTED_EDGE('',*,*,#31502,.F.);
#41060=ORIENTED_EDGE('',*,*,#31503,.T.);
#41061=ORIENTED_EDGE('',*,*,#31504,.T.);
#41062=ORIENTED_EDGE('',*,*,#31500,.F.);
#41063=ORIENTED_EDGE('',*,*,#31505,.F.);
#41064=ORIENTED_EDGE('',*,*,#31506,.T.);
#41065=ORIENTED_EDGE('',*,*,#31507,.T.);
#41066=ORIENTED_EDGE('',*,*,#31503,.F.);
#41067=ORIENTED_EDGE('',*,*,#31508,.F.);
#41068=ORIENTED_EDGE('',*,*,#31509,.T.);
#41069=ORIENTED_EDGE('',*,*,#31510,.T.);
#41070=ORIENTED_EDGE('',*,*,#31506,.F.);
#41071=ORIENTED_EDGE('',*,*,#31511,.F.);
#41072=ORIENTED_EDGE('',*,*,#31492,.T.);
#41073=ORIENTED_EDGE('',*,*,#31512,.T.);
#41074=ORIENTED_EDGE('',*,*,#31509,.F.);
#41075=ORIENTED_EDGE('',*,*,#31513,.F.);
#41076=ORIENTED_EDGE('',*,*,#31514,.T.);
#41077=ORIENTED_EDGE('',*,*,#31515,.T.);
#41078=ORIENTED_EDGE('',*,*,#31516,.F.);
#41079=ORIENTED_EDGE('',*,*,#31517,.F.);
#41080=ORIENTED_EDGE('',*,*,#31518,.T.);
#41081=ORIENTED_EDGE('',*,*,#31519,.T.);
#41082=ORIENTED_EDGE('',*,*,#31514,.F.);
#41083=ORIENTED_EDGE('',*,*,#31520,.F.);
#41084=ORIENTED_EDGE('',*,*,#31521,.T.);
#41085=ORIENTED_EDGE('',*,*,#31522,.T.);
#41086=ORIENTED_EDGE('',*,*,#31518,.F.);
#41087=ORIENTED_EDGE('',*,*,#31523,.F.);
#41088=ORIENTED_EDGE('',*,*,#31524,.T.);
#41089=ORIENTED_EDGE('',*,*,#31525,.T.);
#41090=ORIENTED_EDGE('',*,*,#31521,.F.);
#41091=ORIENTED_EDGE('',*,*,#31526,.F.);
#41092=ORIENTED_EDGE('',*,*,#31527,.T.);
#41093=ORIENTED_EDGE('',*,*,#31528,.T.);
#41094=ORIENTED_EDGE('',*,*,#31524,.F.);
#41095=ORIENTED_EDGE('',*,*,#31529,.F.);
#41096=ORIENTED_EDGE('',*,*,#31530,.T.);
#41097=ORIENTED_EDGE('',*,*,#31531,.T.);
#41098=ORIENTED_EDGE('',*,*,#31527,.F.);
#41099=ORIENTED_EDGE('',*,*,#31532,.F.);
#41100=ORIENTED_EDGE('',*,*,#31533,.T.);
#41101=ORIENTED_EDGE('',*,*,#31534,.T.);
#41102=ORIENTED_EDGE('',*,*,#31530,.F.);
#41103=ORIENTED_EDGE('',*,*,#31535,.F.);
#41104=ORIENTED_EDGE('',*,*,#31536,.T.);
#41105=ORIENTED_EDGE('',*,*,#31537,.T.);
#41106=ORIENTED_EDGE('',*,*,#31533,.F.);
#41107=ORIENTED_EDGE('',*,*,#31538,.F.);
#41108=ORIENTED_EDGE('',*,*,#31539,.T.);
#41109=ORIENTED_EDGE('',*,*,#31540,.T.);
#41110=ORIENTED_EDGE('',*,*,#31536,.F.);
#41111=ORIENTED_EDGE('',*,*,#31541,.F.);
#41112=ORIENTED_EDGE('',*,*,#31542,.T.);
#41113=ORIENTED_EDGE('',*,*,#31543,.T.);
#41114=ORIENTED_EDGE('',*,*,#31539,.F.);
#41115=ORIENTED_EDGE('',*,*,#31544,.F.);
#41116=ORIENTED_EDGE('',*,*,#31545,.T.);
#41117=ORIENTED_EDGE('',*,*,#31546,.T.);
#41118=ORIENTED_EDGE('',*,*,#31542,.F.);
#41119=ORIENTED_EDGE('',*,*,#31547,.F.);
#41120=ORIENTED_EDGE('',*,*,#31516,.T.);
#41121=ORIENTED_EDGE('',*,*,#31548,.T.);
#41122=ORIENTED_EDGE('',*,*,#31545,.F.);
#41123=ORIENTED_EDGE('',*,*,#31548,.F.);
#41124=ORIENTED_EDGE('',*,*,#31515,.F.);
#41125=ORIENTED_EDGE('',*,*,#31519,.F.);
#41126=ORIENTED_EDGE('',*,*,#31522,.F.);
#41127=ORIENTED_EDGE('',*,*,#31525,.F.);
#41128=ORIENTED_EDGE('',*,*,#31528,.F.);
#41129=ORIENTED_EDGE('',*,*,#31531,.F.);
#41130=ORIENTED_EDGE('',*,*,#31534,.F.);
#41131=ORIENTED_EDGE('',*,*,#31537,.F.);
#41132=ORIENTED_EDGE('',*,*,#31540,.F.);
#41133=ORIENTED_EDGE('',*,*,#31543,.F.);
#41134=ORIENTED_EDGE('',*,*,#31546,.F.);
#41135=ORIENTED_EDGE('',*,*,#31512,.F.);
#41136=ORIENTED_EDGE('',*,*,#31491,.F.);
#41137=ORIENTED_EDGE('',*,*,#31495,.F.);
#41138=ORIENTED_EDGE('',*,*,#31498,.F.);
#41139=ORIENTED_EDGE('',*,*,#31501,.F.);
#41140=ORIENTED_EDGE('',*,*,#31504,.F.);
#41141=ORIENTED_EDGE('',*,*,#31507,.F.);
#41142=ORIENTED_EDGE('',*,*,#31510,.F.);
#41143=ORIENTED_EDGE('',*,*,#31489,.T.);
#41144=ORIENTED_EDGE('',*,*,#31511,.T.);
#41145=ORIENTED_EDGE('',*,*,#31508,.T.);
#41146=ORIENTED_EDGE('',*,*,#31505,.T.);
#41147=ORIENTED_EDGE('',*,*,#31502,.T.);
#41148=ORIENTED_EDGE('',*,*,#31499,.T.);
#41149=ORIENTED_EDGE('',*,*,#31496,.T.);
#41150=ORIENTED_EDGE('',*,*,#31493,.T.);
#41151=ORIENTED_EDGE('',*,*,#31549,.F.);
#41152=ORIENTED_EDGE('',*,*,#31550,.T.);
#41153=ORIENTED_EDGE('',*,*,#31551,.T.);
#41154=ORIENTED_EDGE('',*,*,#31552,.F.);
#41155=ORIENTED_EDGE('',*,*,#31553,.F.);
#41156=ORIENTED_EDGE('',*,*,#31554,.T.);
#41157=ORIENTED_EDGE('',*,*,#31555,.T.);
#41158=ORIENTED_EDGE('',*,*,#31550,.F.);
#41159=ORIENTED_EDGE('',*,*,#31556,.F.);
#41160=ORIENTED_EDGE('',*,*,#31557,.T.);
#41161=ORIENTED_EDGE('',*,*,#31558,.T.);
#41162=ORIENTED_EDGE('',*,*,#31554,.F.);
#41163=ORIENTED_EDGE('',*,*,#31559,.F.);
#41164=ORIENTED_EDGE('',*,*,#31560,.T.);
#41165=ORIENTED_EDGE('',*,*,#31561,.T.);
#41166=ORIENTED_EDGE('',*,*,#31557,.F.);
#41167=ORIENTED_EDGE('',*,*,#31562,.F.);
#41168=ORIENTED_EDGE('',*,*,#31563,.T.);
#41169=ORIENTED_EDGE('',*,*,#31564,.T.);
#41170=ORIENTED_EDGE('',*,*,#31560,.F.);
#41171=ORIENTED_EDGE('',*,*,#31565,.F.);
#41172=ORIENTED_EDGE('',*,*,#31566,.T.);
#41173=ORIENTED_EDGE('',*,*,#31567,.T.);
#41174=ORIENTED_EDGE('',*,*,#31563,.F.);
#41175=ORIENTED_EDGE('',*,*,#31568,.F.);
#41176=ORIENTED_EDGE('',*,*,#31569,.T.);
#41177=ORIENTED_EDGE('',*,*,#31570,.T.);
#41178=ORIENTED_EDGE('',*,*,#31566,.F.);
#41179=ORIENTED_EDGE('',*,*,#31571,.F.);
#41180=ORIENTED_EDGE('',*,*,#31552,.T.);
#41181=ORIENTED_EDGE('',*,*,#31572,.T.);
#41182=ORIENTED_EDGE('',*,*,#31569,.F.);
#41183=ORIENTED_EDGE('',*,*,#31573,.F.);
#41184=ORIENTED_EDGE('',*,*,#31574,.T.);
#41185=ORIENTED_EDGE('',*,*,#31575,.T.);
#41186=ORIENTED_EDGE('',*,*,#31576,.F.);
#41187=ORIENTED_EDGE('',*,*,#31577,.F.);
#41188=ORIENTED_EDGE('',*,*,#31578,.T.);
#41189=ORIENTED_EDGE('',*,*,#31579,.T.);
#41190=ORIENTED_EDGE('',*,*,#31574,.F.);
#41191=ORIENTED_EDGE('',*,*,#31580,.F.);
#41192=ORIENTED_EDGE('',*,*,#31581,.T.);
#41193=ORIENTED_EDGE('',*,*,#31582,.T.);
#41194=ORIENTED_EDGE('',*,*,#31578,.F.);
#41195=ORIENTED_EDGE('',*,*,#31583,.F.);
#41196=ORIENTED_EDGE('',*,*,#31584,.T.);
#41197=ORIENTED_EDGE('',*,*,#31585,.T.);
#41198=ORIENTED_EDGE('',*,*,#31581,.F.);
#41199=ORIENTED_EDGE('',*,*,#31586,.F.);
#41200=ORIENTED_EDGE('',*,*,#31587,.T.);
#41201=ORIENTED_EDGE('',*,*,#31588,.T.);
#41202=ORIENTED_EDGE('',*,*,#31584,.F.);
#41203=ORIENTED_EDGE('',*,*,#31589,.F.);
#41204=ORIENTED_EDGE('',*,*,#31590,.T.);
#41205=ORIENTED_EDGE('',*,*,#31591,.T.);
#41206=ORIENTED_EDGE('',*,*,#31587,.F.);
#41207=ORIENTED_EDGE('',*,*,#31592,.F.);
#41208=ORIENTED_EDGE('',*,*,#31593,.T.);
#41209=ORIENTED_EDGE('',*,*,#31594,.T.);
#41210=ORIENTED_EDGE('',*,*,#31590,.F.);
#41211=ORIENTED_EDGE('',*,*,#31595,.F.);
#41212=ORIENTED_EDGE('',*,*,#31596,.T.);
#41213=ORIENTED_EDGE('',*,*,#31597,.T.);
#41214=ORIENTED_EDGE('',*,*,#31593,.F.);
#41215=ORIENTED_EDGE('',*,*,#31598,.F.);
#41216=ORIENTED_EDGE('',*,*,#31599,.T.);
#41217=ORIENTED_EDGE('',*,*,#31600,.T.);
#41218=ORIENTED_EDGE('',*,*,#31596,.F.);
#41219=ORIENTED_EDGE('',*,*,#31601,.F.);
#41220=ORIENTED_EDGE('',*,*,#31602,.T.);
#41221=ORIENTED_EDGE('',*,*,#31603,.T.);
#41222=ORIENTED_EDGE('',*,*,#31599,.F.);
#41223=ORIENTED_EDGE('',*,*,#31604,.F.);
#41224=ORIENTED_EDGE('',*,*,#31605,.T.);
#41225=ORIENTED_EDGE('',*,*,#31606,.T.);
#41226=ORIENTED_EDGE('',*,*,#31602,.F.);
#41227=ORIENTED_EDGE('',*,*,#31607,.F.);
#41228=ORIENTED_EDGE('',*,*,#31576,.T.);
#41229=ORIENTED_EDGE('',*,*,#31608,.T.);
#41230=ORIENTED_EDGE('',*,*,#31605,.F.);
#41231=ORIENTED_EDGE('',*,*,#31608,.F.);
#41232=ORIENTED_EDGE('',*,*,#31575,.F.);
#41233=ORIENTED_EDGE('',*,*,#31579,.F.);
#41234=ORIENTED_EDGE('',*,*,#31582,.F.);
#41235=ORIENTED_EDGE('',*,*,#31585,.F.);
#41236=ORIENTED_EDGE('',*,*,#31588,.F.);
#41237=ORIENTED_EDGE('',*,*,#31591,.F.);
#41238=ORIENTED_EDGE('',*,*,#31594,.F.);
#41239=ORIENTED_EDGE('',*,*,#31597,.F.);
#41240=ORIENTED_EDGE('',*,*,#31600,.F.);
#41241=ORIENTED_EDGE('',*,*,#31603,.F.);
#41242=ORIENTED_EDGE('',*,*,#31606,.F.);
#41243=ORIENTED_EDGE('',*,*,#31572,.F.);
#41244=ORIENTED_EDGE('',*,*,#31551,.F.);
#41245=ORIENTED_EDGE('',*,*,#31555,.F.);
#41246=ORIENTED_EDGE('',*,*,#31558,.F.);
#41247=ORIENTED_EDGE('',*,*,#31561,.F.);
#41248=ORIENTED_EDGE('',*,*,#31564,.F.);
#41249=ORIENTED_EDGE('',*,*,#31567,.F.);
#41250=ORIENTED_EDGE('',*,*,#31570,.F.);
#41251=ORIENTED_EDGE('',*,*,#31609,.F.);
#41252=ORIENTED_EDGE('',*,*,#31610,.T.);
#41253=ORIENTED_EDGE('',*,*,#31611,.T.);
#41254=ORIENTED_EDGE('',*,*,#31612,.F.);
#41255=ORIENTED_EDGE('',*,*,#31613,.F.);
#41256=ORIENTED_EDGE('',*,*,#31614,.T.);
#41257=ORIENTED_EDGE('',*,*,#31615,.T.);
#41258=ORIENTED_EDGE('',*,*,#31610,.F.);
#41259=ORIENTED_EDGE('',*,*,#31616,.F.);
#41260=ORIENTED_EDGE('',*,*,#31617,.T.);
#41261=ORIENTED_EDGE('',*,*,#31618,.T.);
#41262=ORIENTED_EDGE('',*,*,#31614,.F.);
#41263=ORIENTED_EDGE('',*,*,#31619,.F.);
#41264=ORIENTED_EDGE('',*,*,#31620,.T.);
#41265=ORIENTED_EDGE('',*,*,#31621,.T.);
#41266=ORIENTED_EDGE('',*,*,#31617,.F.);
#41267=ORIENTED_EDGE('',*,*,#31622,.F.);
#41268=ORIENTED_EDGE('',*,*,#31623,.T.);
#41269=ORIENTED_EDGE('',*,*,#31624,.T.);
#41270=ORIENTED_EDGE('',*,*,#31620,.F.);
#41271=ORIENTED_EDGE('',*,*,#31625,.F.);
#41272=ORIENTED_EDGE('',*,*,#31626,.T.);
#41273=ORIENTED_EDGE('',*,*,#31627,.T.);
#41274=ORIENTED_EDGE('',*,*,#31623,.F.);
#41275=ORIENTED_EDGE('',*,*,#31628,.F.);
#41276=ORIENTED_EDGE('',*,*,#31629,.T.);
#41277=ORIENTED_EDGE('',*,*,#31630,.T.);
#41278=ORIENTED_EDGE('',*,*,#31626,.F.);
#41279=ORIENTED_EDGE('',*,*,#31631,.F.);
#41280=ORIENTED_EDGE('',*,*,#31632,.T.);
#41281=ORIENTED_EDGE('',*,*,#31633,.T.);
#41282=ORIENTED_EDGE('',*,*,#31629,.F.);
#41283=ORIENTED_EDGE('',*,*,#31634,.F.);
#41284=ORIENTED_EDGE('',*,*,#31612,.T.);
#41285=ORIENTED_EDGE('',*,*,#31635,.T.);
#41286=ORIENTED_EDGE('',*,*,#31632,.F.);
#41287=ORIENTED_EDGE('',*,*,#31635,.F.);
#41288=ORIENTED_EDGE('',*,*,#31611,.F.);
#41289=ORIENTED_EDGE('',*,*,#31615,.F.);
#41290=ORIENTED_EDGE('',*,*,#31618,.F.);
#41291=ORIENTED_EDGE('',*,*,#31621,.F.);
#41292=ORIENTED_EDGE('',*,*,#31624,.F.);
#41293=ORIENTED_EDGE('',*,*,#31627,.F.);
#41294=ORIENTED_EDGE('',*,*,#31630,.F.);
#41295=ORIENTED_EDGE('',*,*,#31633,.F.);
#41296=ORIENTED_EDGE('',*,*,#31549,.T.);
#41297=ORIENTED_EDGE('',*,*,#31571,.T.);
#41298=ORIENTED_EDGE('',*,*,#31568,.T.);
#41299=ORIENTED_EDGE('',*,*,#31565,.T.);
#41300=ORIENTED_EDGE('',*,*,#31562,.T.);
#41301=ORIENTED_EDGE('',*,*,#31559,.T.);
#41302=ORIENTED_EDGE('',*,*,#31556,.T.);
#41303=ORIENTED_EDGE('',*,*,#31553,.T.);
#41304=ORIENTED_EDGE('',*,*,#31636,.F.);
#41305=ORIENTED_EDGE('',*,*,#31637,.T.);
#41306=ORIENTED_EDGE('',*,*,#31638,.T.);
#41307=ORIENTED_EDGE('',*,*,#31639,.F.);
#41308=ORIENTED_EDGE('',*,*,#31640,.F.);
#41309=ORIENTED_EDGE('',*,*,#31641,.T.);
#41310=ORIENTED_EDGE('',*,*,#31642,.T.);
#41311=ORIENTED_EDGE('',*,*,#31637,.F.);
#41312=ORIENTED_EDGE('',*,*,#31643,.F.);
#41313=ORIENTED_EDGE('',*,*,#31644,.T.);
#41314=ORIENTED_EDGE('',*,*,#31645,.T.);
#41315=ORIENTED_EDGE('',*,*,#31641,.F.);
#41316=ORIENTED_EDGE('',*,*,#31646,.F.);
#41317=ORIENTED_EDGE('',*,*,#31647,.T.);
#41318=ORIENTED_EDGE('',*,*,#31648,.T.);
#41319=ORIENTED_EDGE('',*,*,#31644,.F.);
#41320=ORIENTED_EDGE('',*,*,#31649,.F.);
#41321=ORIENTED_EDGE('',*,*,#31650,.T.);
#41322=ORIENTED_EDGE('',*,*,#31651,.T.);
#41323=ORIENTED_EDGE('',*,*,#31647,.F.);
#41324=ORIENTED_EDGE('',*,*,#31652,.F.);
#41325=ORIENTED_EDGE('',*,*,#31653,.T.);
#41326=ORIENTED_EDGE('',*,*,#31654,.T.);
#41327=ORIENTED_EDGE('',*,*,#31650,.F.);
#41328=ORIENTED_EDGE('',*,*,#31655,.F.);
#41329=ORIENTED_EDGE('',*,*,#31656,.T.);
#41330=ORIENTED_EDGE('',*,*,#31657,.T.);
#41331=ORIENTED_EDGE('',*,*,#31653,.F.);
#41332=ORIENTED_EDGE('',*,*,#31658,.F.);
#41333=ORIENTED_EDGE('',*,*,#31639,.T.);
#41334=ORIENTED_EDGE('',*,*,#31659,.T.);
#41335=ORIENTED_EDGE('',*,*,#31656,.F.);
#41336=ORIENTED_EDGE('',*,*,#31660,.F.);
#41337=ORIENTED_EDGE('',*,*,#31661,.T.);
#41338=ORIENTED_EDGE('',*,*,#31662,.T.);
#41339=ORIENTED_EDGE('',*,*,#31663,.F.);
#41340=ORIENTED_EDGE('',*,*,#31664,.F.);
#41341=ORIENTED_EDGE('',*,*,#31665,.T.);
#41342=ORIENTED_EDGE('',*,*,#31666,.T.);
#41343=ORIENTED_EDGE('',*,*,#31661,.F.);
#41344=ORIENTED_EDGE('',*,*,#31667,.F.);
#41345=ORIENTED_EDGE('',*,*,#31668,.T.);
#41346=ORIENTED_EDGE('',*,*,#31669,.T.);
#41347=ORIENTED_EDGE('',*,*,#31665,.F.);
#41348=ORIENTED_EDGE('',*,*,#31670,.F.);
#41349=ORIENTED_EDGE('',*,*,#31671,.T.);
#41350=ORIENTED_EDGE('',*,*,#31672,.T.);
#41351=ORIENTED_EDGE('',*,*,#31668,.F.);
#41352=ORIENTED_EDGE('',*,*,#31673,.F.);
#41353=ORIENTED_EDGE('',*,*,#31674,.T.);
#41354=ORIENTED_EDGE('',*,*,#31675,.T.);
#41355=ORIENTED_EDGE('',*,*,#31671,.F.);
#41356=ORIENTED_EDGE('',*,*,#31676,.F.);
#41357=ORIENTED_EDGE('',*,*,#31677,.T.);
#41358=ORIENTED_EDGE('',*,*,#31678,.T.);
#41359=ORIENTED_EDGE('',*,*,#31674,.F.);
#41360=ORIENTED_EDGE('',*,*,#31679,.F.);
#41361=ORIENTED_EDGE('',*,*,#31680,.T.);
#41362=ORIENTED_EDGE('',*,*,#31681,.T.);
#41363=ORIENTED_EDGE('',*,*,#31677,.F.);
#41364=ORIENTED_EDGE('',*,*,#31682,.F.);
#41365=ORIENTED_EDGE('',*,*,#31683,.T.);
#41366=ORIENTED_EDGE('',*,*,#31684,.T.);
#41367=ORIENTED_EDGE('',*,*,#31680,.F.);
#41368=ORIENTED_EDGE('',*,*,#31685,.F.);
#41369=ORIENTED_EDGE('',*,*,#31686,.T.);
#41370=ORIENTED_EDGE('',*,*,#31687,.T.);
#41371=ORIENTED_EDGE('',*,*,#31683,.F.);
#41372=ORIENTED_EDGE('',*,*,#31688,.F.);
#41373=ORIENTED_EDGE('',*,*,#31689,.T.);
#41374=ORIENTED_EDGE('',*,*,#31690,.T.);
#41375=ORIENTED_EDGE('',*,*,#31686,.F.);
#41376=ORIENTED_EDGE('',*,*,#31691,.F.);
#41377=ORIENTED_EDGE('',*,*,#31692,.T.);
#41378=ORIENTED_EDGE('',*,*,#31693,.T.);
#41379=ORIENTED_EDGE('',*,*,#31689,.F.);
#41380=ORIENTED_EDGE('',*,*,#31694,.F.);
#41381=ORIENTED_EDGE('',*,*,#31663,.T.);
#41382=ORIENTED_EDGE('',*,*,#31695,.T.);
#41383=ORIENTED_EDGE('',*,*,#31692,.F.);
#41384=ORIENTED_EDGE('',*,*,#31695,.F.);
#41385=ORIENTED_EDGE('',*,*,#31662,.F.);
#41386=ORIENTED_EDGE('',*,*,#31666,.F.);
#41387=ORIENTED_EDGE('',*,*,#31669,.F.);
#41388=ORIENTED_EDGE('',*,*,#31672,.F.);
#41389=ORIENTED_EDGE('',*,*,#31675,.F.);
#41390=ORIENTED_EDGE('',*,*,#31678,.F.);
#41391=ORIENTED_EDGE('',*,*,#31681,.F.);
#41392=ORIENTED_EDGE('',*,*,#31684,.F.);
#41393=ORIENTED_EDGE('',*,*,#31687,.F.);
#41394=ORIENTED_EDGE('',*,*,#31690,.F.);
#41395=ORIENTED_EDGE('',*,*,#31693,.F.);
#41396=ORIENTED_EDGE('',*,*,#31659,.F.);
#41397=ORIENTED_EDGE('',*,*,#31638,.F.);
#41398=ORIENTED_EDGE('',*,*,#31642,.F.);
#41399=ORIENTED_EDGE('',*,*,#31645,.F.);
#41400=ORIENTED_EDGE('',*,*,#31648,.F.);
#41401=ORIENTED_EDGE('',*,*,#31651,.F.);
#41402=ORIENTED_EDGE('',*,*,#31654,.F.);
#41403=ORIENTED_EDGE('',*,*,#31657,.F.);
#41404=ORIENTED_EDGE('',*,*,#31696,.F.);
#41405=ORIENTED_EDGE('',*,*,#31697,.T.);
#41406=ORIENTED_EDGE('',*,*,#31698,.T.);
#41407=ORIENTED_EDGE('',*,*,#31699,.F.);
#41408=ORIENTED_EDGE('',*,*,#31700,.F.);
#41409=ORIENTED_EDGE('',*,*,#31701,.T.);
#41410=ORIENTED_EDGE('',*,*,#31702,.T.);
#41411=ORIENTED_EDGE('',*,*,#31697,.F.);
#41412=ORIENTED_EDGE('',*,*,#31703,.F.);
#41413=ORIENTED_EDGE('',*,*,#31704,.T.);
#41414=ORIENTED_EDGE('',*,*,#31705,.T.);
#41415=ORIENTED_EDGE('',*,*,#31701,.F.);
#41416=ORIENTED_EDGE('',*,*,#31706,.F.);
#41417=ORIENTED_EDGE('',*,*,#31707,.T.);
#41418=ORIENTED_EDGE('',*,*,#31708,.T.);
#41419=ORIENTED_EDGE('',*,*,#31704,.F.);
#41420=ORIENTED_EDGE('',*,*,#31709,.F.);
#41421=ORIENTED_EDGE('',*,*,#31710,.T.);
#41422=ORIENTED_EDGE('',*,*,#31711,.T.);
#41423=ORIENTED_EDGE('',*,*,#31707,.F.);
#41424=ORIENTED_EDGE('',*,*,#31712,.F.);
#41425=ORIENTED_EDGE('',*,*,#31713,.T.);
#41426=ORIENTED_EDGE('',*,*,#31714,.T.);
#41427=ORIENTED_EDGE('',*,*,#31710,.F.);
#41428=ORIENTED_EDGE('',*,*,#31715,.F.);
#41429=ORIENTED_EDGE('',*,*,#31716,.T.);
#41430=ORIENTED_EDGE('',*,*,#31717,.T.);
#41431=ORIENTED_EDGE('',*,*,#31713,.F.);
#41432=ORIENTED_EDGE('',*,*,#31718,.F.);
#41433=ORIENTED_EDGE('',*,*,#31719,.T.);
#41434=ORIENTED_EDGE('',*,*,#31720,.T.);
#41435=ORIENTED_EDGE('',*,*,#31716,.F.);
#41436=ORIENTED_EDGE('',*,*,#31721,.F.);
#41437=ORIENTED_EDGE('',*,*,#31722,.T.);
#41438=ORIENTED_EDGE('',*,*,#31723,.T.);
#41439=ORIENTED_EDGE('',*,*,#31719,.F.);
#41440=ORIENTED_EDGE('',*,*,#31724,.F.);
#41441=ORIENTED_EDGE('',*,*,#31725,.T.);
#41442=ORIENTED_EDGE('',*,*,#31726,.T.);
#41443=ORIENTED_EDGE('',*,*,#31722,.F.);
#41444=ORIENTED_EDGE('',*,*,#31727,.F.);
#41445=ORIENTED_EDGE('',*,*,#31728,.T.);
#41446=ORIENTED_EDGE('',*,*,#31729,.T.);
#41447=ORIENTED_EDGE('',*,*,#31725,.F.);
#41448=ORIENTED_EDGE('',*,*,#31730,.F.);
#41449=ORIENTED_EDGE('',*,*,#31731,.T.);
#41450=ORIENTED_EDGE('',*,*,#31732,.T.);
#41451=ORIENTED_EDGE('',*,*,#31728,.F.);
#41452=ORIENTED_EDGE('',*,*,#31733,.F.);
#41453=ORIENTED_EDGE('',*,*,#31734,.T.);
#41454=ORIENTED_EDGE('',*,*,#31735,.T.);
#41455=ORIENTED_EDGE('',*,*,#31731,.F.);
#41456=ORIENTED_EDGE('',*,*,#31736,.F.);
#41457=ORIENTED_EDGE('',*,*,#31737,.T.);
#41458=ORIENTED_EDGE('',*,*,#31738,.T.);
#41459=ORIENTED_EDGE('',*,*,#31734,.F.);
#41460=ORIENTED_EDGE('',*,*,#31739,.F.);
#41461=ORIENTED_EDGE('',*,*,#31740,.T.);
#41462=ORIENTED_EDGE('',*,*,#31741,.T.);
#41463=ORIENTED_EDGE('',*,*,#31737,.F.);
#41464=ORIENTED_EDGE('',*,*,#31742,.F.);
#41465=ORIENTED_EDGE('',*,*,#31743,.T.);
#41466=ORIENTED_EDGE('',*,*,#31744,.T.);
#41467=ORIENTED_EDGE('',*,*,#31740,.F.);
#41468=ORIENTED_EDGE('',*,*,#31745,.F.);
#41469=ORIENTED_EDGE('',*,*,#31746,.T.);
#41470=ORIENTED_EDGE('',*,*,#31747,.T.);
#41471=ORIENTED_EDGE('',*,*,#31743,.F.);
#41472=ORIENTED_EDGE('',*,*,#31748,.F.);
#41473=ORIENTED_EDGE('',*,*,#31749,.T.);
#41474=ORIENTED_EDGE('',*,*,#31750,.T.);
#41475=ORIENTED_EDGE('',*,*,#31746,.F.);
#41476=ORIENTED_EDGE('',*,*,#31751,.F.);
#41477=ORIENTED_EDGE('',*,*,#31752,.T.);
#41478=ORIENTED_EDGE('',*,*,#31753,.T.);
#41479=ORIENTED_EDGE('',*,*,#31749,.F.);
#41480=ORIENTED_EDGE('',*,*,#31754,.F.);
#41481=ORIENTED_EDGE('',*,*,#31755,.T.);
#41482=ORIENTED_EDGE('',*,*,#31756,.T.);
#41483=ORIENTED_EDGE('',*,*,#31752,.F.);
#41484=ORIENTED_EDGE('',*,*,#31757,.F.);
#41485=ORIENTED_EDGE('',*,*,#31758,.T.);
#41486=ORIENTED_EDGE('',*,*,#31759,.T.);
#41487=ORIENTED_EDGE('',*,*,#31755,.F.);
#41488=ORIENTED_EDGE('',*,*,#31760,.F.);
#41489=ORIENTED_EDGE('',*,*,#31699,.T.);
#41490=ORIENTED_EDGE('',*,*,#31761,.T.);
#41491=ORIENTED_EDGE('',*,*,#31758,.F.);
#41492=ORIENTED_EDGE('',*,*,#31761,.F.);
#41493=ORIENTED_EDGE('',*,*,#31698,.F.);
#41494=ORIENTED_EDGE('',*,*,#31702,.F.);
#41495=ORIENTED_EDGE('',*,*,#31705,.F.);
#41496=ORIENTED_EDGE('',*,*,#31708,.F.);
#41497=ORIENTED_EDGE('',*,*,#31711,.F.);
#41498=ORIENTED_EDGE('',*,*,#31714,.F.);
#41499=ORIENTED_EDGE('',*,*,#31717,.F.);
#41500=ORIENTED_EDGE('',*,*,#31720,.F.);
#41501=ORIENTED_EDGE('',*,*,#31723,.F.);
#41502=ORIENTED_EDGE('',*,*,#31726,.F.);
#41503=ORIENTED_EDGE('',*,*,#31729,.F.);
#41504=ORIENTED_EDGE('',*,*,#31732,.F.);
#41505=ORIENTED_EDGE('',*,*,#31735,.F.);
#41506=ORIENTED_EDGE('',*,*,#31738,.F.);
#41507=ORIENTED_EDGE('',*,*,#31741,.F.);
#41508=ORIENTED_EDGE('',*,*,#31744,.F.);
#41509=ORIENTED_EDGE('',*,*,#31747,.F.);
#41510=ORIENTED_EDGE('',*,*,#31750,.F.);
#41511=ORIENTED_EDGE('',*,*,#31753,.F.);
#41512=ORIENTED_EDGE('',*,*,#31756,.F.);
#41513=ORIENTED_EDGE('',*,*,#31759,.F.);
#41514=ORIENTED_EDGE('',*,*,#31636,.T.);
#41515=ORIENTED_EDGE('',*,*,#31658,.T.);
#41516=ORIENTED_EDGE('',*,*,#31655,.T.);
#41517=ORIENTED_EDGE('',*,*,#31652,.T.);
#41518=ORIENTED_EDGE('',*,*,#31649,.T.);
#41519=ORIENTED_EDGE('',*,*,#31646,.T.);
#41520=ORIENTED_EDGE('',*,*,#31643,.T.);
#41521=ORIENTED_EDGE('',*,*,#31640,.T.);
#41522=ORIENTED_EDGE('',*,*,#31762,.F.);
#41523=ORIENTED_EDGE('',*,*,#31763,.T.);
#41524=ORIENTED_EDGE('',*,*,#31764,.T.);
#41525=ORIENTED_EDGE('',*,*,#31765,.F.);
#41526=ORIENTED_EDGE('',*,*,#31766,.F.);
#41527=ORIENTED_EDGE('',*,*,#31767,.T.);
#41528=ORIENTED_EDGE('',*,*,#31768,.T.);
#41529=ORIENTED_EDGE('',*,*,#31763,.F.);
#41530=ORIENTED_EDGE('',*,*,#31769,.F.);
#41531=ORIENTED_EDGE('',*,*,#31770,.T.);
#41532=ORIENTED_EDGE('',*,*,#31771,.T.);
#41533=ORIENTED_EDGE('',*,*,#31767,.F.);
#41534=ORIENTED_EDGE('',*,*,#31772,.F.);
#41535=ORIENTED_EDGE('',*,*,#31773,.T.);
#41536=ORIENTED_EDGE('',*,*,#31774,.T.);
#41537=ORIENTED_EDGE('',*,*,#31770,.F.);
#41538=ORIENTED_EDGE('',*,*,#31775,.F.);
#41539=ORIENTED_EDGE('',*,*,#31776,.T.);
#41540=ORIENTED_EDGE('',*,*,#31777,.T.);
#41541=ORIENTED_EDGE('',*,*,#31773,.F.);
#41542=ORIENTED_EDGE('',*,*,#31778,.F.);
#41543=ORIENTED_EDGE('',*,*,#31779,.T.);
#41544=ORIENTED_EDGE('',*,*,#31780,.T.);
#41545=ORIENTED_EDGE('',*,*,#31776,.F.);
#41546=ORIENTED_EDGE('',*,*,#31781,.F.);
#41547=ORIENTED_EDGE('',*,*,#31782,.T.);
#41548=ORIENTED_EDGE('',*,*,#31783,.T.);
#41549=ORIENTED_EDGE('',*,*,#31779,.F.);
#41550=ORIENTED_EDGE('',*,*,#31784,.F.);
#41551=ORIENTED_EDGE('',*,*,#31765,.T.);
#41552=ORIENTED_EDGE('',*,*,#31785,.T.);
#41553=ORIENTED_EDGE('',*,*,#31782,.F.);
#41554=ORIENTED_EDGE('',*,*,#31786,.F.);
#41555=ORIENTED_EDGE('',*,*,#31787,.T.);
#41556=ORIENTED_EDGE('',*,*,#31788,.T.);
#41557=ORIENTED_EDGE('',*,*,#31789,.F.);
#41558=ORIENTED_EDGE('',*,*,#31790,.F.);
#41559=ORIENTED_EDGE('',*,*,#31791,.T.);
#41560=ORIENTED_EDGE('',*,*,#31792,.T.);
#41561=ORIENTED_EDGE('',*,*,#31787,.F.);
#41562=ORIENTED_EDGE('',*,*,#31793,.F.);
#41563=ORIENTED_EDGE('',*,*,#31794,.T.);
#41564=ORIENTED_EDGE('',*,*,#31795,.T.);
#41565=ORIENTED_EDGE('',*,*,#31791,.F.);
#41566=ORIENTED_EDGE('',*,*,#31796,.F.);
#41567=ORIENTED_EDGE('',*,*,#31797,.T.);
#41568=ORIENTED_EDGE('',*,*,#31798,.T.);
#41569=ORIENTED_EDGE('',*,*,#31794,.F.);
#41570=ORIENTED_EDGE('',*,*,#31799,.F.);
#41571=ORIENTED_EDGE('',*,*,#31800,.T.);
#41572=ORIENTED_EDGE('',*,*,#31801,.T.);
#41573=ORIENTED_EDGE('',*,*,#31797,.F.);
#41574=ORIENTED_EDGE('',*,*,#31802,.F.);
#41575=ORIENTED_EDGE('',*,*,#31803,.T.);
#41576=ORIENTED_EDGE('',*,*,#31804,.T.);
#41577=ORIENTED_EDGE('',*,*,#31800,.F.);
#41578=ORIENTED_EDGE('',*,*,#31805,.F.);
#41579=ORIENTED_EDGE('',*,*,#31806,.T.);
#41580=ORIENTED_EDGE('',*,*,#31807,.T.);
#41581=ORIENTED_EDGE('',*,*,#31803,.F.);
#41582=ORIENTED_EDGE('',*,*,#31808,.F.);
#41583=ORIENTED_EDGE('',*,*,#31809,.T.);
#41584=ORIENTED_EDGE('',*,*,#31810,.T.);
#41585=ORIENTED_EDGE('',*,*,#31806,.F.);
#41586=ORIENTED_EDGE('',*,*,#31811,.F.);
#41587=ORIENTED_EDGE('',*,*,#31812,.T.);
#41588=ORIENTED_EDGE('',*,*,#31813,.T.);
#41589=ORIENTED_EDGE('',*,*,#31809,.F.);
#41590=ORIENTED_EDGE('',*,*,#31814,.F.);
#41591=ORIENTED_EDGE('',*,*,#31815,.T.);
#41592=ORIENTED_EDGE('',*,*,#31816,.T.);
#41593=ORIENTED_EDGE('',*,*,#31812,.F.);
#41594=ORIENTED_EDGE('',*,*,#31817,.F.);
#41595=ORIENTED_EDGE('',*,*,#31818,.T.);
#41596=ORIENTED_EDGE('',*,*,#31819,.T.);
#41597=ORIENTED_EDGE('',*,*,#31815,.F.);
#41598=ORIENTED_EDGE('',*,*,#31820,.F.);
#41599=ORIENTED_EDGE('',*,*,#31789,.T.);
#41600=ORIENTED_EDGE('',*,*,#31821,.T.);
#41601=ORIENTED_EDGE('',*,*,#31818,.F.);
#41602=ORIENTED_EDGE('',*,*,#31821,.F.);
#41603=ORIENTED_EDGE('',*,*,#31788,.F.);
#41604=ORIENTED_EDGE('',*,*,#31792,.F.);
#41605=ORIENTED_EDGE('',*,*,#31795,.F.);
#41606=ORIENTED_EDGE('',*,*,#31798,.F.);
#41607=ORIENTED_EDGE('',*,*,#31801,.F.);
#41608=ORIENTED_EDGE('',*,*,#31804,.F.);
#41609=ORIENTED_EDGE('',*,*,#31807,.F.);
#41610=ORIENTED_EDGE('',*,*,#31810,.F.);
#41611=ORIENTED_EDGE('',*,*,#31813,.F.);
#41612=ORIENTED_EDGE('',*,*,#31816,.F.);
#41613=ORIENTED_EDGE('',*,*,#31819,.F.);
#41614=ORIENTED_EDGE('',*,*,#31785,.F.);
#41615=ORIENTED_EDGE('',*,*,#31764,.F.);
#41616=ORIENTED_EDGE('',*,*,#31768,.F.);
#41617=ORIENTED_EDGE('',*,*,#31771,.F.);
#41618=ORIENTED_EDGE('',*,*,#31774,.F.);
#41619=ORIENTED_EDGE('',*,*,#31777,.F.);
#41620=ORIENTED_EDGE('',*,*,#31780,.F.);
#41621=ORIENTED_EDGE('',*,*,#31783,.F.);
#41622=ORIENTED_EDGE('',*,*,#31822,.F.);
#41623=ORIENTED_EDGE('',*,*,#31823,.T.);
#41624=ORIENTED_EDGE('',*,*,#31824,.T.);
#41625=ORIENTED_EDGE('',*,*,#31825,.F.);
#41626=ORIENTED_EDGE('',*,*,#31826,.F.);
#41627=ORIENTED_EDGE('',*,*,#31827,.T.);
#41628=ORIENTED_EDGE('',*,*,#31828,.T.);
#41629=ORIENTED_EDGE('',*,*,#31823,.F.);
#41630=ORIENTED_EDGE('',*,*,#31829,.F.);
#41631=ORIENTED_EDGE('',*,*,#31830,.T.);
#41632=ORIENTED_EDGE('',*,*,#31831,.T.);
#41633=ORIENTED_EDGE('',*,*,#31827,.F.);
#41634=ORIENTED_EDGE('',*,*,#31832,.F.);
#41635=ORIENTED_EDGE('',*,*,#31833,.T.);
#41636=ORIENTED_EDGE('',*,*,#31834,.T.);
#41637=ORIENTED_EDGE('',*,*,#31830,.F.);
#41638=ORIENTED_EDGE('',*,*,#31835,.F.);
#41639=ORIENTED_EDGE('',*,*,#31836,.T.);
#41640=ORIENTED_EDGE('',*,*,#31837,.T.);
#41641=ORIENTED_EDGE('',*,*,#31833,.F.);
#41642=ORIENTED_EDGE('',*,*,#31838,.F.);
#41643=ORIENTED_EDGE('',*,*,#31839,.T.);
#41644=ORIENTED_EDGE('',*,*,#31840,.T.);
#41645=ORIENTED_EDGE('',*,*,#31836,.F.);
#41646=ORIENTED_EDGE('',*,*,#31841,.F.);
#41647=ORIENTED_EDGE('',*,*,#31842,.T.);
#41648=ORIENTED_EDGE('',*,*,#31843,.T.);
#41649=ORIENTED_EDGE('',*,*,#31839,.F.);
#41650=ORIENTED_EDGE('',*,*,#31844,.F.);
#41651=ORIENTED_EDGE('',*,*,#31845,.T.);
#41652=ORIENTED_EDGE('',*,*,#31846,.T.);
#41653=ORIENTED_EDGE('',*,*,#31842,.F.);
#41654=ORIENTED_EDGE('',*,*,#31847,.F.);
#41655=ORIENTED_EDGE('',*,*,#31848,.T.);
#41656=ORIENTED_EDGE('',*,*,#31849,.T.);
#41657=ORIENTED_EDGE('',*,*,#31845,.F.);
#41658=ORIENTED_EDGE('',*,*,#31850,.F.);
#41659=ORIENTED_EDGE('',*,*,#31851,.T.);
#41660=ORIENTED_EDGE('',*,*,#31852,.T.);
#41661=ORIENTED_EDGE('',*,*,#31848,.F.);
#41662=ORIENTED_EDGE('',*,*,#31853,.F.);
#41663=ORIENTED_EDGE('',*,*,#31854,.T.);
#41664=ORIENTED_EDGE('',*,*,#31855,.T.);
#41665=ORIENTED_EDGE('',*,*,#31851,.F.);
#41666=ORIENTED_EDGE('',*,*,#31856,.F.);
#41667=ORIENTED_EDGE('',*,*,#31857,.T.);
#41668=ORIENTED_EDGE('',*,*,#31858,.T.);
#41669=ORIENTED_EDGE('',*,*,#31854,.F.);
#41670=ORIENTED_EDGE('',*,*,#31859,.F.);
#41671=ORIENTED_EDGE('',*,*,#31860,.T.);
#41672=ORIENTED_EDGE('',*,*,#31861,.T.);
#41673=ORIENTED_EDGE('',*,*,#31857,.F.);
#41674=ORIENTED_EDGE('',*,*,#31862,.F.);
#41675=ORIENTED_EDGE('',*,*,#31863,.T.);
#41676=ORIENTED_EDGE('',*,*,#31864,.T.);
#41677=ORIENTED_EDGE('',*,*,#31860,.F.);
#41678=ORIENTED_EDGE('',*,*,#31865,.F.);
#41679=ORIENTED_EDGE('',*,*,#31866,.T.);
#41680=ORIENTED_EDGE('',*,*,#31867,.T.);
#41681=ORIENTED_EDGE('',*,*,#31863,.F.);
#41682=ORIENTED_EDGE('',*,*,#31868,.F.);
#41683=ORIENTED_EDGE('',*,*,#31869,.T.);
#41684=ORIENTED_EDGE('',*,*,#31870,.T.);
#41685=ORIENTED_EDGE('',*,*,#31866,.F.);
#41686=ORIENTED_EDGE('',*,*,#31871,.F.);
#41687=ORIENTED_EDGE('',*,*,#31872,.T.);
#41688=ORIENTED_EDGE('',*,*,#31873,.T.);
#41689=ORIENTED_EDGE('',*,*,#31869,.F.);
#41690=ORIENTED_EDGE('',*,*,#31874,.F.);
#41691=ORIENTED_EDGE('',*,*,#31875,.T.);
#41692=ORIENTED_EDGE('',*,*,#31876,.T.);
#41693=ORIENTED_EDGE('',*,*,#31872,.F.);
#41694=ORIENTED_EDGE('',*,*,#31877,.F.);
#41695=ORIENTED_EDGE('',*,*,#31878,.T.);
#41696=ORIENTED_EDGE('',*,*,#31879,.T.);
#41697=ORIENTED_EDGE('',*,*,#31875,.F.);
#41698=ORIENTED_EDGE('',*,*,#31880,.F.);
#41699=ORIENTED_EDGE('',*,*,#31881,.T.);
#41700=ORIENTED_EDGE('',*,*,#31882,.T.);
#41701=ORIENTED_EDGE('',*,*,#31878,.F.);
#41702=ORIENTED_EDGE('',*,*,#31883,.F.);
#41703=ORIENTED_EDGE('',*,*,#31884,.T.);
#41704=ORIENTED_EDGE('',*,*,#31885,.T.);
#41705=ORIENTED_EDGE('',*,*,#31881,.F.);
#41706=ORIENTED_EDGE('',*,*,#31886,.F.);
#41707=ORIENTED_EDGE('',*,*,#31887,.T.);
#41708=ORIENTED_EDGE('',*,*,#31888,.T.);
#41709=ORIENTED_EDGE('',*,*,#31884,.F.);
#41710=ORIENTED_EDGE('',*,*,#31889,.F.);
#41711=ORIENTED_EDGE('',*,*,#31890,.T.);
#41712=ORIENTED_EDGE('',*,*,#31891,.T.);
#41713=ORIENTED_EDGE('',*,*,#31887,.F.);
#41714=ORIENTED_EDGE('',*,*,#31892,.F.);
#41715=ORIENTED_EDGE('',*,*,#31893,.T.);
#41716=ORIENTED_EDGE('',*,*,#31894,.T.);
#41717=ORIENTED_EDGE('',*,*,#31890,.F.);
#41718=ORIENTED_EDGE('',*,*,#31895,.F.);
#41719=ORIENTED_EDGE('',*,*,#31896,.T.);
#41720=ORIENTED_EDGE('',*,*,#31897,.T.);
#41721=ORIENTED_EDGE('',*,*,#31893,.F.);
#41722=ORIENTED_EDGE('',*,*,#31898,.F.);
#41723=ORIENTED_EDGE('',*,*,#31899,.T.);
#41724=ORIENTED_EDGE('',*,*,#31900,.T.);
#41725=ORIENTED_EDGE('',*,*,#31896,.F.);
#41726=ORIENTED_EDGE('',*,*,#31901,.F.);
#41727=ORIENTED_EDGE('',*,*,#31902,.T.);
#41728=ORIENTED_EDGE('',*,*,#31903,.T.);
#41729=ORIENTED_EDGE('',*,*,#31899,.F.);
#41730=ORIENTED_EDGE('',*,*,#31904,.F.);
#41731=ORIENTED_EDGE('',*,*,#31905,.T.);
#41732=ORIENTED_EDGE('',*,*,#31906,.T.);
#41733=ORIENTED_EDGE('',*,*,#31902,.F.);
#41734=ORIENTED_EDGE('',*,*,#31907,.F.);
#41735=ORIENTED_EDGE('',*,*,#31908,.T.);
#41736=ORIENTED_EDGE('',*,*,#31909,.T.);
#41737=ORIENTED_EDGE('',*,*,#31905,.F.);
#41738=ORIENTED_EDGE('',*,*,#31910,.F.);
#41739=ORIENTED_EDGE('',*,*,#31825,.T.);
#41740=ORIENTED_EDGE('',*,*,#31911,.T.);
#41741=ORIENTED_EDGE('',*,*,#31908,.F.);
#41742=ORIENTED_EDGE('',*,*,#31911,.F.);
#41743=ORIENTED_EDGE('',*,*,#31824,.F.);
#41744=ORIENTED_EDGE('',*,*,#31828,.F.);
#41745=ORIENTED_EDGE('',*,*,#31831,.F.);
#41746=ORIENTED_EDGE('',*,*,#31834,.F.);
#41747=ORIENTED_EDGE('',*,*,#31837,.F.);
#41748=ORIENTED_EDGE('',*,*,#31840,.F.);
#41749=ORIENTED_EDGE('',*,*,#31843,.F.);
#41750=ORIENTED_EDGE('',*,*,#31846,.F.);
#41751=ORIENTED_EDGE('',*,*,#31849,.F.);
#41752=ORIENTED_EDGE('',*,*,#31852,.F.);
#41753=ORIENTED_EDGE('',*,*,#31855,.F.);
#41754=ORIENTED_EDGE('',*,*,#31858,.F.);
#41755=ORIENTED_EDGE('',*,*,#31861,.F.);
#41756=ORIENTED_EDGE('',*,*,#31864,.F.);
#41757=ORIENTED_EDGE('',*,*,#31867,.F.);
#41758=ORIENTED_EDGE('',*,*,#31870,.F.);
#41759=ORIENTED_EDGE('',*,*,#31873,.F.);
#41760=ORIENTED_EDGE('',*,*,#31876,.F.);
#41761=ORIENTED_EDGE('',*,*,#31879,.F.);
#41762=ORIENTED_EDGE('',*,*,#31882,.F.);
#41763=ORIENTED_EDGE('',*,*,#31885,.F.);
#41764=ORIENTED_EDGE('',*,*,#31888,.F.);
#41765=ORIENTED_EDGE('',*,*,#31891,.F.);
#41766=ORIENTED_EDGE('',*,*,#31894,.F.);
#41767=ORIENTED_EDGE('',*,*,#31897,.F.);
#41768=ORIENTED_EDGE('',*,*,#31900,.F.);
#41769=ORIENTED_EDGE('',*,*,#31903,.F.);
#41770=ORIENTED_EDGE('',*,*,#31906,.F.);
#41771=ORIENTED_EDGE('',*,*,#31909,.F.);
#41772=ORIENTED_EDGE('',*,*,#31762,.T.);
#41773=ORIENTED_EDGE('',*,*,#31784,.T.);
#41774=ORIENTED_EDGE('',*,*,#31781,.T.);
#41775=ORIENTED_EDGE('',*,*,#31778,.T.);
#41776=ORIENTED_EDGE('',*,*,#31775,.T.);
#41777=ORIENTED_EDGE('',*,*,#31772,.T.);
#41778=ORIENTED_EDGE('',*,*,#31769,.T.);
#41779=ORIENTED_EDGE('',*,*,#31766,.T.);
#41780=ORIENTED_EDGE('',*,*,#31912,.F.);
#41781=ORIENTED_EDGE('',*,*,#31913,.T.);
#41782=ORIENTED_EDGE('',*,*,#31914,.T.);
#41783=ORIENTED_EDGE('',*,*,#31915,.F.);
#41784=ORIENTED_EDGE('',*,*,#31916,.F.);
#41785=ORIENTED_EDGE('',*,*,#31917,.T.);
#41786=ORIENTED_EDGE('',*,*,#31918,.T.);
#41787=ORIENTED_EDGE('',*,*,#31913,.F.);
#41788=ORIENTED_EDGE('',*,*,#31919,.F.);
#41789=ORIENTED_EDGE('',*,*,#31920,.T.);
#41790=ORIENTED_EDGE('',*,*,#31921,.T.);
#41791=ORIENTED_EDGE('',*,*,#31917,.F.);
#41792=ORIENTED_EDGE('',*,*,#31922,.F.);
#41793=ORIENTED_EDGE('',*,*,#31923,.T.);
#41794=ORIENTED_EDGE('',*,*,#31924,.T.);
#41795=ORIENTED_EDGE('',*,*,#31920,.F.);
#41796=ORIENTED_EDGE('',*,*,#31925,.F.);
#41797=ORIENTED_EDGE('',*,*,#31926,.T.);
#41798=ORIENTED_EDGE('',*,*,#31927,.T.);
#41799=ORIENTED_EDGE('',*,*,#31923,.F.);
#41800=ORIENTED_EDGE('',*,*,#31928,.F.);
#41801=ORIENTED_EDGE('',*,*,#31929,.T.);
#41802=ORIENTED_EDGE('',*,*,#31930,.T.);
#41803=ORIENTED_EDGE('',*,*,#31926,.F.);
#41804=ORIENTED_EDGE('',*,*,#31931,.F.);
#41805=ORIENTED_EDGE('',*,*,#31932,.T.);
#41806=ORIENTED_EDGE('',*,*,#31933,.T.);
#41807=ORIENTED_EDGE('',*,*,#31929,.F.);
#41808=ORIENTED_EDGE('',*,*,#31934,.F.);
#41809=ORIENTED_EDGE('',*,*,#31915,.T.);
#41810=ORIENTED_EDGE('',*,*,#31935,.T.);
#41811=ORIENTED_EDGE('',*,*,#31932,.F.);
#41812=ORIENTED_EDGE('',*,*,#31936,.F.);
#41813=ORIENTED_EDGE('',*,*,#31937,.T.);
#41814=ORIENTED_EDGE('',*,*,#31938,.T.);
#41815=ORIENTED_EDGE('',*,*,#31939,.F.);
#41816=ORIENTED_EDGE('',*,*,#31940,.F.);
#41817=ORIENTED_EDGE('',*,*,#31941,.T.);
#41818=ORIENTED_EDGE('',*,*,#31942,.T.);
#41819=ORIENTED_EDGE('',*,*,#31937,.F.);
#41820=ORIENTED_EDGE('',*,*,#31943,.F.);
#41821=ORIENTED_EDGE('',*,*,#31944,.T.);
#41822=ORIENTED_EDGE('',*,*,#31945,.T.);
#41823=ORIENTED_EDGE('',*,*,#31941,.F.);
#41824=ORIENTED_EDGE('',*,*,#31946,.F.);
#41825=ORIENTED_EDGE('',*,*,#31947,.T.);
#41826=ORIENTED_EDGE('',*,*,#31948,.T.);
#41827=ORIENTED_EDGE('',*,*,#31944,.F.);
#41828=ORIENTED_EDGE('',*,*,#31949,.F.);
#41829=ORIENTED_EDGE('',*,*,#31950,.T.);
#41830=ORIENTED_EDGE('',*,*,#31951,.T.);
#41831=ORIENTED_EDGE('',*,*,#31947,.F.);
#41832=ORIENTED_EDGE('',*,*,#31952,.F.);
#41833=ORIENTED_EDGE('',*,*,#31953,.T.);
#41834=ORIENTED_EDGE('',*,*,#31954,.T.);
#41835=ORIENTED_EDGE('',*,*,#31950,.F.);
#41836=ORIENTED_EDGE('',*,*,#31955,.F.);
#41837=ORIENTED_EDGE('',*,*,#31956,.T.);
#41838=ORIENTED_EDGE('',*,*,#31957,.T.);
#41839=ORIENTED_EDGE('',*,*,#31953,.F.);
#41840=ORIENTED_EDGE('',*,*,#31958,.F.);
#41841=ORIENTED_EDGE('',*,*,#31959,.T.);
#41842=ORIENTED_EDGE('',*,*,#31960,.T.);
#41843=ORIENTED_EDGE('',*,*,#31956,.F.);
#41844=ORIENTED_EDGE('',*,*,#31961,.F.);
#41845=ORIENTED_EDGE('',*,*,#31962,.T.);
#41846=ORIENTED_EDGE('',*,*,#31963,.T.);
#41847=ORIENTED_EDGE('',*,*,#31959,.F.);
#41848=ORIENTED_EDGE('',*,*,#31964,.F.);
#41849=ORIENTED_EDGE('',*,*,#31965,.T.);
#41850=ORIENTED_EDGE('',*,*,#31966,.T.);
#41851=ORIENTED_EDGE('',*,*,#31962,.F.);
#41852=ORIENTED_EDGE('',*,*,#31967,.F.);
#41853=ORIENTED_EDGE('',*,*,#31968,.T.);
#41854=ORIENTED_EDGE('',*,*,#31969,.T.);
#41855=ORIENTED_EDGE('',*,*,#31965,.F.);
#41856=ORIENTED_EDGE('',*,*,#31970,.F.);
#41857=ORIENTED_EDGE('',*,*,#31939,.T.);
#41858=ORIENTED_EDGE('',*,*,#31971,.T.);
#41859=ORIENTED_EDGE('',*,*,#31968,.F.);
#41860=ORIENTED_EDGE('',*,*,#31971,.F.);
#41861=ORIENTED_EDGE('',*,*,#31938,.F.);
#41862=ORIENTED_EDGE('',*,*,#31942,.F.);
#41863=ORIENTED_EDGE('',*,*,#31945,.F.);
#41864=ORIENTED_EDGE('',*,*,#31948,.F.);
#41865=ORIENTED_EDGE('',*,*,#31951,.F.);
#41866=ORIENTED_EDGE('',*,*,#31954,.F.);
#41867=ORIENTED_EDGE('',*,*,#31957,.F.);
#41868=ORIENTED_EDGE('',*,*,#31960,.F.);
#41869=ORIENTED_EDGE('',*,*,#31963,.F.);
#41870=ORIENTED_EDGE('',*,*,#31966,.F.);
#41871=ORIENTED_EDGE('',*,*,#31969,.F.);
#41872=ORIENTED_EDGE('',*,*,#31935,.F.);
#41873=ORIENTED_EDGE('',*,*,#31914,.F.);
#41874=ORIENTED_EDGE('',*,*,#31918,.F.);
#41875=ORIENTED_EDGE('',*,*,#31921,.F.);
#41876=ORIENTED_EDGE('',*,*,#31924,.F.);
#41877=ORIENTED_EDGE('',*,*,#31927,.F.);
#41878=ORIENTED_EDGE('',*,*,#31930,.F.);
#41879=ORIENTED_EDGE('',*,*,#31933,.F.);
#41880=ORIENTED_EDGE('',*,*,#31972,.F.);
#41881=ORIENTED_EDGE('',*,*,#31973,.T.);
#41882=ORIENTED_EDGE('',*,*,#31974,.T.);
#41883=ORIENTED_EDGE('',*,*,#31975,.F.);
#41884=ORIENTED_EDGE('',*,*,#31976,.F.);
#41885=ORIENTED_EDGE('',*,*,#31977,.T.);
#41886=ORIENTED_EDGE('',*,*,#31978,.T.);
#41887=ORIENTED_EDGE('',*,*,#31973,.F.);
#41888=ORIENTED_EDGE('',*,*,#31979,.F.);
#41889=ORIENTED_EDGE('',*,*,#31975,.T.);
#41890=ORIENTED_EDGE('',*,*,#31980,.T.);
#41891=ORIENTED_EDGE('',*,*,#31977,.F.);
#41892=ORIENTED_EDGE('',*,*,#31981,.F.);
#41893=ORIENTED_EDGE('',*,*,#31982,.T.);
#41894=ORIENTED_EDGE('',*,*,#31983,.T.);
#41895=ORIENTED_EDGE('',*,*,#31984,.F.);
#41896=ORIENTED_EDGE('',*,*,#31985,.F.);
#41897=ORIENTED_EDGE('',*,*,#31986,.T.);
#41898=ORIENTED_EDGE('',*,*,#31987,.T.);
#41899=ORIENTED_EDGE('',*,*,#31982,.F.);
#41900=ORIENTED_EDGE('',*,*,#31988,.F.);
#41901=ORIENTED_EDGE('',*,*,#31989,.T.);
#41902=ORIENTED_EDGE('',*,*,#31990,.T.);
#41903=ORIENTED_EDGE('',*,*,#31986,.F.);
#41904=ORIENTED_EDGE('',*,*,#31991,.F.);
#41905=ORIENTED_EDGE('',*,*,#31992,.T.);
#41906=ORIENTED_EDGE('',*,*,#31993,.T.);
#41907=ORIENTED_EDGE('',*,*,#31989,.F.);
#41908=ORIENTED_EDGE('',*,*,#31994,.F.);
#41909=ORIENTED_EDGE('',*,*,#31995,.T.);
#41910=ORIENTED_EDGE('',*,*,#31996,.T.);
#41911=ORIENTED_EDGE('',*,*,#31992,.F.);
#41912=ORIENTED_EDGE('',*,*,#31997,.F.);
#41913=ORIENTED_EDGE('',*,*,#31998,.T.);
#41914=ORIENTED_EDGE('',*,*,#31999,.T.);
#41915=ORIENTED_EDGE('',*,*,#31995,.F.);
#41916=ORIENTED_EDGE('',*,*,#32000,.F.);
#41917=ORIENTED_EDGE('',*,*,#32001,.T.);
#41918=ORIENTED_EDGE('',*,*,#32002,.T.);
#41919=ORIENTED_EDGE('',*,*,#31998,.F.);
#41920=ORIENTED_EDGE('',*,*,#32003,.F.);
#41921=ORIENTED_EDGE('',*,*,#32004,.T.);
#41922=ORIENTED_EDGE('',*,*,#32005,.T.);
#41923=ORIENTED_EDGE('',*,*,#32001,.F.);
#41924=ORIENTED_EDGE('',*,*,#32006,.F.);
#41925=ORIENTED_EDGE('',*,*,#32007,.T.);
#41926=ORIENTED_EDGE('',*,*,#32008,.T.);
#41927=ORIENTED_EDGE('',*,*,#32004,.F.);
#41928=ORIENTED_EDGE('',*,*,#32009,.F.);
#41929=ORIENTED_EDGE('',*,*,#32010,.T.);
#41930=ORIENTED_EDGE('',*,*,#32011,.T.);
#41931=ORIENTED_EDGE('',*,*,#32007,.F.);
#41932=ORIENTED_EDGE('',*,*,#32012,.F.);
#41933=ORIENTED_EDGE('',*,*,#31984,.T.);
#41934=ORIENTED_EDGE('',*,*,#32013,.T.);
#41935=ORIENTED_EDGE('',*,*,#32010,.F.);
#41936=ORIENTED_EDGE('',*,*,#32013,.F.);
#41937=ORIENTED_EDGE('',*,*,#31983,.F.);
#41938=ORIENTED_EDGE('',*,*,#31987,.F.);
#41939=ORIENTED_EDGE('',*,*,#31990,.F.);
#41940=ORIENTED_EDGE('',*,*,#31993,.F.);
#41941=ORIENTED_EDGE('',*,*,#31996,.F.);
#41942=ORIENTED_EDGE('',*,*,#31999,.F.);
#41943=ORIENTED_EDGE('',*,*,#32002,.F.);
#41944=ORIENTED_EDGE('',*,*,#32005,.F.);
#41945=ORIENTED_EDGE('',*,*,#32008,.F.);
#41946=ORIENTED_EDGE('',*,*,#32011,.F.);
#41947=ORIENTED_EDGE('',*,*,#31980,.F.);
#41948=ORIENTED_EDGE('',*,*,#31974,.F.);
#41949=ORIENTED_EDGE('',*,*,#31978,.F.);
#41950=ORIENTED_EDGE('',*,*,#31972,.T.);
#41951=ORIENTED_EDGE('',*,*,#31979,.T.);
#41952=ORIENTED_EDGE('',*,*,#31976,.T.);
#41953=ORIENTED_EDGE('',*,*,#31912,.T.);
#41954=ORIENTED_EDGE('',*,*,#31934,.T.);
#41955=ORIENTED_EDGE('',*,*,#31931,.T.);
#41956=ORIENTED_EDGE('',*,*,#31928,.T.);
#41957=ORIENTED_EDGE('',*,*,#31925,.T.);
#41958=ORIENTED_EDGE('',*,*,#31922,.T.);
#41959=ORIENTED_EDGE('',*,*,#31919,.T.);
#41960=ORIENTED_EDGE('',*,*,#31916,.T.);
#41961=ORIENTED_EDGE('',*,*,#32014,.F.);
#41962=ORIENTED_EDGE('',*,*,#32015,.T.);
#41963=ORIENTED_EDGE('',*,*,#32016,.T.);
#41964=ORIENTED_EDGE('',*,*,#32017,.F.);
#41965=ORIENTED_EDGE('',*,*,#32018,.F.);
#41966=ORIENTED_EDGE('',*,*,#32019,.T.);
#41967=ORIENTED_EDGE('',*,*,#32020,.T.);
#41968=ORIENTED_EDGE('',*,*,#32015,.F.);
#41969=ORIENTED_EDGE('',*,*,#32021,.F.);
#41970=ORIENTED_EDGE('',*,*,#32022,.T.);
#41971=ORIENTED_EDGE('',*,*,#32023,.T.);
#41972=ORIENTED_EDGE('',*,*,#32019,.F.);
#41973=ORIENTED_EDGE('',*,*,#32024,.F.);
#41974=ORIENTED_EDGE('',*,*,#32025,.T.);
#41975=ORIENTED_EDGE('',*,*,#32026,.T.);
#41976=ORIENTED_EDGE('',*,*,#32022,.F.);
#41977=ORIENTED_EDGE('',*,*,#32027,.F.);
#41978=ORIENTED_EDGE('',*,*,#32028,.T.);
#41979=ORIENTED_EDGE('',*,*,#32029,.T.);
#41980=ORIENTED_EDGE('',*,*,#32025,.F.);
#41981=ORIENTED_EDGE('',*,*,#32030,.F.);
#41982=ORIENTED_EDGE('',*,*,#32031,.T.);
#41983=ORIENTED_EDGE('',*,*,#32032,.T.);
#41984=ORIENTED_EDGE('',*,*,#32028,.F.);
#41985=ORIENTED_EDGE('',*,*,#32033,.F.);
#41986=ORIENTED_EDGE('',*,*,#32034,.T.);
#41987=ORIENTED_EDGE('',*,*,#32035,.T.);
#41988=ORIENTED_EDGE('',*,*,#32031,.F.);
#41989=ORIENTED_EDGE('',*,*,#32036,.F.);
#41990=ORIENTED_EDGE('',*,*,#32017,.T.);
#41991=ORIENTED_EDGE('',*,*,#32037,.T.);
#41992=ORIENTED_EDGE('',*,*,#32034,.F.);
#41993=ORIENTED_EDGE('',*,*,#32038,.F.);
#41994=ORIENTED_EDGE('',*,*,#32039,.T.);
#41995=ORIENTED_EDGE('',*,*,#32040,.T.);
#41996=ORIENTED_EDGE('',*,*,#32041,.F.);
#41997=ORIENTED_EDGE('',*,*,#32042,.F.);
#41998=ORIENTED_EDGE('',*,*,#32043,.T.);
#41999=ORIENTED_EDGE('',*,*,#32044,.T.);
#42000=ORIENTED_EDGE('',*,*,#32039,.F.);
#42001=ORIENTED_EDGE('',*,*,#32045,.F.);
#42002=ORIENTED_EDGE('',*,*,#32046,.T.);
#42003=ORIENTED_EDGE('',*,*,#32047,.T.);
#42004=ORIENTED_EDGE('',*,*,#32043,.F.);
#42005=ORIENTED_EDGE('',*,*,#32048,.F.);
#42006=ORIENTED_EDGE('',*,*,#32049,.T.);
#42007=ORIENTED_EDGE('',*,*,#32050,.T.);
#42008=ORIENTED_EDGE('',*,*,#32046,.F.);
#42009=ORIENTED_EDGE('',*,*,#32051,.F.);
#42010=ORIENTED_EDGE('',*,*,#32052,.T.);
#42011=ORIENTED_EDGE('',*,*,#32053,.T.);
#42012=ORIENTED_EDGE('',*,*,#32049,.F.);
#42013=ORIENTED_EDGE('',*,*,#32054,.F.);
#42014=ORIENTED_EDGE('',*,*,#32055,.T.);
#42015=ORIENTED_EDGE('',*,*,#32056,.T.);
#42016=ORIENTED_EDGE('',*,*,#32052,.F.);
#42017=ORIENTED_EDGE('',*,*,#32057,.F.);
#42018=ORIENTED_EDGE('',*,*,#32058,.T.);
#42019=ORIENTED_EDGE('',*,*,#32059,.T.);
#42020=ORIENTED_EDGE('',*,*,#32055,.F.);
#42021=ORIENTED_EDGE('',*,*,#32060,.F.);
#42022=ORIENTED_EDGE('',*,*,#32061,.T.);
#42023=ORIENTED_EDGE('',*,*,#32062,.T.);
#42024=ORIENTED_EDGE('',*,*,#32058,.F.);
#42025=ORIENTED_EDGE('',*,*,#32063,.F.);
#42026=ORIENTED_EDGE('',*,*,#32064,.T.);
#42027=ORIENTED_EDGE('',*,*,#32065,.T.);
#42028=ORIENTED_EDGE('',*,*,#32061,.F.);
#42029=ORIENTED_EDGE('',*,*,#32066,.F.);
#42030=ORIENTED_EDGE('',*,*,#32067,.T.);
#42031=ORIENTED_EDGE('',*,*,#32068,.T.);
#42032=ORIENTED_EDGE('',*,*,#32064,.F.);
#42033=ORIENTED_EDGE('',*,*,#32069,.F.);
#42034=ORIENTED_EDGE('',*,*,#32070,.T.);
#42035=ORIENTED_EDGE('',*,*,#32071,.T.);
#42036=ORIENTED_EDGE('',*,*,#32067,.F.);
#42037=ORIENTED_EDGE('',*,*,#32072,.F.);
#42038=ORIENTED_EDGE('',*,*,#32041,.T.);
#42039=ORIENTED_EDGE('',*,*,#32073,.T.);
#42040=ORIENTED_EDGE('',*,*,#32070,.F.);
#42041=ORIENTED_EDGE('',*,*,#32073,.F.);
#42042=ORIENTED_EDGE('',*,*,#32040,.F.);
#42043=ORIENTED_EDGE('',*,*,#32044,.F.);
#42044=ORIENTED_EDGE('',*,*,#32047,.F.);
#42045=ORIENTED_EDGE('',*,*,#32050,.F.);
#42046=ORIENTED_EDGE('',*,*,#32053,.F.);
#42047=ORIENTED_EDGE('',*,*,#32056,.F.);
#42048=ORIENTED_EDGE('',*,*,#32059,.F.);
#42049=ORIENTED_EDGE('',*,*,#32062,.F.);
#42050=ORIENTED_EDGE('',*,*,#32065,.F.);
#42051=ORIENTED_EDGE('',*,*,#32068,.F.);
#42052=ORIENTED_EDGE('',*,*,#32071,.F.);
#42053=ORIENTED_EDGE('',*,*,#32037,.F.);
#42054=ORIENTED_EDGE('',*,*,#32016,.F.);
#42055=ORIENTED_EDGE('',*,*,#32020,.F.);
#42056=ORIENTED_EDGE('',*,*,#32023,.F.);
#42057=ORIENTED_EDGE('',*,*,#32026,.F.);
#42058=ORIENTED_EDGE('',*,*,#32029,.F.);
#42059=ORIENTED_EDGE('',*,*,#32032,.F.);
#42060=ORIENTED_EDGE('',*,*,#32035,.F.);
#42061=ORIENTED_EDGE('',*,*,#32074,.F.);
#42062=ORIENTED_EDGE('',*,*,#32075,.T.);
#42063=ORIENTED_EDGE('',*,*,#32076,.T.);
#42064=ORIENTED_EDGE('',*,*,#32077,.F.);
#42065=ORIENTED_EDGE('',*,*,#32078,.F.);
#42066=ORIENTED_EDGE('',*,*,#32079,.T.);
#42067=ORIENTED_EDGE('',*,*,#32080,.T.);
#42068=ORIENTED_EDGE('',*,*,#32075,.F.);
#42069=ORIENTED_EDGE('',*,*,#32081,.F.);
#42070=ORIENTED_EDGE('',*,*,#32082,.T.);
#42071=ORIENTED_EDGE('',*,*,#32083,.T.);
#42072=ORIENTED_EDGE('',*,*,#32079,.F.);
#42073=ORIENTED_EDGE('',*,*,#32084,.F.);
#42074=ORIENTED_EDGE('',*,*,#32085,.T.);
#42075=ORIENTED_EDGE('',*,*,#32086,.T.);
#42076=ORIENTED_EDGE('',*,*,#32082,.F.);
#42077=ORIENTED_EDGE('',*,*,#32087,.F.);
#42078=ORIENTED_EDGE('',*,*,#32088,.T.);
#42079=ORIENTED_EDGE('',*,*,#32089,.T.);
#42080=ORIENTED_EDGE('',*,*,#32085,.F.);
#42081=ORIENTED_EDGE('',*,*,#32090,.F.);
#42082=ORIENTED_EDGE('',*,*,#32091,.T.);
#42083=ORIENTED_EDGE('',*,*,#32092,.T.);
#42084=ORIENTED_EDGE('',*,*,#32088,.F.);
#42085=ORIENTED_EDGE('',*,*,#32093,.F.);
#42086=ORIENTED_EDGE('',*,*,#32094,.T.);
#42087=ORIENTED_EDGE('',*,*,#32095,.T.);
#42088=ORIENTED_EDGE('',*,*,#32091,.F.);
#42089=ORIENTED_EDGE('',*,*,#32096,.F.);
#42090=ORIENTED_EDGE('',*,*,#32097,.T.);
#42091=ORIENTED_EDGE('',*,*,#32098,.T.);
#42092=ORIENTED_EDGE('',*,*,#32094,.F.);
#42093=ORIENTED_EDGE('',*,*,#32099,.F.);
#42094=ORIENTED_EDGE('',*,*,#32100,.T.);
#42095=ORIENTED_EDGE('',*,*,#32101,.T.);
#42096=ORIENTED_EDGE('',*,*,#32097,.F.);
#42097=ORIENTED_EDGE('',*,*,#32102,.F.);
#42098=ORIENTED_EDGE('',*,*,#32103,.T.);
#42099=ORIENTED_EDGE('',*,*,#32104,.T.);
#42100=ORIENTED_EDGE('',*,*,#32100,.F.);
#42101=ORIENTED_EDGE('',*,*,#32105,.F.);
#42102=ORIENTED_EDGE('',*,*,#32106,.T.);
#42103=ORIENTED_EDGE('',*,*,#32107,.T.);
#42104=ORIENTED_EDGE('',*,*,#32103,.F.);
#42105=ORIENTED_EDGE('',*,*,#32108,.F.);
#42106=ORIENTED_EDGE('',*,*,#32109,.T.);
#42107=ORIENTED_EDGE('',*,*,#32110,.T.);
#42108=ORIENTED_EDGE('',*,*,#32106,.F.);
#42109=ORIENTED_EDGE('',*,*,#32111,.F.);
#42110=ORIENTED_EDGE('',*,*,#32112,.T.);
#42111=ORIENTED_EDGE('',*,*,#32113,.T.);
#42112=ORIENTED_EDGE('',*,*,#32109,.F.);
#42113=ORIENTED_EDGE('',*,*,#32114,.F.);
#42114=ORIENTED_EDGE('',*,*,#32115,.T.);
#42115=ORIENTED_EDGE('',*,*,#32116,.T.);
#42116=ORIENTED_EDGE('',*,*,#32112,.F.);
#42117=ORIENTED_EDGE('',*,*,#32117,.F.);
#42118=ORIENTED_EDGE('',*,*,#32118,.T.);
#42119=ORIENTED_EDGE('',*,*,#32119,.T.);
#42120=ORIENTED_EDGE('',*,*,#32115,.F.);
#42121=ORIENTED_EDGE('',*,*,#32120,.F.);
#42122=ORIENTED_EDGE('',*,*,#32121,.T.);
#42123=ORIENTED_EDGE('',*,*,#32122,.T.);
#42124=ORIENTED_EDGE('',*,*,#32118,.F.);
#42125=ORIENTED_EDGE('',*,*,#32123,.F.);
#42126=ORIENTED_EDGE('',*,*,#32124,.T.);
#42127=ORIENTED_EDGE('',*,*,#32125,.T.);
#42128=ORIENTED_EDGE('',*,*,#32121,.F.);
#42129=ORIENTED_EDGE('',*,*,#32126,.F.);
#42130=ORIENTED_EDGE('',*,*,#32127,.T.);
#42131=ORIENTED_EDGE('',*,*,#32128,.T.);
#42132=ORIENTED_EDGE('',*,*,#32124,.F.);
#42133=ORIENTED_EDGE('',*,*,#32129,.F.);
#42134=ORIENTED_EDGE('',*,*,#32130,.T.);
#42135=ORIENTED_EDGE('',*,*,#32131,.T.);
#42136=ORIENTED_EDGE('',*,*,#32127,.F.);
#42137=ORIENTED_EDGE('',*,*,#32132,.F.);
#42138=ORIENTED_EDGE('',*,*,#32133,.T.);
#42139=ORIENTED_EDGE('',*,*,#32134,.T.);
#42140=ORIENTED_EDGE('',*,*,#32130,.F.);
#42141=ORIENTED_EDGE('',*,*,#32135,.F.);
#42142=ORIENTED_EDGE('',*,*,#32136,.T.);
#42143=ORIENTED_EDGE('',*,*,#32137,.T.);
#42144=ORIENTED_EDGE('',*,*,#32133,.F.);
#42145=ORIENTED_EDGE('',*,*,#32138,.F.);
#42146=ORIENTED_EDGE('',*,*,#32077,.T.);
#42147=ORIENTED_EDGE('',*,*,#32139,.T.);
#42148=ORIENTED_EDGE('',*,*,#32136,.F.);
#42149=ORIENTED_EDGE('',*,*,#32139,.F.);
#42150=ORIENTED_EDGE('',*,*,#32076,.F.);
#42151=ORIENTED_EDGE('',*,*,#32080,.F.);
#42152=ORIENTED_EDGE('',*,*,#32083,.F.);
#42153=ORIENTED_EDGE('',*,*,#32086,.F.);
#42154=ORIENTED_EDGE('',*,*,#32089,.F.);
#42155=ORIENTED_EDGE('',*,*,#32092,.F.);
#42156=ORIENTED_EDGE('',*,*,#32095,.F.);
#42157=ORIENTED_EDGE('',*,*,#32098,.F.);
#42158=ORIENTED_EDGE('',*,*,#32101,.F.);
#42159=ORIENTED_EDGE('',*,*,#32104,.F.);
#42160=ORIENTED_EDGE('',*,*,#32107,.F.);
#42161=ORIENTED_EDGE('',*,*,#32110,.F.);
#42162=ORIENTED_EDGE('',*,*,#32113,.F.);
#42163=ORIENTED_EDGE('',*,*,#32116,.F.);
#42164=ORIENTED_EDGE('',*,*,#32119,.F.);
#42165=ORIENTED_EDGE('',*,*,#32122,.F.);
#42166=ORIENTED_EDGE('',*,*,#32125,.F.);
#42167=ORIENTED_EDGE('',*,*,#32128,.F.);
#42168=ORIENTED_EDGE('',*,*,#32131,.F.);
#42169=ORIENTED_EDGE('',*,*,#32134,.F.);
#42170=ORIENTED_EDGE('',*,*,#32137,.F.);
#42171=ORIENTED_EDGE('',*,*,#32014,.T.);
#42172=ORIENTED_EDGE('',*,*,#32036,.T.);
#42173=ORIENTED_EDGE('',*,*,#32033,.T.);
#42174=ORIENTED_EDGE('',*,*,#32030,.T.);
#42175=ORIENTED_EDGE('',*,*,#32027,.T.);
#42176=ORIENTED_EDGE('',*,*,#32024,.T.);
#42177=ORIENTED_EDGE('',*,*,#32021,.T.);
#42178=ORIENTED_EDGE('',*,*,#32018,.T.);
#42179=ORIENTED_EDGE('',*,*,#32140,.F.);
#42180=ORIENTED_EDGE('',*,*,#32141,.T.);
#42181=ORIENTED_EDGE('',*,*,#32142,.T.);
#42182=ORIENTED_EDGE('',*,*,#32143,.F.);
#42183=ORIENTED_EDGE('',*,*,#32144,.F.);
#42184=ORIENTED_EDGE('',*,*,#32145,.T.);
#42185=ORIENTED_EDGE('',*,*,#32146,.T.);
#42186=ORIENTED_EDGE('',*,*,#32141,.F.);
#42187=ORIENTED_EDGE('',*,*,#32147,.F.);
#42188=ORIENTED_EDGE('',*,*,#32148,.T.);
#42189=ORIENTED_EDGE('',*,*,#32149,.T.);
#42190=ORIENTED_EDGE('',*,*,#32145,.F.);
#42191=ORIENTED_EDGE('',*,*,#32150,.F.);
#42192=ORIENTED_EDGE('',*,*,#32151,.T.);
#42193=ORIENTED_EDGE('',*,*,#32152,.T.);
#42194=ORIENTED_EDGE('',*,*,#32148,.F.);
#42195=ORIENTED_EDGE('',*,*,#32153,.F.);
#42196=ORIENTED_EDGE('',*,*,#32154,.T.);
#42197=ORIENTED_EDGE('',*,*,#32155,.T.);
#42198=ORIENTED_EDGE('',*,*,#32151,.F.);
#42199=ORIENTED_EDGE('',*,*,#32156,.F.);
#42200=ORIENTED_EDGE('',*,*,#32157,.T.);
#42201=ORIENTED_EDGE('',*,*,#32158,.T.);
#42202=ORIENTED_EDGE('',*,*,#32154,.F.);
#42203=ORIENTED_EDGE('',*,*,#32159,.F.);
#42204=ORIENTED_EDGE('',*,*,#32160,.T.);
#42205=ORIENTED_EDGE('',*,*,#32161,.T.);
#42206=ORIENTED_EDGE('',*,*,#32157,.F.);
#42207=ORIENTED_EDGE('',*,*,#32162,.F.);
#42208=ORIENTED_EDGE('',*,*,#32143,.T.);
#42209=ORIENTED_EDGE('',*,*,#32163,.T.);
#42210=ORIENTED_EDGE('',*,*,#32160,.F.);
#42211=ORIENTED_EDGE('',*,*,#32164,.F.);
#42212=ORIENTED_EDGE('',*,*,#32165,.T.);
#42213=ORIENTED_EDGE('',*,*,#32166,.T.);
#42214=ORIENTED_EDGE('',*,*,#32167,.F.);
#42215=ORIENTED_EDGE('',*,*,#32168,.F.);
#42216=ORIENTED_EDGE('',*,*,#32169,.T.);
#42217=ORIENTED_EDGE('',*,*,#32170,.T.);
#42218=ORIENTED_EDGE('',*,*,#32165,.F.);
#42219=ORIENTED_EDGE('',*,*,#32171,.F.);
#42220=ORIENTED_EDGE('',*,*,#32172,.T.);
#42221=ORIENTED_EDGE('',*,*,#32173,.T.);
#42222=ORIENTED_EDGE('',*,*,#32169,.F.);
#42223=ORIENTED_EDGE('',*,*,#32174,.F.);
#42224=ORIENTED_EDGE('',*,*,#32175,.T.);
#42225=ORIENTED_EDGE('',*,*,#32176,.T.);
#42226=ORIENTED_EDGE('',*,*,#32172,.F.);
#42227=ORIENTED_EDGE('',*,*,#32177,.F.);
#42228=ORIENTED_EDGE('',*,*,#32178,.T.);
#42229=ORIENTED_EDGE('',*,*,#32179,.T.);
#42230=ORIENTED_EDGE('',*,*,#32175,.F.);
#42231=ORIENTED_EDGE('',*,*,#32180,.F.);
#42232=ORIENTED_EDGE('',*,*,#32181,.T.);
#42233=ORIENTED_EDGE('',*,*,#32182,.T.);
#42234=ORIENTED_EDGE('',*,*,#32178,.F.);
#42235=ORIENTED_EDGE('',*,*,#32183,.F.);
#42236=ORIENTED_EDGE('',*,*,#32184,.T.);
#42237=ORIENTED_EDGE('',*,*,#32185,.T.);
#42238=ORIENTED_EDGE('',*,*,#32181,.F.);
#42239=ORIENTED_EDGE('',*,*,#32186,.F.);
#42240=ORIENTED_EDGE('',*,*,#32187,.T.);
#42241=ORIENTED_EDGE('',*,*,#32188,.T.);
#42242=ORIENTED_EDGE('',*,*,#32184,.F.);
#42243=ORIENTED_EDGE('',*,*,#32189,.F.);
#42244=ORIENTED_EDGE('',*,*,#32190,.T.);
#42245=ORIENTED_EDGE('',*,*,#32191,.T.);
#42246=ORIENTED_EDGE('',*,*,#32187,.F.);
#42247=ORIENTED_EDGE('',*,*,#32192,.F.);
#42248=ORIENTED_EDGE('',*,*,#32193,.T.);
#42249=ORIENTED_EDGE('',*,*,#32194,.T.);
#42250=ORIENTED_EDGE('',*,*,#32190,.F.);
#42251=ORIENTED_EDGE('',*,*,#32195,.F.);
#42252=ORIENTED_EDGE('',*,*,#32196,.T.);
#42253=ORIENTED_EDGE('',*,*,#32197,.T.);
#42254=ORIENTED_EDGE('',*,*,#32193,.F.);
#42255=ORIENTED_EDGE('',*,*,#32198,.F.);
#42256=ORIENTED_EDGE('',*,*,#32167,.T.);
#42257=ORIENTED_EDGE('',*,*,#32199,.T.);
#42258=ORIENTED_EDGE('',*,*,#32196,.F.);
#42259=ORIENTED_EDGE('',*,*,#32199,.F.);
#42260=ORIENTED_EDGE('',*,*,#32166,.F.);
#42261=ORIENTED_EDGE('',*,*,#32170,.F.);
#42262=ORIENTED_EDGE('',*,*,#32173,.F.);
#42263=ORIENTED_EDGE('',*,*,#32176,.F.);
#42264=ORIENTED_EDGE('',*,*,#32179,.F.);
#42265=ORIENTED_EDGE('',*,*,#32182,.F.);
#42266=ORIENTED_EDGE('',*,*,#32185,.F.);
#42267=ORIENTED_EDGE('',*,*,#32188,.F.);
#42268=ORIENTED_EDGE('',*,*,#32191,.F.);
#42269=ORIENTED_EDGE('',*,*,#32194,.F.);
#42270=ORIENTED_EDGE('',*,*,#32197,.F.);
#42271=ORIENTED_EDGE('',*,*,#32163,.F.);
#42272=ORIENTED_EDGE('',*,*,#32142,.F.);
#42273=ORIENTED_EDGE('',*,*,#32146,.F.);
#42274=ORIENTED_EDGE('',*,*,#32149,.F.);
#42275=ORIENTED_EDGE('',*,*,#32152,.F.);
#42276=ORIENTED_EDGE('',*,*,#32155,.F.);
#42277=ORIENTED_EDGE('',*,*,#32158,.F.);
#42278=ORIENTED_EDGE('',*,*,#32161,.F.);
#42279=ORIENTED_EDGE('',*,*,#32200,.F.);
#42280=ORIENTED_EDGE('',*,*,#32201,.T.);
#42281=ORIENTED_EDGE('',*,*,#32202,.T.);
#42282=ORIENTED_EDGE('',*,*,#32203,.F.);
#42283=ORIENTED_EDGE('',*,*,#32204,.F.);
#42284=ORIENTED_EDGE('',*,*,#32205,.T.);
#42285=ORIENTED_EDGE('',*,*,#32206,.T.);
#42286=ORIENTED_EDGE('',*,*,#32201,.F.);
#42287=ORIENTED_EDGE('',*,*,#32207,.F.);
#42288=ORIENTED_EDGE('',*,*,#32208,.T.);
#42289=ORIENTED_EDGE('',*,*,#32209,.T.);
#42290=ORIENTED_EDGE('',*,*,#32205,.F.);
#42291=ORIENTED_EDGE('',*,*,#32210,.F.);
#42292=ORIENTED_EDGE('',*,*,#32211,.T.);
#42293=ORIENTED_EDGE('',*,*,#32212,.T.);
#42294=ORIENTED_EDGE('',*,*,#32208,.F.);
#42295=ORIENTED_EDGE('',*,*,#32213,.F.);
#42296=ORIENTED_EDGE('',*,*,#32214,.T.);
#42297=ORIENTED_EDGE('',*,*,#32215,.T.);
#42298=ORIENTED_EDGE('',*,*,#32211,.F.);
#42299=ORIENTED_EDGE('',*,*,#32216,.F.);
#42300=ORIENTED_EDGE('',*,*,#32217,.T.);
#42301=ORIENTED_EDGE('',*,*,#32218,.T.);
#42302=ORIENTED_EDGE('',*,*,#32214,.F.);
#42303=ORIENTED_EDGE('',*,*,#32219,.F.);
#42304=ORIENTED_EDGE('',*,*,#32220,.T.);
#42305=ORIENTED_EDGE('',*,*,#32221,.T.);
#42306=ORIENTED_EDGE('',*,*,#32217,.F.);
#42307=ORIENTED_EDGE('',*,*,#32222,.F.);
#42308=ORIENTED_EDGE('',*,*,#32223,.T.);
#42309=ORIENTED_EDGE('',*,*,#32224,.T.);
#42310=ORIENTED_EDGE('',*,*,#32220,.F.);
#42311=ORIENTED_EDGE('',*,*,#32225,.F.);
#42312=ORIENTED_EDGE('',*,*,#32203,.T.);
#42313=ORIENTED_EDGE('',*,*,#32226,.T.);
#42314=ORIENTED_EDGE('',*,*,#32223,.F.);
#42315=ORIENTED_EDGE('',*,*,#32227,.F.);
#42316=ORIENTED_EDGE('',*,*,#32228,.T.);
#42317=ORIENTED_EDGE('',*,*,#32229,.T.);
#42318=ORIENTED_EDGE('',*,*,#32230,.F.);
#42319=ORIENTED_EDGE('',*,*,#32231,.F.);
#42320=ORIENTED_EDGE('',*,*,#32232,.T.);
#42321=ORIENTED_EDGE('',*,*,#32233,.T.);
#42322=ORIENTED_EDGE('',*,*,#32228,.F.);
#42323=ORIENTED_EDGE('',*,*,#32234,.F.);
#42324=ORIENTED_EDGE('',*,*,#32235,.T.);
#42325=ORIENTED_EDGE('',*,*,#32236,.T.);
#42326=ORIENTED_EDGE('',*,*,#32232,.F.);
#42327=ORIENTED_EDGE('',*,*,#32237,.F.);
#42328=ORIENTED_EDGE('',*,*,#32238,.T.);
#42329=ORIENTED_EDGE('',*,*,#32239,.T.);
#42330=ORIENTED_EDGE('',*,*,#32235,.F.);
#42331=ORIENTED_EDGE('',*,*,#32240,.F.);
#42332=ORIENTED_EDGE('',*,*,#32241,.T.);
#42333=ORIENTED_EDGE('',*,*,#32242,.T.);
#42334=ORIENTED_EDGE('',*,*,#32238,.F.);
#42335=ORIENTED_EDGE('',*,*,#32243,.F.);
#42336=ORIENTED_EDGE('',*,*,#32244,.T.);
#42337=ORIENTED_EDGE('',*,*,#32245,.T.);
#42338=ORIENTED_EDGE('',*,*,#32241,.F.);
#42339=ORIENTED_EDGE('',*,*,#32246,.F.);
#42340=ORIENTED_EDGE('',*,*,#32247,.T.);
#42341=ORIENTED_EDGE('',*,*,#32248,.T.);
#42342=ORIENTED_EDGE('',*,*,#32244,.F.);
#42343=ORIENTED_EDGE('',*,*,#32249,.F.);
#42344=ORIENTED_EDGE('',*,*,#32250,.T.);
#42345=ORIENTED_EDGE('',*,*,#32251,.T.);
#42346=ORIENTED_EDGE('',*,*,#32247,.F.);
#42347=ORIENTED_EDGE('',*,*,#32252,.F.);
#42348=ORIENTED_EDGE('',*,*,#32253,.T.);
#42349=ORIENTED_EDGE('',*,*,#32254,.T.);
#42350=ORIENTED_EDGE('',*,*,#32250,.F.);
#42351=ORIENTED_EDGE('',*,*,#32255,.F.);
#42352=ORIENTED_EDGE('',*,*,#32256,.T.);
#42353=ORIENTED_EDGE('',*,*,#32257,.T.);
#42354=ORIENTED_EDGE('',*,*,#32253,.F.);
#42355=ORIENTED_EDGE('',*,*,#32258,.F.);
#42356=ORIENTED_EDGE('',*,*,#32259,.T.);
#42357=ORIENTED_EDGE('',*,*,#32260,.T.);
#42358=ORIENTED_EDGE('',*,*,#32256,.F.);
#42359=ORIENTED_EDGE('',*,*,#32261,.F.);
#42360=ORIENTED_EDGE('',*,*,#32262,.T.);
#42361=ORIENTED_EDGE('',*,*,#32263,.T.);
#42362=ORIENTED_EDGE('',*,*,#32259,.F.);
#42363=ORIENTED_EDGE('',*,*,#32264,.F.);
#42364=ORIENTED_EDGE('',*,*,#32265,.T.);
#42365=ORIENTED_EDGE('',*,*,#32266,.T.);
#42366=ORIENTED_EDGE('',*,*,#32262,.F.);
#42367=ORIENTED_EDGE('',*,*,#32267,.F.);
#42368=ORIENTED_EDGE('',*,*,#32268,.T.);
#42369=ORIENTED_EDGE('',*,*,#32269,.T.);
#42370=ORIENTED_EDGE('',*,*,#32265,.F.);
#42371=ORIENTED_EDGE('',*,*,#32270,.F.);
#42372=ORIENTED_EDGE('',*,*,#32271,.T.);
#42373=ORIENTED_EDGE('',*,*,#32272,.T.);
#42374=ORIENTED_EDGE('',*,*,#32268,.F.);
#42375=ORIENTED_EDGE('',*,*,#32273,.F.);
#42376=ORIENTED_EDGE('',*,*,#32274,.T.);
#42377=ORIENTED_EDGE('',*,*,#32275,.T.);
#42378=ORIENTED_EDGE('',*,*,#32271,.F.);
#42379=ORIENTED_EDGE('',*,*,#32276,.F.);
#42380=ORIENTED_EDGE('',*,*,#32277,.T.);
#42381=ORIENTED_EDGE('',*,*,#32278,.T.);
#42382=ORIENTED_EDGE('',*,*,#32274,.F.);
#42383=ORIENTED_EDGE('',*,*,#32279,.F.);
#42384=ORIENTED_EDGE('',*,*,#32280,.T.);
#42385=ORIENTED_EDGE('',*,*,#32281,.T.);
#42386=ORIENTED_EDGE('',*,*,#32277,.F.);
#42387=ORIENTED_EDGE('',*,*,#32282,.F.);
#42388=ORIENTED_EDGE('',*,*,#32230,.T.);
#42389=ORIENTED_EDGE('',*,*,#32283,.T.);
#42390=ORIENTED_EDGE('',*,*,#32280,.F.);
#42391=ORIENTED_EDGE('',*,*,#32283,.F.);
#42392=ORIENTED_EDGE('',*,*,#32229,.F.);
#42393=ORIENTED_EDGE('',*,*,#32233,.F.);
#42394=ORIENTED_EDGE('',*,*,#32236,.F.);
#42395=ORIENTED_EDGE('',*,*,#32239,.F.);
#42396=ORIENTED_EDGE('',*,*,#32242,.F.);
#42397=ORIENTED_EDGE('',*,*,#32245,.F.);
#42398=ORIENTED_EDGE('',*,*,#32248,.F.);
#42399=ORIENTED_EDGE('',*,*,#32251,.F.);
#42400=ORIENTED_EDGE('',*,*,#32254,.F.);
#42401=ORIENTED_EDGE('',*,*,#32257,.F.);
#42402=ORIENTED_EDGE('',*,*,#32260,.F.);
#42403=ORIENTED_EDGE('',*,*,#32263,.F.);
#42404=ORIENTED_EDGE('',*,*,#32266,.F.);
#42405=ORIENTED_EDGE('',*,*,#32269,.F.);
#42406=ORIENTED_EDGE('',*,*,#32272,.F.);
#42407=ORIENTED_EDGE('',*,*,#32275,.F.);
#42408=ORIENTED_EDGE('',*,*,#32278,.F.);
#42409=ORIENTED_EDGE('',*,*,#32281,.F.);
#42410=ORIENTED_EDGE('',*,*,#32226,.F.);
#42411=ORIENTED_EDGE('',*,*,#32202,.F.);
#42412=ORIENTED_EDGE('',*,*,#32206,.F.);
#42413=ORIENTED_EDGE('',*,*,#32209,.F.);
#42414=ORIENTED_EDGE('',*,*,#32212,.F.);
#42415=ORIENTED_EDGE('',*,*,#32215,.F.);
#42416=ORIENTED_EDGE('',*,*,#32218,.F.);
#42417=ORIENTED_EDGE('',*,*,#32221,.F.);
#42418=ORIENTED_EDGE('',*,*,#32224,.F.);
#42419=ORIENTED_EDGE('',*,*,#32200,.T.);
#42420=ORIENTED_EDGE('',*,*,#32225,.T.);
#42421=ORIENTED_EDGE('',*,*,#32222,.T.);
#42422=ORIENTED_EDGE('',*,*,#32219,.T.);
#42423=ORIENTED_EDGE('',*,*,#32216,.T.);
#42424=ORIENTED_EDGE('',*,*,#32213,.T.);
#42425=ORIENTED_EDGE('',*,*,#32210,.T.);
#42426=ORIENTED_EDGE('',*,*,#32207,.T.);
#42427=ORIENTED_EDGE('',*,*,#32204,.T.);
#42428=ORIENTED_EDGE('',*,*,#32140,.T.);
#42429=ORIENTED_EDGE('',*,*,#32162,.T.);
#42430=ORIENTED_EDGE('',*,*,#32159,.T.);
#42431=ORIENTED_EDGE('',*,*,#32156,.T.);
#42432=ORIENTED_EDGE('',*,*,#32153,.T.);
#42433=ORIENTED_EDGE('',*,*,#32150,.T.);
#42434=ORIENTED_EDGE('',*,*,#32147,.T.);
#42435=ORIENTED_EDGE('',*,*,#32144,.T.);
#42436=ORIENTED_EDGE('',*,*,#32284,.F.);
#42437=ORIENTED_EDGE('',*,*,#32285,.T.);
#42438=ORIENTED_EDGE('',*,*,#32286,.T.);
#42439=ORIENTED_EDGE('',*,*,#32287,.F.);
#42440=ORIENTED_EDGE('',*,*,#32288,.F.);
#42441=ORIENTED_EDGE('',*,*,#32289,.T.);
#42442=ORIENTED_EDGE('',*,*,#32290,.T.);
#42443=ORIENTED_EDGE('',*,*,#32285,.F.);
#42444=ORIENTED_EDGE('',*,*,#32291,.F.);
#42445=ORIENTED_EDGE('',*,*,#32292,.T.);
#42446=ORIENTED_EDGE('',*,*,#32293,.T.);
#42447=ORIENTED_EDGE('',*,*,#32289,.F.);
#42448=ORIENTED_EDGE('',*,*,#32294,.F.);
#42449=ORIENTED_EDGE('',*,*,#32295,.T.);
#42450=ORIENTED_EDGE('',*,*,#32296,.T.);
#42451=ORIENTED_EDGE('',*,*,#32292,.F.);
#42452=ORIENTED_EDGE('',*,*,#32297,.F.);
#42453=ORIENTED_EDGE('',*,*,#32298,.T.);
#42454=ORIENTED_EDGE('',*,*,#32299,.T.);
#42455=ORIENTED_EDGE('',*,*,#32295,.F.);
#42456=ORIENTED_EDGE('',*,*,#32300,.F.);
#42457=ORIENTED_EDGE('',*,*,#32301,.T.);
#42458=ORIENTED_EDGE('',*,*,#32302,.T.);
#42459=ORIENTED_EDGE('',*,*,#32298,.F.);
#42460=ORIENTED_EDGE('',*,*,#32303,.F.);
#42461=ORIENTED_EDGE('',*,*,#32304,.T.);
#42462=ORIENTED_EDGE('',*,*,#32305,.T.);
#42463=ORIENTED_EDGE('',*,*,#32301,.F.);
#42464=ORIENTED_EDGE('',*,*,#32306,.F.);
#42465=ORIENTED_EDGE('',*,*,#32287,.T.);
#42466=ORIENTED_EDGE('',*,*,#32307,.T.);
#42467=ORIENTED_EDGE('',*,*,#32304,.F.);
#42468=ORIENTED_EDGE('',*,*,#32308,.F.);
#42469=ORIENTED_EDGE('',*,*,#32309,.T.);
#42470=ORIENTED_EDGE('',*,*,#32310,.T.);
#42471=ORIENTED_EDGE('',*,*,#32311,.F.);
#42472=ORIENTED_EDGE('',*,*,#32312,.F.);
#42473=ORIENTED_EDGE('',*,*,#32313,.T.);
#42474=ORIENTED_EDGE('',*,*,#32314,.T.);
#42475=ORIENTED_EDGE('',*,*,#32309,.F.);
#42476=ORIENTED_EDGE('',*,*,#32315,.F.);
#42477=ORIENTED_EDGE('',*,*,#32316,.T.);
#42478=ORIENTED_EDGE('',*,*,#32317,.T.);
#42479=ORIENTED_EDGE('',*,*,#32313,.F.);
#42480=ORIENTED_EDGE('',*,*,#32318,.F.);
#42481=ORIENTED_EDGE('',*,*,#32319,.T.);
#42482=ORIENTED_EDGE('',*,*,#32320,.T.);
#42483=ORIENTED_EDGE('',*,*,#32316,.F.);
#42484=ORIENTED_EDGE('',*,*,#32321,.F.);
#42485=ORIENTED_EDGE('',*,*,#32322,.T.);
#42486=ORIENTED_EDGE('',*,*,#32323,.T.);
#42487=ORIENTED_EDGE('',*,*,#32319,.F.);
#42488=ORIENTED_EDGE('',*,*,#32324,.F.);
#42489=ORIENTED_EDGE('',*,*,#32325,.T.);
#42490=ORIENTED_EDGE('',*,*,#32326,.T.);
#42491=ORIENTED_EDGE('',*,*,#32322,.F.);
#42492=ORIENTED_EDGE('',*,*,#32327,.F.);
#42493=ORIENTED_EDGE('',*,*,#32328,.T.);
#42494=ORIENTED_EDGE('',*,*,#32329,.T.);
#42495=ORIENTED_EDGE('',*,*,#32325,.F.);
#42496=ORIENTED_EDGE('',*,*,#32330,.F.);
#42497=ORIENTED_EDGE('',*,*,#32331,.T.);
#42498=ORIENTED_EDGE('',*,*,#32332,.T.);
#42499=ORIENTED_EDGE('',*,*,#32328,.F.);
#42500=ORIENTED_EDGE('',*,*,#32333,.F.);
#42501=ORIENTED_EDGE('',*,*,#32334,.T.);
#42502=ORIENTED_EDGE('',*,*,#32335,.T.);
#42503=ORIENTED_EDGE('',*,*,#32331,.F.);
#42504=ORIENTED_EDGE('',*,*,#32336,.F.);
#42505=ORIENTED_EDGE('',*,*,#32337,.T.);
#42506=ORIENTED_EDGE('',*,*,#32338,.T.);
#42507=ORIENTED_EDGE('',*,*,#32334,.F.);
#42508=ORIENTED_EDGE('',*,*,#32339,.F.);
#42509=ORIENTED_EDGE('',*,*,#32340,.T.);
#42510=ORIENTED_EDGE('',*,*,#32341,.T.);
#42511=ORIENTED_EDGE('',*,*,#32337,.F.);
#42512=ORIENTED_EDGE('',*,*,#32342,.F.);
#42513=ORIENTED_EDGE('',*,*,#32311,.T.);
#42514=ORIENTED_EDGE('',*,*,#32343,.T.);
#42515=ORIENTED_EDGE('',*,*,#32340,.F.);
#42516=ORIENTED_EDGE('',*,*,#32343,.F.);
#42517=ORIENTED_EDGE('',*,*,#32310,.F.);
#42518=ORIENTED_EDGE('',*,*,#32314,.F.);
#42519=ORIENTED_EDGE('',*,*,#32317,.F.);
#42520=ORIENTED_EDGE('',*,*,#32320,.F.);
#42521=ORIENTED_EDGE('',*,*,#32323,.F.);
#42522=ORIENTED_EDGE('',*,*,#32326,.F.);
#42523=ORIENTED_EDGE('',*,*,#32329,.F.);
#42524=ORIENTED_EDGE('',*,*,#32332,.F.);
#42525=ORIENTED_EDGE('',*,*,#32335,.F.);
#42526=ORIENTED_EDGE('',*,*,#32338,.F.);
#42527=ORIENTED_EDGE('',*,*,#32341,.F.);
#42528=ORIENTED_EDGE('',*,*,#32307,.F.);
#42529=ORIENTED_EDGE('',*,*,#32286,.F.);
#42530=ORIENTED_EDGE('',*,*,#32290,.F.);
#42531=ORIENTED_EDGE('',*,*,#32293,.F.);
#42532=ORIENTED_EDGE('',*,*,#32296,.F.);
#42533=ORIENTED_EDGE('',*,*,#32299,.F.);
#42534=ORIENTED_EDGE('',*,*,#32302,.F.);
#42535=ORIENTED_EDGE('',*,*,#32305,.F.);
#42536=ORIENTED_EDGE('',*,*,#32344,.F.);
#42537=ORIENTED_EDGE('',*,*,#32345,.T.);
#42538=ORIENTED_EDGE('',*,*,#32346,.T.);
#42539=ORIENTED_EDGE('',*,*,#32347,.F.);
#42540=ORIENTED_EDGE('',*,*,#32348,.F.);
#42541=ORIENTED_EDGE('',*,*,#32349,.T.);
#42542=ORIENTED_EDGE('',*,*,#32350,.T.);
#42543=ORIENTED_EDGE('',*,*,#32345,.F.);
#42544=ORIENTED_EDGE('',*,*,#32351,.F.);
#42545=ORIENTED_EDGE('',*,*,#32352,.T.);
#42546=ORIENTED_EDGE('',*,*,#32353,.T.);
#42547=ORIENTED_EDGE('',*,*,#32349,.F.);
#42548=ORIENTED_EDGE('',*,*,#32354,.F.);
#42549=ORIENTED_EDGE('',*,*,#32355,.T.);
#42550=ORIENTED_EDGE('',*,*,#32356,.T.);
#42551=ORIENTED_EDGE('',*,*,#32352,.F.);
#42552=ORIENTED_EDGE('',*,*,#32357,.F.);
#42553=ORIENTED_EDGE('',*,*,#32358,.T.);
#42554=ORIENTED_EDGE('',*,*,#32359,.T.);
#42555=ORIENTED_EDGE('',*,*,#32355,.F.);
#42556=ORIENTED_EDGE('',*,*,#32360,.F.);
#42557=ORIENTED_EDGE('',*,*,#32361,.T.);
#42558=ORIENTED_EDGE('',*,*,#32362,.T.);
#42559=ORIENTED_EDGE('',*,*,#32358,.F.);
#42560=ORIENTED_EDGE('',*,*,#32363,.F.);
#42561=ORIENTED_EDGE('',*,*,#32364,.T.);
#42562=ORIENTED_EDGE('',*,*,#32365,.T.);
#42563=ORIENTED_EDGE('',*,*,#32361,.F.);
#42564=ORIENTED_EDGE('',*,*,#32366,.F.);
#42565=ORIENTED_EDGE('',*,*,#32367,.T.);
#42566=ORIENTED_EDGE('',*,*,#32368,.T.);
#42567=ORIENTED_EDGE('',*,*,#32364,.F.);
#42568=ORIENTED_EDGE('',*,*,#32369,.F.);
#42569=ORIENTED_EDGE('',*,*,#32370,.T.);
#42570=ORIENTED_EDGE('',*,*,#32371,.T.);
#42571=ORIENTED_EDGE('',*,*,#32367,.F.);
#42572=ORIENTED_EDGE('',*,*,#32372,.F.);
#42573=ORIENTED_EDGE('',*,*,#32373,.T.);
#42574=ORIENTED_EDGE('',*,*,#32374,.T.);
#42575=ORIENTED_EDGE('',*,*,#32370,.F.);
#42576=ORIENTED_EDGE('',*,*,#32375,.F.);
#42577=ORIENTED_EDGE('',*,*,#32347,.T.);
#42578=ORIENTED_EDGE('',*,*,#32376,.T.);
#42579=ORIENTED_EDGE('',*,*,#32373,.F.);
#42580=ORIENTED_EDGE('',*,*,#32376,.F.);
#42581=ORIENTED_EDGE('',*,*,#32346,.F.);
#42582=ORIENTED_EDGE('',*,*,#32350,.F.);
#42583=ORIENTED_EDGE('',*,*,#32353,.F.);
#42584=ORIENTED_EDGE('',*,*,#32356,.F.);
#42585=ORIENTED_EDGE('',*,*,#32359,.F.);
#42586=ORIENTED_EDGE('',*,*,#32362,.F.);
#42587=ORIENTED_EDGE('',*,*,#32365,.F.);
#42588=ORIENTED_EDGE('',*,*,#32368,.F.);
#42589=ORIENTED_EDGE('',*,*,#32371,.F.);
#42590=ORIENTED_EDGE('',*,*,#32374,.F.);
#42591=ORIENTED_EDGE('',*,*,#32284,.T.);
#42592=ORIENTED_EDGE('',*,*,#32306,.T.);
#42593=ORIENTED_EDGE('',*,*,#32303,.T.);
#42594=ORIENTED_EDGE('',*,*,#32300,.T.);
#42595=ORIENTED_EDGE('',*,*,#32297,.T.);
#42596=ORIENTED_EDGE('',*,*,#32294,.T.);
#42597=ORIENTED_EDGE('',*,*,#32291,.T.);
#42598=ORIENTED_EDGE('',*,*,#32288,.T.);
#42599=ORIENTED_EDGE('',*,*,#32377,.F.);
#42600=ORIENTED_EDGE('',*,*,#32378,.T.);
#42601=ORIENTED_EDGE('',*,*,#32379,.T.);
#42602=ORIENTED_EDGE('',*,*,#32380,.F.);
#42603=ORIENTED_EDGE('',*,*,#32381,.F.);
#42604=ORIENTED_EDGE('',*,*,#32382,.T.);
#42605=ORIENTED_EDGE('',*,*,#32383,.T.);
#42606=ORIENTED_EDGE('',*,*,#32378,.F.);
#42607=ORIENTED_EDGE('',*,*,#32384,.F.);
#42608=ORIENTED_EDGE('',*,*,#32385,.T.);
#42609=ORIENTED_EDGE('',*,*,#32386,.T.);
#42610=ORIENTED_EDGE('',*,*,#32382,.F.);
#42611=ORIENTED_EDGE('',*,*,#32387,.F.);
#42612=ORIENTED_EDGE('',*,*,#32388,.T.);
#42613=ORIENTED_EDGE('',*,*,#32389,.T.);
#42614=ORIENTED_EDGE('',*,*,#32385,.F.);
#42615=ORIENTED_EDGE('',*,*,#32390,.F.);
#42616=ORIENTED_EDGE('',*,*,#32391,.T.);
#42617=ORIENTED_EDGE('',*,*,#32392,.T.);
#42618=ORIENTED_EDGE('',*,*,#32388,.F.);
#42619=ORIENTED_EDGE('',*,*,#32393,.F.);
#42620=ORIENTED_EDGE('',*,*,#32394,.T.);
#42621=ORIENTED_EDGE('',*,*,#32395,.T.);
#42622=ORIENTED_EDGE('',*,*,#32391,.F.);
#42623=ORIENTED_EDGE('',*,*,#32396,.F.);
#42624=ORIENTED_EDGE('',*,*,#32397,.T.);
#42625=ORIENTED_EDGE('',*,*,#32398,.T.);
#42626=ORIENTED_EDGE('',*,*,#32394,.F.);
#42627=ORIENTED_EDGE('',*,*,#32399,.F.);
#42628=ORIENTED_EDGE('',*,*,#32380,.T.);
#42629=ORIENTED_EDGE('',*,*,#32400,.T.);
#42630=ORIENTED_EDGE('',*,*,#32397,.F.);
#42631=ORIENTED_EDGE('',*,*,#32401,.F.);
#42632=ORIENTED_EDGE('',*,*,#32402,.T.);
#42633=ORIENTED_EDGE('',*,*,#32403,.T.);
#42634=ORIENTED_EDGE('',*,*,#32404,.F.);
#42635=ORIENTED_EDGE('',*,*,#32405,.F.);
#42636=ORIENTED_EDGE('',*,*,#32406,.T.);
#42637=ORIENTED_EDGE('',*,*,#32407,.T.);
#42638=ORIENTED_EDGE('',*,*,#32402,.F.);
#42639=ORIENTED_EDGE('',*,*,#32408,.F.);
#42640=ORIENTED_EDGE('',*,*,#32409,.T.);
#42641=ORIENTED_EDGE('',*,*,#32410,.T.);
#42642=ORIENTED_EDGE('',*,*,#32406,.F.);
#42643=ORIENTED_EDGE('',*,*,#32411,.F.);
#42644=ORIENTED_EDGE('',*,*,#32412,.T.);
#42645=ORIENTED_EDGE('',*,*,#32413,.T.);
#42646=ORIENTED_EDGE('',*,*,#32409,.F.);
#42647=ORIENTED_EDGE('',*,*,#32414,.F.);
#42648=ORIENTED_EDGE('',*,*,#32415,.T.);
#42649=ORIENTED_EDGE('',*,*,#32416,.T.);
#42650=ORIENTED_EDGE('',*,*,#32412,.F.);
#42651=ORIENTED_EDGE('',*,*,#32417,.F.);
#42652=ORIENTED_EDGE('',*,*,#32418,.T.);
#42653=ORIENTED_EDGE('',*,*,#32419,.T.);
#42654=ORIENTED_EDGE('',*,*,#32415,.F.);
#42655=ORIENTED_EDGE('',*,*,#32420,.F.);
#42656=ORIENTED_EDGE('',*,*,#32421,.T.);
#42657=ORIENTED_EDGE('',*,*,#32422,.T.);
#42658=ORIENTED_EDGE('',*,*,#32418,.F.);
#42659=ORIENTED_EDGE('',*,*,#32423,.F.);
#42660=ORIENTED_EDGE('',*,*,#32424,.T.);
#42661=ORIENTED_EDGE('',*,*,#32425,.T.);
#42662=ORIENTED_EDGE('',*,*,#32421,.F.);
#42663=ORIENTED_EDGE('',*,*,#32426,.F.);
#42664=ORIENTED_EDGE('',*,*,#32427,.T.);
#42665=ORIENTED_EDGE('',*,*,#32428,.T.);
#42666=ORIENTED_EDGE('',*,*,#32424,.F.);
#42667=ORIENTED_EDGE('',*,*,#32429,.F.);
#42668=ORIENTED_EDGE('',*,*,#32430,.T.);
#42669=ORIENTED_EDGE('',*,*,#32431,.T.);
#42670=ORIENTED_EDGE('',*,*,#32427,.F.);
#42671=ORIENTED_EDGE('',*,*,#32432,.F.);
#42672=ORIENTED_EDGE('',*,*,#32433,.T.);
#42673=ORIENTED_EDGE('',*,*,#32434,.T.);
#42674=ORIENTED_EDGE('',*,*,#32430,.F.);
#42675=ORIENTED_EDGE('',*,*,#32435,.F.);
#42676=ORIENTED_EDGE('',*,*,#32404,.T.);
#42677=ORIENTED_EDGE('',*,*,#32436,.T.);
#42678=ORIENTED_EDGE('',*,*,#32433,.F.);
#42679=ORIENTED_EDGE('',*,*,#32436,.F.);
#42680=ORIENTED_EDGE('',*,*,#32403,.F.);
#42681=ORIENTED_EDGE('',*,*,#32407,.F.);
#42682=ORIENTED_EDGE('',*,*,#32410,.F.);
#42683=ORIENTED_EDGE('',*,*,#32413,.F.);
#42684=ORIENTED_EDGE('',*,*,#32416,.F.);
#42685=ORIENTED_EDGE('',*,*,#32419,.F.);
#42686=ORIENTED_EDGE('',*,*,#32422,.F.);
#42687=ORIENTED_EDGE('',*,*,#32425,.F.);
#42688=ORIENTED_EDGE('',*,*,#32428,.F.);
#42689=ORIENTED_EDGE('',*,*,#32431,.F.);
#42690=ORIENTED_EDGE('',*,*,#32434,.F.);
#42691=ORIENTED_EDGE('',*,*,#32400,.F.);
#42692=ORIENTED_EDGE('',*,*,#32379,.F.);
#42693=ORIENTED_EDGE('',*,*,#32383,.F.);
#42694=ORIENTED_EDGE('',*,*,#32386,.F.);
#42695=ORIENTED_EDGE('',*,*,#32389,.F.);
#42696=ORIENTED_EDGE('',*,*,#32392,.F.);
#42697=ORIENTED_EDGE('',*,*,#32395,.F.);
#42698=ORIENTED_EDGE('',*,*,#32398,.F.);
#42699=ORIENTED_EDGE('',*,*,#32437,.F.);
#42700=ORIENTED_EDGE('',*,*,#32438,.T.);
#42701=ORIENTED_EDGE('',*,*,#32439,.T.);
#42702=ORIENTED_EDGE('',*,*,#32440,.F.);
#42703=ORIENTED_EDGE('',*,*,#32441,.F.);
#42704=ORIENTED_EDGE('',*,*,#32442,.T.);
#42705=ORIENTED_EDGE('',*,*,#32443,.T.);
#42706=ORIENTED_EDGE('',*,*,#32438,.F.);
#42707=ORIENTED_EDGE('',*,*,#32444,.F.);
#42708=ORIENTED_EDGE('',*,*,#32445,.T.);
#42709=ORIENTED_EDGE('',*,*,#32446,.T.);
#42710=ORIENTED_EDGE('',*,*,#32442,.F.);
#42711=ORIENTED_EDGE('',*,*,#32447,.F.);
#42712=ORIENTED_EDGE('',*,*,#32448,.T.);
#42713=ORIENTED_EDGE('',*,*,#32449,.T.);
#42714=ORIENTED_EDGE('',*,*,#32445,.F.);
#42715=ORIENTED_EDGE('',*,*,#32450,.F.);
#42716=ORIENTED_EDGE('',*,*,#32451,.T.);
#42717=ORIENTED_EDGE('',*,*,#32452,.T.);
#42718=ORIENTED_EDGE('',*,*,#32448,.F.);
#42719=ORIENTED_EDGE('',*,*,#32453,.F.);
#42720=ORIENTED_EDGE('',*,*,#32454,.T.);
#42721=ORIENTED_EDGE('',*,*,#32455,.T.);
#42722=ORIENTED_EDGE('',*,*,#32451,.F.);
#42723=ORIENTED_EDGE('',*,*,#32456,.F.);
#42724=ORIENTED_EDGE('',*,*,#32457,.T.);
#42725=ORIENTED_EDGE('',*,*,#32458,.T.);
#42726=ORIENTED_EDGE('',*,*,#32454,.F.);
#42727=ORIENTED_EDGE('',*,*,#32459,.F.);
#42728=ORIENTED_EDGE('',*,*,#32440,.T.);
#42729=ORIENTED_EDGE('',*,*,#32460,.T.);
#42730=ORIENTED_EDGE('',*,*,#32457,.F.);
#42731=ORIENTED_EDGE('',*,*,#32461,.F.);
#42732=ORIENTED_EDGE('',*,*,#32462,.T.);
#42733=ORIENTED_EDGE('',*,*,#32463,.T.);
#42734=ORIENTED_EDGE('',*,*,#32464,.F.);
#42735=ORIENTED_EDGE('',*,*,#32465,.F.);
#42736=ORIENTED_EDGE('',*,*,#32466,.T.);
#42737=ORIENTED_EDGE('',*,*,#32467,.T.);
#42738=ORIENTED_EDGE('',*,*,#32462,.F.);
#42739=ORIENTED_EDGE('',*,*,#32468,.F.);
#42740=ORIENTED_EDGE('',*,*,#32469,.T.);
#42741=ORIENTED_EDGE('',*,*,#32470,.T.);
#42742=ORIENTED_EDGE('',*,*,#32466,.F.);
#42743=ORIENTED_EDGE('',*,*,#32471,.F.);
#42744=ORIENTED_EDGE('',*,*,#32472,.T.);
#42745=ORIENTED_EDGE('',*,*,#32473,.T.);
#42746=ORIENTED_EDGE('',*,*,#32469,.F.);
#42747=ORIENTED_EDGE('',*,*,#32474,.F.);
#42748=ORIENTED_EDGE('',*,*,#32475,.T.);
#42749=ORIENTED_EDGE('',*,*,#32476,.T.);
#42750=ORIENTED_EDGE('',*,*,#32472,.F.);
#42751=ORIENTED_EDGE('',*,*,#32477,.F.);
#42752=ORIENTED_EDGE('',*,*,#32478,.T.);
#42753=ORIENTED_EDGE('',*,*,#32479,.T.);
#42754=ORIENTED_EDGE('',*,*,#32475,.F.);
#42755=ORIENTED_EDGE('',*,*,#32480,.F.);
#42756=ORIENTED_EDGE('',*,*,#32481,.T.);
#42757=ORIENTED_EDGE('',*,*,#32482,.T.);
#42758=ORIENTED_EDGE('',*,*,#32478,.F.);
#42759=ORIENTED_EDGE('',*,*,#32483,.F.);
#42760=ORIENTED_EDGE('',*,*,#32484,.T.);
#42761=ORIENTED_EDGE('',*,*,#32485,.T.);
#42762=ORIENTED_EDGE('',*,*,#32481,.F.);
#42763=ORIENTED_EDGE('',*,*,#32486,.F.);
#42764=ORIENTED_EDGE('',*,*,#32464,.T.);
#42765=ORIENTED_EDGE('',*,*,#32487,.T.);
#42766=ORIENTED_EDGE('',*,*,#32484,.F.);
#42767=ORIENTED_EDGE('',*,*,#32488,.F.);
#42768=ORIENTED_EDGE('',*,*,#32489,.T.);
#42769=ORIENTED_EDGE('',*,*,#32490,.T.);
#42770=ORIENTED_EDGE('',*,*,#32491,.F.);
#42771=ORIENTED_EDGE('',*,*,#32492,.F.);
#42772=ORIENTED_EDGE('',*,*,#32493,.T.);
#42773=ORIENTED_EDGE('',*,*,#32494,.T.);
#42774=ORIENTED_EDGE('',*,*,#32489,.F.);
#42775=ORIENTED_EDGE('',*,*,#32495,.F.);
#42776=ORIENTED_EDGE('',*,*,#32496,.T.);
#42777=ORIENTED_EDGE('',*,*,#32497,.T.);
#42778=ORIENTED_EDGE('',*,*,#32493,.F.);
#42779=ORIENTED_EDGE('',*,*,#32498,.F.);
#42780=ORIENTED_EDGE('',*,*,#32499,.T.);
#42781=ORIENTED_EDGE('',*,*,#32500,.T.);
#42782=ORIENTED_EDGE('',*,*,#32496,.F.);
#42783=ORIENTED_EDGE('',*,*,#32501,.F.);
#42784=ORIENTED_EDGE('',*,*,#32502,.T.);
#42785=ORIENTED_EDGE('',*,*,#32503,.T.);
#42786=ORIENTED_EDGE('',*,*,#32499,.F.);
#42787=ORIENTED_EDGE('',*,*,#32504,.F.);
#42788=ORIENTED_EDGE('',*,*,#32505,.T.);
#42789=ORIENTED_EDGE('',*,*,#32506,.T.);
#42790=ORIENTED_EDGE('',*,*,#32502,.F.);
#42791=ORIENTED_EDGE('',*,*,#32507,.F.);
#42792=ORIENTED_EDGE('',*,*,#32508,.T.);
#42793=ORIENTED_EDGE('',*,*,#32509,.T.);
#42794=ORIENTED_EDGE('',*,*,#32505,.F.);
#42795=ORIENTED_EDGE('',*,*,#32510,.F.);
#42796=ORIENTED_EDGE('',*,*,#32511,.T.);
#42797=ORIENTED_EDGE('',*,*,#32512,.T.);
#42798=ORIENTED_EDGE('',*,*,#32508,.F.);
#42799=ORIENTED_EDGE('',*,*,#32513,.F.);
#42800=ORIENTED_EDGE('',*,*,#32514,.T.);
#42801=ORIENTED_EDGE('',*,*,#32515,.T.);
#42802=ORIENTED_EDGE('',*,*,#32511,.F.);
#42803=ORIENTED_EDGE('',*,*,#32516,.F.);
#42804=ORIENTED_EDGE('',*,*,#32517,.T.);
#42805=ORIENTED_EDGE('',*,*,#32518,.T.);
#42806=ORIENTED_EDGE('',*,*,#32514,.F.);
#42807=ORIENTED_EDGE('',*,*,#32519,.F.);
#42808=ORIENTED_EDGE('',*,*,#32520,.T.);
#42809=ORIENTED_EDGE('',*,*,#32521,.T.);
#42810=ORIENTED_EDGE('',*,*,#32517,.F.);
#42811=ORIENTED_EDGE('',*,*,#32522,.F.);
#42812=ORIENTED_EDGE('',*,*,#32523,.T.);
#42813=ORIENTED_EDGE('',*,*,#32524,.T.);
#42814=ORIENTED_EDGE('',*,*,#32520,.F.);
#42815=ORIENTED_EDGE('',*,*,#32525,.F.);
#42816=ORIENTED_EDGE('',*,*,#32526,.T.);
#42817=ORIENTED_EDGE('',*,*,#32527,.T.);
#42818=ORIENTED_EDGE('',*,*,#32523,.F.);
#42819=ORIENTED_EDGE('',*,*,#32528,.F.);
#42820=ORIENTED_EDGE('',*,*,#32529,.T.);
#42821=ORIENTED_EDGE('',*,*,#32530,.T.);
#42822=ORIENTED_EDGE('',*,*,#32526,.F.);
#42823=ORIENTED_EDGE('',*,*,#32531,.F.);
#42824=ORIENTED_EDGE('',*,*,#32532,.T.);
#42825=ORIENTED_EDGE('',*,*,#32533,.T.);
#42826=ORIENTED_EDGE('',*,*,#32529,.F.);
#42827=ORIENTED_EDGE('',*,*,#32534,.F.);
#42828=ORIENTED_EDGE('',*,*,#32491,.T.);
#42829=ORIENTED_EDGE('',*,*,#32535,.T.);
#42830=ORIENTED_EDGE('',*,*,#32532,.F.);
#42831=ORIENTED_EDGE('',*,*,#32535,.F.);
#42832=ORIENTED_EDGE('',*,*,#32490,.F.);
#42833=ORIENTED_EDGE('',*,*,#32494,.F.);
#42834=ORIENTED_EDGE('',*,*,#32497,.F.);
#42835=ORIENTED_EDGE('',*,*,#32500,.F.);
#42836=ORIENTED_EDGE('',*,*,#32503,.F.);
#42837=ORIENTED_EDGE('',*,*,#32506,.F.);
#42838=ORIENTED_EDGE('',*,*,#32509,.F.);
#42839=ORIENTED_EDGE('',*,*,#32512,.F.);
#42840=ORIENTED_EDGE('',*,*,#32515,.F.);
#42841=ORIENTED_EDGE('',*,*,#32518,.F.);
#42842=ORIENTED_EDGE('',*,*,#32521,.F.);
#42843=ORIENTED_EDGE('',*,*,#32524,.F.);
#42844=ORIENTED_EDGE('',*,*,#32527,.F.);
#42845=ORIENTED_EDGE('',*,*,#32530,.F.);
#42846=ORIENTED_EDGE('',*,*,#32533,.F.);
#42847=ORIENTED_EDGE('',*,*,#32487,.F.);
#42848=ORIENTED_EDGE('',*,*,#32463,.F.);
#42849=ORIENTED_EDGE('',*,*,#32467,.F.);
#42850=ORIENTED_EDGE('',*,*,#32470,.F.);
#42851=ORIENTED_EDGE('',*,*,#32473,.F.);
#42852=ORIENTED_EDGE('',*,*,#32476,.F.);
#42853=ORIENTED_EDGE('',*,*,#32479,.F.);
#42854=ORIENTED_EDGE('',*,*,#32482,.F.);
#42855=ORIENTED_EDGE('',*,*,#32485,.F.);
#42856=ORIENTED_EDGE('',*,*,#32460,.F.);
#42857=ORIENTED_EDGE('',*,*,#32439,.F.);
#42858=ORIENTED_EDGE('',*,*,#32443,.F.);
#42859=ORIENTED_EDGE('',*,*,#32446,.F.);
#42860=ORIENTED_EDGE('',*,*,#32449,.F.);
#42861=ORIENTED_EDGE('',*,*,#32452,.F.);
#42862=ORIENTED_EDGE('',*,*,#32455,.F.);
#42863=ORIENTED_EDGE('',*,*,#32458,.F.);
#42864=ORIENTED_EDGE('',*,*,#32461,.T.);
#42865=ORIENTED_EDGE('',*,*,#32486,.T.);
#42866=ORIENTED_EDGE('',*,*,#32483,.T.);
#42867=ORIENTED_EDGE('',*,*,#32480,.T.);
#42868=ORIENTED_EDGE('',*,*,#32477,.T.);
#42869=ORIENTED_EDGE('',*,*,#32474,.T.);
#42870=ORIENTED_EDGE('',*,*,#32471,.T.);
#42871=ORIENTED_EDGE('',*,*,#32468,.T.);
#42872=ORIENTED_EDGE('',*,*,#32465,.T.);
#42873=ORIENTED_EDGE('',*,*,#32437,.T.);
#42874=ORIENTED_EDGE('',*,*,#32459,.T.);
#42875=ORIENTED_EDGE('',*,*,#32456,.T.);
#42876=ORIENTED_EDGE('',*,*,#32453,.T.);
#42877=ORIENTED_EDGE('',*,*,#32450,.T.);
#42878=ORIENTED_EDGE('',*,*,#32447,.T.);
#42879=ORIENTED_EDGE('',*,*,#32444,.T.);
#42880=ORIENTED_EDGE('',*,*,#32441,.T.);
#42881=ORIENTED_EDGE('',*,*,#32377,.T.);
#42882=ORIENTED_EDGE('',*,*,#32399,.T.);
#42883=ORIENTED_EDGE('',*,*,#32396,.T.);
#42884=ORIENTED_EDGE('',*,*,#32393,.T.);
#42885=ORIENTED_EDGE('',*,*,#32390,.T.);
#42886=ORIENTED_EDGE('',*,*,#32387,.T.);
#42887=ORIENTED_EDGE('',*,*,#32384,.T.);
#42888=ORIENTED_EDGE('',*,*,#32381,.T.);
#42889=ORIENTED_EDGE('',*,*,#32536,.F.);
#42890=ORIENTED_EDGE('',*,*,#32537,.T.);
#42891=ORIENTED_EDGE('',*,*,#32538,.T.);
#42892=ORIENTED_EDGE('',*,*,#32539,.F.);
#42893=ORIENTED_EDGE('',*,*,#32540,.F.);
#42894=ORIENTED_EDGE('',*,*,#32541,.T.);
#42895=ORIENTED_EDGE('',*,*,#32542,.T.);
#42896=ORIENTED_EDGE('',*,*,#32537,.F.);
#42897=ORIENTED_EDGE('',*,*,#32543,.F.);
#42898=ORIENTED_EDGE('',*,*,#32544,.T.);
#42899=ORIENTED_EDGE('',*,*,#32545,.T.);
#42900=ORIENTED_EDGE('',*,*,#32541,.F.);
#42901=ORIENTED_EDGE('',*,*,#32546,.F.);
#42902=ORIENTED_EDGE('',*,*,#32547,.T.);
#42903=ORIENTED_EDGE('',*,*,#32548,.T.);
#42904=ORIENTED_EDGE('',*,*,#32544,.F.);
#42905=ORIENTED_EDGE('',*,*,#32549,.F.);
#42906=ORIENTED_EDGE('',*,*,#32550,.T.);
#42907=ORIENTED_EDGE('',*,*,#32551,.T.);
#42908=ORIENTED_EDGE('',*,*,#32547,.F.);
#42909=ORIENTED_EDGE('',*,*,#32552,.F.);
#42910=ORIENTED_EDGE('',*,*,#32553,.T.);
#42911=ORIENTED_EDGE('',*,*,#32554,.T.);
#42912=ORIENTED_EDGE('',*,*,#32550,.F.);
#42913=ORIENTED_EDGE('',*,*,#32555,.F.);
#42914=ORIENTED_EDGE('',*,*,#32556,.T.);
#42915=ORIENTED_EDGE('',*,*,#32557,.T.);
#42916=ORIENTED_EDGE('',*,*,#32553,.F.);
#42917=ORIENTED_EDGE('',*,*,#32558,.F.);
#42918=ORIENTED_EDGE('',*,*,#32539,.T.);
#42919=ORIENTED_EDGE('',*,*,#32559,.T.);
#42920=ORIENTED_EDGE('',*,*,#32556,.F.);
#42921=ORIENTED_EDGE('',*,*,#32560,.F.);
#42922=ORIENTED_EDGE('',*,*,#32561,.T.);
#42923=ORIENTED_EDGE('',*,*,#32562,.T.);
#42924=ORIENTED_EDGE('',*,*,#32563,.F.);
#42925=ORIENTED_EDGE('',*,*,#32564,.F.);
#42926=ORIENTED_EDGE('',*,*,#32565,.T.);
#42927=ORIENTED_EDGE('',*,*,#32566,.T.);
#42928=ORIENTED_EDGE('',*,*,#32561,.F.);
#42929=ORIENTED_EDGE('',*,*,#32567,.F.);
#42930=ORIENTED_EDGE('',*,*,#32568,.T.);
#42931=ORIENTED_EDGE('',*,*,#32569,.T.);
#42932=ORIENTED_EDGE('',*,*,#32565,.F.);
#42933=ORIENTED_EDGE('',*,*,#32570,.F.);
#42934=ORIENTED_EDGE('',*,*,#32571,.T.);
#42935=ORIENTED_EDGE('',*,*,#32572,.T.);
#42936=ORIENTED_EDGE('',*,*,#32568,.F.);
#42937=ORIENTED_EDGE('',*,*,#32573,.F.);
#42938=ORIENTED_EDGE('',*,*,#32574,.T.);
#42939=ORIENTED_EDGE('',*,*,#32575,.T.);
#42940=ORIENTED_EDGE('',*,*,#32571,.F.);
#42941=ORIENTED_EDGE('',*,*,#32576,.F.);
#42942=ORIENTED_EDGE('',*,*,#32577,.T.);
#42943=ORIENTED_EDGE('',*,*,#32578,.T.);
#42944=ORIENTED_EDGE('',*,*,#32574,.F.);
#42945=ORIENTED_EDGE('',*,*,#32579,.F.);
#42946=ORIENTED_EDGE('',*,*,#32580,.T.);
#42947=ORIENTED_EDGE('',*,*,#32581,.T.);
#42948=ORIENTED_EDGE('',*,*,#32577,.F.);
#42949=ORIENTED_EDGE('',*,*,#32582,.F.);
#42950=ORIENTED_EDGE('',*,*,#32583,.T.);
#42951=ORIENTED_EDGE('',*,*,#32584,.T.);
#42952=ORIENTED_EDGE('',*,*,#32580,.F.);
#42953=ORIENTED_EDGE('',*,*,#32585,.F.);
#42954=ORIENTED_EDGE('',*,*,#32586,.T.);
#42955=ORIENTED_EDGE('',*,*,#32587,.T.);
#42956=ORIENTED_EDGE('',*,*,#32583,.F.);
#42957=ORIENTED_EDGE('',*,*,#32588,.F.);
#42958=ORIENTED_EDGE('',*,*,#32589,.T.);
#42959=ORIENTED_EDGE('',*,*,#32590,.T.);
#42960=ORIENTED_EDGE('',*,*,#32586,.F.);
#42961=ORIENTED_EDGE('',*,*,#32591,.F.);
#42962=ORIENTED_EDGE('',*,*,#32592,.T.);
#42963=ORIENTED_EDGE('',*,*,#32593,.T.);
#42964=ORIENTED_EDGE('',*,*,#32589,.F.);
#42965=ORIENTED_EDGE('',*,*,#32594,.F.);
#42966=ORIENTED_EDGE('',*,*,#32563,.T.);
#42967=ORIENTED_EDGE('',*,*,#32595,.T.);
#42968=ORIENTED_EDGE('',*,*,#32592,.F.);
#42969=ORIENTED_EDGE('',*,*,#32595,.F.);
#42970=ORIENTED_EDGE('',*,*,#32562,.F.);
#42971=ORIENTED_EDGE('',*,*,#32566,.F.);
#42972=ORIENTED_EDGE('',*,*,#32569,.F.);
#42973=ORIENTED_EDGE('',*,*,#32572,.F.);
#42974=ORIENTED_EDGE('',*,*,#32575,.F.);
#42975=ORIENTED_EDGE('',*,*,#32578,.F.);
#42976=ORIENTED_EDGE('',*,*,#32581,.F.);
#42977=ORIENTED_EDGE('',*,*,#32584,.F.);
#42978=ORIENTED_EDGE('',*,*,#32587,.F.);
#42979=ORIENTED_EDGE('',*,*,#32590,.F.);
#42980=ORIENTED_EDGE('',*,*,#32593,.F.);
#42981=ORIENTED_EDGE('',*,*,#32559,.F.);
#42982=ORIENTED_EDGE('',*,*,#32538,.F.);
#42983=ORIENTED_EDGE('',*,*,#32542,.F.);
#42984=ORIENTED_EDGE('',*,*,#32545,.F.);
#42985=ORIENTED_EDGE('',*,*,#32548,.F.);
#42986=ORIENTED_EDGE('',*,*,#32551,.F.);
#42987=ORIENTED_EDGE('',*,*,#32554,.F.);
#42988=ORIENTED_EDGE('',*,*,#32557,.F.);
#42989=ORIENTED_EDGE('',*,*,#32596,.F.);
#42990=ORIENTED_EDGE('',*,*,#32597,.T.);
#42991=ORIENTED_EDGE('',*,*,#32598,.T.);
#42992=ORIENTED_EDGE('',*,*,#32599,.F.);
#42993=ORIENTED_EDGE('',*,*,#32600,.F.);
#42994=ORIENTED_EDGE('',*,*,#32601,.T.);
#42995=ORIENTED_EDGE('',*,*,#32602,.T.);
#42996=ORIENTED_EDGE('',*,*,#32597,.F.);
#42997=ORIENTED_EDGE('',*,*,#32603,.F.);
#42998=ORIENTED_EDGE('',*,*,#32604,.T.);
#42999=ORIENTED_EDGE('',*,*,#32605,.T.);
#43000=ORIENTED_EDGE('',*,*,#32601,.F.);
#43001=ORIENTED_EDGE('',*,*,#32606,.F.);
#43002=ORIENTED_EDGE('',*,*,#32607,.T.);
#43003=ORIENTED_EDGE('',*,*,#32608,.T.);
#43004=ORIENTED_EDGE('',*,*,#32604,.F.);
#43005=ORIENTED_EDGE('',*,*,#32609,.F.);
#43006=ORIENTED_EDGE('',*,*,#32610,.T.);
#43007=ORIENTED_EDGE('',*,*,#32611,.T.);
#43008=ORIENTED_EDGE('',*,*,#32607,.F.);
#43009=ORIENTED_EDGE('',*,*,#32612,.F.);
#43010=ORIENTED_EDGE('',*,*,#32613,.T.);
#43011=ORIENTED_EDGE('',*,*,#32614,.T.);
#43012=ORIENTED_EDGE('',*,*,#32610,.F.);
#43013=ORIENTED_EDGE('',*,*,#32615,.F.);
#43014=ORIENTED_EDGE('',*,*,#32616,.T.);
#43015=ORIENTED_EDGE('',*,*,#32617,.T.);
#43016=ORIENTED_EDGE('',*,*,#32613,.F.);
#43017=ORIENTED_EDGE('',*,*,#32618,.F.);
#43018=ORIENTED_EDGE('',*,*,#32599,.T.);
#43019=ORIENTED_EDGE('',*,*,#32619,.T.);
#43020=ORIENTED_EDGE('',*,*,#32616,.F.);
#43021=ORIENTED_EDGE('',*,*,#32620,.F.);
#43022=ORIENTED_EDGE('',*,*,#32621,.T.);
#43023=ORIENTED_EDGE('',*,*,#32622,.T.);
#43024=ORIENTED_EDGE('',*,*,#32623,.F.);
#43025=ORIENTED_EDGE('',*,*,#32624,.F.);
#43026=ORIENTED_EDGE('',*,*,#32625,.T.);
#43027=ORIENTED_EDGE('',*,*,#32626,.T.);
#43028=ORIENTED_EDGE('',*,*,#32621,.F.);
#43029=ORIENTED_EDGE('',*,*,#32627,.F.);
#43030=ORIENTED_EDGE('',*,*,#32628,.T.);
#43031=ORIENTED_EDGE('',*,*,#32629,.T.);
#43032=ORIENTED_EDGE('',*,*,#32625,.F.);
#43033=ORIENTED_EDGE('',*,*,#32630,.F.);
#43034=ORIENTED_EDGE('',*,*,#32631,.T.);
#43035=ORIENTED_EDGE('',*,*,#32632,.T.);
#43036=ORIENTED_EDGE('',*,*,#32628,.F.);
#43037=ORIENTED_EDGE('',*,*,#32633,.F.);
#43038=ORIENTED_EDGE('',*,*,#32634,.T.);
#43039=ORIENTED_EDGE('',*,*,#32635,.T.);
#43040=ORIENTED_EDGE('',*,*,#32631,.F.);
#43041=ORIENTED_EDGE('',*,*,#32636,.F.);
#43042=ORIENTED_EDGE('',*,*,#32637,.T.);
#43043=ORIENTED_EDGE('',*,*,#32638,.T.);
#43044=ORIENTED_EDGE('',*,*,#32634,.F.);
#43045=ORIENTED_EDGE('',*,*,#32639,.F.);
#43046=ORIENTED_EDGE('',*,*,#32640,.T.);
#43047=ORIENTED_EDGE('',*,*,#32641,.T.);
#43048=ORIENTED_EDGE('',*,*,#32637,.F.);
#43049=ORIENTED_EDGE('',*,*,#32642,.F.);
#43050=ORIENTED_EDGE('',*,*,#32643,.T.);
#43051=ORIENTED_EDGE('',*,*,#32644,.T.);
#43052=ORIENTED_EDGE('',*,*,#32640,.F.);
#43053=ORIENTED_EDGE('',*,*,#32645,.F.);
#43054=ORIENTED_EDGE('',*,*,#32646,.T.);
#43055=ORIENTED_EDGE('',*,*,#32647,.T.);
#43056=ORIENTED_EDGE('',*,*,#32643,.F.);
#43057=ORIENTED_EDGE('',*,*,#32648,.F.);
#43058=ORIENTED_EDGE('',*,*,#32649,.T.);
#43059=ORIENTED_EDGE('',*,*,#32650,.T.);
#43060=ORIENTED_EDGE('',*,*,#32646,.F.);
#43061=ORIENTED_EDGE('',*,*,#32651,.F.);
#43062=ORIENTED_EDGE('',*,*,#32652,.T.);
#43063=ORIENTED_EDGE('',*,*,#32653,.T.);
#43064=ORIENTED_EDGE('',*,*,#32649,.F.);
#43065=ORIENTED_EDGE('',*,*,#32654,.F.);
#43066=ORIENTED_EDGE('',*,*,#32655,.T.);
#43067=ORIENTED_EDGE('',*,*,#32656,.T.);
#43068=ORIENTED_EDGE('',*,*,#32652,.F.);
#43069=ORIENTED_EDGE('',*,*,#32657,.F.);
#43070=ORIENTED_EDGE('',*,*,#32658,.T.);
#43071=ORIENTED_EDGE('',*,*,#32659,.T.);
#43072=ORIENTED_EDGE('',*,*,#32655,.F.);
#43073=ORIENTED_EDGE('',*,*,#32660,.F.);
#43074=ORIENTED_EDGE('',*,*,#32661,.T.);
#43075=ORIENTED_EDGE('',*,*,#32662,.T.);
#43076=ORIENTED_EDGE('',*,*,#32658,.F.);
#43077=ORIENTED_EDGE('',*,*,#32663,.F.);
#43078=ORIENTED_EDGE('',*,*,#32664,.T.);
#43079=ORIENTED_EDGE('',*,*,#32665,.T.);
#43080=ORIENTED_EDGE('',*,*,#32661,.F.);
#43081=ORIENTED_EDGE('',*,*,#32666,.F.);
#43082=ORIENTED_EDGE('',*,*,#32667,.T.);
#43083=ORIENTED_EDGE('',*,*,#32668,.T.);
#43084=ORIENTED_EDGE('',*,*,#32664,.F.);
#43085=ORIENTED_EDGE('',*,*,#32669,.F.);
#43086=ORIENTED_EDGE('',*,*,#32670,.T.);
#43087=ORIENTED_EDGE('',*,*,#32671,.T.);
#43088=ORIENTED_EDGE('',*,*,#32667,.F.);
#43089=ORIENTED_EDGE('',*,*,#32672,.F.);
#43090=ORIENTED_EDGE('',*,*,#32673,.T.);
#43091=ORIENTED_EDGE('',*,*,#32674,.T.);
#43092=ORIENTED_EDGE('',*,*,#32670,.F.);
#43093=ORIENTED_EDGE('',*,*,#32675,.F.);
#43094=ORIENTED_EDGE('',*,*,#32676,.T.);
#43095=ORIENTED_EDGE('',*,*,#32677,.T.);
#43096=ORIENTED_EDGE('',*,*,#32673,.F.);
#43097=ORIENTED_EDGE('',*,*,#32678,.F.);
#43098=ORIENTED_EDGE('',*,*,#32679,.T.);
#43099=ORIENTED_EDGE('',*,*,#32680,.T.);
#43100=ORIENTED_EDGE('',*,*,#32676,.F.);
#43101=ORIENTED_EDGE('',*,*,#32681,.F.);
#43102=ORIENTED_EDGE('',*,*,#32682,.T.);
#43103=ORIENTED_EDGE('',*,*,#32683,.T.);
#43104=ORIENTED_EDGE('',*,*,#32679,.F.);
#43105=ORIENTED_EDGE('',*,*,#32684,.F.);
#43106=ORIENTED_EDGE('',*,*,#32623,.T.);
#43107=ORIENTED_EDGE('',*,*,#32685,.T.);
#43108=ORIENTED_EDGE('',*,*,#32682,.F.);
#43109=ORIENTED_EDGE('',*,*,#32685,.F.);
#43110=ORIENTED_EDGE('',*,*,#32622,.F.);
#43111=ORIENTED_EDGE('',*,*,#32626,.F.);
#43112=ORIENTED_EDGE('',*,*,#32629,.F.);
#43113=ORIENTED_EDGE('',*,*,#32632,.F.);
#43114=ORIENTED_EDGE('',*,*,#32635,.F.);
#43115=ORIENTED_EDGE('',*,*,#32638,.F.);
#43116=ORIENTED_EDGE('',*,*,#32641,.F.);
#43117=ORIENTED_EDGE('',*,*,#32644,.F.);
#43118=ORIENTED_EDGE('',*,*,#32647,.F.);
#43119=ORIENTED_EDGE('',*,*,#32650,.F.);
#43120=ORIENTED_EDGE('',*,*,#32653,.F.);
#43121=ORIENTED_EDGE('',*,*,#32656,.F.);
#43122=ORIENTED_EDGE('',*,*,#32659,.F.);
#43123=ORIENTED_EDGE('',*,*,#32662,.F.);
#43124=ORIENTED_EDGE('',*,*,#32665,.F.);
#43125=ORIENTED_EDGE('',*,*,#32668,.F.);
#43126=ORIENTED_EDGE('',*,*,#32671,.F.);
#43127=ORIENTED_EDGE('',*,*,#32674,.F.);
#43128=ORIENTED_EDGE('',*,*,#32677,.F.);
#43129=ORIENTED_EDGE('',*,*,#32680,.F.);
#43130=ORIENTED_EDGE('',*,*,#32683,.F.);
#43131=ORIENTED_EDGE('',*,*,#32619,.F.);
#43132=ORIENTED_EDGE('',*,*,#32598,.F.);
#43133=ORIENTED_EDGE('',*,*,#32602,.F.);
#43134=ORIENTED_EDGE('',*,*,#32605,.F.);
#43135=ORIENTED_EDGE('',*,*,#32608,.F.);
#43136=ORIENTED_EDGE('',*,*,#32611,.F.);
#43137=ORIENTED_EDGE('',*,*,#32614,.F.);
#43138=ORIENTED_EDGE('',*,*,#32617,.F.);
#43139=ORIENTED_EDGE('',*,*,#32596,.T.);
#43140=ORIENTED_EDGE('',*,*,#32618,.T.);
#43141=ORIENTED_EDGE('',*,*,#32615,.T.);
#43142=ORIENTED_EDGE('',*,*,#32612,.T.);
#43143=ORIENTED_EDGE('',*,*,#32609,.T.);
#43144=ORIENTED_EDGE('',*,*,#32606,.T.);
#43145=ORIENTED_EDGE('',*,*,#32603,.T.);
#43146=ORIENTED_EDGE('',*,*,#32600,.T.);
#43147=ORIENTED_EDGE('',*,*,#32536,.T.);
#43148=ORIENTED_EDGE('',*,*,#32558,.T.);
#43149=ORIENTED_EDGE('',*,*,#32555,.T.);
#43150=ORIENTED_EDGE('',*,*,#32552,.T.);
#43151=ORIENTED_EDGE('',*,*,#32549,.T.);
#43152=ORIENTED_EDGE('',*,*,#32546,.T.);
#43153=ORIENTED_EDGE('',*,*,#32543,.T.);
#43154=ORIENTED_EDGE('',*,*,#32540,.T.);
#43155=ORIENTED_EDGE('',*,*,#32686,.F.);
#43156=ORIENTED_EDGE('',*,*,#32687,.T.);
#43157=ORIENTED_EDGE('',*,*,#32688,.T.);
#43158=ORIENTED_EDGE('',*,*,#32689,.F.);
#43159=ORIENTED_EDGE('',*,*,#32690,.F.);
#43160=ORIENTED_EDGE('',*,*,#32691,.T.);
#43161=ORIENTED_EDGE('',*,*,#32692,.T.);
#43162=ORIENTED_EDGE('',*,*,#32687,.F.);
#43163=ORIENTED_EDGE('',*,*,#32693,.F.);
#43164=ORIENTED_EDGE('',*,*,#32694,.T.);
#43165=ORIENTED_EDGE('',*,*,#32695,.T.);
#43166=ORIENTED_EDGE('',*,*,#32691,.F.);
#43167=ORIENTED_EDGE('',*,*,#32696,.F.);
#43168=ORIENTED_EDGE('',*,*,#32689,.T.);
#43169=ORIENTED_EDGE('',*,*,#32697,.T.);
#43170=ORIENTED_EDGE('',*,*,#32694,.F.);
#43171=ORIENTED_EDGE('',*,*,#32697,.F.);
#43172=ORIENTED_EDGE('',*,*,#32688,.F.);
#43173=ORIENTED_EDGE('',*,*,#32692,.F.);
#43174=ORIENTED_EDGE('',*,*,#32695,.F.);
#43175=ORIENTED_EDGE('',*,*,#32698,.F.);
#43176=ORIENTED_EDGE('',*,*,#32699,.T.);
#43177=ORIENTED_EDGE('',*,*,#32700,.T.);
#43178=ORIENTED_EDGE('',*,*,#32701,.F.);
#43179=ORIENTED_EDGE('',*,*,#32702,.F.);
#43180=ORIENTED_EDGE('',*,*,#32703,.T.);
#43181=ORIENTED_EDGE('',*,*,#32704,.T.);
#43182=ORIENTED_EDGE('',*,*,#32699,.F.);
#43183=ORIENTED_EDGE('',*,*,#32705,.F.);
#43184=ORIENTED_EDGE('',*,*,#32706,.T.);
#43185=ORIENTED_EDGE('',*,*,#32707,.T.);
#43186=ORIENTED_EDGE('',*,*,#32703,.F.);
#43187=ORIENTED_EDGE('',*,*,#32708,.F.);
#43188=ORIENTED_EDGE('',*,*,#32701,.T.);
#43189=ORIENTED_EDGE('',*,*,#32709,.T.);
#43190=ORIENTED_EDGE('',*,*,#32706,.F.);
#43191=ORIENTED_EDGE('',*,*,#32709,.F.);
#43192=ORIENTED_EDGE('',*,*,#32700,.F.);
#43193=ORIENTED_EDGE('',*,*,#32704,.F.);
#43194=ORIENTED_EDGE('',*,*,#32707,.F.);
#43195=ORIENTED_EDGE('',*,*,#32710,.F.);
#43196=ORIENTED_EDGE('',*,*,#32711,.T.);
#43197=ORIENTED_EDGE('',*,*,#32712,.T.);
#43198=ORIENTED_EDGE('',*,*,#32713,.F.);
#43199=ORIENTED_EDGE('',*,*,#32714,.F.);
#43200=ORIENTED_EDGE('',*,*,#32715,.T.);
#43201=ORIENTED_EDGE('',*,*,#32716,.T.);
#43202=ORIENTED_EDGE('',*,*,#32711,.F.);
#43203=ORIENTED_EDGE('',*,*,#32717,.F.);
#43204=ORIENTED_EDGE('',*,*,#32718,.T.);
#43205=ORIENTED_EDGE('',*,*,#32719,.T.);
#43206=ORIENTED_EDGE('',*,*,#32715,.F.);
#43207=ORIENTED_EDGE('',*,*,#32720,.F.);
#43208=ORIENTED_EDGE('',*,*,#32713,.T.);
#43209=ORIENTED_EDGE('',*,*,#32721,.T.);
#43210=ORIENTED_EDGE('',*,*,#32718,.F.);
#43211=ORIENTED_EDGE('',*,*,#32721,.F.);
#43212=ORIENTED_EDGE('',*,*,#32712,.F.);
#43213=ORIENTED_EDGE('',*,*,#32716,.F.);
#43214=ORIENTED_EDGE('',*,*,#32719,.F.);
#43215=ORIENTED_EDGE('',*,*,#32722,.F.);
#43216=ORIENTED_EDGE('',*,*,#32723,.T.);
#43217=ORIENTED_EDGE('',*,*,#32724,.T.);
#43218=ORIENTED_EDGE('',*,*,#32725,.F.);
#43219=ORIENTED_EDGE('',*,*,#32726,.F.);
#43220=ORIENTED_EDGE('',*,*,#32727,.T.);
#43221=ORIENTED_EDGE('',*,*,#32728,.T.);
#43222=ORIENTED_EDGE('',*,*,#32723,.F.);
#43223=ORIENTED_EDGE('',*,*,#32729,.F.);
#43224=ORIENTED_EDGE('',*,*,#32730,.T.);
#43225=ORIENTED_EDGE('',*,*,#32731,.T.);
#43226=ORIENTED_EDGE('',*,*,#32727,.F.);
#43227=ORIENTED_EDGE('',*,*,#32732,.F.);
#43228=ORIENTED_EDGE('',*,*,#32725,.T.);
#43229=ORIENTED_EDGE('',*,*,#32733,.T.);
#43230=ORIENTED_EDGE('',*,*,#32730,.F.);
#43231=ORIENTED_EDGE('',*,*,#32733,.F.);
#43232=ORIENTED_EDGE('',*,*,#32724,.F.);
#43233=ORIENTED_EDGE('',*,*,#32728,.F.);
#43234=ORIENTED_EDGE('',*,*,#32731,.F.);
#43235=ORIENTED_EDGE('',*,*,#32734,.F.);
#43236=ORIENTED_EDGE('',*,*,#32735,.T.);
#43237=ORIENTED_EDGE('',*,*,#32736,.T.);
#43238=ORIENTED_EDGE('',*,*,#32737,.F.);
#43239=ORIENTED_EDGE('',*,*,#32738,.F.);
#43240=ORIENTED_EDGE('',*,*,#32739,.T.);
#43241=ORIENTED_EDGE('',*,*,#32740,.T.);
#43242=ORIENTED_EDGE('',*,*,#32735,.F.);
#43243=ORIENTED_EDGE('',*,*,#32741,.F.);
#43244=ORIENTED_EDGE('',*,*,#32742,.T.);
#43245=ORIENTED_EDGE('',*,*,#32743,.T.);
#43246=ORIENTED_EDGE('',*,*,#32739,.F.);
#43247=ORIENTED_EDGE('',*,*,#32744,.F.);
#43248=ORIENTED_EDGE('',*,*,#32737,.T.);
#43249=ORIENTED_EDGE('',*,*,#32745,.T.);
#43250=ORIENTED_EDGE('',*,*,#32742,.F.);
#43251=ORIENTED_EDGE('',*,*,#32745,.F.);
#43252=ORIENTED_EDGE('',*,*,#32736,.F.);
#43253=ORIENTED_EDGE('',*,*,#32740,.F.);
#43254=ORIENTED_EDGE('',*,*,#32743,.F.);
#43255=ORIENTED_EDGE('',*,*,#32746,.F.);
#43256=ORIENTED_EDGE('',*,*,#32747,.T.);
#43257=ORIENTED_EDGE('',*,*,#32748,.T.);
#43258=ORIENTED_EDGE('',*,*,#32749,.F.);
#43259=ORIENTED_EDGE('',*,*,#32750,.F.);
#43260=ORIENTED_EDGE('',*,*,#32751,.T.);
#43261=ORIENTED_EDGE('',*,*,#32752,.T.);
#43262=ORIENTED_EDGE('',*,*,#32747,.F.);
#43263=ORIENTED_EDGE('',*,*,#32753,.F.);
#43264=ORIENTED_EDGE('',*,*,#32754,.T.);
#43265=ORIENTED_EDGE('',*,*,#32755,.T.);
#43266=ORIENTED_EDGE('',*,*,#32751,.F.);
#43267=ORIENTED_EDGE('',*,*,#32756,.F.);
#43268=ORIENTED_EDGE('',*,*,#32749,.T.);
#43269=ORIENTED_EDGE('',*,*,#32757,.T.);
#43270=ORIENTED_EDGE('',*,*,#32754,.F.);
#43271=ORIENTED_EDGE('',*,*,#32757,.F.);
#43272=ORIENTED_EDGE('',*,*,#32748,.F.);
#43273=ORIENTED_EDGE('',*,*,#32752,.F.);
#43274=ORIENTED_EDGE('',*,*,#32755,.F.);
#43275=ORIENTED_EDGE('',*,*,#32758,.F.);
#43276=ORIENTED_EDGE('',*,*,#32759,.T.);
#43277=ORIENTED_EDGE('',*,*,#32760,.T.);
#43278=ORIENTED_EDGE('',*,*,#32761,.F.);
#43279=ORIENTED_EDGE('',*,*,#32762,.F.);
#43280=ORIENTED_EDGE('',*,*,#32763,.T.);
#43281=ORIENTED_EDGE('',*,*,#32764,.T.);
#43282=ORIENTED_EDGE('',*,*,#32759,.F.);
#43283=ORIENTED_EDGE('',*,*,#32765,.F.);
#43284=ORIENTED_EDGE('',*,*,#32766,.T.);
#43285=ORIENTED_EDGE('',*,*,#32767,.T.);
#43286=ORIENTED_EDGE('',*,*,#32763,.F.);
#43287=ORIENTED_EDGE('',*,*,#32768,.F.);
#43288=ORIENTED_EDGE('',*,*,#32761,.T.);
#43289=ORIENTED_EDGE('',*,*,#32769,.T.);
#43290=ORIENTED_EDGE('',*,*,#32766,.F.);
#43291=ORIENTED_EDGE('',*,*,#32769,.F.);
#43292=ORIENTED_EDGE('',*,*,#32760,.F.);
#43293=ORIENTED_EDGE('',*,*,#32764,.F.);
#43294=ORIENTED_EDGE('',*,*,#32767,.F.);
#43295=ORIENTED_EDGE('',*,*,#32770,.F.);
#43296=ORIENTED_EDGE('',*,*,#32771,.T.);
#43297=ORIENTED_EDGE('',*,*,#32772,.T.);
#43298=ORIENTED_EDGE('',*,*,#32773,.F.);
#43299=ORIENTED_EDGE('',*,*,#32774,.F.);
#43300=ORIENTED_EDGE('',*,*,#32775,.T.);
#43301=ORIENTED_EDGE('',*,*,#32776,.T.);
#43302=ORIENTED_EDGE('',*,*,#32771,.F.);
#43303=ORIENTED_EDGE('',*,*,#32777,.F.);
#43304=ORIENTED_EDGE('',*,*,#32778,.T.);
#43305=ORIENTED_EDGE('',*,*,#32779,.T.);
#43306=ORIENTED_EDGE('',*,*,#32775,.F.);
#43307=ORIENTED_EDGE('',*,*,#32780,.F.);
#43308=ORIENTED_EDGE('',*,*,#32773,.T.);
#43309=ORIENTED_EDGE('',*,*,#32781,.T.);
#43310=ORIENTED_EDGE('',*,*,#32778,.F.);
#43311=ORIENTED_EDGE('',*,*,#32781,.F.);
#43312=ORIENTED_EDGE('',*,*,#32772,.F.);
#43313=ORIENTED_EDGE('',*,*,#32776,.F.);
#43314=ORIENTED_EDGE('',*,*,#32779,.F.);
#43315=ORIENTED_EDGE('',*,*,#32782,.F.);
#43316=ORIENTED_EDGE('',*,*,#32783,.T.);
#43317=ORIENTED_EDGE('',*,*,#32784,.T.);
#43318=ORIENTED_EDGE('',*,*,#32785,.F.);
#43319=ORIENTED_EDGE('',*,*,#32786,.F.);
#43320=ORIENTED_EDGE('',*,*,#32787,.T.);
#43321=ORIENTED_EDGE('',*,*,#32788,.T.);
#43322=ORIENTED_EDGE('',*,*,#32783,.F.);
#43323=ORIENTED_EDGE('',*,*,#32789,.F.);
#43324=ORIENTED_EDGE('',*,*,#32790,.T.);
#43325=ORIENTED_EDGE('',*,*,#32791,.T.);
#43326=ORIENTED_EDGE('',*,*,#32787,.F.);
#43327=ORIENTED_EDGE('',*,*,#32792,.F.);
#43328=ORIENTED_EDGE('',*,*,#32785,.T.);
#43329=ORIENTED_EDGE('',*,*,#32793,.T.);
#43330=ORIENTED_EDGE('',*,*,#32790,.F.);
#43331=ORIENTED_EDGE('',*,*,#32793,.F.);
#43332=ORIENTED_EDGE('',*,*,#32784,.F.);
#43333=ORIENTED_EDGE('',*,*,#32788,.F.);
#43334=ORIENTED_EDGE('',*,*,#32791,.F.);
#43335=ORIENTED_EDGE('',*,*,#32794,.F.);
#43336=ORIENTED_EDGE('',*,*,#32795,.T.);
#43337=ORIENTED_EDGE('',*,*,#32796,.T.);
#43338=ORIENTED_EDGE('',*,*,#32797,.F.);
#43339=ORIENTED_EDGE('',*,*,#32798,.F.);
#43340=ORIENTED_EDGE('',*,*,#32799,.T.);
#43341=ORIENTED_EDGE('',*,*,#32800,.T.);
#43342=ORIENTED_EDGE('',*,*,#32795,.F.);
#43343=ORIENTED_EDGE('',*,*,#32801,.F.);
#43344=ORIENTED_EDGE('',*,*,#32802,.T.);
#43345=ORIENTED_EDGE('',*,*,#32803,.T.);
#43346=ORIENTED_EDGE('',*,*,#32799,.F.);
#43347=ORIENTED_EDGE('',*,*,#32804,.F.);
#43348=ORIENTED_EDGE('',*,*,#32797,.T.);
#43349=ORIENTED_EDGE('',*,*,#32805,.T.);
#43350=ORIENTED_EDGE('',*,*,#32802,.F.);
#43351=ORIENTED_EDGE('',*,*,#32805,.F.);
#43352=ORIENTED_EDGE('',*,*,#32796,.F.);
#43353=ORIENTED_EDGE('',*,*,#32800,.F.);
#43354=ORIENTED_EDGE('',*,*,#32803,.F.);
#43355=ORIENTED_EDGE('',*,*,#32806,.F.);
#43356=ORIENTED_EDGE('',*,*,#32807,.T.);
#43357=ORIENTED_EDGE('',*,*,#32808,.T.);
#43358=ORIENTED_EDGE('',*,*,#32809,.F.);
#43359=ORIENTED_EDGE('',*,*,#32810,.F.);
#43360=ORIENTED_EDGE('',*,*,#32811,.T.);
#43361=ORIENTED_EDGE('',*,*,#32812,.T.);
#43362=ORIENTED_EDGE('',*,*,#32807,.F.);
#43363=ORIENTED_EDGE('',*,*,#32813,.F.);
#43364=ORIENTED_EDGE('',*,*,#32814,.T.);
#43365=ORIENTED_EDGE('',*,*,#32815,.T.);
#43366=ORIENTED_EDGE('',*,*,#32811,.F.);
#43367=ORIENTED_EDGE('',*,*,#32816,.F.);
#43368=ORIENTED_EDGE('',*,*,#32809,.T.);
#43369=ORIENTED_EDGE('',*,*,#32817,.T.);
#43370=ORIENTED_EDGE('',*,*,#32814,.F.);
#43371=ORIENTED_EDGE('',*,*,#32817,.F.);
#43372=ORIENTED_EDGE('',*,*,#32808,.F.);
#43373=ORIENTED_EDGE('',*,*,#32812,.F.);
#43374=ORIENTED_EDGE('',*,*,#32815,.F.);
#43375=ORIENTED_EDGE('',*,*,#32818,.F.);
#43376=ORIENTED_EDGE('',*,*,#32819,.T.);
#43377=ORIENTED_EDGE('',*,*,#32820,.T.);
#43378=ORIENTED_EDGE('',*,*,#32821,.F.);
#43379=ORIENTED_EDGE('',*,*,#32822,.F.);
#43380=ORIENTED_EDGE('',*,*,#32823,.T.);
#43381=ORIENTED_EDGE('',*,*,#32824,.T.);
#43382=ORIENTED_EDGE('',*,*,#32819,.F.);
#43383=ORIENTED_EDGE('',*,*,#32825,.F.);
#43384=ORIENTED_EDGE('',*,*,#32826,.T.);
#43385=ORIENTED_EDGE('',*,*,#32827,.T.);
#43386=ORIENTED_EDGE('',*,*,#32823,.F.);
#43387=ORIENTED_EDGE('',*,*,#32828,.F.);
#43388=ORIENTED_EDGE('',*,*,#32821,.T.);
#43389=ORIENTED_EDGE('',*,*,#32829,.T.);
#43390=ORIENTED_EDGE('',*,*,#32826,.F.);
#43391=ORIENTED_EDGE('',*,*,#32829,.F.);
#43392=ORIENTED_EDGE('',*,*,#32820,.F.);
#43393=ORIENTED_EDGE('',*,*,#32824,.F.);
#43394=ORIENTED_EDGE('',*,*,#32827,.F.);
#43395=ORIENTED_EDGE('',*,*,#32830,.F.);
#43396=ORIENTED_EDGE('',*,*,#32831,.T.);
#43397=ORIENTED_EDGE('',*,*,#32832,.T.);
#43398=ORIENTED_EDGE('',*,*,#32833,.F.);
#43399=ORIENTED_EDGE('',*,*,#32834,.F.);
#43400=ORIENTED_EDGE('',*,*,#32835,.T.);
#43401=ORIENTED_EDGE('',*,*,#32836,.T.);
#43402=ORIENTED_EDGE('',*,*,#32831,.F.);
#43403=ORIENTED_EDGE('',*,*,#32837,.F.);
#43404=ORIENTED_EDGE('',*,*,#32838,.T.);
#43405=ORIENTED_EDGE('',*,*,#32839,.T.);
#43406=ORIENTED_EDGE('',*,*,#32835,.F.);
#43407=ORIENTED_EDGE('',*,*,#32840,.F.);
#43408=ORIENTED_EDGE('',*,*,#32833,.T.);
#43409=ORIENTED_EDGE('',*,*,#32841,.T.);
#43410=ORIENTED_EDGE('',*,*,#32838,.F.);
#43411=ORIENTED_EDGE('',*,*,#32841,.F.);
#43412=ORIENTED_EDGE('',*,*,#32832,.F.);
#43413=ORIENTED_EDGE('',*,*,#32836,.F.);
#43414=ORIENTED_EDGE('',*,*,#32839,.F.);
#43415=ORIENTED_EDGE('',*,*,#32842,.F.);
#43416=ORIENTED_EDGE('',*,*,#32843,.T.);
#43417=ORIENTED_EDGE('',*,*,#32844,.T.);
#43418=ORIENTED_EDGE('',*,*,#32845,.F.);
#43419=ORIENTED_EDGE('',*,*,#32846,.F.);
#43420=ORIENTED_EDGE('',*,*,#32847,.T.);
#43421=ORIENTED_EDGE('',*,*,#32848,.T.);
#43422=ORIENTED_EDGE('',*,*,#32843,.F.);
#43423=ORIENTED_EDGE('',*,*,#32849,.F.);
#43424=ORIENTED_EDGE('',*,*,#32850,.T.);
#43425=ORIENTED_EDGE('',*,*,#32851,.T.);
#43426=ORIENTED_EDGE('',*,*,#32847,.F.);
#43427=ORIENTED_EDGE('',*,*,#32852,.F.);
#43428=ORIENTED_EDGE('',*,*,#32845,.T.);
#43429=ORIENTED_EDGE('',*,*,#32853,.T.);
#43430=ORIENTED_EDGE('',*,*,#32850,.F.);
#43431=ORIENTED_EDGE('',*,*,#32853,.F.);
#43432=ORIENTED_EDGE('',*,*,#32844,.F.);
#43433=ORIENTED_EDGE('',*,*,#32848,.F.);
#43434=ORIENTED_EDGE('',*,*,#32851,.F.);
#43435=ORIENTED_EDGE('',*,*,#32854,.F.);
#43436=ORIENTED_EDGE('',*,*,#32855,.T.);
#43437=ORIENTED_EDGE('',*,*,#32856,.T.);
#43438=ORIENTED_EDGE('',*,*,#32857,.F.);
#43439=ORIENTED_EDGE('',*,*,#32858,.F.);
#43440=ORIENTED_EDGE('',*,*,#32859,.T.);
#43441=ORIENTED_EDGE('',*,*,#32860,.T.);
#43442=ORIENTED_EDGE('',*,*,#32855,.F.);
#43443=ORIENTED_EDGE('',*,*,#32861,.F.);
#43444=ORIENTED_EDGE('',*,*,#32862,.T.);
#43445=ORIENTED_EDGE('',*,*,#32863,.T.);
#43446=ORIENTED_EDGE('',*,*,#32859,.F.);
#43447=ORIENTED_EDGE('',*,*,#32864,.F.);
#43448=ORIENTED_EDGE('',*,*,#32857,.T.);
#43449=ORIENTED_EDGE('',*,*,#32865,.T.);
#43450=ORIENTED_EDGE('',*,*,#32862,.F.);
#43451=ORIENTED_EDGE('',*,*,#32865,.F.);
#43452=ORIENTED_EDGE('',*,*,#32856,.F.);
#43453=ORIENTED_EDGE('',*,*,#32860,.F.);
#43454=ORIENTED_EDGE('',*,*,#32863,.F.);
#43455=ORIENTED_EDGE('',*,*,#32866,.F.);
#43456=ORIENTED_EDGE('',*,*,#32867,.T.);
#43457=ORIENTED_EDGE('',*,*,#32868,.T.);
#43458=ORIENTED_EDGE('',*,*,#32869,.F.);
#43459=ORIENTED_EDGE('',*,*,#32870,.F.);
#43460=ORIENTED_EDGE('',*,*,#32871,.T.);
#43461=ORIENTED_EDGE('',*,*,#32872,.T.);
#43462=ORIENTED_EDGE('',*,*,#32867,.F.);
#43463=ORIENTED_EDGE('',*,*,#32873,.F.);
#43464=ORIENTED_EDGE('',*,*,#32874,.T.);
#43465=ORIENTED_EDGE('',*,*,#32875,.T.);
#43466=ORIENTED_EDGE('',*,*,#32871,.F.);
#43467=ORIENTED_EDGE('',*,*,#32876,.F.);
#43468=ORIENTED_EDGE('',*,*,#32869,.T.);
#43469=ORIENTED_EDGE('',*,*,#32877,.T.);
#43470=ORIENTED_EDGE('',*,*,#32874,.F.);
#43471=ORIENTED_EDGE('',*,*,#32877,.F.);
#43472=ORIENTED_EDGE('',*,*,#32868,.F.);
#43473=ORIENTED_EDGE('',*,*,#32872,.F.);
#43474=ORIENTED_EDGE('',*,*,#32875,.F.);
#43475=ORIENTED_EDGE('',*,*,#32878,.F.);
#43476=ORIENTED_EDGE('',*,*,#32879,.T.);
#43477=ORIENTED_EDGE('',*,*,#32880,.T.);
#43478=ORIENTED_EDGE('',*,*,#32881,.F.);
#43479=ORIENTED_EDGE('',*,*,#32882,.F.);
#43480=ORIENTED_EDGE('',*,*,#32883,.T.);
#43481=ORIENTED_EDGE('',*,*,#32884,.T.);
#43482=ORIENTED_EDGE('',*,*,#32879,.F.);
#43483=ORIENTED_EDGE('',*,*,#32885,.F.);
#43484=ORIENTED_EDGE('',*,*,#32886,.T.);
#43485=ORIENTED_EDGE('',*,*,#32887,.T.);
#43486=ORIENTED_EDGE('',*,*,#32883,.F.);
#43487=ORIENTED_EDGE('',*,*,#32888,.F.);
#43488=ORIENTED_EDGE('',*,*,#32881,.T.);
#43489=ORIENTED_EDGE('',*,*,#32889,.T.);
#43490=ORIENTED_EDGE('',*,*,#32886,.F.);
#43491=ORIENTED_EDGE('',*,*,#32889,.F.);
#43492=ORIENTED_EDGE('',*,*,#32880,.F.);
#43493=ORIENTED_EDGE('',*,*,#32884,.F.);
#43494=ORIENTED_EDGE('',*,*,#32887,.F.);
#43495=ORIENTED_EDGE('',*,*,#32890,.F.);
#43496=ORIENTED_EDGE('',*,*,#32891,.T.);
#43497=ORIENTED_EDGE('',*,*,#32892,.T.);
#43498=ORIENTED_EDGE('',*,*,#32893,.F.);
#43499=ORIENTED_EDGE('',*,*,#32894,.F.);
#43500=ORIENTED_EDGE('',*,*,#32895,.T.);
#43501=ORIENTED_EDGE('',*,*,#32896,.T.);
#43502=ORIENTED_EDGE('',*,*,#32891,.F.);
#43503=ORIENTED_EDGE('',*,*,#32897,.F.);
#43504=ORIENTED_EDGE('',*,*,#32898,.T.);
#43505=ORIENTED_EDGE('',*,*,#32899,.T.);
#43506=ORIENTED_EDGE('',*,*,#32895,.F.);
#43507=ORIENTED_EDGE('',*,*,#32900,.F.);
#43508=ORIENTED_EDGE('',*,*,#32893,.T.);
#43509=ORIENTED_EDGE('',*,*,#32901,.T.);
#43510=ORIENTED_EDGE('',*,*,#32898,.F.);
#43511=ORIENTED_EDGE('',*,*,#32901,.F.);
#43512=ORIENTED_EDGE('',*,*,#32892,.F.);
#43513=ORIENTED_EDGE('',*,*,#32896,.F.);
#43514=ORIENTED_EDGE('',*,*,#32899,.F.);
#43515=ORIENTED_EDGE('',*,*,#32902,.F.);
#43516=ORIENTED_EDGE('',*,*,#32903,.T.);
#43517=ORIENTED_EDGE('',*,*,#32904,.T.);
#43518=ORIENTED_EDGE('',*,*,#32905,.F.);
#43519=ORIENTED_EDGE('',*,*,#32906,.F.);
#43520=ORIENTED_EDGE('',*,*,#32907,.T.);
#43521=ORIENTED_EDGE('',*,*,#32908,.T.);
#43522=ORIENTED_EDGE('',*,*,#32903,.F.);
#43523=ORIENTED_EDGE('',*,*,#32909,.F.);
#43524=ORIENTED_EDGE('',*,*,#32910,.T.);
#43525=ORIENTED_EDGE('',*,*,#32911,.T.);
#43526=ORIENTED_EDGE('',*,*,#32907,.F.);
#43527=ORIENTED_EDGE('',*,*,#32912,.F.);
#43528=ORIENTED_EDGE('',*,*,#32905,.T.);
#43529=ORIENTED_EDGE('',*,*,#32913,.T.);
#43530=ORIENTED_EDGE('',*,*,#32910,.F.);
#43531=ORIENTED_EDGE('',*,*,#32913,.F.);
#43532=ORIENTED_EDGE('',*,*,#32904,.F.);
#43533=ORIENTED_EDGE('',*,*,#32908,.F.);
#43534=ORIENTED_EDGE('',*,*,#32911,.F.);
#43535=ORIENTED_EDGE('',*,*,#32914,.F.);
#43536=ORIENTED_EDGE('',*,*,#32915,.T.);
#43537=ORIENTED_EDGE('',*,*,#32916,.T.);
#43538=ORIENTED_EDGE('',*,*,#32917,.F.);
#43539=ORIENTED_EDGE('',*,*,#32918,.F.);
#43540=ORIENTED_EDGE('',*,*,#32919,.T.);
#43541=ORIENTED_EDGE('',*,*,#32920,.T.);
#43542=ORIENTED_EDGE('',*,*,#32915,.F.);
#43543=ORIENTED_EDGE('',*,*,#32921,.F.);
#43544=ORIENTED_EDGE('',*,*,#32922,.T.);
#43545=ORIENTED_EDGE('',*,*,#32923,.T.);
#43546=ORIENTED_EDGE('',*,*,#32919,.F.);
#43547=ORIENTED_EDGE('',*,*,#32924,.F.);
#43548=ORIENTED_EDGE('',*,*,#32917,.T.);
#43549=ORIENTED_EDGE('',*,*,#32925,.T.);
#43550=ORIENTED_EDGE('',*,*,#32922,.F.);
#43551=ORIENTED_EDGE('',*,*,#32925,.F.);
#43552=ORIENTED_EDGE('',*,*,#32916,.F.);
#43553=ORIENTED_EDGE('',*,*,#32920,.F.);
#43554=ORIENTED_EDGE('',*,*,#32923,.F.);
#43555=ORIENTED_EDGE('',*,*,#32926,.F.);
#43556=ORIENTED_EDGE('',*,*,#32927,.T.);
#43557=ORIENTED_EDGE('',*,*,#32928,.T.);
#43558=ORIENTED_EDGE('',*,*,#32929,.F.);
#43559=ORIENTED_EDGE('',*,*,#32930,.F.);
#43560=ORIENTED_EDGE('',*,*,#32931,.T.);
#43561=ORIENTED_EDGE('',*,*,#32932,.T.);
#43562=ORIENTED_EDGE('',*,*,#32927,.F.);
#43563=ORIENTED_EDGE('',*,*,#32933,.F.);
#43564=ORIENTED_EDGE('',*,*,#32934,.T.);
#43565=ORIENTED_EDGE('',*,*,#32935,.T.);
#43566=ORIENTED_EDGE('',*,*,#32931,.F.);
#43567=ORIENTED_EDGE('',*,*,#32936,.F.);
#43568=ORIENTED_EDGE('',*,*,#32929,.T.);
#43569=ORIENTED_EDGE('',*,*,#32937,.T.);
#43570=ORIENTED_EDGE('',*,*,#32934,.F.);
#43571=ORIENTED_EDGE('',*,*,#32937,.F.);
#43572=ORIENTED_EDGE('',*,*,#32928,.F.);
#43573=ORIENTED_EDGE('',*,*,#32932,.F.);
#43574=ORIENTED_EDGE('',*,*,#32935,.F.);
#43575=ORIENTED_EDGE('',*,*,#32938,.F.);
#43576=ORIENTED_EDGE('',*,*,#32939,.T.);
#43577=ORIENTED_EDGE('',*,*,#32940,.T.);
#43578=ORIENTED_EDGE('',*,*,#32941,.F.);
#43579=ORIENTED_EDGE('',*,*,#32942,.F.);
#43580=ORIENTED_EDGE('',*,*,#32943,.T.);
#43581=ORIENTED_EDGE('',*,*,#32944,.T.);
#43582=ORIENTED_EDGE('',*,*,#32939,.F.);
#43583=ORIENTED_EDGE('',*,*,#32945,.F.);
#43584=ORIENTED_EDGE('',*,*,#32946,.T.);
#43585=ORIENTED_EDGE('',*,*,#32947,.T.);
#43586=ORIENTED_EDGE('',*,*,#32943,.F.);
#43587=ORIENTED_EDGE('',*,*,#32948,.F.);
#43588=ORIENTED_EDGE('',*,*,#32941,.T.);
#43589=ORIENTED_EDGE('',*,*,#32949,.T.);
#43590=ORIENTED_EDGE('',*,*,#32946,.F.);
#43591=ORIENTED_EDGE('',*,*,#32949,.F.);
#43592=ORIENTED_EDGE('',*,*,#32940,.F.);
#43593=ORIENTED_EDGE('',*,*,#32944,.F.);
#43594=ORIENTED_EDGE('',*,*,#32947,.F.);
#43595=ORIENTED_EDGE('',*,*,#32950,.F.);
#43596=ORIENTED_EDGE('',*,*,#32951,.T.);
#43597=ORIENTED_EDGE('',*,*,#32952,.T.);
#43598=ORIENTED_EDGE('',*,*,#32953,.F.);
#43599=ORIENTED_EDGE('',*,*,#32954,.F.);
#43600=ORIENTED_EDGE('',*,*,#32955,.T.);
#43601=ORIENTED_EDGE('',*,*,#32956,.T.);
#43602=ORIENTED_EDGE('',*,*,#32951,.F.);
#43603=ORIENTED_EDGE('',*,*,#32957,.F.);
#43604=ORIENTED_EDGE('',*,*,#32958,.T.);
#43605=ORIENTED_EDGE('',*,*,#32959,.T.);
#43606=ORIENTED_EDGE('',*,*,#32955,.F.);
#43607=ORIENTED_EDGE('',*,*,#32960,.F.);
#43608=ORIENTED_EDGE('',*,*,#32953,.T.);
#43609=ORIENTED_EDGE('',*,*,#32961,.T.);
#43610=ORIENTED_EDGE('',*,*,#32958,.F.);
#43611=ORIENTED_EDGE('',*,*,#32961,.F.);
#43612=ORIENTED_EDGE('',*,*,#32952,.F.);
#43613=ORIENTED_EDGE('',*,*,#32956,.F.);
#43614=ORIENTED_EDGE('',*,*,#32959,.F.);
#43615=ORIENTED_EDGE('',*,*,#32962,.F.);
#43616=ORIENTED_EDGE('',*,*,#32963,.T.);
#43617=ORIENTED_EDGE('',*,*,#32964,.T.);
#43618=ORIENTED_EDGE('',*,*,#32965,.F.);
#43619=ORIENTED_EDGE('',*,*,#32966,.F.);
#43620=ORIENTED_EDGE('',*,*,#32967,.T.);
#43621=ORIENTED_EDGE('',*,*,#32968,.T.);
#43622=ORIENTED_EDGE('',*,*,#32963,.F.);
#43623=ORIENTED_EDGE('',*,*,#32969,.F.);
#43624=ORIENTED_EDGE('',*,*,#32970,.T.);
#43625=ORIENTED_EDGE('',*,*,#32971,.T.);
#43626=ORIENTED_EDGE('',*,*,#32967,.F.);
#43627=ORIENTED_EDGE('',*,*,#32972,.F.);
#43628=ORIENTED_EDGE('',*,*,#32965,.T.);
#43629=ORIENTED_EDGE('',*,*,#32973,.T.);
#43630=ORIENTED_EDGE('',*,*,#32970,.F.);
#43631=ORIENTED_EDGE('',*,*,#32973,.F.);
#43632=ORIENTED_EDGE('',*,*,#32964,.F.);
#43633=ORIENTED_EDGE('',*,*,#32968,.F.);
#43634=ORIENTED_EDGE('',*,*,#32971,.F.);
#43635=ORIENTED_EDGE('',*,*,#32974,.F.);
#43636=ORIENTED_EDGE('',*,*,#32975,.T.);
#43637=ORIENTED_EDGE('',*,*,#32976,.T.);
#43638=ORIENTED_EDGE('',*,*,#32977,.F.);
#43639=ORIENTED_EDGE('',*,*,#32978,.F.);
#43640=ORIENTED_EDGE('',*,*,#32979,.T.);
#43641=ORIENTED_EDGE('',*,*,#32980,.T.);
#43642=ORIENTED_EDGE('',*,*,#32975,.F.);
#43643=ORIENTED_EDGE('',*,*,#32981,.F.);
#43644=ORIENTED_EDGE('',*,*,#32982,.T.);
#43645=ORIENTED_EDGE('',*,*,#32983,.T.);
#43646=ORIENTED_EDGE('',*,*,#32979,.F.);
#43647=ORIENTED_EDGE('',*,*,#32984,.F.);
#43648=ORIENTED_EDGE('',*,*,#32977,.T.);
#43649=ORIENTED_EDGE('',*,*,#32985,.T.);
#43650=ORIENTED_EDGE('',*,*,#32982,.F.);
#43651=ORIENTED_EDGE('',*,*,#32985,.F.);
#43652=ORIENTED_EDGE('',*,*,#32976,.F.);
#43653=ORIENTED_EDGE('',*,*,#32980,.F.);
#43654=ORIENTED_EDGE('',*,*,#32983,.F.);
#43655=ORIENTED_EDGE('',*,*,#32986,.F.);
#43656=ORIENTED_EDGE('',*,*,#32987,.T.);
#43657=ORIENTED_EDGE('',*,*,#32988,.T.);
#43658=ORIENTED_EDGE('',*,*,#32989,.F.);
#43659=ORIENTED_EDGE('',*,*,#32990,.F.);
#43660=ORIENTED_EDGE('',*,*,#32991,.T.);
#43661=ORIENTED_EDGE('',*,*,#32992,.T.);
#43662=ORIENTED_EDGE('',*,*,#32987,.F.);
#43663=ORIENTED_EDGE('',*,*,#32993,.F.);
#43664=ORIENTED_EDGE('',*,*,#32994,.T.);
#43665=ORIENTED_EDGE('',*,*,#32995,.T.);
#43666=ORIENTED_EDGE('',*,*,#32991,.F.);
#43667=ORIENTED_EDGE('',*,*,#32996,.F.);
#43668=ORIENTED_EDGE('',*,*,#32989,.T.);
#43669=ORIENTED_EDGE('',*,*,#32997,.T.);
#43670=ORIENTED_EDGE('',*,*,#32994,.F.);
#43671=ORIENTED_EDGE('',*,*,#32997,.F.);
#43672=ORIENTED_EDGE('',*,*,#32988,.F.);
#43673=ORIENTED_EDGE('',*,*,#32992,.F.);
#43674=ORIENTED_EDGE('',*,*,#32995,.F.);
#43675=ORIENTED_EDGE('',*,*,#32998,.F.);
#43676=ORIENTED_EDGE('',*,*,#32999,.T.);
#43677=ORIENTED_EDGE('',*,*,#33000,.T.);
#43678=ORIENTED_EDGE('',*,*,#33001,.F.);
#43679=ORIENTED_EDGE('',*,*,#33002,.F.);
#43680=ORIENTED_EDGE('',*,*,#33003,.T.);
#43681=ORIENTED_EDGE('',*,*,#33004,.T.);
#43682=ORIENTED_EDGE('',*,*,#32999,.F.);
#43683=ORIENTED_EDGE('',*,*,#33005,.F.);
#43684=ORIENTED_EDGE('',*,*,#33006,.T.);
#43685=ORIENTED_EDGE('',*,*,#33007,.T.);
#43686=ORIENTED_EDGE('',*,*,#33003,.F.);
#43687=ORIENTED_EDGE('',*,*,#33008,.F.);
#43688=ORIENTED_EDGE('',*,*,#33001,.T.);
#43689=ORIENTED_EDGE('',*,*,#33009,.T.);
#43690=ORIENTED_EDGE('',*,*,#33006,.F.);
#43691=ORIENTED_EDGE('',*,*,#33009,.F.);
#43692=ORIENTED_EDGE('',*,*,#33000,.F.);
#43693=ORIENTED_EDGE('',*,*,#33004,.F.);
#43694=ORIENTED_EDGE('',*,*,#33007,.F.);
#43695=ORIENTED_EDGE('',*,*,#33010,.F.);
#43696=ORIENTED_EDGE('',*,*,#33011,.T.);
#43697=ORIENTED_EDGE('',*,*,#33012,.T.);
#43698=ORIENTED_EDGE('',*,*,#33013,.F.);
#43699=ORIENTED_EDGE('',*,*,#33014,.F.);
#43700=ORIENTED_EDGE('',*,*,#33015,.T.);
#43701=ORIENTED_EDGE('',*,*,#33016,.T.);
#43702=ORIENTED_EDGE('',*,*,#33011,.F.);
#43703=ORIENTED_EDGE('',*,*,#33017,.F.);
#43704=ORIENTED_EDGE('',*,*,#33018,.T.);
#43705=ORIENTED_EDGE('',*,*,#33019,.T.);
#43706=ORIENTED_EDGE('',*,*,#33015,.F.);
#43707=ORIENTED_EDGE('',*,*,#33020,.F.);
#43708=ORIENTED_EDGE('',*,*,#33013,.T.);
#43709=ORIENTED_EDGE('',*,*,#33021,.T.);
#43710=ORIENTED_EDGE('',*,*,#33018,.F.);
#43711=ORIENTED_EDGE('',*,*,#33021,.F.);
#43712=ORIENTED_EDGE('',*,*,#33012,.F.);
#43713=ORIENTED_EDGE('',*,*,#33016,.F.);
#43714=ORIENTED_EDGE('',*,*,#33019,.F.);
#43715=ORIENTED_EDGE('',*,*,#33022,.F.);
#43716=ORIENTED_EDGE('',*,*,#33023,.T.);
#43717=ORIENTED_EDGE('',*,*,#33024,.T.);
#43718=ORIENTED_EDGE('',*,*,#33025,.F.);
#43719=ORIENTED_EDGE('',*,*,#33026,.F.);
#43720=ORIENTED_EDGE('',*,*,#33027,.T.);
#43721=ORIENTED_EDGE('',*,*,#33028,.T.);
#43722=ORIENTED_EDGE('',*,*,#33023,.F.);
#43723=ORIENTED_EDGE('',*,*,#33029,.F.);
#43724=ORIENTED_EDGE('',*,*,#33030,.T.);
#43725=ORIENTED_EDGE('',*,*,#33031,.T.);
#43726=ORIENTED_EDGE('',*,*,#33027,.F.);
#43727=ORIENTED_EDGE('',*,*,#33032,.F.);
#43728=ORIENTED_EDGE('',*,*,#33025,.T.);
#43729=ORIENTED_EDGE('',*,*,#33033,.T.);
#43730=ORIENTED_EDGE('',*,*,#33030,.F.);
#43731=ORIENTED_EDGE('',*,*,#33033,.F.);
#43732=ORIENTED_EDGE('',*,*,#33024,.F.);
#43733=ORIENTED_EDGE('',*,*,#33028,.F.);
#43734=ORIENTED_EDGE('',*,*,#33031,.F.);
#43735=ORIENTED_EDGE('',*,*,#33034,.F.);
#43736=ORIENTED_EDGE('',*,*,#33035,.T.);
#43737=ORIENTED_EDGE('',*,*,#33036,.T.);
#43738=ORIENTED_EDGE('',*,*,#33037,.F.);
#43739=ORIENTED_EDGE('',*,*,#33038,.F.);
#43740=ORIENTED_EDGE('',*,*,#33039,.T.);
#43741=ORIENTED_EDGE('',*,*,#33040,.T.);
#43742=ORIENTED_EDGE('',*,*,#33035,.F.);
#43743=ORIENTED_EDGE('',*,*,#33041,.F.);
#43744=ORIENTED_EDGE('',*,*,#33042,.T.);
#43745=ORIENTED_EDGE('',*,*,#33043,.T.);
#43746=ORIENTED_EDGE('',*,*,#33039,.F.);
#43747=ORIENTED_EDGE('',*,*,#33044,.F.);
#43748=ORIENTED_EDGE('',*,*,#33037,.T.);
#43749=ORIENTED_EDGE('',*,*,#33045,.T.);
#43750=ORIENTED_EDGE('',*,*,#33042,.F.);
#43751=ORIENTED_EDGE('',*,*,#33045,.F.);
#43752=ORIENTED_EDGE('',*,*,#33036,.F.);
#43753=ORIENTED_EDGE('',*,*,#33040,.F.);
#43754=ORIENTED_EDGE('',*,*,#33043,.F.);
#43755=ORIENTED_EDGE('',*,*,#33046,.F.);
#43756=ORIENTED_EDGE('',*,*,#33047,.T.);
#43757=ORIENTED_EDGE('',*,*,#33048,.T.);
#43758=ORIENTED_EDGE('',*,*,#33049,.F.);
#43759=ORIENTED_EDGE('',*,*,#33050,.F.);
#43760=ORIENTED_EDGE('',*,*,#33051,.T.);
#43761=ORIENTED_EDGE('',*,*,#33052,.T.);
#43762=ORIENTED_EDGE('',*,*,#33047,.F.);
#43763=ORIENTED_EDGE('',*,*,#33053,.F.);
#43764=ORIENTED_EDGE('',*,*,#33054,.T.);
#43765=ORIENTED_EDGE('',*,*,#33055,.T.);
#43766=ORIENTED_EDGE('',*,*,#33051,.F.);
#43767=ORIENTED_EDGE('',*,*,#33056,.F.);
#43768=ORIENTED_EDGE('',*,*,#33049,.T.);
#43769=ORIENTED_EDGE('',*,*,#33057,.T.);
#43770=ORIENTED_EDGE('',*,*,#33054,.F.);
#43771=ORIENTED_EDGE('',*,*,#33057,.F.);
#43772=ORIENTED_EDGE('',*,*,#33048,.F.);
#43773=ORIENTED_EDGE('',*,*,#33052,.F.);
#43774=ORIENTED_EDGE('',*,*,#33055,.F.);
#43775=ORIENTED_EDGE('',*,*,#33058,.F.);
#43776=ORIENTED_EDGE('',*,*,#33059,.T.);
#43777=ORIENTED_EDGE('',*,*,#33060,.T.);
#43778=ORIENTED_EDGE('',*,*,#33061,.F.);
#43779=ORIENTED_EDGE('',*,*,#33062,.F.);
#43780=ORIENTED_EDGE('',*,*,#33063,.T.);
#43781=ORIENTED_EDGE('',*,*,#33064,.T.);
#43782=ORIENTED_EDGE('',*,*,#33059,.F.);
#43783=ORIENTED_EDGE('',*,*,#33065,.F.);
#43784=ORIENTED_EDGE('',*,*,#33066,.T.);
#43785=ORIENTED_EDGE('',*,*,#33067,.T.);
#43786=ORIENTED_EDGE('',*,*,#33063,.F.);
#43787=ORIENTED_EDGE('',*,*,#33068,.F.);
#43788=ORIENTED_EDGE('',*,*,#33061,.T.);
#43789=ORIENTED_EDGE('',*,*,#33069,.T.);
#43790=ORIENTED_EDGE('',*,*,#33066,.F.);
#43791=ORIENTED_EDGE('',*,*,#33069,.F.);
#43792=ORIENTED_EDGE('',*,*,#33060,.F.);
#43793=ORIENTED_EDGE('',*,*,#33064,.F.);
#43794=ORIENTED_EDGE('',*,*,#33067,.F.);
#43795=ORIENTED_EDGE('',*,*,#33070,.F.);
#43796=ORIENTED_EDGE('',*,*,#33071,.T.);
#43797=ORIENTED_EDGE('',*,*,#33072,.T.);
#43798=ORIENTED_EDGE('',*,*,#33073,.F.);
#43799=ORIENTED_EDGE('',*,*,#33074,.F.);
#43800=ORIENTED_EDGE('',*,*,#33075,.T.);
#43801=ORIENTED_EDGE('',*,*,#33076,.T.);
#43802=ORIENTED_EDGE('',*,*,#33071,.F.);
#43803=ORIENTED_EDGE('',*,*,#33077,.F.);
#43804=ORIENTED_EDGE('',*,*,#33078,.T.);
#43805=ORIENTED_EDGE('',*,*,#33079,.T.);
#43806=ORIENTED_EDGE('',*,*,#33075,.F.);
#43807=ORIENTED_EDGE('',*,*,#33080,.F.);
#43808=ORIENTED_EDGE('',*,*,#33073,.T.);
#43809=ORIENTED_EDGE('',*,*,#33081,.T.);
#43810=ORIENTED_EDGE('',*,*,#33078,.F.);
#43811=ORIENTED_EDGE('',*,*,#33081,.F.);
#43812=ORIENTED_EDGE('',*,*,#33072,.F.);
#43813=ORIENTED_EDGE('',*,*,#33076,.F.);
#43814=ORIENTED_EDGE('',*,*,#33079,.F.);
#43815=ORIENTED_EDGE('',*,*,#33082,.F.);
#43816=ORIENTED_EDGE('',*,*,#33083,.T.);
#43817=ORIENTED_EDGE('',*,*,#33084,.T.);
#43818=ORIENTED_EDGE('',*,*,#33085,.F.);
#43819=ORIENTED_EDGE('',*,*,#33086,.F.);
#43820=ORIENTED_EDGE('',*,*,#33087,.T.);
#43821=ORIENTED_EDGE('',*,*,#33088,.T.);
#43822=ORIENTED_EDGE('',*,*,#33083,.F.);
#43823=ORIENTED_EDGE('',*,*,#33089,.F.);
#43824=ORIENTED_EDGE('',*,*,#33090,.T.);
#43825=ORIENTED_EDGE('',*,*,#33091,.T.);
#43826=ORIENTED_EDGE('',*,*,#33087,.F.);
#43827=ORIENTED_EDGE('',*,*,#33092,.F.);
#43828=ORIENTED_EDGE('',*,*,#33085,.T.);
#43829=ORIENTED_EDGE('',*,*,#33093,.T.);
#43830=ORIENTED_EDGE('',*,*,#33090,.F.);
#43831=ORIENTED_EDGE('',*,*,#33093,.F.);
#43832=ORIENTED_EDGE('',*,*,#33084,.F.);
#43833=ORIENTED_EDGE('',*,*,#33088,.F.);
#43834=ORIENTED_EDGE('',*,*,#33091,.F.);
#43835=ORIENTED_EDGE('',*,*,#33094,.F.);
#43836=ORIENTED_EDGE('',*,*,#33095,.T.);
#43837=ORIENTED_EDGE('',*,*,#33096,.T.);
#43838=ORIENTED_EDGE('',*,*,#33097,.F.);
#43839=ORIENTED_EDGE('',*,*,#33098,.F.);
#43840=ORIENTED_EDGE('',*,*,#33099,.T.);
#43841=ORIENTED_EDGE('',*,*,#33100,.T.);
#43842=ORIENTED_EDGE('',*,*,#33095,.F.);
#43843=ORIENTED_EDGE('',*,*,#33101,.F.);
#43844=ORIENTED_EDGE('',*,*,#33102,.T.);
#43845=ORIENTED_EDGE('',*,*,#33103,.T.);
#43846=ORIENTED_EDGE('',*,*,#33099,.F.);
#43847=ORIENTED_EDGE('',*,*,#33104,.F.);
#43848=ORIENTED_EDGE('',*,*,#33097,.T.);
#43849=ORIENTED_EDGE('',*,*,#33105,.T.);
#43850=ORIENTED_EDGE('',*,*,#33102,.F.);
#43851=ORIENTED_EDGE('',*,*,#33105,.F.);
#43852=ORIENTED_EDGE('',*,*,#33096,.F.);
#43853=ORIENTED_EDGE('',*,*,#33100,.F.);
#43854=ORIENTED_EDGE('',*,*,#33103,.F.);
#43855=ORIENTED_EDGE('',*,*,#33106,.F.);
#43856=ORIENTED_EDGE('',*,*,#33107,.T.);
#43857=ORIENTED_EDGE('',*,*,#33108,.T.);
#43858=ORIENTED_EDGE('',*,*,#33109,.F.);
#43859=ORIENTED_EDGE('',*,*,#33110,.F.);
#43860=ORIENTED_EDGE('',*,*,#33111,.T.);
#43861=ORIENTED_EDGE('',*,*,#33112,.T.);
#43862=ORIENTED_EDGE('',*,*,#33107,.F.);
#43863=ORIENTED_EDGE('',*,*,#33113,.F.);
#43864=ORIENTED_EDGE('',*,*,#33114,.T.);
#43865=ORIENTED_EDGE('',*,*,#33115,.T.);
#43866=ORIENTED_EDGE('',*,*,#33111,.F.);
#43867=ORIENTED_EDGE('',*,*,#33116,.F.);
#43868=ORIENTED_EDGE('',*,*,#33109,.T.);
#43869=ORIENTED_EDGE('',*,*,#33117,.T.);
#43870=ORIENTED_EDGE('',*,*,#33114,.F.);
#43871=ORIENTED_EDGE('',*,*,#33117,.F.);
#43872=ORIENTED_EDGE('',*,*,#33108,.F.);
#43873=ORIENTED_EDGE('',*,*,#33112,.F.);
#43874=ORIENTED_EDGE('',*,*,#33115,.F.);
#43875=ORIENTED_EDGE('',*,*,#33118,.F.);
#43876=ORIENTED_EDGE('',*,*,#33119,.T.);
#43877=ORIENTED_EDGE('',*,*,#33120,.T.);
#43878=ORIENTED_EDGE('',*,*,#33121,.F.);
#43879=ORIENTED_EDGE('',*,*,#33122,.F.);
#43880=ORIENTED_EDGE('',*,*,#33123,.T.);
#43881=ORIENTED_EDGE('',*,*,#33124,.T.);
#43882=ORIENTED_EDGE('',*,*,#33119,.F.);
#43883=ORIENTED_EDGE('',*,*,#33125,.F.);
#43884=ORIENTED_EDGE('',*,*,#33126,.T.);
#43885=ORIENTED_EDGE('',*,*,#33127,.T.);
#43886=ORIENTED_EDGE('',*,*,#33123,.F.);
#43887=ORIENTED_EDGE('',*,*,#33128,.F.);
#43888=ORIENTED_EDGE('',*,*,#33121,.T.);
#43889=ORIENTED_EDGE('',*,*,#33129,.T.);
#43890=ORIENTED_EDGE('',*,*,#33126,.F.);
#43891=ORIENTED_EDGE('',*,*,#33129,.F.);
#43892=ORIENTED_EDGE('',*,*,#33120,.F.);
#43893=ORIENTED_EDGE('',*,*,#33124,.F.);
#43894=ORIENTED_EDGE('',*,*,#33127,.F.);
#43895=ORIENTED_EDGE('',*,*,#33130,.F.);
#43896=ORIENTED_EDGE('',*,*,#33131,.T.);
#43897=ORIENTED_EDGE('',*,*,#33132,.T.);
#43898=ORIENTED_EDGE('',*,*,#33133,.F.);
#43899=ORIENTED_EDGE('',*,*,#33134,.F.);
#43900=ORIENTED_EDGE('',*,*,#33135,.T.);
#43901=ORIENTED_EDGE('',*,*,#33136,.T.);
#43902=ORIENTED_EDGE('',*,*,#33131,.F.);
#43903=ORIENTED_EDGE('',*,*,#33137,.F.);
#43904=ORIENTED_EDGE('',*,*,#33138,.T.);
#43905=ORIENTED_EDGE('',*,*,#33139,.T.);
#43906=ORIENTED_EDGE('',*,*,#33135,.F.);
#43907=ORIENTED_EDGE('',*,*,#33140,.F.);
#43908=ORIENTED_EDGE('',*,*,#33133,.T.);
#43909=ORIENTED_EDGE('',*,*,#33141,.T.);
#43910=ORIENTED_EDGE('',*,*,#33138,.F.);
#43911=ORIENTED_EDGE('',*,*,#33141,.F.);
#43912=ORIENTED_EDGE('',*,*,#33132,.F.);
#43913=ORIENTED_EDGE('',*,*,#33136,.F.);
#43914=ORIENTED_EDGE('',*,*,#33139,.F.);
#43915=ORIENTED_EDGE('',*,*,#33142,.F.);
#43916=ORIENTED_EDGE('',*,*,#33143,.T.);
#43917=ORIENTED_EDGE('',*,*,#33144,.T.);
#43918=ORIENTED_EDGE('',*,*,#33145,.F.);
#43919=ORIENTED_EDGE('',*,*,#33146,.F.);
#43920=ORIENTED_EDGE('',*,*,#33147,.T.);
#43921=ORIENTED_EDGE('',*,*,#33148,.T.);
#43922=ORIENTED_EDGE('',*,*,#33143,.F.);
#43923=ORIENTED_EDGE('',*,*,#33149,.F.);
#43924=ORIENTED_EDGE('',*,*,#33150,.T.);
#43925=ORIENTED_EDGE('',*,*,#33151,.T.);
#43926=ORIENTED_EDGE('',*,*,#33147,.F.);
#43927=ORIENTED_EDGE('',*,*,#33152,.F.);
#43928=ORIENTED_EDGE('',*,*,#33145,.T.);
#43929=ORIENTED_EDGE('',*,*,#33153,.T.);
#43930=ORIENTED_EDGE('',*,*,#33150,.F.);
#43931=ORIENTED_EDGE('',*,*,#33153,.F.);
#43932=ORIENTED_EDGE('',*,*,#33144,.F.);
#43933=ORIENTED_EDGE('',*,*,#33148,.F.);
#43934=ORIENTED_EDGE('',*,*,#33151,.F.);
#43935=ORIENTED_EDGE('',*,*,#33154,.F.);
#43936=ORIENTED_EDGE('',*,*,#33155,.T.);
#43937=ORIENTED_EDGE('',*,*,#33156,.T.);
#43938=ORIENTED_EDGE('',*,*,#33157,.F.);
#43939=ORIENTED_EDGE('',*,*,#33158,.F.);
#43940=ORIENTED_EDGE('',*,*,#33159,.T.);
#43941=ORIENTED_EDGE('',*,*,#33160,.T.);
#43942=ORIENTED_EDGE('',*,*,#33155,.F.);
#43943=ORIENTED_EDGE('',*,*,#33161,.F.);
#43944=ORIENTED_EDGE('',*,*,#33162,.T.);
#43945=ORIENTED_EDGE('',*,*,#33163,.T.);
#43946=ORIENTED_EDGE('',*,*,#33159,.F.);
#43947=ORIENTED_EDGE('',*,*,#33164,.F.);
#43948=ORIENTED_EDGE('',*,*,#33157,.T.);
#43949=ORIENTED_EDGE('',*,*,#33165,.T.);
#43950=ORIENTED_EDGE('',*,*,#33162,.F.);
#43951=ORIENTED_EDGE('',*,*,#33165,.F.);
#43952=ORIENTED_EDGE('',*,*,#33156,.F.);
#43953=ORIENTED_EDGE('',*,*,#33160,.F.);
#43954=ORIENTED_EDGE('',*,*,#33163,.F.);
#43955=ORIENTED_EDGE('',*,*,#33166,.F.);
#43956=ORIENTED_EDGE('',*,*,#33167,.T.);
#43957=ORIENTED_EDGE('',*,*,#33168,.T.);
#43958=ORIENTED_EDGE('',*,*,#33169,.F.);
#43959=ORIENTED_EDGE('',*,*,#33170,.F.);
#43960=ORIENTED_EDGE('',*,*,#33171,.T.);
#43961=ORIENTED_EDGE('',*,*,#33172,.T.);
#43962=ORIENTED_EDGE('',*,*,#33167,.F.);
#43963=ORIENTED_EDGE('',*,*,#33173,.F.);
#43964=ORIENTED_EDGE('',*,*,#33174,.T.);
#43965=ORIENTED_EDGE('',*,*,#33175,.T.);
#43966=ORIENTED_EDGE('',*,*,#33171,.F.);
#43967=ORIENTED_EDGE('',*,*,#33176,.F.);
#43968=ORIENTED_EDGE('',*,*,#33169,.T.);
#43969=ORIENTED_EDGE('',*,*,#33177,.T.);
#43970=ORIENTED_EDGE('',*,*,#33174,.F.);
#43971=ORIENTED_EDGE('',*,*,#33177,.F.);
#43972=ORIENTED_EDGE('',*,*,#33168,.F.);
#43973=ORIENTED_EDGE('',*,*,#33172,.F.);
#43974=ORIENTED_EDGE('',*,*,#33175,.F.);
#43975=ORIENTED_EDGE('',*,*,#33178,.F.);
#43976=ORIENTED_EDGE('',*,*,#33179,.T.);
#43977=ORIENTED_EDGE('',*,*,#33180,.T.);
#43978=ORIENTED_EDGE('',*,*,#33181,.F.);
#43979=ORIENTED_EDGE('',*,*,#33182,.F.);
#43980=ORIENTED_EDGE('',*,*,#33183,.T.);
#43981=ORIENTED_EDGE('',*,*,#33184,.T.);
#43982=ORIENTED_EDGE('',*,*,#33179,.F.);
#43983=ORIENTED_EDGE('',*,*,#33185,.F.);
#43984=ORIENTED_EDGE('',*,*,#33186,.T.);
#43985=ORIENTED_EDGE('',*,*,#33187,.T.);
#43986=ORIENTED_EDGE('',*,*,#33183,.F.);
#43987=ORIENTED_EDGE('',*,*,#33188,.F.);
#43988=ORIENTED_EDGE('',*,*,#33181,.T.);
#43989=ORIENTED_EDGE('',*,*,#33189,.T.);
#43990=ORIENTED_EDGE('',*,*,#33186,.F.);
#43991=ORIENTED_EDGE('',*,*,#33189,.F.);
#43992=ORIENTED_EDGE('',*,*,#33180,.F.);
#43993=ORIENTED_EDGE('',*,*,#33184,.F.);
#43994=ORIENTED_EDGE('',*,*,#33187,.F.);
#43995=ORIENTED_EDGE('',*,*,#33190,.F.);
#43996=ORIENTED_EDGE('',*,*,#33191,.T.);
#43997=ORIENTED_EDGE('',*,*,#33192,.T.);
#43998=ORIENTED_EDGE('',*,*,#33193,.F.);
#43999=ORIENTED_EDGE('',*,*,#33194,.F.);
#44000=ORIENTED_EDGE('',*,*,#33195,.T.);
#44001=ORIENTED_EDGE('',*,*,#33196,.T.);
#44002=ORIENTED_EDGE('',*,*,#33191,.F.);
#44003=ORIENTED_EDGE('',*,*,#33197,.F.);
#44004=ORIENTED_EDGE('',*,*,#33198,.T.);
#44005=ORIENTED_EDGE('',*,*,#33199,.T.);
#44006=ORIENTED_EDGE('',*,*,#33195,.F.);
#44007=ORIENTED_EDGE('',*,*,#33200,.F.);
#44008=ORIENTED_EDGE('',*,*,#33193,.T.);
#44009=ORIENTED_EDGE('',*,*,#33201,.T.);
#44010=ORIENTED_EDGE('',*,*,#33198,.F.);
#44011=ORIENTED_EDGE('',*,*,#33201,.F.);
#44012=ORIENTED_EDGE('',*,*,#33192,.F.);
#44013=ORIENTED_EDGE('',*,*,#33196,.F.);
#44014=ORIENTED_EDGE('',*,*,#33199,.F.);
#44015=ORIENTED_EDGE('',*,*,#33202,.F.);
#44016=ORIENTED_EDGE('',*,*,#33203,.T.);
#44017=ORIENTED_EDGE('',*,*,#33204,.T.);
#44018=ORIENTED_EDGE('',*,*,#33205,.F.);
#44019=ORIENTED_EDGE('',*,*,#33206,.F.);
#44020=ORIENTED_EDGE('',*,*,#33207,.T.);
#44021=ORIENTED_EDGE('',*,*,#33208,.T.);
#44022=ORIENTED_EDGE('',*,*,#33203,.F.);
#44023=ORIENTED_EDGE('',*,*,#33209,.F.);
#44024=ORIENTED_EDGE('',*,*,#33210,.T.);
#44025=ORIENTED_EDGE('',*,*,#33211,.T.);
#44026=ORIENTED_EDGE('',*,*,#33207,.F.);
#44027=ORIENTED_EDGE('',*,*,#33212,.F.);
#44028=ORIENTED_EDGE('',*,*,#33205,.T.);
#44029=ORIENTED_EDGE('',*,*,#33213,.T.);
#44030=ORIENTED_EDGE('',*,*,#33210,.F.);
#44031=ORIENTED_EDGE('',*,*,#33213,.F.);
#44032=ORIENTED_EDGE('',*,*,#33204,.F.);
#44033=ORIENTED_EDGE('',*,*,#33208,.F.);
#44034=ORIENTED_EDGE('',*,*,#33211,.F.);
#44035=ORIENTED_EDGE('',*,*,#33214,.F.);
#44036=ORIENTED_EDGE('',*,*,#33215,.T.);
#44037=ORIENTED_EDGE('',*,*,#33216,.T.);
#44038=ORIENTED_EDGE('',*,*,#33217,.F.);
#44039=ORIENTED_EDGE('',*,*,#33218,.F.);
#44040=ORIENTED_EDGE('',*,*,#33219,.T.);
#44041=ORIENTED_EDGE('',*,*,#33220,.T.);
#44042=ORIENTED_EDGE('',*,*,#33215,.F.);
#44043=ORIENTED_EDGE('',*,*,#33221,.F.);
#44044=ORIENTED_EDGE('',*,*,#33222,.T.);
#44045=ORIENTED_EDGE('',*,*,#33223,.T.);
#44046=ORIENTED_EDGE('',*,*,#33219,.F.);
#44047=ORIENTED_EDGE('',*,*,#33224,.F.);
#44048=ORIENTED_EDGE('',*,*,#33217,.T.);
#44049=ORIENTED_EDGE('',*,*,#33225,.T.);
#44050=ORIENTED_EDGE('',*,*,#33222,.F.);
#44051=ORIENTED_EDGE('',*,*,#33225,.F.);
#44052=ORIENTED_EDGE('',*,*,#33216,.F.);
#44053=ORIENTED_EDGE('',*,*,#33220,.F.);
#44054=ORIENTED_EDGE('',*,*,#33223,.F.);
#44055=ORIENTED_EDGE('',*,*,#33226,.F.);
#44056=ORIENTED_EDGE('',*,*,#33227,.T.);
#44057=ORIENTED_EDGE('',*,*,#33228,.T.);
#44058=ORIENTED_EDGE('',*,*,#33229,.F.);
#44059=ORIENTED_EDGE('',*,*,#33230,.F.);
#44060=ORIENTED_EDGE('',*,*,#33231,.T.);
#44061=ORIENTED_EDGE('',*,*,#33232,.T.);
#44062=ORIENTED_EDGE('',*,*,#33227,.F.);
#44063=ORIENTED_EDGE('',*,*,#33233,.F.);
#44064=ORIENTED_EDGE('',*,*,#33234,.T.);
#44065=ORIENTED_EDGE('',*,*,#33235,.T.);
#44066=ORIENTED_EDGE('',*,*,#33231,.F.);
#44067=ORIENTED_EDGE('',*,*,#33236,.F.);
#44068=ORIENTED_EDGE('',*,*,#33229,.T.);
#44069=ORIENTED_EDGE('',*,*,#33237,.T.);
#44070=ORIENTED_EDGE('',*,*,#33234,.F.);
#44071=ORIENTED_EDGE('',*,*,#33237,.F.);
#44072=ORIENTED_EDGE('',*,*,#33228,.F.);
#44073=ORIENTED_EDGE('',*,*,#33232,.F.);
#44074=ORIENTED_EDGE('',*,*,#33235,.F.);
#44075=ORIENTED_EDGE('',*,*,#33238,.F.);
#44076=ORIENTED_EDGE('',*,*,#33239,.T.);
#44077=ORIENTED_EDGE('',*,*,#33240,.T.);
#44078=ORIENTED_EDGE('',*,*,#33241,.F.);
#44079=ORIENTED_EDGE('',*,*,#33242,.F.);
#44080=ORIENTED_EDGE('',*,*,#33243,.T.);
#44081=ORIENTED_EDGE('',*,*,#33244,.T.);
#44082=ORIENTED_EDGE('',*,*,#33239,.F.);
#44083=ORIENTED_EDGE('',*,*,#33245,.F.);
#44084=ORIENTED_EDGE('',*,*,#33246,.T.);
#44085=ORIENTED_EDGE('',*,*,#33247,.T.);
#44086=ORIENTED_EDGE('',*,*,#33243,.F.);
#44087=ORIENTED_EDGE('',*,*,#33248,.F.);
#44088=ORIENTED_EDGE('',*,*,#33241,.T.);
#44089=ORIENTED_EDGE('',*,*,#33249,.T.);
#44090=ORIENTED_EDGE('',*,*,#33246,.F.);
#44091=ORIENTED_EDGE('',*,*,#33249,.F.);
#44092=ORIENTED_EDGE('',*,*,#33240,.F.);
#44093=ORIENTED_EDGE('',*,*,#33244,.F.);
#44094=ORIENTED_EDGE('',*,*,#33247,.F.);
#44095=ORIENTED_EDGE('',*,*,#33250,.F.);
#44096=ORIENTED_EDGE('',*,*,#33251,.T.);
#44097=ORIENTED_EDGE('',*,*,#33252,.T.);
#44098=ORIENTED_EDGE('',*,*,#33253,.F.);
#44099=ORIENTED_EDGE('',*,*,#33254,.F.);
#44100=ORIENTED_EDGE('',*,*,#33255,.T.);
#44101=ORIENTED_EDGE('',*,*,#33256,.T.);
#44102=ORIENTED_EDGE('',*,*,#33251,.F.);
#44103=ORIENTED_EDGE('',*,*,#33257,.F.);
#44104=ORIENTED_EDGE('',*,*,#33258,.T.);
#44105=ORIENTED_EDGE('',*,*,#33259,.T.);
#44106=ORIENTED_EDGE('',*,*,#33255,.F.);
#44107=ORIENTED_EDGE('',*,*,#33260,.F.);
#44108=ORIENTED_EDGE('',*,*,#33253,.T.);
#44109=ORIENTED_EDGE('',*,*,#33261,.T.);
#44110=ORIENTED_EDGE('',*,*,#33258,.F.);
#44111=ORIENTED_EDGE('',*,*,#33261,.F.);
#44112=ORIENTED_EDGE('',*,*,#33252,.F.);
#44113=ORIENTED_EDGE('',*,*,#33256,.F.);
#44114=ORIENTED_EDGE('',*,*,#33259,.F.);
#44115=ORIENTED_EDGE('',*,*,#33262,.F.);
#44116=ORIENTED_EDGE('',*,*,#33263,.T.);
#44117=ORIENTED_EDGE('',*,*,#33264,.T.);
#44118=ORIENTED_EDGE('',*,*,#33265,.F.);
#44119=ORIENTED_EDGE('',*,*,#33266,.F.);
#44120=ORIENTED_EDGE('',*,*,#33267,.T.);
#44121=ORIENTED_EDGE('',*,*,#33268,.T.);
#44122=ORIENTED_EDGE('',*,*,#33263,.F.);
#44123=ORIENTED_EDGE('',*,*,#33269,.F.);
#44124=ORIENTED_EDGE('',*,*,#33270,.T.);
#44125=ORIENTED_EDGE('',*,*,#33271,.T.);
#44126=ORIENTED_EDGE('',*,*,#33267,.F.);
#44127=ORIENTED_EDGE('',*,*,#33272,.F.);
#44128=ORIENTED_EDGE('',*,*,#33265,.T.);
#44129=ORIENTED_EDGE('',*,*,#33273,.T.);
#44130=ORIENTED_EDGE('',*,*,#33270,.F.);
#44131=ORIENTED_EDGE('',*,*,#33273,.F.);
#44132=ORIENTED_EDGE('',*,*,#33264,.F.);
#44133=ORIENTED_EDGE('',*,*,#33268,.F.);
#44134=ORIENTED_EDGE('',*,*,#33271,.F.);
#44135=ORIENTED_EDGE('',*,*,#33274,.F.);
#44136=ORIENTED_EDGE('',*,*,#33275,.T.);
#44137=ORIENTED_EDGE('',*,*,#33276,.T.);
#44138=ORIENTED_EDGE('',*,*,#33277,.F.);
#44139=ORIENTED_EDGE('',*,*,#33278,.F.);
#44140=ORIENTED_EDGE('',*,*,#33279,.T.);
#44141=ORIENTED_EDGE('',*,*,#33280,.T.);
#44142=ORIENTED_EDGE('',*,*,#33275,.F.);
#44143=ORIENTED_EDGE('',*,*,#33281,.F.);
#44144=ORIENTED_EDGE('',*,*,#33282,.T.);
#44145=ORIENTED_EDGE('',*,*,#33283,.T.);
#44146=ORIENTED_EDGE('',*,*,#33279,.F.);
#44147=ORIENTED_EDGE('',*,*,#33284,.F.);
#44148=ORIENTED_EDGE('',*,*,#33277,.T.);
#44149=ORIENTED_EDGE('',*,*,#33285,.T.);
#44150=ORIENTED_EDGE('',*,*,#33282,.F.);
#44151=ORIENTED_EDGE('',*,*,#33285,.F.);
#44152=ORIENTED_EDGE('',*,*,#33276,.F.);
#44153=ORIENTED_EDGE('',*,*,#33280,.F.);
#44154=ORIENTED_EDGE('',*,*,#33283,.F.);
#44155=ORIENTED_EDGE('',*,*,#33286,.F.);
#44156=ORIENTED_EDGE('',*,*,#33287,.T.);
#44157=ORIENTED_EDGE('',*,*,#33288,.T.);
#44158=ORIENTED_EDGE('',*,*,#33289,.F.);
#44159=ORIENTED_EDGE('',*,*,#33290,.F.);
#44160=ORIENTED_EDGE('',*,*,#33291,.T.);
#44161=ORIENTED_EDGE('',*,*,#33292,.T.);
#44162=ORIENTED_EDGE('',*,*,#33287,.F.);
#44163=ORIENTED_EDGE('',*,*,#33293,.F.);
#44164=ORIENTED_EDGE('',*,*,#33294,.T.);
#44165=ORIENTED_EDGE('',*,*,#33295,.T.);
#44166=ORIENTED_EDGE('',*,*,#33291,.F.);
#44167=ORIENTED_EDGE('',*,*,#33296,.F.);
#44168=ORIENTED_EDGE('',*,*,#33289,.T.);
#44169=ORIENTED_EDGE('',*,*,#33297,.T.);
#44170=ORIENTED_EDGE('',*,*,#33294,.F.);
#44171=ORIENTED_EDGE('',*,*,#33297,.F.);
#44172=ORIENTED_EDGE('',*,*,#33288,.F.);
#44173=ORIENTED_EDGE('',*,*,#33292,.F.);
#44174=ORIENTED_EDGE('',*,*,#33295,.F.);
#44175=ORIENTED_EDGE('',*,*,#33298,.F.);
#44176=ORIENTED_EDGE('',*,*,#33299,.T.);
#44177=ORIENTED_EDGE('',*,*,#33300,.T.);
#44178=ORIENTED_EDGE('',*,*,#33301,.F.);
#44179=ORIENTED_EDGE('',*,*,#33302,.F.);
#44180=ORIENTED_EDGE('',*,*,#33303,.T.);
#44181=ORIENTED_EDGE('',*,*,#33304,.T.);
#44182=ORIENTED_EDGE('',*,*,#33299,.F.);
#44183=ORIENTED_EDGE('',*,*,#33305,.F.);
#44184=ORIENTED_EDGE('',*,*,#33306,.T.);
#44185=ORIENTED_EDGE('',*,*,#33307,.T.);
#44186=ORIENTED_EDGE('',*,*,#33303,.F.);
#44187=ORIENTED_EDGE('',*,*,#33308,.F.);
#44188=ORIENTED_EDGE('',*,*,#33301,.T.);
#44189=ORIENTED_EDGE('',*,*,#33309,.T.);
#44190=ORIENTED_EDGE('',*,*,#33306,.F.);
#44191=ORIENTED_EDGE('',*,*,#33309,.F.);
#44192=ORIENTED_EDGE('',*,*,#33300,.F.);
#44193=ORIENTED_EDGE('',*,*,#33304,.F.);
#44194=ORIENTED_EDGE('',*,*,#33307,.F.);
#44195=ORIENTED_EDGE('',*,*,#33310,.F.);
#44196=ORIENTED_EDGE('',*,*,#33311,.T.);
#44197=ORIENTED_EDGE('',*,*,#33312,.T.);
#44198=ORIENTED_EDGE('',*,*,#33313,.F.);
#44199=ORIENTED_EDGE('',*,*,#33314,.F.);
#44200=ORIENTED_EDGE('',*,*,#33315,.T.);
#44201=ORIENTED_EDGE('',*,*,#33316,.T.);
#44202=ORIENTED_EDGE('',*,*,#33311,.F.);
#44203=ORIENTED_EDGE('',*,*,#33317,.F.);
#44204=ORIENTED_EDGE('',*,*,#33318,.T.);
#44205=ORIENTED_EDGE('',*,*,#33319,.T.);
#44206=ORIENTED_EDGE('',*,*,#33315,.F.);
#44207=ORIENTED_EDGE('',*,*,#33320,.F.);
#44208=ORIENTED_EDGE('',*,*,#33313,.T.);
#44209=ORIENTED_EDGE('',*,*,#33321,.T.);
#44210=ORIENTED_EDGE('',*,*,#33318,.F.);
#44211=ORIENTED_EDGE('',*,*,#33321,.F.);
#44212=ORIENTED_EDGE('',*,*,#33312,.F.);
#44213=ORIENTED_EDGE('',*,*,#33316,.F.);
#44214=ORIENTED_EDGE('',*,*,#33319,.F.);
#44215=ORIENTED_EDGE('',*,*,#33322,.F.);
#44216=ORIENTED_EDGE('',*,*,#33323,.T.);
#44217=ORIENTED_EDGE('',*,*,#33324,.T.);
#44218=ORIENTED_EDGE('',*,*,#33325,.F.);
#44219=ORIENTED_EDGE('',*,*,#33326,.F.);
#44220=ORIENTED_EDGE('',*,*,#33327,.T.);
#44221=ORIENTED_EDGE('',*,*,#33328,.T.);
#44222=ORIENTED_EDGE('',*,*,#33323,.F.);
#44223=ORIENTED_EDGE('',*,*,#33329,.F.);
#44224=ORIENTED_EDGE('',*,*,#33330,.T.);
#44225=ORIENTED_EDGE('',*,*,#33331,.T.);
#44226=ORIENTED_EDGE('',*,*,#33327,.F.);
#44227=ORIENTED_EDGE('',*,*,#33332,.F.);
#44228=ORIENTED_EDGE('',*,*,#33325,.T.);
#44229=ORIENTED_EDGE('',*,*,#33333,.T.);
#44230=ORIENTED_EDGE('',*,*,#33330,.F.);
#44231=ORIENTED_EDGE('',*,*,#33333,.F.);
#44232=ORIENTED_EDGE('',*,*,#33324,.F.);
#44233=ORIENTED_EDGE('',*,*,#33328,.F.);
#44234=ORIENTED_EDGE('',*,*,#33331,.F.);
#44235=ORIENTED_EDGE('',*,*,#33334,.F.);
#44236=ORIENTED_EDGE('',*,*,#33335,.T.);
#44237=ORIENTED_EDGE('',*,*,#33336,.T.);
#44238=ORIENTED_EDGE('',*,*,#33337,.F.);
#44239=ORIENTED_EDGE('',*,*,#33338,.F.);
#44240=ORIENTED_EDGE('',*,*,#33339,.T.);
#44241=ORIENTED_EDGE('',*,*,#33340,.T.);
#44242=ORIENTED_EDGE('',*,*,#33335,.F.);
#44243=ORIENTED_EDGE('',*,*,#33341,.F.);
#44244=ORIENTED_EDGE('',*,*,#33342,.T.);
#44245=ORIENTED_EDGE('',*,*,#33343,.T.);
#44246=ORIENTED_EDGE('',*,*,#33339,.F.);
#44247=ORIENTED_EDGE('',*,*,#33344,.F.);
#44248=ORIENTED_EDGE('',*,*,#33337,.T.);
#44249=ORIENTED_EDGE('',*,*,#33345,.T.);
#44250=ORIENTED_EDGE('',*,*,#33342,.F.);
#44251=ORIENTED_EDGE('',*,*,#33345,.F.);
#44252=ORIENTED_EDGE('',*,*,#33336,.F.);
#44253=ORIENTED_EDGE('',*,*,#33340,.F.);
#44254=ORIENTED_EDGE('',*,*,#33343,.F.);
#44255=ORIENTED_EDGE('',*,*,#33346,.F.);
#44256=ORIENTED_EDGE('',*,*,#33347,.T.);
#44257=ORIENTED_EDGE('',*,*,#33348,.T.);
#44258=ORIENTED_EDGE('',*,*,#33349,.F.);
#44259=ORIENTED_EDGE('',*,*,#33350,.F.);
#44260=ORIENTED_EDGE('',*,*,#33351,.T.);
#44261=ORIENTED_EDGE('',*,*,#33352,.T.);
#44262=ORIENTED_EDGE('',*,*,#33347,.F.);
#44263=ORIENTED_EDGE('',*,*,#33353,.F.);
#44264=ORIENTED_EDGE('',*,*,#33354,.T.);
#44265=ORIENTED_EDGE('',*,*,#33355,.T.);
#44266=ORIENTED_EDGE('',*,*,#33351,.F.);
#44267=ORIENTED_EDGE('',*,*,#33356,.F.);
#44268=ORIENTED_EDGE('',*,*,#33349,.T.);
#44269=ORIENTED_EDGE('',*,*,#33357,.T.);
#44270=ORIENTED_EDGE('',*,*,#33354,.F.);
#44271=ORIENTED_EDGE('',*,*,#33357,.F.);
#44272=ORIENTED_EDGE('',*,*,#33348,.F.);
#44273=ORIENTED_EDGE('',*,*,#33352,.F.);
#44274=ORIENTED_EDGE('',*,*,#33355,.F.);
#44275=ORIENTED_EDGE('',*,*,#33358,.F.);
#44276=ORIENTED_EDGE('',*,*,#33359,.T.);
#44277=ORIENTED_EDGE('',*,*,#33360,.T.);
#44278=ORIENTED_EDGE('',*,*,#33361,.F.);
#44279=ORIENTED_EDGE('',*,*,#33362,.F.);
#44280=ORIENTED_EDGE('',*,*,#33363,.T.);
#44281=ORIENTED_EDGE('',*,*,#33364,.T.);
#44282=ORIENTED_EDGE('',*,*,#33359,.F.);
#44283=ORIENTED_EDGE('',*,*,#33365,.F.);
#44284=ORIENTED_EDGE('',*,*,#33366,.T.);
#44285=ORIENTED_EDGE('',*,*,#33367,.T.);
#44286=ORIENTED_EDGE('',*,*,#33363,.F.);
#44287=ORIENTED_EDGE('',*,*,#33368,.F.);
#44288=ORIENTED_EDGE('',*,*,#33361,.T.);
#44289=ORIENTED_EDGE('',*,*,#33369,.T.);
#44290=ORIENTED_EDGE('',*,*,#33366,.F.);
#44291=ORIENTED_EDGE('',*,*,#33369,.F.);
#44292=ORIENTED_EDGE('',*,*,#33360,.F.);
#44293=ORIENTED_EDGE('',*,*,#33364,.F.);
#44294=ORIENTED_EDGE('',*,*,#33367,.F.);
#44295=ORIENTED_EDGE('',*,*,#33370,.F.);
#44296=ORIENTED_EDGE('',*,*,#33371,.T.);
#44297=ORIENTED_EDGE('',*,*,#33372,.T.);
#44298=ORIENTED_EDGE('',*,*,#33373,.F.);
#44299=ORIENTED_EDGE('',*,*,#33374,.F.);
#44300=ORIENTED_EDGE('',*,*,#33375,.T.);
#44301=ORIENTED_EDGE('',*,*,#33376,.T.);
#44302=ORIENTED_EDGE('',*,*,#33371,.F.);
#44303=ORIENTED_EDGE('',*,*,#33377,.F.);
#44304=ORIENTED_EDGE('',*,*,#33378,.T.);
#44305=ORIENTED_EDGE('',*,*,#33379,.T.);
#44306=ORIENTED_EDGE('',*,*,#33375,.F.);
#44307=ORIENTED_EDGE('',*,*,#33380,.F.);
#44308=ORIENTED_EDGE('',*,*,#33373,.T.);
#44309=ORIENTED_EDGE('',*,*,#33381,.T.);
#44310=ORIENTED_EDGE('',*,*,#33378,.F.);
#44311=ORIENTED_EDGE('',*,*,#33381,.F.);
#44312=ORIENTED_EDGE('',*,*,#33372,.F.);
#44313=ORIENTED_EDGE('',*,*,#33376,.F.);
#44314=ORIENTED_EDGE('',*,*,#33379,.F.);
#44315=ORIENTED_EDGE('',*,*,#33382,.F.);
#44316=ORIENTED_EDGE('',*,*,#33383,.T.);
#44317=ORIENTED_EDGE('',*,*,#33384,.T.);
#44318=ORIENTED_EDGE('',*,*,#33385,.F.);
#44319=ORIENTED_EDGE('',*,*,#33386,.F.);
#44320=ORIENTED_EDGE('',*,*,#33387,.T.);
#44321=ORIENTED_EDGE('',*,*,#33388,.T.);
#44322=ORIENTED_EDGE('',*,*,#33383,.F.);
#44323=ORIENTED_EDGE('',*,*,#33389,.F.);
#44324=ORIENTED_EDGE('',*,*,#33390,.T.);
#44325=ORIENTED_EDGE('',*,*,#33391,.T.);
#44326=ORIENTED_EDGE('',*,*,#33387,.F.);
#44327=ORIENTED_EDGE('',*,*,#33392,.F.);
#44328=ORIENTED_EDGE('',*,*,#33385,.T.);
#44329=ORIENTED_EDGE('',*,*,#33393,.T.);
#44330=ORIENTED_EDGE('',*,*,#33390,.F.);
#44331=ORIENTED_EDGE('',*,*,#33393,.F.);
#44332=ORIENTED_EDGE('',*,*,#33384,.F.);
#44333=ORIENTED_EDGE('',*,*,#33388,.F.);
#44334=ORIENTED_EDGE('',*,*,#33391,.F.);
#44335=ORIENTED_EDGE('',*,*,#33394,.F.);
#44336=ORIENTED_EDGE('',*,*,#33395,.T.);
#44337=ORIENTED_EDGE('',*,*,#33396,.T.);
#44338=ORIENTED_EDGE('',*,*,#33397,.F.);
#44339=ORIENTED_EDGE('',*,*,#33398,.F.);
#44340=ORIENTED_EDGE('',*,*,#33399,.T.);
#44341=ORIENTED_EDGE('',*,*,#33400,.T.);
#44342=ORIENTED_EDGE('',*,*,#33395,.F.);
#44343=ORIENTED_EDGE('',*,*,#33401,.F.);
#44344=ORIENTED_EDGE('',*,*,#33402,.T.);
#44345=ORIENTED_EDGE('',*,*,#33403,.T.);
#44346=ORIENTED_EDGE('',*,*,#33399,.F.);
#44347=ORIENTED_EDGE('',*,*,#33404,.F.);
#44348=ORIENTED_EDGE('',*,*,#33397,.T.);
#44349=ORIENTED_EDGE('',*,*,#33405,.T.);
#44350=ORIENTED_EDGE('',*,*,#33402,.F.);
#44351=ORIENTED_EDGE('',*,*,#33405,.F.);
#44352=ORIENTED_EDGE('',*,*,#33396,.F.);
#44353=ORIENTED_EDGE('',*,*,#33400,.F.);
#44354=ORIENTED_EDGE('',*,*,#33403,.F.);
#44355=ORIENTED_EDGE('',*,*,#33406,.F.);
#44356=ORIENTED_EDGE('',*,*,#33407,.T.);
#44357=ORIENTED_EDGE('',*,*,#33408,.T.);
#44358=ORIENTED_EDGE('',*,*,#33409,.F.);
#44359=ORIENTED_EDGE('',*,*,#33410,.F.);
#44360=ORIENTED_EDGE('',*,*,#33411,.T.);
#44361=ORIENTED_EDGE('',*,*,#33412,.T.);
#44362=ORIENTED_EDGE('',*,*,#33407,.F.);
#44363=ORIENTED_EDGE('',*,*,#33413,.F.);
#44364=ORIENTED_EDGE('',*,*,#33414,.T.);
#44365=ORIENTED_EDGE('',*,*,#33415,.T.);
#44366=ORIENTED_EDGE('',*,*,#33411,.F.);
#44367=ORIENTED_EDGE('',*,*,#33416,.F.);
#44368=ORIENTED_EDGE('',*,*,#33409,.T.);
#44369=ORIENTED_EDGE('',*,*,#33417,.T.);
#44370=ORIENTED_EDGE('',*,*,#33414,.F.);
#44371=ORIENTED_EDGE('',*,*,#33417,.F.);
#44372=ORIENTED_EDGE('',*,*,#33408,.F.);
#44373=ORIENTED_EDGE('',*,*,#33412,.F.);
#44374=ORIENTED_EDGE('',*,*,#33415,.F.);
#44375=ORIENTED_EDGE('',*,*,#33418,.F.);
#44376=ORIENTED_EDGE('',*,*,#33419,.T.);
#44377=ORIENTED_EDGE('',*,*,#33420,.T.);
#44378=ORIENTED_EDGE('',*,*,#33421,.F.);
#44379=ORIENTED_EDGE('',*,*,#33422,.F.);
#44380=ORIENTED_EDGE('',*,*,#33423,.T.);
#44381=ORIENTED_EDGE('',*,*,#33424,.T.);
#44382=ORIENTED_EDGE('',*,*,#33419,.F.);
#44383=ORIENTED_EDGE('',*,*,#33425,.F.);
#44384=ORIENTED_EDGE('',*,*,#33426,.T.);
#44385=ORIENTED_EDGE('',*,*,#33427,.T.);
#44386=ORIENTED_EDGE('',*,*,#33423,.F.);
#44387=ORIENTED_EDGE('',*,*,#33428,.F.);
#44388=ORIENTED_EDGE('',*,*,#33421,.T.);
#44389=ORIENTED_EDGE('',*,*,#33429,.T.);
#44390=ORIENTED_EDGE('',*,*,#33426,.F.);
#44391=ORIENTED_EDGE('',*,*,#33429,.F.);
#44392=ORIENTED_EDGE('',*,*,#33420,.F.);
#44393=ORIENTED_EDGE('',*,*,#33424,.F.);
#44394=ORIENTED_EDGE('',*,*,#33427,.F.);
#44395=ORIENTED_EDGE('',*,*,#33430,.F.);
#44396=ORIENTED_EDGE('',*,*,#33431,.T.);
#44397=ORIENTED_EDGE('',*,*,#33432,.T.);
#44398=ORIENTED_EDGE('',*,*,#33433,.F.);
#44399=ORIENTED_EDGE('',*,*,#33434,.F.);
#44400=ORIENTED_EDGE('',*,*,#33435,.T.);
#44401=ORIENTED_EDGE('',*,*,#33436,.T.);
#44402=ORIENTED_EDGE('',*,*,#33431,.F.);
#44403=ORIENTED_EDGE('',*,*,#33437,.F.);
#44404=ORIENTED_EDGE('',*,*,#33438,.T.);
#44405=ORIENTED_EDGE('',*,*,#33439,.T.);
#44406=ORIENTED_EDGE('',*,*,#33435,.F.);
#44407=ORIENTED_EDGE('',*,*,#33440,.F.);
#44408=ORIENTED_EDGE('',*,*,#33433,.T.);
#44409=ORIENTED_EDGE('',*,*,#33441,.T.);
#44410=ORIENTED_EDGE('',*,*,#33438,.F.);
#44411=ORIENTED_EDGE('',*,*,#33441,.F.);
#44412=ORIENTED_EDGE('',*,*,#33432,.F.);
#44413=ORIENTED_EDGE('',*,*,#33436,.F.);
#44414=ORIENTED_EDGE('',*,*,#33439,.F.);
#44415=ORIENTED_EDGE('',*,*,#33442,.F.);
#44416=ORIENTED_EDGE('',*,*,#33443,.T.);
#44417=ORIENTED_EDGE('',*,*,#33444,.T.);
#44418=ORIENTED_EDGE('',*,*,#33445,.F.);
#44419=ORIENTED_EDGE('',*,*,#33446,.F.);
#44420=ORIENTED_EDGE('',*,*,#33447,.T.);
#44421=ORIENTED_EDGE('',*,*,#33448,.T.);
#44422=ORIENTED_EDGE('',*,*,#33443,.F.);
#44423=ORIENTED_EDGE('',*,*,#33449,.F.);
#44424=ORIENTED_EDGE('',*,*,#33450,.T.);
#44425=ORIENTED_EDGE('',*,*,#33451,.T.);
#44426=ORIENTED_EDGE('',*,*,#33447,.F.);
#44427=ORIENTED_EDGE('',*,*,#33452,.F.);
#44428=ORIENTED_EDGE('',*,*,#33445,.T.);
#44429=ORIENTED_EDGE('',*,*,#33453,.T.);
#44430=ORIENTED_EDGE('',*,*,#33450,.F.);
#44431=ORIENTED_EDGE('',*,*,#33453,.F.);
#44432=ORIENTED_EDGE('',*,*,#33444,.F.);
#44433=ORIENTED_EDGE('',*,*,#33448,.F.);
#44434=ORIENTED_EDGE('',*,*,#33451,.F.);
#44435=ORIENTED_EDGE('',*,*,#33454,.F.);
#44436=ORIENTED_EDGE('',*,*,#33455,.T.);
#44437=ORIENTED_EDGE('',*,*,#33456,.T.);
#44438=ORIENTED_EDGE('',*,*,#33457,.F.);
#44439=ORIENTED_EDGE('',*,*,#33458,.F.);
#44440=ORIENTED_EDGE('',*,*,#33459,.T.);
#44441=ORIENTED_EDGE('',*,*,#33460,.T.);
#44442=ORIENTED_EDGE('',*,*,#33455,.F.);
#44443=ORIENTED_EDGE('',*,*,#33461,.F.);
#44444=ORIENTED_EDGE('',*,*,#33462,.T.);
#44445=ORIENTED_EDGE('',*,*,#33463,.T.);
#44446=ORIENTED_EDGE('',*,*,#33459,.F.);
#44447=ORIENTED_EDGE('',*,*,#33464,.F.);
#44448=ORIENTED_EDGE('',*,*,#33457,.T.);
#44449=ORIENTED_EDGE('',*,*,#33465,.T.);
#44450=ORIENTED_EDGE('',*,*,#33462,.F.);
#44451=ORIENTED_EDGE('',*,*,#33465,.F.);
#44452=ORIENTED_EDGE('',*,*,#33456,.F.);
#44453=ORIENTED_EDGE('',*,*,#33460,.F.);
#44454=ORIENTED_EDGE('',*,*,#33463,.F.);
#44455=ORIENTED_EDGE('',*,*,#33466,.F.);
#44456=ORIENTED_EDGE('',*,*,#33467,.T.);
#44457=ORIENTED_EDGE('',*,*,#33468,.T.);
#44458=ORIENTED_EDGE('',*,*,#33469,.F.);
#44459=ORIENTED_EDGE('',*,*,#33470,.F.);
#44460=ORIENTED_EDGE('',*,*,#33471,.T.);
#44461=ORIENTED_EDGE('',*,*,#33472,.T.);
#44462=ORIENTED_EDGE('',*,*,#33467,.F.);
#44463=ORIENTED_EDGE('',*,*,#33473,.F.);
#44464=ORIENTED_EDGE('',*,*,#33474,.T.);
#44465=ORIENTED_EDGE('',*,*,#33475,.T.);
#44466=ORIENTED_EDGE('',*,*,#33471,.F.);
#44467=ORIENTED_EDGE('',*,*,#33476,.F.);
#44468=ORIENTED_EDGE('',*,*,#33469,.T.);
#44469=ORIENTED_EDGE('',*,*,#33477,.T.);
#44470=ORIENTED_EDGE('',*,*,#33474,.F.);
#44471=ORIENTED_EDGE('',*,*,#33477,.F.);
#44472=ORIENTED_EDGE('',*,*,#33468,.F.);
#44473=ORIENTED_EDGE('',*,*,#33472,.F.);
#44474=ORIENTED_EDGE('',*,*,#33475,.F.);
#44475=ORIENTED_EDGE('',*,*,#33478,.F.);
#44476=ORIENTED_EDGE('',*,*,#33479,.T.);
#44477=ORIENTED_EDGE('',*,*,#33480,.T.);
#44478=ORIENTED_EDGE('',*,*,#33481,.F.);
#44479=ORIENTED_EDGE('',*,*,#33482,.F.);
#44480=ORIENTED_EDGE('',*,*,#33483,.T.);
#44481=ORIENTED_EDGE('',*,*,#33484,.T.);
#44482=ORIENTED_EDGE('',*,*,#33479,.F.);
#44483=ORIENTED_EDGE('',*,*,#33485,.F.);
#44484=ORIENTED_EDGE('',*,*,#33486,.T.);
#44485=ORIENTED_EDGE('',*,*,#33487,.T.);
#44486=ORIENTED_EDGE('',*,*,#33483,.F.);
#44487=ORIENTED_EDGE('',*,*,#33488,.F.);
#44488=ORIENTED_EDGE('',*,*,#33481,.T.);
#44489=ORIENTED_EDGE('',*,*,#33489,.T.);
#44490=ORIENTED_EDGE('',*,*,#33486,.F.);
#44491=ORIENTED_EDGE('',*,*,#33489,.F.);
#44492=ORIENTED_EDGE('',*,*,#33480,.F.);
#44493=ORIENTED_EDGE('',*,*,#33484,.F.);
#44494=ORIENTED_EDGE('',*,*,#33487,.F.);
#44495=ORIENTED_EDGE('',*,*,#33490,.F.);
#44496=ORIENTED_EDGE('',*,*,#33491,.T.);
#44497=ORIENTED_EDGE('',*,*,#33492,.T.);
#44498=ORIENTED_EDGE('',*,*,#33493,.F.);
#44499=ORIENTED_EDGE('',*,*,#33494,.F.);
#44500=ORIENTED_EDGE('',*,*,#33495,.T.);
#44501=ORIENTED_EDGE('',*,*,#33496,.T.);
#44502=ORIENTED_EDGE('',*,*,#33491,.F.);
#44503=ORIENTED_EDGE('',*,*,#33497,.F.);
#44504=ORIENTED_EDGE('',*,*,#33498,.T.);
#44505=ORIENTED_EDGE('',*,*,#33499,.T.);
#44506=ORIENTED_EDGE('',*,*,#33495,.F.);
#44507=ORIENTED_EDGE('',*,*,#33500,.F.);
#44508=ORIENTED_EDGE('',*,*,#33493,.T.);
#44509=ORIENTED_EDGE('',*,*,#33501,.T.);
#44510=ORIENTED_EDGE('',*,*,#33498,.F.);
#44511=ORIENTED_EDGE('',*,*,#33501,.F.);
#44512=ORIENTED_EDGE('',*,*,#33492,.F.);
#44513=ORIENTED_EDGE('',*,*,#33496,.F.);
#44514=ORIENTED_EDGE('',*,*,#33499,.F.);
#44515=ORIENTED_EDGE('',*,*,#33502,.F.);
#44516=ORIENTED_EDGE('',*,*,#33503,.T.);
#44517=ORIENTED_EDGE('',*,*,#33504,.T.);
#44518=ORIENTED_EDGE('',*,*,#33505,.F.);
#44519=ORIENTED_EDGE('',*,*,#33506,.F.);
#44520=ORIENTED_EDGE('',*,*,#33507,.T.);
#44521=ORIENTED_EDGE('',*,*,#33508,.T.);
#44522=ORIENTED_EDGE('',*,*,#33503,.F.);
#44523=ORIENTED_EDGE('',*,*,#33509,.F.);
#44524=ORIENTED_EDGE('',*,*,#33510,.T.);
#44525=ORIENTED_EDGE('',*,*,#33511,.T.);
#44526=ORIENTED_EDGE('',*,*,#33507,.F.);
#44527=ORIENTED_EDGE('',*,*,#33512,.F.);
#44528=ORIENTED_EDGE('',*,*,#33505,.T.);
#44529=ORIENTED_EDGE('',*,*,#33513,.T.);
#44530=ORIENTED_EDGE('',*,*,#33510,.F.);
#44531=ORIENTED_EDGE('',*,*,#33513,.F.);
#44532=ORIENTED_EDGE('',*,*,#33504,.F.);
#44533=ORIENTED_EDGE('',*,*,#33508,.F.);
#44534=ORIENTED_EDGE('',*,*,#33511,.F.);
#44535=ORIENTED_EDGE('',*,*,#33514,.F.);
#44536=ORIENTED_EDGE('',*,*,#33515,.T.);
#44537=ORIENTED_EDGE('',*,*,#33516,.T.);
#44538=ORIENTED_EDGE('',*,*,#33517,.F.);
#44539=ORIENTED_EDGE('',*,*,#33518,.F.);
#44540=ORIENTED_EDGE('',*,*,#33519,.T.);
#44541=ORIENTED_EDGE('',*,*,#33520,.T.);
#44542=ORIENTED_EDGE('',*,*,#33515,.F.);
#44543=ORIENTED_EDGE('',*,*,#33521,.F.);
#44544=ORIENTED_EDGE('',*,*,#33522,.T.);
#44545=ORIENTED_EDGE('',*,*,#33523,.T.);
#44546=ORIENTED_EDGE('',*,*,#33519,.F.);
#44547=ORIENTED_EDGE('',*,*,#33524,.F.);
#44548=ORIENTED_EDGE('',*,*,#33517,.T.);
#44549=ORIENTED_EDGE('',*,*,#33525,.T.);
#44550=ORIENTED_EDGE('',*,*,#33522,.F.);
#44551=ORIENTED_EDGE('',*,*,#33525,.F.);
#44552=ORIENTED_EDGE('',*,*,#33516,.F.);
#44553=ORIENTED_EDGE('',*,*,#33520,.F.);
#44554=ORIENTED_EDGE('',*,*,#33523,.F.);
#44555=ORIENTED_EDGE('',*,*,#33526,.F.);
#44556=ORIENTED_EDGE('',*,*,#33527,.T.);
#44557=ORIENTED_EDGE('',*,*,#33528,.T.);
#44558=ORIENTED_EDGE('',*,*,#33529,.F.);
#44559=ORIENTED_EDGE('',*,*,#33530,.F.);
#44560=ORIENTED_EDGE('',*,*,#33531,.T.);
#44561=ORIENTED_EDGE('',*,*,#33532,.T.);
#44562=ORIENTED_EDGE('',*,*,#33527,.F.);
#44563=ORIENTED_EDGE('',*,*,#33533,.F.);
#44564=ORIENTED_EDGE('',*,*,#33534,.T.);
#44565=ORIENTED_EDGE('',*,*,#33535,.T.);
#44566=ORIENTED_EDGE('',*,*,#33531,.F.);
#44567=ORIENTED_EDGE('',*,*,#33536,.F.);
#44568=ORIENTED_EDGE('',*,*,#33529,.T.);
#44569=ORIENTED_EDGE('',*,*,#33537,.T.);
#44570=ORIENTED_EDGE('',*,*,#33534,.F.);
#44571=ORIENTED_EDGE('',*,*,#33537,.F.);
#44572=ORIENTED_EDGE('',*,*,#33528,.F.);
#44573=ORIENTED_EDGE('',*,*,#33532,.F.);
#44574=ORIENTED_EDGE('',*,*,#33535,.F.);
#44575=ORIENTED_EDGE('',*,*,#33538,.F.);
#44576=ORIENTED_EDGE('',*,*,#33539,.T.);
#44577=ORIENTED_EDGE('',*,*,#33540,.T.);
#44578=ORIENTED_EDGE('',*,*,#33541,.F.);
#44579=ORIENTED_EDGE('',*,*,#33542,.F.);
#44580=ORIENTED_EDGE('',*,*,#33543,.T.);
#44581=ORIENTED_EDGE('',*,*,#33544,.T.);
#44582=ORIENTED_EDGE('',*,*,#33539,.F.);
#44583=ORIENTED_EDGE('',*,*,#33545,.F.);
#44584=ORIENTED_EDGE('',*,*,#33546,.T.);
#44585=ORIENTED_EDGE('',*,*,#33547,.T.);
#44586=ORIENTED_EDGE('',*,*,#33543,.F.);
#44587=ORIENTED_EDGE('',*,*,#33548,.F.);
#44588=ORIENTED_EDGE('',*,*,#33541,.T.);
#44589=ORIENTED_EDGE('',*,*,#33549,.T.);
#44590=ORIENTED_EDGE('',*,*,#33546,.F.);
#44591=ORIENTED_EDGE('',*,*,#33549,.F.);
#44592=ORIENTED_EDGE('',*,*,#33540,.F.);
#44593=ORIENTED_EDGE('',*,*,#33544,.F.);
#44594=ORIENTED_EDGE('',*,*,#33547,.F.);
#44595=ORIENTED_EDGE('',*,*,#33550,.F.);
#44596=ORIENTED_EDGE('',*,*,#33551,.T.);
#44597=ORIENTED_EDGE('',*,*,#33552,.T.);
#44598=ORIENTED_EDGE('',*,*,#33553,.F.);
#44599=ORIENTED_EDGE('',*,*,#33554,.F.);
#44600=ORIENTED_EDGE('',*,*,#33555,.T.);
#44601=ORIENTED_EDGE('',*,*,#33556,.T.);
#44602=ORIENTED_EDGE('',*,*,#33551,.F.);
#44603=ORIENTED_EDGE('',*,*,#33557,.F.);
#44604=ORIENTED_EDGE('',*,*,#33558,.T.);
#44605=ORIENTED_EDGE('',*,*,#33559,.T.);
#44606=ORIENTED_EDGE('',*,*,#33555,.F.);
#44607=ORIENTED_EDGE('',*,*,#33560,.F.);
#44608=ORIENTED_EDGE('',*,*,#33553,.T.);
#44609=ORIENTED_EDGE('',*,*,#33561,.T.);
#44610=ORIENTED_EDGE('',*,*,#33558,.F.);
#44611=ORIENTED_EDGE('',*,*,#33561,.F.);
#44612=ORIENTED_EDGE('',*,*,#33552,.F.);
#44613=ORIENTED_EDGE('',*,*,#33556,.F.);
#44614=ORIENTED_EDGE('',*,*,#33559,.F.);
#44615=ORIENTED_EDGE('',*,*,#33562,.F.);
#44616=ORIENTED_EDGE('',*,*,#33563,.T.);
#44617=ORIENTED_EDGE('',*,*,#33564,.T.);
#44618=ORIENTED_EDGE('',*,*,#33565,.F.);
#44619=ORIENTED_EDGE('',*,*,#33566,.F.);
#44620=ORIENTED_EDGE('',*,*,#33567,.T.);
#44621=ORIENTED_EDGE('',*,*,#33568,.T.);
#44622=ORIENTED_EDGE('',*,*,#33563,.F.);
#44623=ORIENTED_EDGE('',*,*,#33569,.F.);
#44624=ORIENTED_EDGE('',*,*,#33570,.T.);
#44625=ORIENTED_EDGE('',*,*,#33571,.T.);
#44626=ORIENTED_EDGE('',*,*,#33567,.F.);
#44627=ORIENTED_EDGE('',*,*,#33572,.F.);
#44628=ORIENTED_EDGE('',*,*,#33565,.T.);
#44629=ORIENTED_EDGE('',*,*,#33573,.T.);
#44630=ORIENTED_EDGE('',*,*,#33570,.F.);
#44631=ORIENTED_EDGE('',*,*,#33573,.F.);
#44632=ORIENTED_EDGE('',*,*,#33564,.F.);
#44633=ORIENTED_EDGE('',*,*,#33568,.F.);
#44634=ORIENTED_EDGE('',*,*,#33571,.F.);
#44635=ORIENTED_EDGE('',*,*,#33574,.F.);
#44636=ORIENTED_EDGE('',*,*,#33575,.T.);
#44637=ORIENTED_EDGE('',*,*,#33576,.T.);
#44638=ORIENTED_EDGE('',*,*,#33577,.F.);
#44639=ORIENTED_EDGE('',*,*,#33578,.F.);
#44640=ORIENTED_EDGE('',*,*,#33579,.T.);
#44641=ORIENTED_EDGE('',*,*,#33580,.T.);
#44642=ORIENTED_EDGE('',*,*,#33575,.F.);
#44643=ORIENTED_EDGE('',*,*,#33581,.F.);
#44644=ORIENTED_EDGE('',*,*,#33582,.T.);
#44645=ORIENTED_EDGE('',*,*,#33583,.T.);
#44646=ORIENTED_EDGE('',*,*,#33579,.F.);
#44647=ORIENTED_EDGE('',*,*,#33584,.F.);
#44648=ORIENTED_EDGE('',*,*,#33577,.T.);
#44649=ORIENTED_EDGE('',*,*,#33585,.T.);
#44650=ORIENTED_EDGE('',*,*,#33582,.F.);
#44651=ORIENTED_EDGE('',*,*,#33585,.F.);
#44652=ORIENTED_EDGE('',*,*,#33576,.F.);
#44653=ORIENTED_EDGE('',*,*,#33580,.F.);
#44654=ORIENTED_EDGE('',*,*,#33583,.F.);
#44655=ORIENTED_EDGE('',*,*,#33586,.F.);
#44656=ORIENTED_EDGE('',*,*,#33587,.T.);
#44657=ORIENTED_EDGE('',*,*,#33588,.T.);
#44658=ORIENTED_EDGE('',*,*,#33589,.F.);
#44659=ORIENTED_EDGE('',*,*,#33590,.F.);
#44660=ORIENTED_EDGE('',*,*,#33591,.T.);
#44661=ORIENTED_EDGE('',*,*,#33592,.T.);
#44662=ORIENTED_EDGE('',*,*,#33587,.F.);
#44663=ORIENTED_EDGE('',*,*,#33593,.F.);
#44664=ORIENTED_EDGE('',*,*,#33594,.T.);
#44665=ORIENTED_EDGE('',*,*,#33595,.T.);
#44666=ORIENTED_EDGE('',*,*,#33591,.F.);
#44667=ORIENTED_EDGE('',*,*,#33596,.F.);
#44668=ORIENTED_EDGE('',*,*,#33589,.T.);
#44669=ORIENTED_EDGE('',*,*,#33597,.T.);
#44670=ORIENTED_EDGE('',*,*,#33594,.F.);
#44671=ORIENTED_EDGE('',*,*,#33597,.F.);
#44672=ORIENTED_EDGE('',*,*,#33588,.F.);
#44673=ORIENTED_EDGE('',*,*,#33592,.F.);
#44674=ORIENTED_EDGE('',*,*,#33595,.F.);
#44675=ORIENTED_EDGE('',*,*,#33598,.F.);
#44676=ORIENTED_EDGE('',*,*,#33599,.T.);
#44677=ORIENTED_EDGE('',*,*,#33600,.T.);
#44678=ORIENTED_EDGE('',*,*,#33601,.F.);
#44679=ORIENTED_EDGE('',*,*,#33602,.F.);
#44680=ORIENTED_EDGE('',*,*,#33603,.T.);
#44681=ORIENTED_EDGE('',*,*,#33604,.T.);
#44682=ORIENTED_EDGE('',*,*,#33599,.F.);
#44683=ORIENTED_EDGE('',*,*,#33605,.F.);
#44684=ORIENTED_EDGE('',*,*,#33606,.T.);
#44685=ORIENTED_EDGE('',*,*,#33607,.T.);
#44686=ORIENTED_EDGE('',*,*,#33603,.F.);
#44687=ORIENTED_EDGE('',*,*,#33608,.F.);
#44688=ORIENTED_EDGE('',*,*,#33601,.T.);
#44689=ORIENTED_EDGE('',*,*,#33609,.T.);
#44690=ORIENTED_EDGE('',*,*,#33606,.F.);
#44691=ORIENTED_EDGE('',*,*,#33609,.F.);
#44692=ORIENTED_EDGE('',*,*,#33600,.F.);
#44693=ORIENTED_EDGE('',*,*,#33604,.F.);
#44694=ORIENTED_EDGE('',*,*,#33607,.F.);
#44695=ORIENTED_EDGE('',*,*,#33610,.F.);
#44696=ORIENTED_EDGE('',*,*,#33611,.T.);
#44697=ORIENTED_EDGE('',*,*,#33612,.T.);
#44698=ORIENTED_EDGE('',*,*,#33613,.F.);
#44699=ORIENTED_EDGE('',*,*,#33614,.F.);
#44700=ORIENTED_EDGE('',*,*,#33615,.T.);
#44701=ORIENTED_EDGE('',*,*,#33616,.T.);
#44702=ORIENTED_EDGE('',*,*,#33611,.F.);
#44703=ORIENTED_EDGE('',*,*,#33617,.F.);
#44704=ORIENTED_EDGE('',*,*,#33618,.T.);
#44705=ORIENTED_EDGE('',*,*,#33619,.T.);
#44706=ORIENTED_EDGE('',*,*,#33615,.F.);
#44707=ORIENTED_EDGE('',*,*,#33620,.F.);
#44708=ORIENTED_EDGE('',*,*,#33613,.T.);
#44709=ORIENTED_EDGE('',*,*,#33621,.T.);
#44710=ORIENTED_EDGE('',*,*,#33618,.F.);
#44711=ORIENTED_EDGE('',*,*,#33621,.F.);
#44712=ORIENTED_EDGE('',*,*,#33612,.F.);
#44713=ORIENTED_EDGE('',*,*,#33616,.F.);
#44714=ORIENTED_EDGE('',*,*,#33619,.F.);
#44715=ORIENTED_EDGE('',*,*,#33622,.F.);
#44716=ORIENTED_EDGE('',*,*,#33623,.T.);
#44717=ORIENTED_EDGE('',*,*,#33624,.T.);
#44718=ORIENTED_EDGE('',*,*,#33625,.F.);
#44719=ORIENTED_EDGE('',*,*,#33626,.F.);
#44720=ORIENTED_EDGE('',*,*,#33627,.T.);
#44721=ORIENTED_EDGE('',*,*,#33628,.T.);
#44722=ORIENTED_EDGE('',*,*,#33623,.F.);
#44723=ORIENTED_EDGE('',*,*,#33629,.F.);
#44724=ORIENTED_EDGE('',*,*,#33630,.T.);
#44725=ORIENTED_EDGE('',*,*,#33631,.T.);
#44726=ORIENTED_EDGE('',*,*,#33627,.F.);
#44727=ORIENTED_EDGE('',*,*,#33632,.F.);
#44728=ORIENTED_EDGE('',*,*,#33625,.T.);
#44729=ORIENTED_EDGE('',*,*,#33633,.T.);
#44730=ORIENTED_EDGE('',*,*,#33630,.F.);
#44731=ORIENTED_EDGE('',*,*,#33633,.F.);
#44732=ORIENTED_EDGE('',*,*,#33624,.F.);
#44733=ORIENTED_EDGE('',*,*,#33628,.F.);
#44734=ORIENTED_EDGE('',*,*,#33631,.F.);
#44735=ORIENTED_EDGE('',*,*,#33634,.F.);
#44736=ORIENTED_EDGE('',*,*,#33635,.T.);
#44737=ORIENTED_EDGE('',*,*,#33636,.T.);
#44738=ORIENTED_EDGE('',*,*,#33637,.F.);
#44739=ORIENTED_EDGE('',*,*,#33638,.F.);
#44740=ORIENTED_EDGE('',*,*,#33639,.T.);
#44741=ORIENTED_EDGE('',*,*,#33640,.T.);
#44742=ORIENTED_EDGE('',*,*,#33635,.F.);
#44743=ORIENTED_EDGE('',*,*,#33641,.F.);
#44744=ORIENTED_EDGE('',*,*,#33642,.T.);
#44745=ORIENTED_EDGE('',*,*,#33643,.T.);
#44746=ORIENTED_EDGE('',*,*,#33639,.F.);
#44747=ORIENTED_EDGE('',*,*,#33644,.F.);
#44748=ORIENTED_EDGE('',*,*,#33637,.T.);
#44749=ORIENTED_EDGE('',*,*,#33645,.T.);
#44750=ORIENTED_EDGE('',*,*,#33642,.F.);
#44751=ORIENTED_EDGE('',*,*,#33645,.F.);
#44752=ORIENTED_EDGE('',*,*,#33636,.F.);
#44753=ORIENTED_EDGE('',*,*,#33640,.F.);
#44754=ORIENTED_EDGE('',*,*,#33643,.F.);
#44755=ORIENTED_EDGE('',*,*,#33646,.F.);
#44756=ORIENTED_EDGE('',*,*,#33647,.T.);
#44757=ORIENTED_EDGE('',*,*,#33648,.T.);
#44758=ORIENTED_EDGE('',*,*,#33649,.F.);
#44759=ORIENTED_EDGE('',*,*,#33650,.F.);
#44760=ORIENTED_EDGE('',*,*,#33651,.T.);
#44761=ORIENTED_EDGE('',*,*,#33652,.T.);
#44762=ORIENTED_EDGE('',*,*,#33647,.F.);
#44763=ORIENTED_EDGE('',*,*,#33653,.F.);
#44764=ORIENTED_EDGE('',*,*,#33654,.T.);
#44765=ORIENTED_EDGE('',*,*,#33655,.T.);
#44766=ORIENTED_EDGE('',*,*,#33651,.F.);
#44767=ORIENTED_EDGE('',*,*,#33656,.F.);
#44768=ORIENTED_EDGE('',*,*,#33649,.T.);
#44769=ORIENTED_EDGE('',*,*,#33657,.T.);
#44770=ORIENTED_EDGE('',*,*,#33654,.F.);
#44771=ORIENTED_EDGE('',*,*,#33657,.F.);
#44772=ORIENTED_EDGE('',*,*,#33648,.F.);
#44773=ORIENTED_EDGE('',*,*,#33652,.F.);
#44774=ORIENTED_EDGE('',*,*,#33655,.F.);
#44775=ORIENTED_EDGE('',*,*,#33658,.F.);
#44776=ORIENTED_EDGE('',*,*,#33659,.T.);
#44777=ORIENTED_EDGE('',*,*,#33660,.T.);
#44778=ORIENTED_EDGE('',*,*,#33661,.F.);
#44779=ORIENTED_EDGE('',*,*,#33662,.F.);
#44780=ORIENTED_EDGE('',*,*,#33663,.T.);
#44781=ORIENTED_EDGE('',*,*,#33664,.T.);
#44782=ORIENTED_EDGE('',*,*,#33659,.F.);
#44783=ORIENTED_EDGE('',*,*,#33665,.F.);
#44784=ORIENTED_EDGE('',*,*,#33666,.T.);
#44785=ORIENTED_EDGE('',*,*,#33667,.T.);
#44786=ORIENTED_EDGE('',*,*,#33663,.F.);
#44787=ORIENTED_EDGE('',*,*,#33668,.F.);
#44788=ORIENTED_EDGE('',*,*,#33661,.T.);
#44789=ORIENTED_EDGE('',*,*,#33669,.T.);
#44790=ORIENTED_EDGE('',*,*,#33666,.F.);
#44791=ORIENTED_EDGE('',*,*,#33669,.F.);
#44792=ORIENTED_EDGE('',*,*,#33660,.F.);
#44793=ORIENTED_EDGE('',*,*,#33664,.F.);
#44794=ORIENTED_EDGE('',*,*,#33667,.F.);
#44795=ORIENTED_EDGE('',*,*,#33670,.F.);
#44796=ORIENTED_EDGE('',*,*,#33671,.T.);
#44797=ORIENTED_EDGE('',*,*,#33672,.T.);
#44798=ORIENTED_EDGE('',*,*,#33673,.F.);
#44799=ORIENTED_EDGE('',*,*,#33674,.F.);
#44800=ORIENTED_EDGE('',*,*,#33675,.T.);
#44801=ORIENTED_EDGE('',*,*,#33676,.T.);
#44802=ORIENTED_EDGE('',*,*,#33671,.F.);
#44803=ORIENTED_EDGE('',*,*,#33677,.F.);
#44804=ORIENTED_EDGE('',*,*,#33678,.T.);
#44805=ORIENTED_EDGE('',*,*,#33679,.T.);
#44806=ORIENTED_EDGE('',*,*,#33675,.F.);
#44807=ORIENTED_EDGE('',*,*,#33680,.F.);
#44808=ORIENTED_EDGE('',*,*,#33673,.T.);
#44809=ORIENTED_EDGE('',*,*,#33681,.T.);
#44810=ORIENTED_EDGE('',*,*,#33678,.F.);
#44811=ORIENTED_EDGE('',*,*,#33681,.F.);
#44812=ORIENTED_EDGE('',*,*,#33672,.F.);
#44813=ORIENTED_EDGE('',*,*,#33676,.F.);
#44814=ORIENTED_EDGE('',*,*,#33679,.F.);
#44815=ORIENTED_EDGE('',*,*,#33682,.F.);
#44816=ORIENTED_EDGE('',*,*,#33683,.T.);
#44817=ORIENTED_EDGE('',*,*,#33684,.T.);
#44818=ORIENTED_EDGE('',*,*,#33685,.F.);
#44819=ORIENTED_EDGE('',*,*,#33686,.F.);
#44820=ORIENTED_EDGE('',*,*,#33687,.T.);
#44821=ORIENTED_EDGE('',*,*,#33688,.T.);
#44822=ORIENTED_EDGE('',*,*,#33683,.F.);
#44823=ORIENTED_EDGE('',*,*,#33689,.F.);
#44824=ORIENTED_EDGE('',*,*,#33690,.T.);
#44825=ORIENTED_EDGE('',*,*,#33691,.T.);
#44826=ORIENTED_EDGE('',*,*,#33687,.F.);
#44827=ORIENTED_EDGE('',*,*,#33692,.F.);
#44828=ORIENTED_EDGE('',*,*,#33685,.T.);
#44829=ORIENTED_EDGE('',*,*,#33693,.T.);
#44830=ORIENTED_EDGE('',*,*,#33690,.F.);
#44831=ORIENTED_EDGE('',*,*,#33693,.F.);
#44832=ORIENTED_EDGE('',*,*,#33684,.F.);
#44833=ORIENTED_EDGE('',*,*,#33688,.F.);
#44834=ORIENTED_EDGE('',*,*,#33691,.F.);
#44835=ORIENTED_EDGE('',*,*,#33694,.F.);
#44836=ORIENTED_EDGE('',*,*,#33695,.T.);
#44837=ORIENTED_EDGE('',*,*,#33696,.T.);
#44838=ORIENTED_EDGE('',*,*,#33697,.F.);
#44839=ORIENTED_EDGE('',*,*,#33698,.F.);
#44840=ORIENTED_EDGE('',*,*,#33699,.T.);
#44841=ORIENTED_EDGE('',*,*,#33700,.T.);
#44842=ORIENTED_EDGE('',*,*,#33695,.F.);
#44843=ORIENTED_EDGE('',*,*,#33701,.F.);
#44844=ORIENTED_EDGE('',*,*,#33702,.T.);
#44845=ORIENTED_EDGE('',*,*,#33703,.T.);
#44846=ORIENTED_EDGE('',*,*,#33699,.F.);
#44847=ORIENTED_EDGE('',*,*,#33704,.F.);
#44848=ORIENTED_EDGE('',*,*,#33697,.T.);
#44849=ORIENTED_EDGE('',*,*,#33705,.T.);
#44850=ORIENTED_EDGE('',*,*,#33702,.F.);
#44851=ORIENTED_EDGE('',*,*,#33705,.F.);
#44852=ORIENTED_EDGE('',*,*,#33696,.F.);
#44853=ORIENTED_EDGE('',*,*,#33700,.F.);
#44854=ORIENTED_EDGE('',*,*,#33703,.F.);
#44855=ORIENTED_EDGE('',*,*,#33706,.F.);
#44856=ORIENTED_EDGE('',*,*,#33707,.T.);
#44857=ORIENTED_EDGE('',*,*,#33708,.T.);
#44858=ORIENTED_EDGE('',*,*,#33709,.F.);
#44859=ORIENTED_EDGE('',*,*,#33710,.F.);
#44860=ORIENTED_EDGE('',*,*,#33711,.T.);
#44861=ORIENTED_EDGE('',*,*,#33712,.T.);
#44862=ORIENTED_EDGE('',*,*,#33707,.F.);
#44863=ORIENTED_EDGE('',*,*,#33713,.F.);
#44864=ORIENTED_EDGE('',*,*,#33714,.T.);
#44865=ORIENTED_EDGE('',*,*,#33715,.T.);
#44866=ORIENTED_EDGE('',*,*,#33711,.F.);
#44867=ORIENTED_EDGE('',*,*,#33716,.F.);
#44868=ORIENTED_EDGE('',*,*,#33709,.T.);
#44869=ORIENTED_EDGE('',*,*,#33717,.T.);
#44870=ORIENTED_EDGE('',*,*,#33714,.F.);
#44871=ORIENTED_EDGE('',*,*,#33717,.F.);
#44872=ORIENTED_EDGE('',*,*,#33708,.F.);
#44873=ORIENTED_EDGE('',*,*,#33712,.F.);
#44874=ORIENTED_EDGE('',*,*,#33715,.F.);
#44875=ORIENTED_EDGE('',*,*,#33718,.F.);
#44876=ORIENTED_EDGE('',*,*,#33719,.T.);
#44877=ORIENTED_EDGE('',*,*,#33720,.T.);
#44878=ORIENTED_EDGE('',*,*,#33721,.F.);
#44879=ORIENTED_EDGE('',*,*,#33722,.F.);
#44880=ORIENTED_EDGE('',*,*,#33723,.T.);
#44881=ORIENTED_EDGE('',*,*,#33724,.T.);
#44882=ORIENTED_EDGE('',*,*,#33719,.F.);
#44883=ORIENTED_EDGE('',*,*,#33725,.F.);
#44884=ORIENTED_EDGE('',*,*,#33726,.T.);
#44885=ORIENTED_EDGE('',*,*,#33727,.T.);
#44886=ORIENTED_EDGE('',*,*,#33723,.F.);
#44887=ORIENTED_EDGE('',*,*,#33728,.F.);
#44888=ORIENTED_EDGE('',*,*,#33721,.T.);
#44889=ORIENTED_EDGE('',*,*,#33729,.T.);
#44890=ORIENTED_EDGE('',*,*,#33726,.F.);
#44891=ORIENTED_EDGE('',*,*,#33729,.F.);
#44892=ORIENTED_EDGE('',*,*,#33720,.F.);
#44893=ORIENTED_EDGE('',*,*,#33724,.F.);
#44894=ORIENTED_EDGE('',*,*,#33727,.F.);
#44895=ORIENTED_EDGE('',*,*,#33730,.F.);
#44896=ORIENTED_EDGE('',*,*,#33731,.T.);
#44897=ORIENTED_EDGE('',*,*,#33732,.T.);
#44898=ORIENTED_EDGE('',*,*,#33733,.F.);
#44899=ORIENTED_EDGE('',*,*,#33734,.F.);
#44900=ORIENTED_EDGE('',*,*,#33735,.T.);
#44901=ORIENTED_EDGE('',*,*,#33736,.T.);
#44902=ORIENTED_EDGE('',*,*,#33731,.F.);
#44903=ORIENTED_EDGE('',*,*,#33737,.F.);
#44904=ORIENTED_EDGE('',*,*,#33738,.T.);
#44905=ORIENTED_EDGE('',*,*,#33739,.T.);
#44906=ORIENTED_EDGE('',*,*,#33735,.F.);
#44907=ORIENTED_EDGE('',*,*,#33740,.F.);
#44908=ORIENTED_EDGE('',*,*,#33733,.T.);
#44909=ORIENTED_EDGE('',*,*,#33741,.T.);
#44910=ORIENTED_EDGE('',*,*,#33738,.F.);
#44911=ORIENTED_EDGE('',*,*,#33741,.F.);
#44912=ORIENTED_EDGE('',*,*,#33732,.F.);
#44913=ORIENTED_EDGE('',*,*,#33736,.F.);
#44914=ORIENTED_EDGE('',*,*,#33739,.F.);
#44915=ORIENTED_EDGE('',*,*,#33742,.F.);
#44916=ORIENTED_EDGE('',*,*,#33743,.T.);
#44917=ORIENTED_EDGE('',*,*,#33744,.T.);
#44918=ORIENTED_EDGE('',*,*,#33745,.F.);
#44919=ORIENTED_EDGE('',*,*,#33746,.F.);
#44920=ORIENTED_EDGE('',*,*,#33747,.T.);
#44921=ORIENTED_EDGE('',*,*,#33748,.T.);
#44922=ORIENTED_EDGE('',*,*,#33743,.F.);
#44923=ORIENTED_EDGE('',*,*,#33749,.F.);
#44924=ORIENTED_EDGE('',*,*,#33750,.T.);
#44925=ORIENTED_EDGE('',*,*,#33751,.T.);
#44926=ORIENTED_EDGE('',*,*,#33747,.F.);
#44927=ORIENTED_EDGE('',*,*,#33752,.F.);
#44928=ORIENTED_EDGE('',*,*,#33745,.T.);
#44929=ORIENTED_EDGE('',*,*,#33753,.T.);
#44930=ORIENTED_EDGE('',*,*,#33750,.F.);
#44931=ORIENTED_EDGE('',*,*,#33753,.F.);
#44932=ORIENTED_EDGE('',*,*,#33744,.F.);
#44933=ORIENTED_EDGE('',*,*,#33748,.F.);
#44934=ORIENTED_EDGE('',*,*,#33751,.F.);
#44935=ORIENTED_EDGE('',*,*,#33754,.F.);
#44936=ORIENTED_EDGE('',*,*,#33755,.T.);
#44937=ORIENTED_EDGE('',*,*,#33756,.T.);
#44938=ORIENTED_EDGE('',*,*,#33757,.F.);
#44939=ORIENTED_EDGE('',*,*,#33758,.F.);
#44940=ORIENTED_EDGE('',*,*,#33759,.T.);
#44941=ORIENTED_EDGE('',*,*,#33760,.T.);
#44942=ORIENTED_EDGE('',*,*,#33755,.F.);
#44943=ORIENTED_EDGE('',*,*,#33761,.F.);
#44944=ORIENTED_EDGE('',*,*,#33762,.T.);
#44945=ORIENTED_EDGE('',*,*,#33763,.T.);
#44946=ORIENTED_EDGE('',*,*,#33759,.F.);
#44947=ORIENTED_EDGE('',*,*,#33764,.F.);
#44948=ORIENTED_EDGE('',*,*,#33757,.T.);
#44949=ORIENTED_EDGE('',*,*,#33765,.T.);
#44950=ORIENTED_EDGE('',*,*,#33762,.F.);
#44951=ORIENTED_EDGE('',*,*,#33765,.F.);
#44952=ORIENTED_EDGE('',*,*,#33756,.F.);
#44953=ORIENTED_EDGE('',*,*,#33760,.F.);
#44954=ORIENTED_EDGE('',*,*,#33763,.F.);
#44955=ORIENTED_EDGE('',*,*,#33766,.F.);
#44956=ORIENTED_EDGE('',*,*,#33767,.T.);
#44957=ORIENTED_EDGE('',*,*,#33768,.T.);
#44958=ORIENTED_EDGE('',*,*,#33769,.F.);
#44959=ORIENTED_EDGE('',*,*,#33770,.F.);
#44960=ORIENTED_EDGE('',*,*,#33771,.T.);
#44961=ORIENTED_EDGE('',*,*,#33772,.T.);
#44962=ORIENTED_EDGE('',*,*,#33767,.F.);
#44963=ORIENTED_EDGE('',*,*,#33773,.F.);
#44964=ORIENTED_EDGE('',*,*,#33774,.T.);
#44965=ORIENTED_EDGE('',*,*,#33775,.T.);
#44966=ORIENTED_EDGE('',*,*,#33771,.F.);
#44967=ORIENTED_EDGE('',*,*,#33776,.F.);
#44968=ORIENTED_EDGE('',*,*,#33769,.T.);
#44969=ORIENTED_EDGE('',*,*,#33777,.T.);
#44970=ORIENTED_EDGE('',*,*,#33774,.F.);
#44971=ORIENTED_EDGE('',*,*,#33777,.F.);
#44972=ORIENTED_EDGE('',*,*,#33768,.F.);
#44973=ORIENTED_EDGE('',*,*,#33772,.F.);
#44974=ORIENTED_EDGE('',*,*,#33775,.F.);
#44975=ORIENTED_EDGE('',*,*,#33778,.F.);
#44976=ORIENTED_EDGE('',*,*,#33779,.T.);
#44977=ORIENTED_EDGE('',*,*,#33780,.T.);
#44978=ORIENTED_EDGE('',*,*,#33781,.F.);
#44979=ORIENTED_EDGE('',*,*,#33782,.F.);
#44980=ORIENTED_EDGE('',*,*,#33783,.T.);
#44981=ORIENTED_EDGE('',*,*,#33784,.T.);
#44982=ORIENTED_EDGE('',*,*,#33779,.F.);
#44983=ORIENTED_EDGE('',*,*,#33785,.F.);
#44984=ORIENTED_EDGE('',*,*,#33786,.T.);
#44985=ORIENTED_EDGE('',*,*,#33787,.T.);
#44986=ORIENTED_EDGE('',*,*,#33783,.F.);
#44987=ORIENTED_EDGE('',*,*,#33788,.F.);
#44988=ORIENTED_EDGE('',*,*,#33781,.T.);
#44989=ORIENTED_EDGE('',*,*,#33789,.T.);
#44990=ORIENTED_EDGE('',*,*,#33786,.F.);
#44991=ORIENTED_EDGE('',*,*,#33789,.F.);
#44992=ORIENTED_EDGE('',*,*,#33780,.F.);
#44993=ORIENTED_EDGE('',*,*,#33784,.F.);
#44994=ORIENTED_EDGE('',*,*,#33787,.F.);
#44995=ORIENTED_EDGE('',*,*,#33790,.F.);
#44996=ORIENTED_EDGE('',*,*,#33791,.T.);
#44997=ORIENTED_EDGE('',*,*,#33792,.T.);
#44998=ORIENTED_EDGE('',*,*,#33793,.F.);
#44999=ORIENTED_EDGE('',*,*,#33794,.F.);
#45000=ORIENTED_EDGE('',*,*,#33795,.T.);
#45001=ORIENTED_EDGE('',*,*,#33796,.T.);
#45002=ORIENTED_EDGE('',*,*,#33791,.F.);
#45003=ORIENTED_EDGE('',*,*,#33797,.F.);
#45004=ORIENTED_EDGE('',*,*,#33798,.T.);
#45005=ORIENTED_EDGE('',*,*,#33799,.T.);
#45006=ORIENTED_EDGE('',*,*,#33795,.F.);
#45007=ORIENTED_EDGE('',*,*,#33800,.F.);
#45008=ORIENTED_EDGE('',*,*,#33793,.T.);
#45009=ORIENTED_EDGE('',*,*,#33801,.T.);
#45010=ORIENTED_EDGE('',*,*,#33798,.F.);
#45011=ORIENTED_EDGE('',*,*,#33801,.F.);
#45012=ORIENTED_EDGE('',*,*,#33792,.F.);
#45013=ORIENTED_EDGE('',*,*,#33796,.F.);
#45014=ORIENTED_EDGE('',*,*,#33799,.F.);
#45015=ORIENTED_EDGE('',*,*,#33802,.F.);
#45016=ORIENTED_EDGE('',*,*,#33803,.T.);
#45017=ORIENTED_EDGE('',*,*,#33804,.T.);
#45018=ORIENTED_EDGE('',*,*,#33805,.F.);
#45019=ORIENTED_EDGE('',*,*,#33806,.F.);
#45020=ORIENTED_EDGE('',*,*,#33807,.T.);
#45021=ORIENTED_EDGE('',*,*,#33808,.T.);
#45022=ORIENTED_EDGE('',*,*,#33803,.F.);
#45023=ORIENTED_EDGE('',*,*,#33809,.F.);
#45024=ORIENTED_EDGE('',*,*,#33810,.T.);
#45025=ORIENTED_EDGE('',*,*,#33811,.T.);
#45026=ORIENTED_EDGE('',*,*,#33807,.F.);
#45027=ORIENTED_EDGE('',*,*,#33812,.F.);
#45028=ORIENTED_EDGE('',*,*,#33805,.T.);
#45029=ORIENTED_EDGE('',*,*,#33813,.T.);
#45030=ORIENTED_EDGE('',*,*,#33810,.F.);
#45031=ORIENTED_EDGE('',*,*,#33813,.F.);
#45032=ORIENTED_EDGE('',*,*,#33804,.F.);
#45033=ORIENTED_EDGE('',*,*,#33808,.F.);
#45034=ORIENTED_EDGE('',*,*,#33811,.F.);
#45035=ORIENTED_EDGE('',*,*,#33814,.F.);
#45036=ORIENTED_EDGE('',*,*,#33815,.T.);
#45037=ORIENTED_EDGE('',*,*,#33816,.T.);
#45038=ORIENTED_EDGE('',*,*,#33817,.F.);
#45039=ORIENTED_EDGE('',*,*,#33818,.F.);
#45040=ORIENTED_EDGE('',*,*,#33819,.T.);
#45041=ORIENTED_EDGE('',*,*,#33820,.T.);
#45042=ORIENTED_EDGE('',*,*,#33815,.F.);
#45043=ORIENTED_EDGE('',*,*,#33821,.F.);
#45044=ORIENTED_EDGE('',*,*,#33822,.T.);
#45045=ORIENTED_EDGE('',*,*,#33823,.T.);
#45046=ORIENTED_EDGE('',*,*,#33819,.F.);
#45047=ORIENTED_EDGE('',*,*,#33824,.F.);
#45048=ORIENTED_EDGE('',*,*,#33817,.T.);
#45049=ORIENTED_EDGE('',*,*,#33825,.T.);
#45050=ORIENTED_EDGE('',*,*,#33822,.F.);
#45051=ORIENTED_EDGE('',*,*,#33825,.F.);
#45052=ORIENTED_EDGE('',*,*,#33816,.F.);
#45053=ORIENTED_EDGE('',*,*,#33820,.F.);
#45054=ORIENTED_EDGE('',*,*,#33823,.F.);
#45055=ORIENTED_EDGE('',*,*,#33826,.F.);
#45056=ORIENTED_EDGE('',*,*,#33827,.T.);
#45057=ORIENTED_EDGE('',*,*,#33828,.T.);
#45058=ORIENTED_EDGE('',*,*,#33829,.F.);
#45059=ORIENTED_EDGE('',*,*,#33830,.F.);
#45060=ORIENTED_EDGE('',*,*,#33831,.T.);
#45061=ORIENTED_EDGE('',*,*,#33832,.T.);
#45062=ORIENTED_EDGE('',*,*,#33827,.F.);
#45063=ORIENTED_EDGE('',*,*,#33833,.F.);
#45064=ORIENTED_EDGE('',*,*,#33834,.T.);
#45065=ORIENTED_EDGE('',*,*,#33835,.T.);
#45066=ORIENTED_EDGE('',*,*,#33831,.F.);
#45067=ORIENTED_EDGE('',*,*,#33836,.F.);
#45068=ORIENTED_EDGE('',*,*,#33829,.T.);
#45069=ORIENTED_EDGE('',*,*,#33837,.T.);
#45070=ORIENTED_EDGE('',*,*,#33834,.F.);
#45071=ORIENTED_EDGE('',*,*,#33837,.F.);
#45072=ORIENTED_EDGE('',*,*,#33828,.F.);
#45073=ORIENTED_EDGE('',*,*,#33832,.F.);
#45074=ORIENTED_EDGE('',*,*,#33835,.F.);
#45075=ORIENTED_EDGE('',*,*,#33838,.F.);
#45076=ORIENTED_EDGE('',*,*,#33839,.T.);
#45077=ORIENTED_EDGE('',*,*,#33840,.T.);
#45078=ORIENTED_EDGE('',*,*,#33841,.F.);
#45079=ORIENTED_EDGE('',*,*,#33842,.F.);
#45080=ORIENTED_EDGE('',*,*,#33843,.T.);
#45081=ORIENTED_EDGE('',*,*,#33844,.T.);
#45082=ORIENTED_EDGE('',*,*,#33839,.F.);
#45083=ORIENTED_EDGE('',*,*,#33845,.F.);
#45084=ORIENTED_EDGE('',*,*,#33846,.T.);
#45085=ORIENTED_EDGE('',*,*,#33847,.T.);
#45086=ORIENTED_EDGE('',*,*,#33843,.F.);
#45087=ORIENTED_EDGE('',*,*,#33848,.F.);
#45088=ORIENTED_EDGE('',*,*,#33841,.T.);
#45089=ORIENTED_EDGE('',*,*,#33849,.T.);
#45090=ORIENTED_EDGE('',*,*,#33846,.F.);
#45091=ORIENTED_EDGE('',*,*,#33849,.F.);
#45092=ORIENTED_EDGE('',*,*,#33840,.F.);
#45093=ORIENTED_EDGE('',*,*,#33844,.F.);
#45094=ORIENTED_EDGE('',*,*,#33847,.F.);
#45095=ORIENTED_EDGE('',*,*,#33850,.F.);
#45096=ORIENTED_EDGE('',*,*,#33851,.T.);
#45097=ORIENTED_EDGE('',*,*,#33852,.T.);
#45098=ORIENTED_EDGE('',*,*,#33853,.F.);
#45099=ORIENTED_EDGE('',*,*,#33854,.F.);
#45100=ORIENTED_EDGE('',*,*,#33855,.T.);
#45101=ORIENTED_EDGE('',*,*,#33856,.T.);
#45102=ORIENTED_EDGE('',*,*,#33851,.F.);
#45103=ORIENTED_EDGE('',*,*,#33857,.F.);
#45104=ORIENTED_EDGE('',*,*,#33858,.T.);
#45105=ORIENTED_EDGE('',*,*,#33859,.T.);
#45106=ORIENTED_EDGE('',*,*,#33855,.F.);
#45107=ORIENTED_EDGE('',*,*,#33860,.F.);
#45108=ORIENTED_EDGE('',*,*,#33853,.T.);
#45109=ORIENTED_EDGE('',*,*,#33861,.T.);
#45110=ORIENTED_EDGE('',*,*,#33858,.F.);
#45111=ORIENTED_EDGE('',*,*,#33861,.F.);
#45112=ORIENTED_EDGE('',*,*,#33852,.F.);
#45113=ORIENTED_EDGE('',*,*,#33856,.F.);
#45114=ORIENTED_EDGE('',*,*,#33859,.F.);
#45115=ORIENTED_EDGE('',*,*,#33862,.F.);
#45116=ORIENTED_EDGE('',*,*,#33863,.T.);
#45117=ORIENTED_EDGE('',*,*,#33864,.T.);
#45118=ORIENTED_EDGE('',*,*,#33865,.F.);
#45119=ORIENTED_EDGE('',*,*,#33866,.F.);
#45120=ORIENTED_EDGE('',*,*,#33867,.T.);
#45121=ORIENTED_EDGE('',*,*,#33868,.T.);
#45122=ORIENTED_EDGE('',*,*,#33863,.F.);
#45123=ORIENTED_EDGE('',*,*,#33869,.F.);
#45124=ORIENTED_EDGE('',*,*,#33870,.T.);
#45125=ORIENTED_EDGE('',*,*,#33871,.T.);
#45126=ORIENTED_EDGE('',*,*,#33867,.F.);
#45127=ORIENTED_EDGE('',*,*,#33872,.F.);
#45128=ORIENTED_EDGE('',*,*,#33865,.T.);
#45129=ORIENTED_EDGE('',*,*,#33873,.T.);
#45130=ORIENTED_EDGE('',*,*,#33870,.F.);
#45131=ORIENTED_EDGE('',*,*,#33873,.F.);
#45132=ORIENTED_EDGE('',*,*,#33864,.F.);
#45133=ORIENTED_EDGE('',*,*,#33868,.F.);
#45134=ORIENTED_EDGE('',*,*,#33871,.F.);
#45135=ORIENTED_EDGE('',*,*,#33874,.F.);
#45136=ORIENTED_EDGE('',*,*,#33875,.T.);
#45137=ORIENTED_EDGE('',*,*,#33876,.T.);
#45138=ORIENTED_EDGE('',*,*,#33877,.F.);
#45139=ORIENTED_EDGE('',*,*,#33878,.F.);
#45140=ORIENTED_EDGE('',*,*,#33879,.T.);
#45141=ORIENTED_EDGE('',*,*,#33880,.T.);
#45142=ORIENTED_EDGE('',*,*,#33875,.F.);
#45143=ORIENTED_EDGE('',*,*,#33881,.F.);
#45144=ORIENTED_EDGE('',*,*,#33882,.T.);
#45145=ORIENTED_EDGE('',*,*,#33883,.T.);
#45146=ORIENTED_EDGE('',*,*,#33879,.F.);
#45147=ORIENTED_EDGE('',*,*,#33884,.F.);
#45148=ORIENTED_EDGE('',*,*,#33877,.T.);
#45149=ORIENTED_EDGE('',*,*,#33885,.T.);
#45150=ORIENTED_EDGE('',*,*,#33882,.F.);
#45151=ORIENTED_EDGE('',*,*,#33885,.F.);
#45152=ORIENTED_EDGE('',*,*,#33876,.F.);
#45153=ORIENTED_EDGE('',*,*,#33880,.F.);
#45154=ORIENTED_EDGE('',*,*,#33883,.F.);
#45155=ORIENTED_EDGE('',*,*,#33886,.F.);
#45156=ORIENTED_EDGE('',*,*,#33887,.T.);
#45157=ORIENTED_EDGE('',*,*,#33888,.T.);
#45158=ORIENTED_EDGE('',*,*,#33889,.F.);
#45159=ORIENTED_EDGE('',*,*,#33890,.F.);
#45160=ORIENTED_EDGE('',*,*,#33891,.T.);
#45161=ORIENTED_EDGE('',*,*,#33892,.T.);
#45162=ORIENTED_EDGE('',*,*,#33887,.F.);
#45163=ORIENTED_EDGE('',*,*,#33893,.F.);
#45164=ORIENTED_EDGE('',*,*,#33894,.T.);
#45165=ORIENTED_EDGE('',*,*,#33895,.T.);
#45166=ORIENTED_EDGE('',*,*,#33891,.F.);
#45167=ORIENTED_EDGE('',*,*,#33896,.F.);
#45168=ORIENTED_EDGE('',*,*,#33889,.T.);
#45169=ORIENTED_EDGE('',*,*,#33897,.T.);
#45170=ORIENTED_EDGE('',*,*,#33894,.F.);
#45171=ORIENTED_EDGE('',*,*,#33897,.F.);
#45172=ORIENTED_EDGE('',*,*,#33888,.F.);
#45173=ORIENTED_EDGE('',*,*,#33892,.F.);
#45174=ORIENTED_EDGE('',*,*,#33895,.F.);
#45175=ORIENTED_EDGE('',*,*,#33898,.F.);
#45176=ORIENTED_EDGE('',*,*,#33899,.T.);
#45177=ORIENTED_EDGE('',*,*,#33900,.T.);
#45178=ORIENTED_EDGE('',*,*,#33901,.F.);
#45179=ORIENTED_EDGE('',*,*,#33902,.F.);
#45180=ORIENTED_EDGE('',*,*,#33903,.T.);
#45181=ORIENTED_EDGE('',*,*,#33904,.T.);
#45182=ORIENTED_EDGE('',*,*,#33899,.F.);
#45183=ORIENTED_EDGE('',*,*,#33905,.F.);
#45184=ORIENTED_EDGE('',*,*,#33906,.T.);
#45185=ORIENTED_EDGE('',*,*,#33907,.T.);
#45186=ORIENTED_EDGE('',*,*,#33903,.F.);
#45187=ORIENTED_EDGE('',*,*,#33908,.F.);
#45188=ORIENTED_EDGE('',*,*,#33901,.T.);
#45189=ORIENTED_EDGE('',*,*,#33909,.T.);
#45190=ORIENTED_EDGE('',*,*,#33906,.F.);
#45191=ORIENTED_EDGE('',*,*,#33909,.F.);
#45192=ORIENTED_EDGE('',*,*,#33900,.F.);
#45193=ORIENTED_EDGE('',*,*,#33904,.F.);
#45194=ORIENTED_EDGE('',*,*,#33907,.F.);
#45195=ORIENTED_EDGE('',*,*,#33910,.F.);
#45196=ORIENTED_EDGE('',*,*,#33911,.T.);
#45197=ORIENTED_EDGE('',*,*,#33912,.T.);
#45198=ORIENTED_EDGE('',*,*,#33913,.F.);
#45199=ORIENTED_EDGE('',*,*,#33914,.F.);
#45200=ORIENTED_EDGE('',*,*,#33915,.T.);
#45201=ORIENTED_EDGE('',*,*,#33916,.T.);
#45202=ORIENTED_EDGE('',*,*,#33911,.F.);
#45203=ORIENTED_EDGE('',*,*,#33917,.F.);
#45204=ORIENTED_EDGE('',*,*,#33918,.T.);
#45205=ORIENTED_EDGE('',*,*,#33919,.T.);
#45206=ORIENTED_EDGE('',*,*,#33915,.F.);
#45207=ORIENTED_EDGE('',*,*,#33920,.F.);
#45208=ORIENTED_EDGE('',*,*,#33913,.T.);
#45209=ORIENTED_EDGE('',*,*,#33921,.T.);
#45210=ORIENTED_EDGE('',*,*,#33918,.F.);
#45211=ORIENTED_EDGE('',*,*,#33921,.F.);
#45212=ORIENTED_EDGE('',*,*,#33912,.F.);
#45213=ORIENTED_EDGE('',*,*,#33916,.F.);
#45214=ORIENTED_EDGE('',*,*,#33919,.F.);
#45215=ORIENTED_EDGE('',*,*,#33922,.F.);
#45216=ORIENTED_EDGE('',*,*,#33923,.T.);
#45217=ORIENTED_EDGE('',*,*,#33924,.T.);
#45218=ORIENTED_EDGE('',*,*,#33925,.F.);
#45219=ORIENTED_EDGE('',*,*,#33926,.F.);
#45220=ORIENTED_EDGE('',*,*,#33927,.T.);
#45221=ORIENTED_EDGE('',*,*,#33928,.T.);
#45222=ORIENTED_EDGE('',*,*,#33923,.F.);
#45223=ORIENTED_EDGE('',*,*,#33929,.F.);
#45224=ORIENTED_EDGE('',*,*,#33930,.T.);
#45225=ORIENTED_EDGE('',*,*,#33931,.T.);
#45226=ORIENTED_EDGE('',*,*,#33927,.F.);
#45227=ORIENTED_EDGE('',*,*,#33932,.F.);
#45228=ORIENTED_EDGE('',*,*,#33925,.T.);
#45229=ORIENTED_EDGE('',*,*,#33933,.T.);
#45230=ORIENTED_EDGE('',*,*,#33930,.F.);
#45231=ORIENTED_EDGE('',*,*,#33933,.F.);
#45232=ORIENTED_EDGE('',*,*,#33924,.F.);
#45233=ORIENTED_EDGE('',*,*,#33928,.F.);
#45234=ORIENTED_EDGE('',*,*,#33931,.F.);
#45235=ORIENTED_EDGE('',*,*,#33934,.F.);
#45236=ORIENTED_EDGE('',*,*,#33935,.T.);
#45237=ORIENTED_EDGE('',*,*,#33936,.T.);
#45238=ORIENTED_EDGE('',*,*,#33937,.F.);
#45239=ORIENTED_EDGE('',*,*,#33938,.F.);
#45240=ORIENTED_EDGE('',*,*,#33939,.T.);
#45241=ORIENTED_EDGE('',*,*,#33940,.T.);
#45242=ORIENTED_EDGE('',*,*,#33935,.F.);
#45243=ORIENTED_EDGE('',*,*,#33941,.F.);
#45244=ORIENTED_EDGE('',*,*,#33942,.T.);
#45245=ORIENTED_EDGE('',*,*,#33943,.T.);
#45246=ORIENTED_EDGE('',*,*,#33939,.F.);
#45247=ORIENTED_EDGE('',*,*,#33944,.F.);
#45248=ORIENTED_EDGE('',*,*,#33937,.T.);
#45249=ORIENTED_EDGE('',*,*,#33945,.T.);
#45250=ORIENTED_EDGE('',*,*,#33942,.F.);
#45251=ORIENTED_EDGE('',*,*,#33945,.F.);
#45252=ORIENTED_EDGE('',*,*,#33936,.F.);
#45253=ORIENTED_EDGE('',*,*,#33940,.F.);
#45254=ORIENTED_EDGE('',*,*,#33943,.F.);
#45255=ORIENTED_EDGE('',*,*,#33946,.F.);
#45256=ORIENTED_EDGE('',*,*,#33947,.T.);
#45257=ORIENTED_EDGE('',*,*,#33948,.T.);
#45258=ORIENTED_EDGE('',*,*,#33949,.F.);
#45259=ORIENTED_EDGE('',*,*,#33950,.F.);
#45260=ORIENTED_EDGE('',*,*,#33951,.T.);
#45261=ORIENTED_EDGE('',*,*,#33952,.T.);
#45262=ORIENTED_EDGE('',*,*,#33947,.F.);
#45263=ORIENTED_EDGE('',*,*,#33953,.F.);
#45264=ORIENTED_EDGE('',*,*,#33954,.T.);
#45265=ORIENTED_EDGE('',*,*,#33955,.T.);
#45266=ORIENTED_EDGE('',*,*,#33951,.F.);
#45267=ORIENTED_EDGE('',*,*,#33956,.F.);
#45268=ORIENTED_EDGE('',*,*,#33949,.T.);
#45269=ORIENTED_EDGE('',*,*,#33957,.T.);
#45270=ORIENTED_EDGE('',*,*,#33954,.F.);
#45271=ORIENTED_EDGE('',*,*,#33957,.F.);
#45272=ORIENTED_EDGE('',*,*,#33948,.F.);
#45273=ORIENTED_EDGE('',*,*,#33952,.F.);
#45274=ORIENTED_EDGE('',*,*,#33955,.F.);
#45275=ORIENTED_EDGE('',*,*,#33958,.F.);
#45276=ORIENTED_EDGE('',*,*,#33959,.T.);
#45277=ORIENTED_EDGE('',*,*,#33960,.T.);
#45278=ORIENTED_EDGE('',*,*,#33961,.F.);
#45279=ORIENTED_EDGE('',*,*,#33962,.F.);
#45280=ORIENTED_EDGE('',*,*,#33963,.T.);
#45281=ORIENTED_EDGE('',*,*,#33964,.T.);
#45282=ORIENTED_EDGE('',*,*,#33959,.F.);
#45283=ORIENTED_EDGE('',*,*,#33965,.F.);
#45284=ORIENTED_EDGE('',*,*,#33966,.T.);
#45285=ORIENTED_EDGE('',*,*,#33967,.T.);
#45286=ORIENTED_EDGE('',*,*,#33963,.F.);
#45287=ORIENTED_EDGE('',*,*,#33968,.F.);
#45288=ORIENTED_EDGE('',*,*,#33961,.T.);
#45289=ORIENTED_EDGE('',*,*,#33969,.T.);
#45290=ORIENTED_EDGE('',*,*,#33966,.F.);
#45291=ORIENTED_EDGE('',*,*,#33969,.F.);
#45292=ORIENTED_EDGE('',*,*,#33960,.F.);
#45293=ORIENTED_EDGE('',*,*,#33964,.F.);
#45294=ORIENTED_EDGE('',*,*,#33967,.F.);
#45295=ORIENTED_EDGE('',*,*,#33970,.F.);
#45296=ORIENTED_EDGE('',*,*,#33971,.T.);
#45297=ORIENTED_EDGE('',*,*,#33972,.T.);
#45298=ORIENTED_EDGE('',*,*,#33973,.F.);
#45299=ORIENTED_EDGE('',*,*,#33974,.F.);
#45300=ORIENTED_EDGE('',*,*,#33975,.T.);
#45301=ORIENTED_EDGE('',*,*,#33976,.T.);
#45302=ORIENTED_EDGE('',*,*,#33971,.F.);
#45303=ORIENTED_EDGE('',*,*,#33977,.F.);
#45304=ORIENTED_EDGE('',*,*,#33978,.T.);
#45305=ORIENTED_EDGE('',*,*,#33979,.T.);
#45306=ORIENTED_EDGE('',*,*,#33975,.F.);
#45307=ORIENTED_EDGE('',*,*,#33980,.F.);
#45308=ORIENTED_EDGE('',*,*,#33973,.T.);
#45309=ORIENTED_EDGE('',*,*,#33981,.T.);
#45310=ORIENTED_EDGE('',*,*,#33978,.F.);
#45311=ORIENTED_EDGE('',*,*,#33981,.F.);
#45312=ORIENTED_EDGE('',*,*,#33972,.F.);
#45313=ORIENTED_EDGE('',*,*,#33976,.F.);
#45314=ORIENTED_EDGE('',*,*,#33979,.F.);
#45315=ORIENTED_EDGE('',*,*,#33982,.F.);
#45316=ORIENTED_EDGE('',*,*,#33983,.T.);
#45317=ORIENTED_EDGE('',*,*,#33984,.T.);
#45318=ORIENTED_EDGE('',*,*,#33985,.F.);
#45319=ORIENTED_EDGE('',*,*,#33986,.F.);
#45320=ORIENTED_EDGE('',*,*,#33987,.T.);
#45321=ORIENTED_EDGE('',*,*,#33988,.T.);
#45322=ORIENTED_EDGE('',*,*,#33983,.F.);
#45323=ORIENTED_EDGE('',*,*,#33989,.F.);
#45324=ORIENTED_EDGE('',*,*,#33990,.T.);
#45325=ORIENTED_EDGE('',*,*,#33991,.T.);
#45326=ORIENTED_EDGE('',*,*,#33987,.F.);
#45327=ORIENTED_EDGE('',*,*,#33992,.F.);
#45328=ORIENTED_EDGE('',*,*,#33985,.T.);
#45329=ORIENTED_EDGE('',*,*,#33993,.T.);
#45330=ORIENTED_EDGE('',*,*,#33990,.F.);
#45331=ORIENTED_EDGE('',*,*,#33993,.F.);
#45332=ORIENTED_EDGE('',*,*,#33984,.F.);
#45333=ORIENTED_EDGE('',*,*,#33988,.F.);
#45334=ORIENTED_EDGE('',*,*,#33991,.F.);
#45335=ORIENTED_EDGE('',*,*,#33994,.F.);
#45336=ORIENTED_EDGE('',*,*,#33995,.T.);
#45337=ORIENTED_EDGE('',*,*,#33996,.T.);
#45338=ORIENTED_EDGE('',*,*,#33997,.F.);
#45339=ORIENTED_EDGE('',*,*,#33998,.F.);
#45340=ORIENTED_EDGE('',*,*,#33999,.T.);
#45341=ORIENTED_EDGE('',*,*,#34000,.T.);
#45342=ORIENTED_EDGE('',*,*,#33995,.F.);
#45343=ORIENTED_EDGE('',*,*,#34001,.F.);
#45344=ORIENTED_EDGE('',*,*,#34002,.T.);
#45345=ORIENTED_EDGE('',*,*,#34003,.T.);
#45346=ORIENTED_EDGE('',*,*,#33999,.F.);
#45347=ORIENTED_EDGE('',*,*,#34004,.F.);
#45348=ORIENTED_EDGE('',*,*,#33997,.T.);
#45349=ORIENTED_EDGE('',*,*,#34005,.T.);
#45350=ORIENTED_EDGE('',*,*,#34002,.F.);
#45351=ORIENTED_EDGE('',*,*,#34005,.F.);
#45352=ORIENTED_EDGE('',*,*,#33996,.F.);
#45353=ORIENTED_EDGE('',*,*,#34000,.F.);
#45354=ORIENTED_EDGE('',*,*,#34003,.F.);
#45355=ORIENTED_EDGE('',*,*,#34006,.F.);
#45356=ORIENTED_EDGE('',*,*,#34007,.T.);
#45357=ORIENTED_EDGE('',*,*,#34008,.T.);
#45358=ORIENTED_EDGE('',*,*,#34009,.F.);
#45359=ORIENTED_EDGE('',*,*,#34010,.F.);
#45360=ORIENTED_EDGE('',*,*,#34011,.T.);
#45361=ORIENTED_EDGE('',*,*,#34012,.T.);
#45362=ORIENTED_EDGE('',*,*,#34007,.F.);
#45363=ORIENTED_EDGE('',*,*,#34013,.F.);
#45364=ORIENTED_EDGE('',*,*,#34014,.T.);
#45365=ORIENTED_EDGE('',*,*,#34015,.T.);
#45366=ORIENTED_EDGE('',*,*,#34011,.F.);
#45367=ORIENTED_EDGE('',*,*,#34016,.F.);
#45368=ORIENTED_EDGE('',*,*,#34009,.T.);
#45369=ORIENTED_EDGE('',*,*,#34017,.T.);
#45370=ORIENTED_EDGE('',*,*,#34014,.F.);
#45371=ORIENTED_EDGE('',*,*,#34017,.F.);
#45372=ORIENTED_EDGE('',*,*,#34008,.F.);
#45373=ORIENTED_EDGE('',*,*,#34012,.F.);
#45374=ORIENTED_EDGE('',*,*,#34015,.F.);
#45375=ORIENTED_EDGE('',*,*,#34018,.F.);
#45376=ORIENTED_EDGE('',*,*,#34019,.T.);
#45377=ORIENTED_EDGE('',*,*,#34020,.T.);
#45378=ORIENTED_EDGE('',*,*,#34021,.F.);
#45379=ORIENTED_EDGE('',*,*,#34022,.F.);
#45380=ORIENTED_EDGE('',*,*,#34023,.T.);
#45381=ORIENTED_EDGE('',*,*,#34024,.T.);
#45382=ORIENTED_EDGE('',*,*,#34019,.F.);
#45383=ORIENTED_EDGE('',*,*,#34025,.F.);
#45384=ORIENTED_EDGE('',*,*,#34026,.T.);
#45385=ORIENTED_EDGE('',*,*,#34027,.T.);
#45386=ORIENTED_EDGE('',*,*,#34023,.F.);
#45387=ORIENTED_EDGE('',*,*,#34028,.F.);
#45388=ORIENTED_EDGE('',*,*,#34021,.T.);
#45389=ORIENTED_EDGE('',*,*,#34029,.T.);
#45390=ORIENTED_EDGE('',*,*,#34026,.F.);
#45391=ORIENTED_EDGE('',*,*,#34029,.F.);
#45392=ORIENTED_EDGE('',*,*,#34020,.F.);
#45393=ORIENTED_EDGE('',*,*,#34024,.F.);
#45394=ORIENTED_EDGE('',*,*,#34027,.F.);
#45395=ORIENTED_EDGE('',*,*,#34030,.F.);
#45396=ORIENTED_EDGE('',*,*,#34031,.T.);
#45397=ORIENTED_EDGE('',*,*,#34032,.T.);
#45398=ORIENTED_EDGE('',*,*,#34033,.F.);
#45399=ORIENTED_EDGE('',*,*,#34034,.F.);
#45400=ORIENTED_EDGE('',*,*,#34035,.T.);
#45401=ORIENTED_EDGE('',*,*,#34036,.T.);
#45402=ORIENTED_EDGE('',*,*,#34031,.F.);
#45403=ORIENTED_EDGE('',*,*,#34037,.F.);
#45404=ORIENTED_EDGE('',*,*,#34038,.T.);
#45405=ORIENTED_EDGE('',*,*,#34039,.T.);
#45406=ORIENTED_EDGE('',*,*,#34035,.F.);
#45407=ORIENTED_EDGE('',*,*,#34040,.F.);
#45408=ORIENTED_EDGE('',*,*,#34033,.T.);
#45409=ORIENTED_EDGE('',*,*,#34041,.T.);
#45410=ORIENTED_EDGE('',*,*,#34038,.F.);
#45411=ORIENTED_EDGE('',*,*,#34041,.F.);
#45412=ORIENTED_EDGE('',*,*,#34032,.F.);
#45413=ORIENTED_EDGE('',*,*,#34036,.F.);
#45414=ORIENTED_EDGE('',*,*,#34039,.F.);
#45415=ORIENTED_EDGE('',*,*,#34042,.F.);
#45416=ORIENTED_EDGE('',*,*,#34043,.T.);
#45417=ORIENTED_EDGE('',*,*,#34044,.T.);
#45418=ORIENTED_EDGE('',*,*,#34045,.F.);
#45419=ORIENTED_EDGE('',*,*,#34046,.F.);
#45420=ORIENTED_EDGE('',*,*,#34047,.T.);
#45421=ORIENTED_EDGE('',*,*,#34048,.T.);
#45422=ORIENTED_EDGE('',*,*,#34043,.F.);
#45423=ORIENTED_EDGE('',*,*,#34049,.F.);
#45424=ORIENTED_EDGE('',*,*,#34050,.T.);
#45425=ORIENTED_EDGE('',*,*,#34051,.T.);
#45426=ORIENTED_EDGE('',*,*,#34047,.F.);
#45427=ORIENTED_EDGE('',*,*,#34052,.F.);
#45428=ORIENTED_EDGE('',*,*,#34045,.T.);
#45429=ORIENTED_EDGE('',*,*,#34053,.T.);
#45430=ORIENTED_EDGE('',*,*,#34050,.F.);
#45431=ORIENTED_EDGE('',*,*,#34053,.F.);
#45432=ORIENTED_EDGE('',*,*,#34044,.F.);
#45433=ORIENTED_EDGE('',*,*,#34048,.F.);
#45434=ORIENTED_EDGE('',*,*,#34051,.F.);
#45435=ORIENTED_EDGE('',*,*,#34054,.F.);
#45436=ORIENTED_EDGE('',*,*,#34055,.T.);
#45437=ORIENTED_EDGE('',*,*,#34056,.T.);
#45438=ORIENTED_EDGE('',*,*,#34057,.F.);
#45439=ORIENTED_EDGE('',*,*,#34058,.F.);
#45440=ORIENTED_EDGE('',*,*,#34059,.T.);
#45441=ORIENTED_EDGE('',*,*,#34060,.T.);
#45442=ORIENTED_EDGE('',*,*,#34055,.F.);
#45443=ORIENTED_EDGE('',*,*,#34061,.F.);
#45444=ORIENTED_EDGE('',*,*,#34062,.T.);
#45445=ORIENTED_EDGE('',*,*,#34063,.T.);
#45446=ORIENTED_EDGE('',*,*,#34059,.F.);
#45447=ORIENTED_EDGE('',*,*,#34064,.F.);
#45448=ORIENTED_EDGE('',*,*,#34057,.T.);
#45449=ORIENTED_EDGE('',*,*,#34065,.T.);
#45450=ORIENTED_EDGE('',*,*,#34062,.F.);
#45451=ORIENTED_EDGE('',*,*,#34065,.F.);
#45452=ORIENTED_EDGE('',*,*,#34056,.F.);
#45453=ORIENTED_EDGE('',*,*,#34060,.F.);
#45454=ORIENTED_EDGE('',*,*,#34063,.F.);
#45455=ORIENTED_EDGE('',*,*,#34066,.F.);
#45456=ORIENTED_EDGE('',*,*,#34067,.T.);
#45457=ORIENTED_EDGE('',*,*,#34068,.T.);
#45458=ORIENTED_EDGE('',*,*,#34069,.F.);
#45459=ORIENTED_EDGE('',*,*,#34070,.F.);
#45460=ORIENTED_EDGE('',*,*,#34071,.T.);
#45461=ORIENTED_EDGE('',*,*,#34072,.T.);
#45462=ORIENTED_EDGE('',*,*,#34067,.F.);
#45463=ORIENTED_EDGE('',*,*,#34073,.F.);
#45464=ORIENTED_EDGE('',*,*,#34074,.T.);
#45465=ORIENTED_EDGE('',*,*,#34075,.T.);
#45466=ORIENTED_EDGE('',*,*,#34071,.F.);
#45467=ORIENTED_EDGE('',*,*,#34076,.F.);
#45468=ORIENTED_EDGE('',*,*,#34069,.T.);
#45469=ORIENTED_EDGE('',*,*,#34077,.T.);
#45470=ORIENTED_EDGE('',*,*,#34074,.F.);
#45471=ORIENTED_EDGE('',*,*,#34077,.F.);
#45472=ORIENTED_EDGE('',*,*,#34068,.F.);
#45473=ORIENTED_EDGE('',*,*,#34072,.F.);
#45474=ORIENTED_EDGE('',*,*,#34075,.F.);
#45475=ORIENTED_EDGE('',*,*,#34078,.F.);
#45476=ORIENTED_EDGE('',*,*,#34079,.T.);
#45477=ORIENTED_EDGE('',*,*,#34080,.T.);
#45478=ORIENTED_EDGE('',*,*,#34081,.F.);
#45479=ORIENTED_EDGE('',*,*,#34082,.F.);
#45480=ORIENTED_EDGE('',*,*,#34083,.T.);
#45481=ORIENTED_EDGE('',*,*,#34084,.T.);
#45482=ORIENTED_EDGE('',*,*,#34079,.F.);
#45483=ORIENTED_EDGE('',*,*,#34085,.F.);
#45484=ORIENTED_EDGE('',*,*,#34086,.T.);
#45485=ORIENTED_EDGE('',*,*,#34087,.T.);
#45486=ORIENTED_EDGE('',*,*,#34083,.F.);
#45487=ORIENTED_EDGE('',*,*,#34088,.F.);
#45488=ORIENTED_EDGE('',*,*,#34081,.T.);
#45489=ORIENTED_EDGE('',*,*,#34089,.T.);
#45490=ORIENTED_EDGE('',*,*,#34086,.F.);
#45491=ORIENTED_EDGE('',*,*,#34089,.F.);
#45492=ORIENTED_EDGE('',*,*,#34080,.F.);
#45493=ORIENTED_EDGE('',*,*,#34084,.F.);
#45494=ORIENTED_EDGE('',*,*,#34087,.F.);
#45495=ORIENTED_EDGE('',*,*,#34090,.F.);
#45496=ORIENTED_EDGE('',*,*,#34091,.T.);
#45497=ORIENTED_EDGE('',*,*,#34092,.T.);
#45498=ORIENTED_EDGE('',*,*,#34093,.F.);
#45499=ORIENTED_EDGE('',*,*,#34094,.F.);
#45500=ORIENTED_EDGE('',*,*,#34095,.T.);
#45501=ORIENTED_EDGE('',*,*,#34096,.T.);
#45502=ORIENTED_EDGE('',*,*,#34091,.F.);
#45503=ORIENTED_EDGE('',*,*,#34097,.F.);
#45504=ORIENTED_EDGE('',*,*,#34098,.T.);
#45505=ORIENTED_EDGE('',*,*,#34099,.T.);
#45506=ORIENTED_EDGE('',*,*,#34095,.F.);
#45507=ORIENTED_EDGE('',*,*,#34100,.F.);
#45508=ORIENTED_EDGE('',*,*,#34093,.T.);
#45509=ORIENTED_EDGE('',*,*,#34101,.T.);
#45510=ORIENTED_EDGE('',*,*,#34098,.F.);
#45511=ORIENTED_EDGE('',*,*,#34101,.F.);
#45512=ORIENTED_EDGE('',*,*,#34092,.F.);
#45513=ORIENTED_EDGE('',*,*,#34096,.F.);
#45514=ORIENTED_EDGE('',*,*,#34099,.F.);
#45515=ORIENTED_EDGE('',*,*,#34102,.F.);
#45516=ORIENTED_EDGE('',*,*,#34103,.T.);
#45517=ORIENTED_EDGE('',*,*,#34104,.T.);
#45518=ORIENTED_EDGE('',*,*,#34105,.F.);
#45519=ORIENTED_EDGE('',*,*,#34106,.F.);
#45520=ORIENTED_EDGE('',*,*,#34107,.T.);
#45521=ORIENTED_EDGE('',*,*,#34108,.T.);
#45522=ORIENTED_EDGE('',*,*,#34103,.F.);
#45523=ORIENTED_EDGE('',*,*,#34109,.F.);
#45524=ORIENTED_EDGE('',*,*,#34110,.T.);
#45525=ORIENTED_EDGE('',*,*,#34111,.T.);
#45526=ORIENTED_EDGE('',*,*,#34107,.F.);
#45527=ORIENTED_EDGE('',*,*,#34112,.F.);
#45528=ORIENTED_EDGE('',*,*,#34105,.T.);
#45529=ORIENTED_EDGE('',*,*,#34113,.T.);
#45530=ORIENTED_EDGE('',*,*,#34110,.F.);
#45531=ORIENTED_EDGE('',*,*,#34113,.F.);
#45532=ORIENTED_EDGE('',*,*,#34104,.F.);
#45533=ORIENTED_EDGE('',*,*,#34108,.F.);
#45534=ORIENTED_EDGE('',*,*,#34111,.F.);
#45535=ORIENTED_EDGE('',*,*,#34114,.F.);
#45536=ORIENTED_EDGE('',*,*,#34115,.T.);
#45537=ORIENTED_EDGE('',*,*,#34116,.T.);
#45538=ORIENTED_EDGE('',*,*,#34117,.F.);
#45539=ORIENTED_EDGE('',*,*,#34118,.F.);
#45540=ORIENTED_EDGE('',*,*,#34119,.T.);
#45541=ORIENTED_EDGE('',*,*,#34120,.T.);
#45542=ORIENTED_EDGE('',*,*,#34115,.F.);
#45543=ORIENTED_EDGE('',*,*,#34121,.F.);
#45544=ORIENTED_EDGE('',*,*,#34122,.T.);
#45545=ORIENTED_EDGE('',*,*,#34123,.T.);
#45546=ORIENTED_EDGE('',*,*,#34119,.F.);
#45547=ORIENTED_EDGE('',*,*,#34124,.F.);
#45548=ORIENTED_EDGE('',*,*,#34117,.T.);
#45549=ORIENTED_EDGE('',*,*,#34125,.T.);
#45550=ORIENTED_EDGE('',*,*,#34122,.F.);
#45551=ORIENTED_EDGE('',*,*,#34125,.F.);
#45552=ORIENTED_EDGE('',*,*,#34116,.F.);
#45553=ORIENTED_EDGE('',*,*,#34120,.F.);
#45554=ORIENTED_EDGE('',*,*,#34123,.F.);
#45555=ORIENTED_EDGE('',*,*,#34126,.F.);
#45556=ORIENTED_EDGE('',*,*,#34127,.T.);
#45557=ORIENTED_EDGE('',*,*,#34128,.T.);
#45558=ORIENTED_EDGE('',*,*,#34129,.F.);
#45559=ORIENTED_EDGE('',*,*,#34130,.F.);
#45560=ORIENTED_EDGE('',*,*,#34131,.T.);
#45561=ORIENTED_EDGE('',*,*,#34132,.T.);
#45562=ORIENTED_EDGE('',*,*,#34127,.F.);
#45563=ORIENTED_EDGE('',*,*,#34133,.F.);
#45564=ORIENTED_EDGE('',*,*,#34134,.T.);
#45565=ORIENTED_EDGE('',*,*,#34135,.T.);
#45566=ORIENTED_EDGE('',*,*,#34131,.F.);
#45567=ORIENTED_EDGE('',*,*,#34136,.F.);
#45568=ORIENTED_EDGE('',*,*,#34129,.T.);
#45569=ORIENTED_EDGE('',*,*,#34137,.T.);
#45570=ORIENTED_EDGE('',*,*,#34134,.F.);
#45571=ORIENTED_EDGE('',*,*,#34137,.F.);
#45572=ORIENTED_EDGE('',*,*,#34128,.F.);
#45573=ORIENTED_EDGE('',*,*,#34132,.F.);
#45574=ORIENTED_EDGE('',*,*,#34135,.F.);
#45575=ORIENTED_EDGE('',*,*,#34138,.F.);
#45576=ORIENTED_EDGE('',*,*,#34139,.T.);
#45577=ORIENTED_EDGE('',*,*,#34140,.T.);
#45578=ORIENTED_EDGE('',*,*,#34141,.F.);
#45579=ORIENTED_EDGE('',*,*,#34142,.F.);
#45580=ORIENTED_EDGE('',*,*,#34143,.T.);
#45581=ORIENTED_EDGE('',*,*,#34144,.T.);
#45582=ORIENTED_EDGE('',*,*,#34139,.F.);
#45583=ORIENTED_EDGE('',*,*,#34145,.F.);
#45584=ORIENTED_EDGE('',*,*,#34146,.T.);
#45585=ORIENTED_EDGE('',*,*,#34147,.T.);
#45586=ORIENTED_EDGE('',*,*,#34143,.F.);
#45587=ORIENTED_EDGE('',*,*,#34148,.F.);
#45588=ORIENTED_EDGE('',*,*,#34141,.T.);
#45589=ORIENTED_EDGE('',*,*,#34149,.T.);
#45590=ORIENTED_EDGE('',*,*,#34146,.F.);
#45591=ORIENTED_EDGE('',*,*,#34149,.F.);
#45592=ORIENTED_EDGE('',*,*,#34140,.F.);
#45593=ORIENTED_EDGE('',*,*,#34144,.F.);
#45594=ORIENTED_EDGE('',*,*,#34147,.F.);
#45595=ORIENTED_EDGE('',*,*,#34150,.F.);
#45596=ORIENTED_EDGE('',*,*,#34151,.T.);
#45597=ORIENTED_EDGE('',*,*,#34152,.T.);
#45598=ORIENTED_EDGE('',*,*,#34153,.F.);
#45599=ORIENTED_EDGE('',*,*,#34154,.F.);
#45600=ORIENTED_EDGE('',*,*,#34155,.T.);
#45601=ORIENTED_EDGE('',*,*,#34156,.T.);
#45602=ORIENTED_EDGE('',*,*,#34151,.F.);
#45603=ORIENTED_EDGE('',*,*,#34157,.F.);
#45604=ORIENTED_EDGE('',*,*,#34158,.T.);
#45605=ORIENTED_EDGE('',*,*,#34159,.T.);
#45606=ORIENTED_EDGE('',*,*,#34155,.F.);
#45607=ORIENTED_EDGE('',*,*,#34160,.F.);
#45608=ORIENTED_EDGE('',*,*,#34153,.T.);
#45609=ORIENTED_EDGE('',*,*,#34161,.T.);
#45610=ORIENTED_EDGE('',*,*,#34158,.F.);
#45611=ORIENTED_EDGE('',*,*,#34161,.F.);
#45612=ORIENTED_EDGE('',*,*,#34152,.F.);
#45613=ORIENTED_EDGE('',*,*,#34156,.F.);
#45614=ORIENTED_EDGE('',*,*,#34159,.F.);
#45615=ORIENTED_EDGE('',*,*,#34162,.F.);
#45616=ORIENTED_EDGE('',*,*,#34163,.T.);
#45617=ORIENTED_EDGE('',*,*,#34164,.T.);
#45618=ORIENTED_EDGE('',*,*,#34165,.F.);
#45619=ORIENTED_EDGE('',*,*,#34166,.F.);
#45620=ORIENTED_EDGE('',*,*,#34167,.T.);
#45621=ORIENTED_EDGE('',*,*,#34168,.T.);
#45622=ORIENTED_EDGE('',*,*,#34163,.F.);
#45623=ORIENTED_EDGE('',*,*,#34169,.F.);
#45624=ORIENTED_EDGE('',*,*,#34170,.T.);
#45625=ORIENTED_EDGE('',*,*,#34171,.T.);
#45626=ORIENTED_EDGE('',*,*,#34167,.F.);
#45627=ORIENTED_EDGE('',*,*,#34172,.F.);
#45628=ORIENTED_EDGE('',*,*,#34165,.T.);
#45629=ORIENTED_EDGE('',*,*,#34173,.T.);
#45630=ORIENTED_EDGE('',*,*,#34170,.F.);
#45631=ORIENTED_EDGE('',*,*,#34173,.F.);
#45632=ORIENTED_EDGE('',*,*,#34164,.F.);
#45633=ORIENTED_EDGE('',*,*,#34168,.F.);
#45634=ORIENTED_EDGE('',*,*,#34171,.F.);
#45635=ORIENTED_EDGE('',*,*,#34174,.F.);
#45636=ORIENTED_EDGE('',*,*,#34175,.T.);
#45637=ORIENTED_EDGE('',*,*,#34176,.T.);
#45638=ORIENTED_EDGE('',*,*,#34177,.F.);
#45639=ORIENTED_EDGE('',*,*,#34178,.F.);
#45640=ORIENTED_EDGE('',*,*,#34179,.T.);
#45641=ORIENTED_EDGE('',*,*,#34180,.T.);
#45642=ORIENTED_EDGE('',*,*,#34175,.F.);
#45643=ORIENTED_EDGE('',*,*,#34181,.F.);
#45644=ORIENTED_EDGE('',*,*,#34182,.T.);
#45645=ORIENTED_EDGE('',*,*,#34183,.T.);
#45646=ORIENTED_EDGE('',*,*,#34179,.F.);
#45647=ORIENTED_EDGE('',*,*,#34184,.F.);
#45648=ORIENTED_EDGE('',*,*,#34177,.T.);
#45649=ORIENTED_EDGE('',*,*,#34185,.T.);
#45650=ORIENTED_EDGE('',*,*,#34182,.F.);
#45651=ORIENTED_EDGE('',*,*,#34185,.F.);
#45652=ORIENTED_EDGE('',*,*,#34176,.F.);
#45653=ORIENTED_EDGE('',*,*,#34180,.F.);
#45654=ORIENTED_EDGE('',*,*,#34183,.F.);
#45655=ORIENTED_EDGE('',*,*,#34186,.F.);
#45656=ORIENTED_EDGE('',*,*,#34187,.T.);
#45657=ORIENTED_EDGE('',*,*,#34188,.T.);
#45658=ORIENTED_EDGE('',*,*,#34189,.F.);
#45659=ORIENTED_EDGE('',*,*,#34190,.F.);
#45660=ORIENTED_EDGE('',*,*,#34191,.T.);
#45661=ORIENTED_EDGE('',*,*,#34192,.T.);
#45662=ORIENTED_EDGE('',*,*,#34187,.F.);
#45663=ORIENTED_EDGE('',*,*,#34193,.F.);
#45664=ORIENTED_EDGE('',*,*,#34194,.T.);
#45665=ORIENTED_EDGE('',*,*,#34195,.T.);
#45666=ORIENTED_EDGE('',*,*,#34191,.F.);
#45667=ORIENTED_EDGE('',*,*,#34196,.F.);
#45668=ORIENTED_EDGE('',*,*,#34189,.T.);
#45669=ORIENTED_EDGE('',*,*,#34197,.T.);
#45670=ORIENTED_EDGE('',*,*,#34194,.F.);
#45671=ORIENTED_EDGE('',*,*,#34197,.F.);
#45672=ORIENTED_EDGE('',*,*,#34188,.F.);
#45673=ORIENTED_EDGE('',*,*,#34192,.F.);
#45674=ORIENTED_EDGE('',*,*,#34195,.F.);
#45675=ORIENTED_EDGE('',*,*,#34198,.F.);
#45676=ORIENTED_EDGE('',*,*,#34199,.T.);
#45677=ORIENTED_EDGE('',*,*,#34200,.T.);
#45678=ORIENTED_EDGE('',*,*,#34201,.F.);
#45679=ORIENTED_EDGE('',*,*,#34202,.F.);
#45680=ORIENTED_EDGE('',*,*,#34203,.T.);
#45681=ORIENTED_EDGE('',*,*,#34204,.T.);
#45682=ORIENTED_EDGE('',*,*,#34199,.F.);
#45683=ORIENTED_EDGE('',*,*,#34205,.F.);
#45684=ORIENTED_EDGE('',*,*,#34206,.T.);
#45685=ORIENTED_EDGE('',*,*,#34207,.T.);
#45686=ORIENTED_EDGE('',*,*,#34203,.F.);
#45687=ORIENTED_EDGE('',*,*,#34208,.F.);
#45688=ORIENTED_EDGE('',*,*,#34201,.T.);
#45689=ORIENTED_EDGE('',*,*,#34209,.T.);
#45690=ORIENTED_EDGE('',*,*,#34206,.F.);
#45691=ORIENTED_EDGE('',*,*,#34209,.F.);
#45692=ORIENTED_EDGE('',*,*,#34200,.F.);
#45693=ORIENTED_EDGE('',*,*,#34204,.F.);
#45694=ORIENTED_EDGE('',*,*,#34207,.F.);
#45695=ORIENTED_EDGE('',*,*,#34210,.F.);
#45696=ORIENTED_EDGE('',*,*,#34211,.T.);
#45697=ORIENTED_EDGE('',*,*,#34212,.T.);
#45698=ORIENTED_EDGE('',*,*,#34213,.F.);
#45699=ORIENTED_EDGE('',*,*,#34214,.F.);
#45700=ORIENTED_EDGE('',*,*,#34215,.T.);
#45701=ORIENTED_EDGE('',*,*,#34216,.T.);
#45702=ORIENTED_EDGE('',*,*,#34211,.F.);
#45703=ORIENTED_EDGE('',*,*,#34217,.F.);
#45704=ORIENTED_EDGE('',*,*,#34218,.T.);
#45705=ORIENTED_EDGE('',*,*,#34219,.T.);
#45706=ORIENTED_EDGE('',*,*,#34215,.F.);
#45707=ORIENTED_EDGE('',*,*,#34220,.F.);
#45708=ORIENTED_EDGE('',*,*,#34213,.T.);
#45709=ORIENTED_EDGE('',*,*,#34221,.T.);
#45710=ORIENTED_EDGE('',*,*,#34218,.F.);
#45711=ORIENTED_EDGE('',*,*,#34221,.F.);
#45712=ORIENTED_EDGE('',*,*,#34212,.F.);
#45713=ORIENTED_EDGE('',*,*,#34216,.F.);
#45714=ORIENTED_EDGE('',*,*,#34219,.F.);
#45715=ORIENTED_EDGE('',*,*,#34222,.F.);
#45716=ORIENTED_EDGE('',*,*,#34223,.T.);
#45717=ORIENTED_EDGE('',*,*,#34224,.T.);
#45718=ORIENTED_EDGE('',*,*,#34225,.F.);
#45719=ORIENTED_EDGE('',*,*,#34226,.F.);
#45720=ORIENTED_EDGE('',*,*,#34227,.T.);
#45721=ORIENTED_EDGE('',*,*,#34228,.T.);
#45722=ORIENTED_EDGE('',*,*,#34223,.F.);
#45723=ORIENTED_EDGE('',*,*,#34229,.F.);
#45724=ORIENTED_EDGE('',*,*,#34230,.T.);
#45725=ORIENTED_EDGE('',*,*,#34231,.T.);
#45726=ORIENTED_EDGE('',*,*,#34227,.F.);
#45727=ORIENTED_EDGE('',*,*,#34232,.F.);
#45728=ORIENTED_EDGE('',*,*,#34225,.T.);
#45729=ORIENTED_EDGE('',*,*,#34233,.T.);
#45730=ORIENTED_EDGE('',*,*,#34230,.F.);
#45731=ORIENTED_EDGE('',*,*,#34233,.F.);
#45732=ORIENTED_EDGE('',*,*,#34224,.F.);
#45733=ORIENTED_EDGE('',*,*,#34228,.F.);
#45734=ORIENTED_EDGE('',*,*,#34231,.F.);
#45735=ORIENTED_EDGE('',*,*,#34234,.F.);
#45736=ORIENTED_EDGE('',*,*,#34235,.T.);
#45737=ORIENTED_EDGE('',*,*,#34236,.T.);
#45738=ORIENTED_EDGE('',*,*,#34237,.F.);
#45739=ORIENTED_EDGE('',*,*,#34238,.F.);
#45740=ORIENTED_EDGE('',*,*,#34239,.T.);
#45741=ORIENTED_EDGE('',*,*,#34240,.T.);
#45742=ORIENTED_EDGE('',*,*,#34235,.F.);
#45743=ORIENTED_EDGE('',*,*,#34241,.F.);
#45744=ORIENTED_EDGE('',*,*,#34242,.T.);
#45745=ORIENTED_EDGE('',*,*,#34243,.T.);
#45746=ORIENTED_EDGE('',*,*,#34239,.F.);
#45747=ORIENTED_EDGE('',*,*,#34244,.F.);
#45748=ORIENTED_EDGE('',*,*,#34237,.T.);
#45749=ORIENTED_EDGE('',*,*,#34245,.T.);
#45750=ORIENTED_EDGE('',*,*,#34242,.F.);
#45751=ORIENTED_EDGE('',*,*,#34245,.F.);
#45752=ORIENTED_EDGE('',*,*,#34236,.F.);
#45753=ORIENTED_EDGE('',*,*,#34240,.F.);
#45754=ORIENTED_EDGE('',*,*,#34243,.F.);
#45755=ORIENTED_EDGE('',*,*,#34246,.F.);
#45756=ORIENTED_EDGE('',*,*,#34247,.T.);
#45757=ORIENTED_EDGE('',*,*,#34248,.T.);
#45758=ORIENTED_EDGE('',*,*,#34249,.F.);
#45759=ORIENTED_EDGE('',*,*,#34250,.F.);
#45760=ORIENTED_EDGE('',*,*,#34251,.T.);
#45761=ORIENTED_EDGE('',*,*,#34252,.T.);
#45762=ORIENTED_EDGE('',*,*,#34247,.F.);
#45763=ORIENTED_EDGE('',*,*,#34253,.F.);
#45764=ORIENTED_EDGE('',*,*,#34254,.T.);
#45765=ORIENTED_EDGE('',*,*,#34255,.T.);
#45766=ORIENTED_EDGE('',*,*,#34251,.F.);
#45767=ORIENTED_EDGE('',*,*,#34256,.F.);
#45768=ORIENTED_EDGE('',*,*,#34249,.T.);
#45769=ORIENTED_EDGE('',*,*,#34257,.T.);
#45770=ORIENTED_EDGE('',*,*,#34254,.F.);
#45771=ORIENTED_EDGE('',*,*,#34257,.F.);
#45772=ORIENTED_EDGE('',*,*,#34248,.F.);
#45773=ORIENTED_EDGE('',*,*,#34252,.F.);
#45774=ORIENTED_EDGE('',*,*,#34255,.F.);
#45775=ORIENTED_EDGE('',*,*,#34258,.F.);
#45776=ORIENTED_EDGE('',*,*,#34259,.T.);
#45777=ORIENTED_EDGE('',*,*,#34260,.T.);
#45778=ORIENTED_EDGE('',*,*,#34261,.F.);
#45779=ORIENTED_EDGE('',*,*,#34262,.F.);
#45780=ORIENTED_EDGE('',*,*,#34263,.T.);
#45781=ORIENTED_EDGE('',*,*,#34264,.T.);
#45782=ORIENTED_EDGE('',*,*,#34259,.F.);
#45783=ORIENTED_EDGE('',*,*,#34265,.F.);
#45784=ORIENTED_EDGE('',*,*,#34266,.T.);
#45785=ORIENTED_EDGE('',*,*,#34267,.T.);
#45786=ORIENTED_EDGE('',*,*,#34263,.F.);
#45787=ORIENTED_EDGE('',*,*,#34268,.F.);
#45788=ORIENTED_EDGE('',*,*,#34261,.T.);
#45789=ORIENTED_EDGE('',*,*,#34269,.T.);
#45790=ORIENTED_EDGE('',*,*,#34266,.F.);
#45791=ORIENTED_EDGE('',*,*,#34269,.F.);
#45792=ORIENTED_EDGE('',*,*,#34260,.F.);
#45793=ORIENTED_EDGE('',*,*,#34264,.F.);
#45794=ORIENTED_EDGE('',*,*,#34267,.F.);
#45795=ORIENTED_EDGE('',*,*,#34270,.F.);
#45796=ORIENTED_EDGE('',*,*,#34271,.T.);
#45797=ORIENTED_EDGE('',*,*,#34272,.T.);
#45798=ORIENTED_EDGE('',*,*,#34273,.F.);
#45799=ORIENTED_EDGE('',*,*,#34274,.F.);
#45800=ORIENTED_EDGE('',*,*,#34275,.T.);
#45801=ORIENTED_EDGE('',*,*,#34276,.T.);
#45802=ORIENTED_EDGE('',*,*,#34271,.F.);
#45803=ORIENTED_EDGE('',*,*,#34277,.F.);
#45804=ORIENTED_EDGE('',*,*,#34278,.T.);
#45805=ORIENTED_EDGE('',*,*,#34279,.T.);
#45806=ORIENTED_EDGE('',*,*,#34275,.F.);
#45807=ORIENTED_EDGE('',*,*,#34280,.F.);
#45808=ORIENTED_EDGE('',*,*,#34273,.T.);
#45809=ORIENTED_EDGE('',*,*,#34281,.T.);
#45810=ORIENTED_EDGE('',*,*,#34278,.F.);
#45811=ORIENTED_EDGE('',*,*,#34281,.F.);
#45812=ORIENTED_EDGE('',*,*,#34272,.F.);
#45813=ORIENTED_EDGE('',*,*,#34276,.F.);
#45814=ORIENTED_EDGE('',*,*,#34279,.F.);
#45815=ORIENTED_EDGE('',*,*,#34282,.F.);
#45816=ORIENTED_EDGE('',*,*,#34283,.T.);
#45817=ORIENTED_EDGE('',*,*,#34284,.T.);
#45818=ORIENTED_EDGE('',*,*,#34285,.F.);
#45819=ORIENTED_EDGE('',*,*,#34286,.F.);
#45820=ORIENTED_EDGE('',*,*,#34287,.T.);
#45821=ORIENTED_EDGE('',*,*,#34288,.T.);
#45822=ORIENTED_EDGE('',*,*,#34283,.F.);
#45823=ORIENTED_EDGE('',*,*,#34289,.F.);
#45824=ORIENTED_EDGE('',*,*,#34290,.T.);
#45825=ORIENTED_EDGE('',*,*,#34291,.T.);
#45826=ORIENTED_EDGE('',*,*,#34287,.F.);
#45827=ORIENTED_EDGE('',*,*,#34292,.F.);
#45828=ORIENTED_EDGE('',*,*,#34285,.T.);
#45829=ORIENTED_EDGE('',*,*,#34293,.T.);
#45830=ORIENTED_EDGE('',*,*,#34290,.F.);
#45831=ORIENTED_EDGE('',*,*,#34293,.F.);
#45832=ORIENTED_EDGE('',*,*,#34284,.F.);
#45833=ORIENTED_EDGE('',*,*,#34288,.F.);
#45834=ORIENTED_EDGE('',*,*,#34291,.F.);
#45835=ORIENTED_EDGE('',*,*,#34294,.F.);
#45836=ORIENTED_EDGE('',*,*,#34295,.T.);
#45837=ORIENTED_EDGE('',*,*,#34296,.T.);
#45838=ORIENTED_EDGE('',*,*,#34297,.F.);
#45839=ORIENTED_EDGE('',*,*,#34298,.F.);
#45840=ORIENTED_EDGE('',*,*,#34299,.T.);
#45841=ORIENTED_EDGE('',*,*,#34300,.T.);
#45842=ORIENTED_EDGE('',*,*,#34295,.F.);
#45843=ORIENTED_EDGE('',*,*,#34301,.F.);
#45844=ORIENTED_EDGE('',*,*,#34302,.T.);
#45845=ORIENTED_EDGE('',*,*,#34303,.T.);
#45846=ORIENTED_EDGE('',*,*,#34299,.F.);
#45847=ORIENTED_EDGE('',*,*,#34304,.F.);
#45848=ORIENTED_EDGE('',*,*,#34297,.T.);
#45849=ORIENTED_EDGE('',*,*,#34305,.T.);
#45850=ORIENTED_EDGE('',*,*,#34302,.F.);
#45851=ORIENTED_EDGE('',*,*,#34305,.F.);
#45852=ORIENTED_EDGE('',*,*,#34296,.F.);
#45853=ORIENTED_EDGE('',*,*,#34300,.F.);
#45854=ORIENTED_EDGE('',*,*,#34303,.F.);
#45855=ORIENTED_EDGE('',*,*,#34306,.F.);
#45856=ORIENTED_EDGE('',*,*,#34307,.T.);
#45857=ORIENTED_EDGE('',*,*,#34308,.T.);
#45858=ORIENTED_EDGE('',*,*,#34309,.F.);
#45859=ORIENTED_EDGE('',*,*,#34310,.F.);
#45860=ORIENTED_EDGE('',*,*,#34311,.T.);
#45861=ORIENTED_EDGE('',*,*,#34312,.T.);
#45862=ORIENTED_EDGE('',*,*,#34307,.F.);
#45863=ORIENTED_EDGE('',*,*,#34313,.F.);
#45864=ORIENTED_EDGE('',*,*,#34314,.T.);
#45865=ORIENTED_EDGE('',*,*,#34315,.T.);
#45866=ORIENTED_EDGE('',*,*,#34311,.F.);
#45867=ORIENTED_EDGE('',*,*,#34316,.F.);
#45868=ORIENTED_EDGE('',*,*,#34309,.T.);
#45869=ORIENTED_EDGE('',*,*,#34317,.T.);
#45870=ORIENTED_EDGE('',*,*,#34314,.F.);
#45871=ORIENTED_EDGE('',*,*,#34317,.F.);
#45872=ORIENTED_EDGE('',*,*,#34308,.F.);
#45873=ORIENTED_EDGE('',*,*,#34312,.F.);
#45874=ORIENTED_EDGE('',*,*,#34315,.F.);
#45875=ORIENTED_EDGE('',*,*,#34318,.F.);
#45876=ORIENTED_EDGE('',*,*,#34319,.T.);
#45877=ORIENTED_EDGE('',*,*,#34320,.T.);
#45878=ORIENTED_EDGE('',*,*,#34321,.F.);
#45879=ORIENTED_EDGE('',*,*,#34322,.F.);
#45880=ORIENTED_EDGE('',*,*,#34323,.T.);
#45881=ORIENTED_EDGE('',*,*,#34324,.T.);
#45882=ORIENTED_EDGE('',*,*,#34319,.F.);
#45883=ORIENTED_EDGE('',*,*,#34325,.F.);
#45884=ORIENTED_EDGE('',*,*,#34326,.T.);
#45885=ORIENTED_EDGE('',*,*,#34327,.T.);
#45886=ORIENTED_EDGE('',*,*,#34323,.F.);
#45887=ORIENTED_EDGE('',*,*,#34328,.F.);
#45888=ORIENTED_EDGE('',*,*,#34321,.T.);
#45889=ORIENTED_EDGE('',*,*,#34329,.T.);
#45890=ORIENTED_EDGE('',*,*,#34326,.F.);
#45891=ORIENTED_EDGE('',*,*,#34329,.F.);
#45892=ORIENTED_EDGE('',*,*,#34320,.F.);
#45893=ORIENTED_EDGE('',*,*,#34324,.F.);
#45894=ORIENTED_EDGE('',*,*,#34327,.F.);
#45895=ORIENTED_EDGE('',*,*,#34330,.F.);
#45896=ORIENTED_EDGE('',*,*,#34331,.T.);
#45897=ORIENTED_EDGE('',*,*,#34332,.T.);
#45898=ORIENTED_EDGE('',*,*,#34333,.F.);
#45899=ORIENTED_EDGE('',*,*,#34334,.F.);
#45900=ORIENTED_EDGE('',*,*,#34335,.T.);
#45901=ORIENTED_EDGE('',*,*,#34336,.T.);
#45902=ORIENTED_EDGE('',*,*,#34331,.F.);
#45903=ORIENTED_EDGE('',*,*,#34337,.F.);
#45904=ORIENTED_EDGE('',*,*,#34338,.T.);
#45905=ORIENTED_EDGE('',*,*,#34339,.T.);
#45906=ORIENTED_EDGE('',*,*,#34335,.F.);
#45907=ORIENTED_EDGE('',*,*,#34340,.F.);
#45908=ORIENTED_EDGE('',*,*,#34333,.T.);
#45909=ORIENTED_EDGE('',*,*,#34341,.T.);
#45910=ORIENTED_EDGE('',*,*,#34338,.F.);
#45911=ORIENTED_EDGE('',*,*,#34341,.F.);
#45912=ORIENTED_EDGE('',*,*,#34332,.F.);
#45913=ORIENTED_EDGE('',*,*,#34336,.F.);
#45914=ORIENTED_EDGE('',*,*,#34339,.F.);
#45915=ORIENTED_EDGE('',*,*,#34342,.F.);
#45916=ORIENTED_EDGE('',*,*,#34343,.T.);
#45917=ORIENTED_EDGE('',*,*,#34344,.T.);
#45918=ORIENTED_EDGE('',*,*,#34345,.F.);
#45919=ORIENTED_EDGE('',*,*,#34346,.F.);
#45920=ORIENTED_EDGE('',*,*,#34347,.T.);
#45921=ORIENTED_EDGE('',*,*,#34348,.T.);
#45922=ORIENTED_EDGE('',*,*,#34343,.F.);
#45923=ORIENTED_EDGE('',*,*,#34349,.F.);
#45924=ORIENTED_EDGE('',*,*,#34350,.T.);
#45925=ORIENTED_EDGE('',*,*,#34351,.T.);
#45926=ORIENTED_EDGE('',*,*,#34347,.F.);
#45927=ORIENTED_EDGE('',*,*,#34352,.F.);
#45928=ORIENTED_EDGE('',*,*,#34345,.T.);
#45929=ORIENTED_EDGE('',*,*,#34353,.T.);
#45930=ORIENTED_EDGE('',*,*,#34350,.F.);
#45931=ORIENTED_EDGE('',*,*,#34353,.F.);
#45932=ORIENTED_EDGE('',*,*,#34344,.F.);
#45933=ORIENTED_EDGE('',*,*,#34348,.F.);
#45934=ORIENTED_EDGE('',*,*,#34351,.F.);
#45935=ORIENTED_EDGE('',*,*,#34354,.F.);
#45936=ORIENTED_EDGE('',*,*,#34355,.T.);
#45937=ORIENTED_EDGE('',*,*,#34356,.T.);
#45938=ORIENTED_EDGE('',*,*,#34357,.F.);
#45939=ORIENTED_EDGE('',*,*,#34358,.F.);
#45940=ORIENTED_EDGE('',*,*,#34359,.T.);
#45941=ORIENTED_EDGE('',*,*,#34360,.T.);
#45942=ORIENTED_EDGE('',*,*,#34355,.F.);
#45943=ORIENTED_EDGE('',*,*,#34361,.F.);
#45944=ORIENTED_EDGE('',*,*,#34362,.T.);
#45945=ORIENTED_EDGE('',*,*,#34363,.T.);
#45946=ORIENTED_EDGE('',*,*,#34359,.F.);
#45947=ORIENTED_EDGE('',*,*,#34364,.F.);
#45948=ORIENTED_EDGE('',*,*,#34357,.T.);
#45949=ORIENTED_EDGE('',*,*,#34365,.T.);
#45950=ORIENTED_EDGE('',*,*,#34362,.F.);
#45951=ORIENTED_EDGE('',*,*,#34365,.F.);
#45952=ORIENTED_EDGE('',*,*,#34356,.F.);
#45953=ORIENTED_EDGE('',*,*,#34360,.F.);
#45954=ORIENTED_EDGE('',*,*,#34363,.F.);
#45955=ORIENTED_EDGE('',*,*,#34366,.F.);
#45956=ORIENTED_EDGE('',*,*,#34367,.T.);
#45957=ORIENTED_EDGE('',*,*,#34368,.T.);
#45958=ORIENTED_EDGE('',*,*,#34369,.F.);
#45959=ORIENTED_EDGE('',*,*,#34370,.F.);
#45960=ORIENTED_EDGE('',*,*,#34371,.T.);
#45961=ORIENTED_EDGE('',*,*,#34372,.T.);
#45962=ORIENTED_EDGE('',*,*,#34367,.F.);
#45963=ORIENTED_EDGE('',*,*,#34373,.F.);
#45964=ORIENTED_EDGE('',*,*,#34374,.T.);
#45965=ORIENTED_EDGE('',*,*,#34375,.T.);
#45966=ORIENTED_EDGE('',*,*,#34371,.F.);
#45967=ORIENTED_EDGE('',*,*,#34376,.F.);
#45968=ORIENTED_EDGE('',*,*,#34369,.T.);
#45969=ORIENTED_EDGE('',*,*,#34377,.T.);
#45970=ORIENTED_EDGE('',*,*,#34374,.F.);
#45971=ORIENTED_EDGE('',*,*,#34377,.F.);
#45972=ORIENTED_EDGE('',*,*,#34368,.F.);
#45973=ORIENTED_EDGE('',*,*,#34372,.F.);
#45974=ORIENTED_EDGE('',*,*,#34375,.F.);
#45975=ORIENTED_EDGE('',*,*,#34378,.F.);
#45976=ORIENTED_EDGE('',*,*,#34379,.T.);
#45977=ORIENTED_EDGE('',*,*,#34380,.T.);
#45978=ORIENTED_EDGE('',*,*,#34381,.F.);
#45979=ORIENTED_EDGE('',*,*,#34382,.F.);
#45980=ORIENTED_EDGE('',*,*,#34383,.T.);
#45981=ORIENTED_EDGE('',*,*,#34384,.T.);
#45982=ORIENTED_EDGE('',*,*,#34379,.F.);
#45983=ORIENTED_EDGE('',*,*,#34385,.F.);
#45984=ORIENTED_EDGE('',*,*,#34386,.T.);
#45985=ORIENTED_EDGE('',*,*,#34387,.T.);
#45986=ORIENTED_EDGE('',*,*,#34383,.F.);
#45987=ORIENTED_EDGE('',*,*,#34388,.F.);
#45988=ORIENTED_EDGE('',*,*,#34381,.T.);
#45989=ORIENTED_EDGE('',*,*,#34389,.T.);
#45990=ORIENTED_EDGE('',*,*,#34386,.F.);
#45991=ORIENTED_EDGE('',*,*,#34389,.F.);
#45992=ORIENTED_EDGE('',*,*,#34380,.F.);
#45993=ORIENTED_EDGE('',*,*,#34384,.F.);
#45994=ORIENTED_EDGE('',*,*,#34387,.F.);
#45995=ORIENTED_EDGE('',*,*,#34390,.F.);
#45996=ORIENTED_EDGE('',*,*,#34391,.T.);
#45997=ORIENTED_EDGE('',*,*,#34392,.T.);
#45998=ORIENTED_EDGE('',*,*,#34393,.F.);
#45999=ORIENTED_EDGE('',*,*,#34394,.F.);
#46000=ORIENTED_EDGE('',*,*,#34395,.T.);
#46001=ORIENTED_EDGE('',*,*,#34396,.T.);
#46002=ORIENTED_EDGE('',*,*,#34391,.F.);
#46003=ORIENTED_EDGE('',*,*,#34397,.F.);
#46004=ORIENTED_EDGE('',*,*,#34398,.T.);
#46005=ORIENTED_EDGE('',*,*,#34399,.T.);
#46006=ORIENTED_EDGE('',*,*,#34395,.F.);
#46007=ORIENTED_EDGE('',*,*,#34400,.F.);
#46008=ORIENTED_EDGE('',*,*,#34393,.T.);
#46009=ORIENTED_EDGE('',*,*,#34401,.T.);
#46010=ORIENTED_EDGE('',*,*,#34398,.F.);
#46011=ORIENTED_EDGE('',*,*,#34401,.F.);
#46012=ORIENTED_EDGE('',*,*,#34392,.F.);
#46013=ORIENTED_EDGE('',*,*,#34396,.F.);
#46014=ORIENTED_EDGE('',*,*,#34399,.F.);
#46015=ORIENTED_EDGE('',*,*,#34402,.F.);
#46016=ORIENTED_EDGE('',*,*,#34403,.T.);
#46017=ORIENTED_EDGE('',*,*,#34404,.T.);
#46018=ORIENTED_EDGE('',*,*,#34405,.F.);
#46019=ORIENTED_EDGE('',*,*,#34406,.F.);
#46020=ORIENTED_EDGE('',*,*,#34407,.T.);
#46021=ORIENTED_EDGE('',*,*,#34408,.T.);
#46022=ORIENTED_EDGE('',*,*,#34403,.F.);
#46023=ORIENTED_EDGE('',*,*,#34409,.F.);
#46024=ORIENTED_EDGE('',*,*,#34410,.T.);
#46025=ORIENTED_EDGE('',*,*,#34411,.T.);
#46026=ORIENTED_EDGE('',*,*,#34407,.F.);
#46027=ORIENTED_EDGE('',*,*,#34412,.F.);
#46028=ORIENTED_EDGE('',*,*,#34405,.T.);
#46029=ORIENTED_EDGE('',*,*,#34413,.T.);
#46030=ORIENTED_EDGE('',*,*,#34410,.F.);
#46031=ORIENTED_EDGE('',*,*,#34413,.F.);
#46032=ORIENTED_EDGE('',*,*,#34404,.F.);
#46033=ORIENTED_EDGE('',*,*,#34408,.F.);
#46034=ORIENTED_EDGE('',*,*,#34411,.F.);
#46035=ORIENTED_EDGE('',*,*,#34414,.F.);
#46036=ORIENTED_EDGE('',*,*,#34415,.T.);
#46037=ORIENTED_EDGE('',*,*,#34416,.T.);
#46038=ORIENTED_EDGE('',*,*,#34417,.F.);
#46039=ORIENTED_EDGE('',*,*,#34418,.F.);
#46040=ORIENTED_EDGE('',*,*,#34419,.T.);
#46041=ORIENTED_EDGE('',*,*,#34420,.T.);
#46042=ORIENTED_EDGE('',*,*,#34415,.F.);
#46043=ORIENTED_EDGE('',*,*,#34421,.F.);
#46044=ORIENTED_EDGE('',*,*,#34422,.T.);
#46045=ORIENTED_EDGE('',*,*,#34423,.T.);
#46046=ORIENTED_EDGE('',*,*,#34419,.F.);
#46047=ORIENTED_EDGE('',*,*,#34424,.F.);
#46048=ORIENTED_EDGE('',*,*,#34417,.T.);
#46049=ORIENTED_EDGE('',*,*,#34425,.T.);
#46050=ORIENTED_EDGE('',*,*,#34422,.F.);
#46051=ORIENTED_EDGE('',*,*,#34425,.F.);
#46052=ORIENTED_EDGE('',*,*,#34416,.F.);
#46053=ORIENTED_EDGE('',*,*,#34420,.F.);
#46054=ORIENTED_EDGE('',*,*,#34423,.F.);
#46055=ORIENTED_EDGE('',*,*,#34426,.F.);
#46056=ORIENTED_EDGE('',*,*,#34427,.T.);
#46057=ORIENTED_EDGE('',*,*,#34428,.T.);
#46058=ORIENTED_EDGE('',*,*,#34429,.F.);
#46059=ORIENTED_EDGE('',*,*,#34430,.F.);
#46060=ORIENTED_EDGE('',*,*,#34431,.T.);
#46061=ORIENTED_EDGE('',*,*,#34432,.T.);
#46062=ORIENTED_EDGE('',*,*,#34427,.F.);
#46063=ORIENTED_EDGE('',*,*,#34433,.F.);
#46064=ORIENTED_EDGE('',*,*,#34434,.T.);
#46065=ORIENTED_EDGE('',*,*,#34435,.T.);
#46066=ORIENTED_EDGE('',*,*,#34431,.F.);
#46067=ORIENTED_EDGE('',*,*,#34436,.F.);
#46068=ORIENTED_EDGE('',*,*,#34429,.T.);
#46069=ORIENTED_EDGE('',*,*,#34437,.T.);
#46070=ORIENTED_EDGE('',*,*,#34434,.F.);
#46071=ORIENTED_EDGE('',*,*,#34437,.F.);
#46072=ORIENTED_EDGE('',*,*,#34428,.F.);
#46073=ORIENTED_EDGE('',*,*,#34432,.F.);
#46074=ORIENTED_EDGE('',*,*,#34435,.F.);
#46075=ORIENTED_EDGE('',*,*,#34438,.F.);
#46076=ORIENTED_EDGE('',*,*,#34439,.T.);
#46077=ORIENTED_EDGE('',*,*,#34440,.T.);
#46078=ORIENTED_EDGE('',*,*,#34441,.F.);
#46079=ORIENTED_EDGE('',*,*,#34442,.F.);
#46080=ORIENTED_EDGE('',*,*,#34443,.T.);
#46081=ORIENTED_EDGE('',*,*,#34444,.T.);
#46082=ORIENTED_EDGE('',*,*,#34439,.F.);
#46083=ORIENTED_EDGE('',*,*,#34445,.F.);
#46084=ORIENTED_EDGE('',*,*,#34446,.T.);
#46085=ORIENTED_EDGE('',*,*,#34447,.T.);
#46086=ORIENTED_EDGE('',*,*,#34443,.F.);
#46087=ORIENTED_EDGE('',*,*,#34448,.F.);
#46088=ORIENTED_EDGE('',*,*,#34441,.T.);
#46089=ORIENTED_EDGE('',*,*,#34449,.T.);
#46090=ORIENTED_EDGE('',*,*,#34446,.F.);
#46091=ORIENTED_EDGE('',*,*,#34449,.F.);
#46092=ORIENTED_EDGE('',*,*,#34440,.F.);
#46093=ORIENTED_EDGE('',*,*,#34444,.F.);
#46094=ORIENTED_EDGE('',*,*,#34447,.F.);
#46095=ORIENTED_EDGE('',*,*,#34450,.F.);
#46096=ORIENTED_EDGE('',*,*,#34451,.T.);
#46097=ORIENTED_EDGE('',*,*,#34452,.T.);
#46098=ORIENTED_EDGE('',*,*,#34453,.F.);
#46099=ORIENTED_EDGE('',*,*,#34454,.F.);
#46100=ORIENTED_EDGE('',*,*,#34455,.T.);
#46101=ORIENTED_EDGE('',*,*,#34456,.T.);
#46102=ORIENTED_EDGE('',*,*,#34451,.F.);
#46103=ORIENTED_EDGE('',*,*,#34457,.F.);
#46104=ORIENTED_EDGE('',*,*,#34458,.T.);
#46105=ORIENTED_EDGE('',*,*,#34459,.T.);
#46106=ORIENTED_EDGE('',*,*,#34455,.F.);
#46107=ORIENTED_EDGE('',*,*,#34460,.F.);
#46108=ORIENTED_EDGE('',*,*,#34453,.T.);
#46109=ORIENTED_EDGE('',*,*,#34461,.T.);
#46110=ORIENTED_EDGE('',*,*,#34458,.F.);
#46111=ORIENTED_EDGE('',*,*,#34461,.F.);
#46112=ORIENTED_EDGE('',*,*,#34452,.F.);
#46113=ORIENTED_EDGE('',*,*,#34456,.F.);
#46114=ORIENTED_EDGE('',*,*,#34459,.F.);
#46115=ORIENTED_EDGE('',*,*,#34462,.F.);
#46116=ORIENTED_EDGE('',*,*,#34463,.T.);
#46117=ORIENTED_EDGE('',*,*,#34464,.T.);
#46118=ORIENTED_EDGE('',*,*,#34465,.F.);
#46119=ORIENTED_EDGE('',*,*,#34466,.F.);
#46120=ORIENTED_EDGE('',*,*,#34467,.T.);
#46121=ORIENTED_EDGE('',*,*,#34468,.T.);
#46122=ORIENTED_EDGE('',*,*,#34463,.F.);
#46123=ORIENTED_EDGE('',*,*,#34469,.F.);
#46124=ORIENTED_EDGE('',*,*,#34470,.T.);
#46125=ORIENTED_EDGE('',*,*,#34471,.T.);
#46126=ORIENTED_EDGE('',*,*,#34467,.F.);
#46127=ORIENTED_EDGE('',*,*,#34472,.F.);
#46128=ORIENTED_EDGE('',*,*,#34465,.T.);
#46129=ORIENTED_EDGE('',*,*,#34473,.T.);
#46130=ORIENTED_EDGE('',*,*,#34470,.F.);
#46131=ORIENTED_EDGE('',*,*,#34473,.F.);
#46132=ORIENTED_EDGE('',*,*,#34464,.F.);
#46133=ORIENTED_EDGE('',*,*,#34468,.F.);
#46134=ORIENTED_EDGE('',*,*,#34471,.F.);
#46135=ORIENTED_EDGE('',*,*,#34474,.F.);
#46136=ORIENTED_EDGE('',*,*,#34475,.T.);
#46137=ORIENTED_EDGE('',*,*,#34476,.T.);
#46138=ORIENTED_EDGE('',*,*,#34477,.F.);
#46139=ORIENTED_EDGE('',*,*,#34478,.F.);
#46140=ORIENTED_EDGE('',*,*,#34479,.T.);
#46141=ORIENTED_EDGE('',*,*,#34480,.T.);
#46142=ORIENTED_EDGE('',*,*,#34475,.F.);
#46143=ORIENTED_EDGE('',*,*,#34481,.F.);
#46144=ORIENTED_EDGE('',*,*,#34482,.T.);
#46145=ORIENTED_EDGE('',*,*,#34483,.T.);
#46146=ORIENTED_EDGE('',*,*,#34479,.F.);
#46147=ORIENTED_EDGE('',*,*,#34484,.F.);
#46148=ORIENTED_EDGE('',*,*,#34477,.T.);
#46149=ORIENTED_EDGE('',*,*,#34485,.T.);
#46150=ORIENTED_EDGE('',*,*,#34482,.F.);
#46151=ORIENTED_EDGE('',*,*,#34485,.F.);
#46152=ORIENTED_EDGE('',*,*,#34476,.F.);
#46153=ORIENTED_EDGE('',*,*,#34480,.F.);
#46154=ORIENTED_EDGE('',*,*,#34483,.F.);
#46155=ORIENTED_EDGE('',*,*,#34486,.F.);
#46156=ORIENTED_EDGE('',*,*,#34487,.T.);
#46157=ORIENTED_EDGE('',*,*,#34488,.T.);
#46158=ORIENTED_EDGE('',*,*,#34489,.F.);
#46159=ORIENTED_EDGE('',*,*,#34490,.F.);
#46160=ORIENTED_EDGE('',*,*,#34491,.T.);
#46161=ORIENTED_EDGE('',*,*,#34492,.T.);
#46162=ORIENTED_EDGE('',*,*,#34487,.F.);
#46163=ORIENTED_EDGE('',*,*,#34493,.F.);
#46164=ORIENTED_EDGE('',*,*,#34494,.T.);
#46165=ORIENTED_EDGE('',*,*,#34495,.T.);
#46166=ORIENTED_EDGE('',*,*,#34491,.F.);
#46167=ORIENTED_EDGE('',*,*,#34496,.F.);
#46168=ORIENTED_EDGE('',*,*,#34489,.T.);
#46169=ORIENTED_EDGE('',*,*,#34497,.T.);
#46170=ORIENTED_EDGE('',*,*,#34494,.F.);
#46171=ORIENTED_EDGE('',*,*,#34497,.F.);
#46172=ORIENTED_EDGE('',*,*,#34488,.F.);
#46173=ORIENTED_EDGE('',*,*,#34492,.F.);
#46174=ORIENTED_EDGE('',*,*,#34495,.F.);
#46175=ORIENTED_EDGE('',*,*,#34498,.F.);
#46176=ORIENTED_EDGE('',*,*,#34499,.T.);
#46177=ORIENTED_EDGE('',*,*,#34500,.T.);
#46178=ORIENTED_EDGE('',*,*,#34501,.F.);
#46179=ORIENTED_EDGE('',*,*,#34502,.F.);
#46180=ORIENTED_EDGE('',*,*,#34503,.T.);
#46181=ORIENTED_EDGE('',*,*,#34504,.T.);
#46182=ORIENTED_EDGE('',*,*,#34499,.F.);
#46183=ORIENTED_EDGE('',*,*,#34505,.F.);
#46184=ORIENTED_EDGE('',*,*,#34506,.T.);
#46185=ORIENTED_EDGE('',*,*,#34507,.T.);
#46186=ORIENTED_EDGE('',*,*,#34503,.F.);
#46187=ORIENTED_EDGE('',*,*,#34508,.F.);
#46188=ORIENTED_EDGE('',*,*,#34501,.T.);
#46189=ORIENTED_EDGE('',*,*,#34509,.T.);
#46190=ORIENTED_EDGE('',*,*,#34506,.F.);
#46191=ORIENTED_EDGE('',*,*,#34509,.F.);
#46192=ORIENTED_EDGE('',*,*,#34500,.F.);
#46193=ORIENTED_EDGE('',*,*,#34504,.F.);
#46194=ORIENTED_EDGE('',*,*,#34507,.F.);
#46195=ORIENTED_EDGE('',*,*,#34510,.F.);
#46196=ORIENTED_EDGE('',*,*,#34511,.T.);
#46197=ORIENTED_EDGE('',*,*,#34512,.T.);
#46198=ORIENTED_EDGE('',*,*,#34513,.F.);
#46199=ORIENTED_EDGE('',*,*,#34514,.F.);
#46200=ORIENTED_EDGE('',*,*,#34515,.T.);
#46201=ORIENTED_EDGE('',*,*,#34516,.T.);
#46202=ORIENTED_EDGE('',*,*,#34511,.F.);
#46203=ORIENTED_EDGE('',*,*,#34517,.F.);
#46204=ORIENTED_EDGE('',*,*,#34518,.T.);
#46205=ORIENTED_EDGE('',*,*,#34519,.T.);
#46206=ORIENTED_EDGE('',*,*,#34515,.F.);
#46207=ORIENTED_EDGE('',*,*,#34520,.F.);
#46208=ORIENTED_EDGE('',*,*,#34513,.T.);
#46209=ORIENTED_EDGE('',*,*,#34521,.T.);
#46210=ORIENTED_EDGE('',*,*,#34518,.F.);
#46211=ORIENTED_EDGE('',*,*,#34521,.F.);
#46212=ORIENTED_EDGE('',*,*,#34512,.F.);
#46213=ORIENTED_EDGE('',*,*,#34516,.F.);
#46214=ORIENTED_EDGE('',*,*,#34519,.F.);
#46215=ORIENTED_EDGE('',*,*,#34522,.F.);
#46216=ORIENTED_EDGE('',*,*,#34523,.T.);
#46217=ORIENTED_EDGE('',*,*,#34524,.T.);
#46218=ORIENTED_EDGE('',*,*,#34525,.F.);
#46219=ORIENTED_EDGE('',*,*,#34526,.F.);
#46220=ORIENTED_EDGE('',*,*,#34527,.T.);
#46221=ORIENTED_EDGE('',*,*,#34528,.T.);
#46222=ORIENTED_EDGE('',*,*,#34523,.F.);
#46223=ORIENTED_EDGE('',*,*,#34529,.F.);
#46224=ORIENTED_EDGE('',*,*,#34530,.T.);
#46225=ORIENTED_EDGE('',*,*,#34531,.T.);
#46226=ORIENTED_EDGE('',*,*,#34527,.F.);
#46227=ORIENTED_EDGE('',*,*,#34532,.F.);
#46228=ORIENTED_EDGE('',*,*,#34525,.T.);
#46229=ORIENTED_EDGE('',*,*,#34533,.T.);
#46230=ORIENTED_EDGE('',*,*,#34530,.F.);
#46231=ORIENTED_EDGE('',*,*,#34533,.F.);
#46232=ORIENTED_EDGE('',*,*,#34524,.F.);
#46233=ORIENTED_EDGE('',*,*,#34528,.F.);
#46234=ORIENTED_EDGE('',*,*,#34531,.F.);
#46235=ORIENTED_EDGE('',*,*,#34534,.F.);
#46236=ORIENTED_EDGE('',*,*,#34535,.T.);
#46237=ORIENTED_EDGE('',*,*,#34536,.T.);
#46238=ORIENTED_EDGE('',*,*,#34537,.F.);
#46239=ORIENTED_EDGE('',*,*,#34538,.F.);
#46240=ORIENTED_EDGE('',*,*,#34539,.T.);
#46241=ORIENTED_EDGE('',*,*,#34540,.T.);
#46242=ORIENTED_EDGE('',*,*,#34535,.F.);
#46243=ORIENTED_EDGE('',*,*,#34541,.F.);
#46244=ORIENTED_EDGE('',*,*,#34542,.T.);
#46245=ORIENTED_EDGE('',*,*,#34543,.T.);
#46246=ORIENTED_EDGE('',*,*,#34539,.F.);
#46247=ORIENTED_EDGE('',*,*,#34544,.F.);
#46248=ORIENTED_EDGE('',*,*,#34537,.T.);
#46249=ORIENTED_EDGE('',*,*,#34545,.T.);
#46250=ORIENTED_EDGE('',*,*,#34542,.F.);
#46251=ORIENTED_EDGE('',*,*,#34545,.F.);
#46252=ORIENTED_EDGE('',*,*,#34536,.F.);
#46253=ORIENTED_EDGE('',*,*,#34540,.F.);
#46254=ORIENTED_EDGE('',*,*,#34543,.F.);
#46255=ORIENTED_EDGE('',*,*,#34546,.F.);
#46256=ORIENTED_EDGE('',*,*,#34547,.T.);
#46257=ORIENTED_EDGE('',*,*,#34548,.T.);
#46258=ORIENTED_EDGE('',*,*,#34549,.F.);
#46259=ORIENTED_EDGE('',*,*,#34550,.F.);
#46260=ORIENTED_EDGE('',*,*,#34551,.T.);
#46261=ORIENTED_EDGE('',*,*,#34552,.T.);
#46262=ORIENTED_EDGE('',*,*,#34547,.F.);
#46263=ORIENTED_EDGE('',*,*,#34553,.F.);
#46264=ORIENTED_EDGE('',*,*,#34554,.T.);
#46265=ORIENTED_EDGE('',*,*,#34555,.T.);
#46266=ORIENTED_EDGE('',*,*,#34551,.F.);
#46267=ORIENTED_EDGE('',*,*,#34556,.F.);
#46268=ORIENTED_EDGE('',*,*,#34549,.T.);
#46269=ORIENTED_EDGE('',*,*,#34557,.T.);
#46270=ORIENTED_EDGE('',*,*,#34554,.F.);
#46271=ORIENTED_EDGE('',*,*,#34557,.F.);
#46272=ORIENTED_EDGE('',*,*,#34548,.F.);
#46273=ORIENTED_EDGE('',*,*,#34552,.F.);
#46274=ORIENTED_EDGE('',*,*,#34555,.F.);
#46275=ORIENTED_EDGE('',*,*,#34558,.F.);
#46276=ORIENTED_EDGE('',*,*,#34559,.T.);
#46277=ORIENTED_EDGE('',*,*,#34560,.T.);
#46278=ORIENTED_EDGE('',*,*,#34561,.F.);
#46279=ORIENTED_EDGE('',*,*,#34562,.F.);
#46280=ORIENTED_EDGE('',*,*,#34563,.T.);
#46281=ORIENTED_EDGE('',*,*,#34564,.T.);
#46282=ORIENTED_EDGE('',*,*,#34559,.F.);
#46283=ORIENTED_EDGE('',*,*,#34565,.F.);
#46284=ORIENTED_EDGE('',*,*,#34566,.T.);
#46285=ORIENTED_EDGE('',*,*,#34567,.T.);
#46286=ORIENTED_EDGE('',*,*,#34563,.F.);
#46287=ORIENTED_EDGE('',*,*,#34568,.F.);
#46288=ORIENTED_EDGE('',*,*,#34561,.T.);
#46289=ORIENTED_EDGE('',*,*,#34569,.T.);
#46290=ORIENTED_EDGE('',*,*,#34566,.F.);
#46291=ORIENTED_EDGE('',*,*,#34569,.F.);
#46292=ORIENTED_EDGE('',*,*,#34560,.F.);
#46293=ORIENTED_EDGE('',*,*,#34564,.F.);
#46294=ORIENTED_EDGE('',*,*,#34567,.F.);
#46295=ORIENTED_EDGE('',*,*,#34570,.F.);
#46296=ORIENTED_EDGE('',*,*,#34571,.T.);
#46297=ORIENTED_EDGE('',*,*,#34572,.T.);
#46298=ORIENTED_EDGE('',*,*,#34573,.F.);
#46299=ORIENTED_EDGE('',*,*,#34574,.F.);
#46300=ORIENTED_EDGE('',*,*,#34575,.T.);
#46301=ORIENTED_EDGE('',*,*,#34576,.T.);
#46302=ORIENTED_EDGE('',*,*,#34571,.F.);
#46303=ORIENTED_EDGE('',*,*,#34577,.F.);
#46304=ORIENTED_EDGE('',*,*,#34578,.T.);
#46305=ORIENTED_EDGE('',*,*,#34579,.T.);
#46306=ORIENTED_EDGE('',*,*,#34575,.F.);
#46307=ORIENTED_EDGE('',*,*,#34580,.F.);
#46308=ORIENTED_EDGE('',*,*,#34573,.T.);
#46309=ORIENTED_EDGE('',*,*,#34581,.T.);
#46310=ORIENTED_EDGE('',*,*,#34578,.F.);
#46311=ORIENTED_EDGE('',*,*,#34581,.F.);
#46312=ORIENTED_EDGE('',*,*,#34572,.F.);
#46313=ORIENTED_EDGE('',*,*,#34576,.F.);
#46314=ORIENTED_EDGE('',*,*,#34579,.F.);
#46315=ORIENTED_EDGE('',*,*,#34582,.F.);
#46316=ORIENTED_EDGE('',*,*,#34583,.T.);
#46317=ORIENTED_EDGE('',*,*,#34584,.T.);
#46318=ORIENTED_EDGE('',*,*,#34585,.F.);
#46319=ORIENTED_EDGE('',*,*,#34586,.F.);
#46320=ORIENTED_EDGE('',*,*,#34587,.T.);
#46321=ORIENTED_EDGE('',*,*,#34588,.T.);
#46322=ORIENTED_EDGE('',*,*,#34583,.F.);
#46323=ORIENTED_EDGE('',*,*,#34589,.F.);
#46324=ORIENTED_EDGE('',*,*,#34590,.T.);
#46325=ORIENTED_EDGE('',*,*,#34591,.T.);
#46326=ORIENTED_EDGE('',*,*,#34587,.F.);
#46327=ORIENTED_EDGE('',*,*,#34592,.F.);
#46328=ORIENTED_EDGE('',*,*,#34585,.T.);
#46329=ORIENTED_EDGE('',*,*,#34593,.T.);
#46330=ORIENTED_EDGE('',*,*,#34590,.F.);
#46331=ORIENTED_EDGE('',*,*,#34593,.F.);
#46332=ORIENTED_EDGE('',*,*,#34584,.F.);
#46333=ORIENTED_EDGE('',*,*,#34588,.F.);
#46334=ORIENTED_EDGE('',*,*,#34591,.F.);
#46335=ORIENTED_EDGE('',*,*,#34594,.F.);
#46336=ORIENTED_EDGE('',*,*,#34595,.T.);
#46337=ORIENTED_EDGE('',*,*,#34596,.T.);
#46338=ORIENTED_EDGE('',*,*,#34597,.F.);
#46339=ORIENTED_EDGE('',*,*,#34598,.F.);
#46340=ORIENTED_EDGE('',*,*,#34599,.T.);
#46341=ORIENTED_EDGE('',*,*,#34600,.T.);
#46342=ORIENTED_EDGE('',*,*,#34595,.F.);
#46343=ORIENTED_EDGE('',*,*,#34601,.F.);
#46344=ORIENTED_EDGE('',*,*,#34602,.T.);
#46345=ORIENTED_EDGE('',*,*,#34603,.T.);
#46346=ORIENTED_EDGE('',*,*,#34599,.F.);
#46347=ORIENTED_EDGE('',*,*,#34604,.F.);
#46348=ORIENTED_EDGE('',*,*,#34597,.T.);
#46349=ORIENTED_EDGE('',*,*,#34605,.T.);
#46350=ORIENTED_EDGE('',*,*,#34602,.F.);
#46351=ORIENTED_EDGE('',*,*,#34605,.F.);
#46352=ORIENTED_EDGE('',*,*,#34596,.F.);
#46353=ORIENTED_EDGE('',*,*,#34600,.F.);
#46354=ORIENTED_EDGE('',*,*,#34603,.F.);
#46355=ORIENTED_EDGE('',*,*,#34606,.F.);
#46356=ORIENTED_EDGE('',*,*,#34607,.T.);
#46357=ORIENTED_EDGE('',*,*,#34608,.T.);
#46358=ORIENTED_EDGE('',*,*,#34609,.F.);
#46359=ORIENTED_EDGE('',*,*,#34610,.F.);
#46360=ORIENTED_EDGE('',*,*,#34611,.T.);
#46361=ORIENTED_EDGE('',*,*,#34612,.T.);
#46362=ORIENTED_EDGE('',*,*,#34607,.F.);
#46363=ORIENTED_EDGE('',*,*,#34613,.F.);
#46364=ORIENTED_EDGE('',*,*,#34614,.T.);
#46365=ORIENTED_EDGE('',*,*,#34615,.T.);
#46366=ORIENTED_EDGE('',*,*,#34611,.F.);
#46367=ORIENTED_EDGE('',*,*,#34616,.F.);
#46368=ORIENTED_EDGE('',*,*,#34609,.T.);
#46369=ORIENTED_EDGE('',*,*,#34617,.T.);
#46370=ORIENTED_EDGE('',*,*,#34614,.F.);
#46371=ORIENTED_EDGE('',*,*,#34617,.F.);
#46372=ORIENTED_EDGE('',*,*,#34608,.F.);
#46373=ORIENTED_EDGE('',*,*,#34612,.F.);
#46374=ORIENTED_EDGE('',*,*,#34615,.F.);
#46375=ORIENTED_EDGE('',*,*,#34618,.F.);
#46376=ORIENTED_EDGE('',*,*,#34619,.T.);
#46377=ORIENTED_EDGE('',*,*,#34620,.T.);
#46378=ORIENTED_EDGE('',*,*,#34621,.F.);
#46379=ORIENTED_EDGE('',*,*,#34622,.F.);
#46380=ORIENTED_EDGE('',*,*,#34623,.T.);
#46381=ORIENTED_EDGE('',*,*,#34624,.T.);
#46382=ORIENTED_EDGE('',*,*,#34619,.F.);
#46383=ORIENTED_EDGE('',*,*,#34625,.F.);
#46384=ORIENTED_EDGE('',*,*,#34626,.T.);
#46385=ORIENTED_EDGE('',*,*,#34627,.T.);
#46386=ORIENTED_EDGE('',*,*,#34623,.F.);
#46387=ORIENTED_EDGE('',*,*,#34628,.F.);
#46388=ORIENTED_EDGE('',*,*,#34621,.T.);
#46389=ORIENTED_EDGE('',*,*,#34629,.T.);
#46390=ORIENTED_EDGE('',*,*,#34626,.F.);
#46391=ORIENTED_EDGE('',*,*,#34629,.F.);
#46392=ORIENTED_EDGE('',*,*,#34620,.F.);
#46393=ORIENTED_EDGE('',*,*,#34624,.F.);
#46394=ORIENTED_EDGE('',*,*,#34627,.F.);
#46395=ORIENTED_EDGE('',*,*,#34630,.F.);
#46396=ORIENTED_EDGE('',*,*,#34631,.T.);
#46397=ORIENTED_EDGE('',*,*,#34632,.T.);
#46398=ORIENTED_EDGE('',*,*,#34633,.F.);
#46399=ORIENTED_EDGE('',*,*,#34634,.F.);
#46400=ORIENTED_EDGE('',*,*,#34635,.T.);
#46401=ORIENTED_EDGE('',*,*,#34636,.T.);
#46402=ORIENTED_EDGE('',*,*,#34631,.F.);
#46403=ORIENTED_EDGE('',*,*,#34637,.F.);
#46404=ORIENTED_EDGE('',*,*,#34638,.T.);
#46405=ORIENTED_EDGE('',*,*,#34639,.T.);
#46406=ORIENTED_EDGE('',*,*,#34635,.F.);
#46407=ORIENTED_EDGE('',*,*,#34640,.F.);
#46408=ORIENTED_EDGE('',*,*,#34633,.T.);
#46409=ORIENTED_EDGE('',*,*,#34641,.T.);
#46410=ORIENTED_EDGE('',*,*,#34638,.F.);
#46411=ORIENTED_EDGE('',*,*,#34641,.F.);
#46412=ORIENTED_EDGE('',*,*,#34632,.F.);
#46413=ORIENTED_EDGE('',*,*,#34636,.F.);
#46414=ORIENTED_EDGE('',*,*,#34639,.F.);
#46415=ORIENTED_EDGE('',*,*,#34642,.F.);
#46416=ORIENTED_EDGE('',*,*,#34643,.T.);
#46417=ORIENTED_EDGE('',*,*,#34644,.T.);
#46418=ORIENTED_EDGE('',*,*,#34645,.F.);
#46419=ORIENTED_EDGE('',*,*,#34646,.F.);
#46420=ORIENTED_EDGE('',*,*,#34647,.T.);
#46421=ORIENTED_EDGE('',*,*,#34648,.T.);
#46422=ORIENTED_EDGE('',*,*,#34643,.F.);
#46423=ORIENTED_EDGE('',*,*,#34649,.F.);
#46424=ORIENTED_EDGE('',*,*,#34650,.T.);
#46425=ORIENTED_EDGE('',*,*,#34651,.T.);
#46426=ORIENTED_EDGE('',*,*,#34647,.F.);
#46427=ORIENTED_EDGE('',*,*,#34652,.F.);
#46428=ORIENTED_EDGE('',*,*,#34645,.T.);
#46429=ORIENTED_EDGE('',*,*,#34653,.T.);
#46430=ORIENTED_EDGE('',*,*,#34650,.F.);
#46431=ORIENTED_EDGE('',*,*,#34653,.F.);
#46432=ORIENTED_EDGE('',*,*,#34644,.F.);
#46433=ORIENTED_EDGE('',*,*,#34648,.F.);
#46434=ORIENTED_EDGE('',*,*,#34651,.F.);
#46435=ORIENTED_EDGE('',*,*,#34654,.F.);
#46436=ORIENTED_EDGE('',*,*,#34655,.T.);
#46437=ORIENTED_EDGE('',*,*,#34656,.T.);
#46438=ORIENTED_EDGE('',*,*,#34657,.F.);
#46439=ORIENTED_EDGE('',*,*,#34658,.F.);
#46440=ORIENTED_EDGE('',*,*,#34659,.T.);
#46441=ORIENTED_EDGE('',*,*,#34660,.T.);
#46442=ORIENTED_EDGE('',*,*,#34655,.F.);
#46443=ORIENTED_EDGE('',*,*,#34661,.F.);
#46444=ORIENTED_EDGE('',*,*,#34662,.T.);
#46445=ORIENTED_EDGE('',*,*,#34663,.T.);
#46446=ORIENTED_EDGE('',*,*,#34659,.F.);
#46447=ORIENTED_EDGE('',*,*,#34664,.F.);
#46448=ORIENTED_EDGE('',*,*,#34657,.T.);
#46449=ORIENTED_EDGE('',*,*,#34665,.T.);
#46450=ORIENTED_EDGE('',*,*,#34662,.F.);
#46451=ORIENTED_EDGE('',*,*,#34665,.F.);
#46452=ORIENTED_EDGE('',*,*,#34656,.F.);
#46453=ORIENTED_EDGE('',*,*,#34660,.F.);
#46454=ORIENTED_EDGE('',*,*,#34663,.F.);
#46455=ORIENTED_EDGE('',*,*,#34666,.F.);
#46456=ORIENTED_EDGE('',*,*,#34667,.T.);
#46457=ORIENTED_EDGE('',*,*,#34668,.T.);
#46458=ORIENTED_EDGE('',*,*,#34669,.F.);
#46459=ORIENTED_EDGE('',*,*,#34670,.F.);
#46460=ORIENTED_EDGE('',*,*,#34671,.T.);
#46461=ORIENTED_EDGE('',*,*,#34672,.T.);
#46462=ORIENTED_EDGE('',*,*,#34667,.F.);
#46463=ORIENTED_EDGE('',*,*,#34673,.F.);
#46464=ORIENTED_EDGE('',*,*,#34674,.T.);
#46465=ORIENTED_EDGE('',*,*,#34675,.T.);
#46466=ORIENTED_EDGE('',*,*,#34671,.F.);
#46467=ORIENTED_EDGE('',*,*,#34676,.F.);
#46468=ORIENTED_EDGE('',*,*,#34669,.T.);
#46469=ORIENTED_EDGE('',*,*,#34677,.T.);
#46470=ORIENTED_EDGE('',*,*,#34674,.F.);
#46471=ORIENTED_EDGE('',*,*,#34677,.F.);
#46472=ORIENTED_EDGE('',*,*,#34668,.F.);
#46473=ORIENTED_EDGE('',*,*,#34672,.F.);
#46474=ORIENTED_EDGE('',*,*,#34675,.F.);
#46475=ORIENTED_EDGE('',*,*,#34678,.F.);
#46476=ORIENTED_EDGE('',*,*,#34679,.T.);
#46477=ORIENTED_EDGE('',*,*,#34680,.T.);
#46478=ORIENTED_EDGE('',*,*,#34681,.F.);
#46479=ORIENTED_EDGE('',*,*,#34682,.F.);
#46480=ORIENTED_EDGE('',*,*,#34683,.T.);
#46481=ORIENTED_EDGE('',*,*,#34684,.T.);
#46482=ORIENTED_EDGE('',*,*,#34679,.F.);
#46483=ORIENTED_EDGE('',*,*,#34685,.F.);
#46484=ORIENTED_EDGE('',*,*,#34686,.T.);
#46485=ORIENTED_EDGE('',*,*,#34687,.T.);
#46486=ORIENTED_EDGE('',*,*,#34683,.F.);
#46487=ORIENTED_EDGE('',*,*,#34688,.F.);
#46488=ORIENTED_EDGE('',*,*,#34681,.T.);
#46489=ORIENTED_EDGE('',*,*,#34689,.T.);
#46490=ORIENTED_EDGE('',*,*,#34686,.F.);
#46491=ORIENTED_EDGE('',*,*,#34689,.F.);
#46492=ORIENTED_EDGE('',*,*,#34680,.F.);
#46493=ORIENTED_EDGE('',*,*,#34684,.F.);
#46494=ORIENTED_EDGE('',*,*,#34687,.F.);
#46495=ORIENTED_EDGE('',*,*,#34690,.F.);
#46496=ORIENTED_EDGE('',*,*,#34691,.T.);
#46497=ORIENTED_EDGE('',*,*,#34692,.T.);
#46498=ORIENTED_EDGE('',*,*,#34693,.F.);
#46499=ORIENTED_EDGE('',*,*,#34694,.F.);
#46500=ORIENTED_EDGE('',*,*,#34695,.T.);
#46501=ORIENTED_EDGE('',*,*,#34696,.T.);
#46502=ORIENTED_EDGE('',*,*,#34691,.F.);
#46503=ORIENTED_EDGE('',*,*,#34697,.F.);
#46504=ORIENTED_EDGE('',*,*,#34698,.T.);
#46505=ORIENTED_EDGE('',*,*,#34699,.T.);
#46506=ORIENTED_EDGE('',*,*,#34695,.F.);
#46507=ORIENTED_EDGE('',*,*,#34700,.F.);
#46508=ORIENTED_EDGE('',*,*,#34693,.T.);
#46509=ORIENTED_EDGE('',*,*,#34701,.T.);
#46510=ORIENTED_EDGE('',*,*,#34698,.F.);
#46511=ORIENTED_EDGE('',*,*,#34701,.F.);
#46512=ORIENTED_EDGE('',*,*,#34692,.F.);
#46513=ORIENTED_EDGE('',*,*,#34696,.F.);
#46514=ORIENTED_EDGE('',*,*,#34699,.F.);
#46515=ORIENTED_EDGE('',*,*,#34702,.F.);
#46516=ORIENTED_EDGE('',*,*,#34703,.T.);
#46517=ORIENTED_EDGE('',*,*,#34704,.T.);
#46518=ORIENTED_EDGE('',*,*,#34705,.F.);
#46519=ORIENTED_EDGE('',*,*,#34706,.F.);
#46520=ORIENTED_EDGE('',*,*,#34707,.T.);
#46521=ORIENTED_EDGE('',*,*,#34708,.T.);
#46522=ORIENTED_EDGE('',*,*,#34703,.F.);
#46523=ORIENTED_EDGE('',*,*,#34709,.F.);
#46524=ORIENTED_EDGE('',*,*,#34710,.T.);
#46525=ORIENTED_EDGE('',*,*,#34711,.T.);
#46526=ORIENTED_EDGE('',*,*,#34707,.F.);
#46527=ORIENTED_EDGE('',*,*,#34712,.F.);
#46528=ORIENTED_EDGE('',*,*,#34705,.T.);
#46529=ORIENTED_EDGE('',*,*,#34713,.T.);
#46530=ORIENTED_EDGE('',*,*,#34710,.F.);
#46531=ORIENTED_EDGE('',*,*,#34713,.F.);
#46532=ORIENTED_EDGE('',*,*,#34704,.F.);
#46533=ORIENTED_EDGE('',*,*,#34708,.F.);
#46534=ORIENTED_EDGE('',*,*,#34711,.F.);
#46535=ORIENTED_EDGE('',*,*,#34714,.F.);
#46536=ORIENTED_EDGE('',*,*,#34715,.T.);
#46537=ORIENTED_EDGE('',*,*,#34716,.T.);
#46538=ORIENTED_EDGE('',*,*,#34717,.F.);
#46539=ORIENTED_EDGE('',*,*,#34718,.F.);
#46540=ORIENTED_EDGE('',*,*,#34719,.T.);
#46541=ORIENTED_EDGE('',*,*,#34720,.T.);
#46542=ORIENTED_EDGE('',*,*,#34715,.F.);
#46543=ORIENTED_EDGE('',*,*,#34721,.F.);
#46544=ORIENTED_EDGE('',*,*,#34722,.T.);
#46545=ORIENTED_EDGE('',*,*,#34723,.T.);
#46546=ORIENTED_EDGE('',*,*,#34719,.F.);
#46547=ORIENTED_EDGE('',*,*,#34724,.F.);
#46548=ORIENTED_EDGE('',*,*,#34717,.T.);
#46549=ORIENTED_EDGE('',*,*,#34725,.T.);
#46550=ORIENTED_EDGE('',*,*,#34722,.F.);
#46551=ORIENTED_EDGE('',*,*,#34725,.F.);
#46552=ORIENTED_EDGE('',*,*,#34716,.F.);
#46553=ORIENTED_EDGE('',*,*,#34720,.F.);
#46554=ORIENTED_EDGE('',*,*,#34723,.F.);
#46555=ORIENTED_EDGE('',*,*,#34726,.F.);
#46556=ORIENTED_EDGE('',*,*,#34727,.T.);
#46557=ORIENTED_EDGE('',*,*,#34728,.T.);
#46558=ORIENTED_EDGE('',*,*,#34729,.F.);
#46559=ORIENTED_EDGE('',*,*,#34730,.F.);
#46560=ORIENTED_EDGE('',*,*,#34731,.T.);
#46561=ORIENTED_EDGE('',*,*,#34732,.T.);
#46562=ORIENTED_EDGE('',*,*,#34727,.F.);
#46563=ORIENTED_EDGE('',*,*,#34733,.F.);
#46564=ORIENTED_EDGE('',*,*,#34734,.T.);
#46565=ORIENTED_EDGE('',*,*,#34735,.T.);
#46566=ORIENTED_EDGE('',*,*,#34731,.F.);
#46567=ORIENTED_EDGE('',*,*,#34736,.F.);
#46568=ORIENTED_EDGE('',*,*,#34729,.T.);
#46569=ORIENTED_EDGE('',*,*,#34737,.T.);
#46570=ORIENTED_EDGE('',*,*,#34734,.F.);
#46571=ORIENTED_EDGE('',*,*,#34737,.F.);
#46572=ORIENTED_EDGE('',*,*,#34728,.F.);
#46573=ORIENTED_EDGE('',*,*,#34732,.F.);
#46574=ORIENTED_EDGE('',*,*,#34735,.F.);
#46575=ORIENTED_EDGE('',*,*,#34738,.F.);
#46576=ORIENTED_EDGE('',*,*,#34739,.T.);
#46577=ORIENTED_EDGE('',*,*,#34740,.T.);
#46578=ORIENTED_EDGE('',*,*,#34741,.F.);
#46579=ORIENTED_EDGE('',*,*,#34742,.F.);
#46580=ORIENTED_EDGE('',*,*,#34743,.T.);
#46581=ORIENTED_EDGE('',*,*,#34744,.T.);
#46582=ORIENTED_EDGE('',*,*,#34739,.F.);
#46583=ORIENTED_EDGE('',*,*,#34745,.F.);
#46584=ORIENTED_EDGE('',*,*,#34746,.T.);
#46585=ORIENTED_EDGE('',*,*,#34747,.T.);
#46586=ORIENTED_EDGE('',*,*,#34743,.F.);
#46587=ORIENTED_EDGE('',*,*,#34748,.F.);
#46588=ORIENTED_EDGE('',*,*,#34741,.T.);
#46589=ORIENTED_EDGE('',*,*,#34749,.T.);
#46590=ORIENTED_EDGE('',*,*,#34746,.F.);
#46591=ORIENTED_EDGE('',*,*,#34749,.F.);
#46592=ORIENTED_EDGE('',*,*,#34740,.F.);
#46593=ORIENTED_EDGE('',*,*,#34744,.F.);
#46594=ORIENTED_EDGE('',*,*,#34747,.F.);
#46595=ORIENTED_EDGE('',*,*,#34750,.F.);
#46596=ORIENTED_EDGE('',*,*,#34751,.T.);
#46597=ORIENTED_EDGE('',*,*,#34752,.T.);
#46598=ORIENTED_EDGE('',*,*,#34753,.F.);
#46599=ORIENTED_EDGE('',*,*,#34754,.F.);
#46600=ORIENTED_EDGE('',*,*,#34755,.T.);
#46601=ORIENTED_EDGE('',*,*,#34756,.T.);
#46602=ORIENTED_EDGE('',*,*,#34751,.F.);
#46603=ORIENTED_EDGE('',*,*,#34757,.F.);
#46604=ORIENTED_EDGE('',*,*,#34758,.T.);
#46605=ORIENTED_EDGE('',*,*,#34759,.T.);
#46606=ORIENTED_EDGE('',*,*,#34755,.F.);
#46607=ORIENTED_EDGE('',*,*,#34760,.F.);
#46608=ORIENTED_EDGE('',*,*,#34753,.T.);
#46609=ORIENTED_EDGE('',*,*,#34761,.T.);
#46610=ORIENTED_EDGE('',*,*,#34758,.F.);
#46611=ORIENTED_EDGE('',*,*,#34761,.F.);
#46612=ORIENTED_EDGE('',*,*,#34752,.F.);
#46613=ORIENTED_EDGE('',*,*,#34756,.F.);
#46614=ORIENTED_EDGE('',*,*,#34759,.F.);
#46615=ORIENTED_EDGE('',*,*,#34762,.F.);
#46616=ORIENTED_EDGE('',*,*,#34763,.T.);
#46617=ORIENTED_EDGE('',*,*,#34764,.T.);
#46618=ORIENTED_EDGE('',*,*,#34765,.F.);
#46619=ORIENTED_EDGE('',*,*,#34766,.F.);
#46620=ORIENTED_EDGE('',*,*,#34767,.T.);
#46621=ORIENTED_EDGE('',*,*,#34768,.T.);
#46622=ORIENTED_EDGE('',*,*,#34763,.F.);
#46623=ORIENTED_EDGE('',*,*,#34769,.F.);
#46624=ORIENTED_EDGE('',*,*,#34770,.T.);
#46625=ORIENTED_EDGE('',*,*,#34771,.T.);
#46626=ORIENTED_EDGE('',*,*,#34767,.F.);
#46627=ORIENTED_EDGE('',*,*,#34772,.F.);
#46628=ORIENTED_EDGE('',*,*,#34765,.T.);
#46629=ORIENTED_EDGE('',*,*,#34773,.T.);
#46630=ORIENTED_EDGE('',*,*,#34770,.F.);
#46631=ORIENTED_EDGE('',*,*,#34773,.F.);
#46632=ORIENTED_EDGE('',*,*,#34764,.F.);
#46633=ORIENTED_EDGE('',*,*,#34768,.F.);
#46634=ORIENTED_EDGE('',*,*,#34771,.F.);
#46635=ORIENTED_EDGE('',*,*,#34774,.F.);
#46636=ORIENTED_EDGE('',*,*,#34775,.T.);
#46637=ORIENTED_EDGE('',*,*,#34776,.T.);
#46638=ORIENTED_EDGE('',*,*,#34777,.F.);
#46639=ORIENTED_EDGE('',*,*,#34778,.F.);
#46640=ORIENTED_EDGE('',*,*,#34779,.T.);
#46641=ORIENTED_EDGE('',*,*,#34780,.T.);
#46642=ORIENTED_EDGE('',*,*,#34775,.F.);
#46643=ORIENTED_EDGE('',*,*,#34781,.F.);
#46644=ORIENTED_EDGE('',*,*,#34782,.T.);
#46645=ORIENTED_EDGE('',*,*,#34783,.T.);
#46646=ORIENTED_EDGE('',*,*,#34779,.F.);
#46647=ORIENTED_EDGE('',*,*,#34784,.F.);
#46648=ORIENTED_EDGE('',*,*,#34777,.T.);
#46649=ORIENTED_EDGE('',*,*,#34785,.T.);
#46650=ORIENTED_EDGE('',*,*,#34782,.F.);
#46651=ORIENTED_EDGE('',*,*,#34785,.F.);
#46652=ORIENTED_EDGE('',*,*,#34776,.F.);
#46653=ORIENTED_EDGE('',*,*,#34780,.F.);
#46654=ORIENTED_EDGE('',*,*,#34783,.F.);
#46655=ORIENTED_EDGE('',*,*,#34786,.F.);
#46656=ORIENTED_EDGE('',*,*,#34787,.T.);
#46657=ORIENTED_EDGE('',*,*,#34788,.T.);
#46658=ORIENTED_EDGE('',*,*,#34789,.F.);
#46659=ORIENTED_EDGE('',*,*,#34790,.F.);
#46660=ORIENTED_EDGE('',*,*,#34791,.T.);
#46661=ORIENTED_EDGE('',*,*,#34792,.T.);
#46662=ORIENTED_EDGE('',*,*,#34787,.F.);
#46663=ORIENTED_EDGE('',*,*,#34793,.F.);
#46664=ORIENTED_EDGE('',*,*,#34794,.T.);
#46665=ORIENTED_EDGE('',*,*,#34795,.T.);
#46666=ORIENTED_EDGE('',*,*,#34791,.F.);
#46667=ORIENTED_EDGE('',*,*,#34796,.F.);
#46668=ORIENTED_EDGE('',*,*,#34789,.T.);
#46669=ORIENTED_EDGE('',*,*,#34797,.T.);
#46670=ORIENTED_EDGE('',*,*,#34794,.F.);
#46671=ORIENTED_EDGE('',*,*,#34797,.F.);
#46672=ORIENTED_EDGE('',*,*,#34788,.F.);
#46673=ORIENTED_EDGE('',*,*,#34792,.F.);
#46674=ORIENTED_EDGE('',*,*,#34795,.F.);
#46675=ORIENTED_EDGE('',*,*,#34798,.F.);
#46676=ORIENTED_EDGE('',*,*,#34799,.T.);
#46677=ORIENTED_EDGE('',*,*,#34800,.T.);
#46678=ORIENTED_EDGE('',*,*,#34801,.F.);
#46679=ORIENTED_EDGE('',*,*,#34802,.F.);
#46680=ORIENTED_EDGE('',*,*,#34803,.T.);
#46681=ORIENTED_EDGE('',*,*,#34804,.T.);
#46682=ORIENTED_EDGE('',*,*,#34799,.F.);
#46683=ORIENTED_EDGE('',*,*,#34805,.F.);
#46684=ORIENTED_EDGE('',*,*,#34806,.T.);
#46685=ORIENTED_EDGE('',*,*,#34807,.T.);
#46686=ORIENTED_EDGE('',*,*,#34803,.F.);
#46687=ORIENTED_EDGE('',*,*,#34808,.F.);
#46688=ORIENTED_EDGE('',*,*,#34801,.T.);
#46689=ORIENTED_EDGE('',*,*,#34809,.T.);
#46690=ORIENTED_EDGE('',*,*,#34806,.F.);
#46691=ORIENTED_EDGE('',*,*,#34809,.F.);
#46692=ORIENTED_EDGE('',*,*,#34800,.F.);
#46693=ORIENTED_EDGE('',*,*,#34804,.F.);
#46694=ORIENTED_EDGE('',*,*,#34807,.F.);
#46695=ORIENTED_EDGE('',*,*,#34810,.F.);
#46696=ORIENTED_EDGE('',*,*,#34811,.T.);
#46697=ORIENTED_EDGE('',*,*,#34812,.T.);
#46698=ORIENTED_EDGE('',*,*,#34813,.F.);
#46699=ORIENTED_EDGE('',*,*,#34814,.F.);
#46700=ORIENTED_EDGE('',*,*,#34815,.T.);
#46701=ORIENTED_EDGE('',*,*,#34816,.T.);
#46702=ORIENTED_EDGE('',*,*,#34811,.F.);
#46703=ORIENTED_EDGE('',*,*,#34817,.F.);
#46704=ORIENTED_EDGE('',*,*,#34818,.T.);
#46705=ORIENTED_EDGE('',*,*,#34819,.T.);
#46706=ORIENTED_EDGE('',*,*,#34815,.F.);
#46707=ORIENTED_EDGE('',*,*,#34820,.F.);
#46708=ORIENTED_EDGE('',*,*,#34813,.T.);
#46709=ORIENTED_EDGE('',*,*,#34821,.T.);
#46710=ORIENTED_EDGE('',*,*,#34818,.F.);
#46711=ORIENTED_EDGE('',*,*,#34821,.F.);
#46712=ORIENTED_EDGE('',*,*,#34812,.F.);
#46713=ORIENTED_EDGE('',*,*,#34816,.F.);
#46714=ORIENTED_EDGE('',*,*,#34819,.F.);
#46715=ORIENTED_EDGE('',*,*,#34822,.F.);
#46716=ORIENTED_EDGE('',*,*,#34823,.T.);
#46717=ORIENTED_EDGE('',*,*,#34824,.T.);
#46718=ORIENTED_EDGE('',*,*,#34825,.F.);
#46719=ORIENTED_EDGE('',*,*,#34826,.F.);
#46720=ORIENTED_EDGE('',*,*,#34827,.T.);
#46721=ORIENTED_EDGE('',*,*,#34828,.T.);
#46722=ORIENTED_EDGE('',*,*,#34823,.F.);
#46723=ORIENTED_EDGE('',*,*,#34829,.F.);
#46724=ORIENTED_EDGE('',*,*,#34830,.T.);
#46725=ORIENTED_EDGE('',*,*,#34831,.T.);
#46726=ORIENTED_EDGE('',*,*,#34827,.F.);
#46727=ORIENTED_EDGE('',*,*,#34832,.F.);
#46728=ORIENTED_EDGE('',*,*,#34825,.T.);
#46729=ORIENTED_EDGE('',*,*,#34833,.T.);
#46730=ORIENTED_EDGE('',*,*,#34830,.F.);
#46731=ORIENTED_EDGE('',*,*,#34833,.F.);
#46732=ORIENTED_EDGE('',*,*,#34824,.F.);
#46733=ORIENTED_EDGE('',*,*,#34828,.F.);
#46734=ORIENTED_EDGE('',*,*,#34831,.F.);
#46735=ORIENTED_EDGE('',*,*,#34834,.F.);
#46736=ORIENTED_EDGE('',*,*,#34835,.T.);
#46737=ORIENTED_EDGE('',*,*,#34836,.T.);
#46738=ORIENTED_EDGE('',*,*,#34837,.F.);
#46739=ORIENTED_EDGE('',*,*,#34838,.F.);
#46740=ORIENTED_EDGE('',*,*,#34839,.T.);
#46741=ORIENTED_EDGE('',*,*,#34840,.T.);
#46742=ORIENTED_EDGE('',*,*,#34835,.F.);
#46743=ORIENTED_EDGE('',*,*,#34841,.F.);
#46744=ORIENTED_EDGE('',*,*,#34842,.T.);
#46745=ORIENTED_EDGE('',*,*,#34843,.T.);
#46746=ORIENTED_EDGE('',*,*,#34839,.F.);
#46747=ORIENTED_EDGE('',*,*,#34844,.F.);
#46748=ORIENTED_EDGE('',*,*,#34837,.T.);
#46749=ORIENTED_EDGE('',*,*,#34845,.T.);
#46750=ORIENTED_EDGE('',*,*,#34842,.F.);
#46751=ORIENTED_EDGE('',*,*,#34845,.F.);
#46752=ORIENTED_EDGE('',*,*,#34836,.F.);
#46753=ORIENTED_EDGE('',*,*,#34840,.F.);
#46754=ORIENTED_EDGE('',*,*,#34843,.F.);
#46755=ORIENTED_EDGE('',*,*,#34846,.F.);
#46756=ORIENTED_EDGE('',*,*,#34847,.T.);
#46757=ORIENTED_EDGE('',*,*,#34848,.T.);
#46758=ORIENTED_EDGE('',*,*,#34849,.F.);
#46759=ORIENTED_EDGE('',*,*,#34850,.F.);
#46760=ORIENTED_EDGE('',*,*,#34851,.T.);
#46761=ORIENTED_EDGE('',*,*,#34852,.T.);
#46762=ORIENTED_EDGE('',*,*,#34847,.F.);
#46763=ORIENTED_EDGE('',*,*,#34853,.F.);
#46764=ORIENTED_EDGE('',*,*,#34854,.T.);
#46765=ORIENTED_EDGE('',*,*,#34855,.T.);
#46766=ORIENTED_EDGE('',*,*,#34851,.F.);
#46767=ORIENTED_EDGE('',*,*,#34856,.F.);
#46768=ORIENTED_EDGE('',*,*,#34849,.T.);
#46769=ORIENTED_EDGE('',*,*,#34857,.T.);
#46770=ORIENTED_EDGE('',*,*,#34854,.F.);
#46771=ORIENTED_EDGE('',*,*,#34857,.F.);
#46772=ORIENTED_EDGE('',*,*,#34848,.F.);
#46773=ORIENTED_EDGE('',*,*,#34852,.F.);
#46774=ORIENTED_EDGE('',*,*,#34855,.F.);
#46775=ORIENTED_EDGE('',*,*,#34858,.F.);
#46776=ORIENTED_EDGE('',*,*,#34859,.F.);
#46777=ORIENTED_EDGE('',*,*,#34860,.T.);
#46778=ORIENTED_EDGE('',*,*,#34861,.F.);
#46779=ORIENTED_EDGE('',*,*,#34862,.F.);
#46780=ORIENTED_EDGE('',*,*,#34863,.F.);
#46781=ORIENTED_EDGE('',*,*,#34864,.F.);
#46782=ORIENTED_EDGE('',*,*,#34865,.F.);
#46783=ORIENTED_EDGE('',*,*,#34866,.F.);
#46784=ORIENTED_EDGE('',*,*,#34867,.F.);
#46785=ORIENTED_EDGE('',*,*,#34868,.T.);
#46786=ORIENTED_EDGE('',*,*,#34869,.F.);
#46787=ORIENTED_EDGE('',*,*,#34868,.F.);
#46788=ORIENTED_EDGE('',*,*,#34870,.F.);
#46789=ORIENTED_EDGE('',*,*,#34860,.F.);
#46790=ORIENTED_EDGE('',*,*,#34871,.F.);
#46791=ORIENTED_EDGE('',*,*,#34861,.T.);
#46792=ORIENTED_EDGE('',*,*,#34870,.T.);
#46793=ORIENTED_EDGE('',*,*,#34867,.T.);
#46794=ORIENTED_EDGE('',*,*,#34872,.F.);
#46795=ORIENTED_EDGE('',*,*,#34873,.F.);
#46796=ORIENTED_EDGE('',*,*,#34874,.F.);
#46797=ORIENTED_EDGE('',*,*,#34875,.F.);
#46798=ORIENTED_EDGE('',*,*,#34876,.F.);
#46799=ORIENTED_EDGE('',*,*,#34877,.T.);
#46800=ORIENTED_EDGE('',*,*,#34878,.F.);
#46801=ORIENTED_EDGE('',*,*,#34879,.F.);
#46802=ORIENTED_EDGE('',*,*,#34880,.F.);
#46803=ORIENTED_EDGE('',*,*,#34881,.F.);
#46804=ORIENTED_EDGE('',*,*,#34882,.F.);
#46805=ORIENTED_EDGE('',*,*,#34883,.F.);
#46806=ORIENTED_EDGE('',*,*,#34884,.F.);
#46807=ORIENTED_EDGE('',*,*,#34885,.F.);
#46808=ORIENTED_EDGE('',*,*,#34886,.F.);
#46809=ORIENTED_EDGE('',*,*,#34887,.T.);
#46810=ORIENTED_EDGE('',*,*,#34888,.F.);
#46811=ORIENTED_EDGE('',*,*,#34889,.F.);
#46812=ORIENTED_EDGE('',*,*,#34890,.F.);
#46813=ORIENTED_EDGE('',*,*,#34891,.F.);
#46814=ORIENTED_EDGE('',*,*,#34892,.F.);
#46815=ORIENTED_EDGE('',*,*,#34864,.T.);
#46816=ORIENTED_EDGE('',*,*,#34893,.T.);
#46817=ORIENTED_EDGE('',*,*,#34894,.T.);
#46818=ORIENTED_EDGE('',*,*,#34895,.T.);
#46819=ORIENTED_EDGE('',*,*,#34858,.T.);
#46820=ORIENTED_EDGE('',*,*,#34896,.T.);
#46821=ORIENTED_EDGE('',*,*,#34897,.F.);
#46822=ORIENTED_EDGE('',*,*,#34898,.T.);
#46823=ORIENTED_EDGE('',*,*,#34866,.T.);
#46824=ORIENTED_EDGE('',*,*,#34899,.T.);
#46825=ORIENTED_EDGE('',*,*,#34900,.F.);
#46826=ORIENTED_EDGE('',*,*,#34872,.T.);
#46827=ORIENTED_EDGE('',*,*,#34865,.T.);
#46828=ORIENTED_EDGE('',*,*,#34895,.F.);
#46829=ORIENTED_EDGE('',*,*,#34901,.F.);
#46830=ORIENTED_EDGE('',*,*,#34899,.F.);
#46831=ORIENTED_EDGE('',*,*,#34902,.F.);
#46832=ORIENTED_EDGE('',*,*,#34903,.F.);
#46833=ORIENTED_EDGE('',*,*,#34904,.F.);
#46834=ORIENTED_EDGE('',*,*,#34905,.F.);
#46835=ORIENTED_EDGE('',*,*,#34906,.T.);
#46836=ORIENTED_EDGE('',*,*,#34906,.F.);
#46837=ORIENTED_EDGE('',*,*,#34907,.F.);
#46838=ORIENTED_EDGE('',*,*,#34908,.T.);
#46839=ORIENTED_EDGE('',*,*,#34908,.F.);
#46840=ORIENTED_EDGE('',*,*,#34909,.F.);
#46841=ORIENTED_EDGE('',*,*,#34910,.T.);
#46842=ORIENTED_EDGE('',*,*,#34907,.T.);
#46843=ORIENTED_EDGE('',*,*,#34910,.F.);
#46844=ORIENTED_EDGE('',*,*,#34911,.F.);
#46845=ORIENTED_EDGE('',*,*,#34912,.T.);
#46846=ORIENTED_EDGE('',*,*,#34905,.T.);
#46847=ORIENTED_EDGE('',*,*,#34912,.F.);
#46848=ORIENTED_EDGE('',*,*,#34913,.T.);
#46849=ORIENTED_EDGE('',*,*,#34914,.T.);
#46850=ORIENTED_EDGE('',*,*,#34915,.T.);
#46851=ORIENTED_EDGE('',*,*,#34914,.F.);
#46852=ORIENTED_EDGE('',*,*,#34915,.F.);
#46853=ORIENTED_EDGE('',*,*,#34916,.T.);
#46854=ORIENTED_EDGE('',*,*,#34917,.T.);
#46855=ORIENTED_EDGE('',*,*,#34916,.F.);
#46856=ORIENTED_EDGE('',*,*,#34918,.F.);
#46857=ORIENTED_EDGE('',*,*,#34919,.F.);
#46858=ORIENTED_EDGE('',*,*,#34920,.F.);
#46859=ORIENTED_EDGE('',*,*,#34921,.T.);
#46860=ORIENTED_EDGE('',*,*,#34922,.F.);
#46861=ORIENTED_EDGE('',*,*,#34913,.F.);
#46862=ORIENTED_EDGE('',*,*,#34917,.F.);
#46863=ORIENTED_EDGE('',*,*,#34923,.T.);
#46864=ORIENTED_EDGE('',*,*,#34923,.F.);
#46865=ORIENTED_EDGE('',*,*,#34922,.T.);
#46866=ORIENTED_EDGE('',*,*,#34924,.T.);
#46867=ORIENTED_EDGE('',*,*,#34925,.T.);
#46868=ORIENTED_EDGE('',*,*,#34924,.F.);
#46869=ORIENTED_EDGE('',*,*,#34925,.F.);
#46870=ORIENTED_EDGE('',*,*,#34926,.T.);
#46871=ORIENTED_EDGE('',*,*,#34927,.T.);
#46872=ORIENTED_EDGE('',*,*,#34926,.F.);
#46873=ORIENTED_EDGE('',*,*,#34927,.F.);
#46874=ORIENTED_EDGE('',*,*,#34928,.T.);
#46875=ORIENTED_EDGE('',*,*,#34928,.F.);
#46876=ORIENTED_EDGE('',*,*,#34929,.F.);
#46877=ORIENTED_EDGE('',*,*,#34930,.T.);
#46878=ORIENTED_EDGE('',*,*,#34931,.T.);
#46879=ORIENTED_EDGE('',*,*,#34930,.F.);
#46880=ORIENTED_EDGE('',*,*,#34931,.F.);
#46881=ORIENTED_EDGE('',*,*,#34932,.F.);
#46882=ORIENTED_EDGE('',*,*,#34933,.F.);
#46883=ORIENTED_EDGE('',*,*,#34934,.T.);
#46884=ORIENTED_EDGE('',*,*,#34935,.T.);
#46885=ORIENTED_EDGE('',*,*,#34934,.F.);
#46886=ORIENTED_EDGE('',*,*,#34935,.F.);
#46887=ORIENTED_EDGE('',*,*,#34936,.F.);
#46888=ORIENTED_EDGE('',*,*,#34937,.F.);
#46889=ORIENTED_EDGE('',*,*,#34938,.T.);
#46890=ORIENTED_EDGE('',*,*,#34939,.T.);
#46891=ORIENTED_EDGE('',*,*,#34938,.F.);
#46892=ORIENTED_EDGE('',*,*,#34939,.F.);
#46893=ORIENTED_EDGE('',*,*,#34940,.F.);
#46894=ORIENTED_EDGE('',*,*,#34941,.F.);
#46895=ORIENTED_EDGE('',*,*,#34942,.T.);
#46896=ORIENTED_EDGE('',*,*,#34943,.T.);
#46897=ORIENTED_EDGE('',*,*,#34942,.F.);
#46898=ORIENTED_EDGE('',*,*,#34943,.F.);
#46899=ORIENTED_EDGE('',*,*,#34944,.F.);
#46900=ORIENTED_EDGE('',*,*,#34945,.F.);
#46901=ORIENTED_EDGE('',*,*,#34946,.T.);
#46902=ORIENTED_EDGE('',*,*,#34947,.T.);
#46903=ORIENTED_EDGE('',*,*,#34946,.F.);
#46904=ORIENTED_EDGE('',*,*,#34947,.F.);
#46905=ORIENTED_EDGE('',*,*,#34948,.F.);
#46906=ORIENTED_EDGE('',*,*,#34949,.F.);
#46907=ORIENTED_EDGE('',*,*,#34950,.T.);
#46908=ORIENTED_EDGE('',*,*,#34951,.T.);
#46909=ORIENTED_EDGE('',*,*,#34950,.F.);
#46910=ORIENTED_EDGE('',*,*,#34951,.F.);
#46911=ORIENTED_EDGE('',*,*,#34952,.F.);
#46912=ORIENTED_EDGE('',*,*,#34904,.T.);
#46913=ORIENTED_EDGE('',*,*,#34953,.T.);
#46914=ORIENTED_EDGE('',*,*,#34954,.T.);
#46915=ORIENTED_EDGE('',*,*,#34953,.F.);
#46916=ORIENTED_EDGE('',*,*,#34863,.T.);
#46917=ORIENTED_EDGE('',*,*,#34955,.F.);
#46918=ORIENTED_EDGE('',*,*,#34956,.F.);
#46919=ORIENTED_EDGE('',*,*,#34896,.F.);
#46920=ORIENTED_EDGE('',*,*,#34957,.F.);
#46921=ORIENTED_EDGE('',*,*,#34958,.F.);
#46922=ORIENTED_EDGE('',*,*,#34959,.F.);
#46923=ORIENTED_EDGE('',*,*,#34954,.F.);
#46924=ORIENTED_EDGE('',*,*,#34960,.T.);
#46925=ORIENTED_EDGE('',*,*,#34952,.T.);
#46926=ORIENTED_EDGE('',*,*,#34960,.F.);
#46927=ORIENTED_EDGE('',*,*,#34902,.T.);
#46928=ORIENTED_EDGE('',*,*,#34961,.T.);
#46929=ORIENTED_EDGE('',*,*,#34962,.T.);
#46930=ORIENTED_EDGE('',*,*,#34961,.F.);
#46931=ORIENTED_EDGE('',*,*,#34962,.F.);
#46932=ORIENTED_EDGE('',*,*,#34963,.T.);
#46933=ORIENTED_EDGE('',*,*,#34948,.T.);
#46934=ORIENTED_EDGE('',*,*,#34963,.F.);
#46935=ORIENTED_EDGE('',*,*,#34959,.T.);
#46936=ORIENTED_EDGE('',*,*,#34964,.T.);
#46937=ORIENTED_EDGE('',*,*,#34965,.T.);
#46938=ORIENTED_EDGE('',*,*,#34964,.F.);
#46939=ORIENTED_EDGE('',*,*,#34965,.F.);
#46940=ORIENTED_EDGE('',*,*,#34966,.T.);
#46941=ORIENTED_EDGE('',*,*,#34944,.T.);
#46942=ORIENTED_EDGE('',*,*,#34966,.F.);
#46943=ORIENTED_EDGE('',*,*,#34903,.T.);
#46944=ORIENTED_EDGE('',*,*,#34967,.T.);
#46945=ORIENTED_EDGE('',*,*,#34968,.T.);
#46946=ORIENTED_EDGE('',*,*,#34967,.F.);
#46947=ORIENTED_EDGE('',*,*,#34968,.F.);
#46948=ORIENTED_EDGE('',*,*,#34969,.T.);
#46949=ORIENTED_EDGE('',*,*,#34940,.T.);
#46950=ORIENTED_EDGE('',*,*,#34969,.F.);
#46951=ORIENTED_EDGE('',*,*,#34958,.T.);
#46952=ORIENTED_EDGE('',*,*,#34970,.T.);
#46953=ORIENTED_EDGE('',*,*,#34971,.T.);
#46954=ORIENTED_EDGE('',*,*,#34970,.F.);
#46955=ORIENTED_EDGE('',*,*,#34971,.F.);
#46956=ORIENTED_EDGE('',*,*,#34972,.T.);
#46957=ORIENTED_EDGE('',*,*,#34936,.T.);
#46958=ORIENTED_EDGE('',*,*,#34972,.F.);
#46959=ORIENTED_EDGE('',*,*,#34957,.T.);
#46960=ORIENTED_EDGE('',*,*,#34973,.T.);
#46961=ORIENTED_EDGE('',*,*,#34974,.T.);
#46962=ORIENTED_EDGE('',*,*,#34973,.F.);
#46963=ORIENTED_EDGE('',*,*,#34974,.F.);
#46964=ORIENTED_EDGE('',*,*,#34975,.T.);
#46965=ORIENTED_EDGE('',*,*,#34932,.T.);
#46966=ORIENTED_EDGE('',*,*,#34975,.F.);
#46967=ORIENTED_EDGE('',*,*,#34976,.T.);
#46968=ORIENTED_EDGE('',*,*,#34977,.T.);
#46969=ORIENTED_EDGE('',*,*,#34978,.T.);
#46970=ORIENTED_EDGE('',*,*,#34979,.T.);
#46971=ORIENTED_EDGE('',*,*,#34980,.T.);
#46972=ORIENTED_EDGE('',*,*,#34981,.T.);
#46973=ORIENTED_EDGE('',*,*,#34982,.T.);
#46974=ORIENTED_EDGE('',*,*,#34979,.F.);
#46975=ORIENTED_EDGE('',*,*,#34983,.T.);
#46976=ORIENTED_EDGE('',*,*,#34984,.T.);
#46977=ORIENTED_EDGE('',*,*,#34985,.T.);
#46978=ORIENTED_EDGE('',*,*,#34981,.F.);
#46979=ORIENTED_EDGE('',*,*,#34986,.T.);
#46980=ORIENTED_EDGE('',*,*,#34987,.T.);
#46981=ORIENTED_EDGE('',*,*,#34988,.T.);
#46982=ORIENTED_EDGE('',*,*,#34989,.T.);
#46983=ORIENTED_EDGE('',*,*,#34990,.T.);
#46984=ORIENTED_EDGE('',*,*,#34991,.T.);
#46985=ORIENTED_EDGE('',*,*,#34992,.T.);
#46986=ORIENTED_EDGE('',*,*,#34987,.F.);
#46987=ORIENTED_EDGE('',*,*,#34993,.T.);
#46988=ORIENTED_EDGE('',*,*,#34994,.T.);
#46989=ORIENTED_EDGE('',*,*,#34995,.T.);
#46990=ORIENTED_EDGE('',*,*,#34991,.F.);
#46991=ORIENTED_EDGE('',*,*,#34996,.T.);
#46992=ORIENTED_EDGE('',*,*,#34997,.T.);
#46993=ORIENTED_EDGE('',*,*,#34998,.T.);
#46994=ORIENTED_EDGE('',*,*,#34994,.F.);
#46995=ORIENTED_EDGE('',*,*,#34999,.T.);
#46996=ORIENTED_EDGE('',*,*,#34989,.F.);
#46997=ORIENTED_EDGE('',*,*,#34918,.T.);
#46998=ORIENTED_EDGE('',*,*,#35000,.T.);
#46999=ORIENTED_EDGE('',*,*,#35001,.T.);
#47000=ORIENTED_EDGE('',*,*,#35000,.F.);
#47001=ORIENTED_EDGE('',*,*,#35002,.T.);
#47002=ORIENTED_EDGE('',*,*,#34984,.F.);
#47003=ORIENTED_EDGE('',*,*,#34977,.F.);
#47004=ORIENTED_EDGE('',*,*,#35003,.F.);
#47005=ORIENTED_EDGE('',*,*,#35004,.F.);
#47006=ORIENTED_EDGE('',*,*,#34877,.F.);
#47007=ORIENTED_EDGE('',*,*,#35005,.F.);
#47008=ORIENTED_EDGE('',*,*,#35006,.F.);
#47009=ORIENTED_EDGE('',*,*,#35007,.F.);
#47010=ORIENTED_EDGE('',*,*,#35008,.F.);
#47011=ORIENTED_EDGE('',*,*,#34976,.F.);
#47012=ORIENTED_EDGE('',*,*,#35009,.F.);
#47013=ORIENTED_EDGE('',*,*,#35010,.F.);
#47014=ORIENTED_EDGE('',*,*,#35003,.T.);
#47015=ORIENTED_EDGE('',*,*,#34982,.F.);
#47016=ORIENTED_EDGE('',*,*,#35011,.T.);
#47017=ORIENTED_EDGE('',*,*,#35012,.F.);
#47018=ORIENTED_EDGE('',*,*,#35009,.T.);
#47019=ORIENTED_EDGE('',*,*,#34985,.F.);
#47020=ORIENTED_EDGE('',*,*,#35013,.T.);
#47021=ORIENTED_EDGE('',*,*,#35014,.F.);
#47022=ORIENTED_EDGE('',*,*,#35011,.F.);
#47023=ORIENTED_EDGE('',*,*,#35002,.F.);
#47024=ORIENTED_EDGE('',*,*,#34921,.F.);
#47025=ORIENTED_EDGE('',*,*,#35015,.F.);
#47026=ORIENTED_EDGE('',*,*,#35013,.F.);
#47027=ORIENTED_EDGE('',*,*,#34988,.F.);
#47028=ORIENTED_EDGE('',*,*,#35016,.F.);
#47029=ORIENTED_EDGE('',*,*,#35017,.F.);
#47030=ORIENTED_EDGE('',*,*,#34919,.T.);
#47031=ORIENTED_EDGE('',*,*,#35018,.T.);
#47032=ORIENTED_EDGE('',*,*,#35019,.T.);
#47033=ORIENTED_EDGE('',*,*,#35020,.T.);
#47034=ORIENTED_EDGE('',*,*,#35021,.T.);
#47035=ORIENTED_EDGE('',*,*,#35022,.T.);
#47036=ORIENTED_EDGE('',*,*,#35023,.T.);
#47037=ORIENTED_EDGE('',*,*,#35024,.T.);
#47038=ORIENTED_EDGE('',*,*,#35021,.F.);
#47039=ORIENTED_EDGE('',*,*,#35025,.T.);
#47040=ORIENTED_EDGE('',*,*,#35026,.T.);
#47041=ORIENTED_EDGE('',*,*,#35027,.T.);
#47042=ORIENTED_EDGE('',*,*,#35023,.F.);
#47043=ORIENTED_EDGE('',*,*,#35028,.T.);
#47044=ORIENTED_EDGE('',*,*,#34897,.T.);
#47045=ORIENTED_EDGE('',*,*,#35029,.T.);
#47046=ORIENTED_EDGE('',*,*,#35026,.F.);
#47047=ORIENTED_EDGE('',*,*,#35030,.T.);
#47048=ORIENTED_EDGE('',*,*,#35031,.T.);
#47049=ORIENTED_EDGE('',*,*,#35032,.T.);
#47050=ORIENTED_EDGE('',*,*,#34894,.F.);
#47051=ORIENTED_EDGE('',*,*,#35033,.T.);
#47052=ORIENTED_EDGE('',*,*,#35034,.T.);
#47053=ORIENTED_EDGE('',*,*,#35035,.T.);
#47054=ORIENTED_EDGE('',*,*,#35031,.F.);
#47055=ORIENTED_EDGE('',*,*,#35036,.T.);
#47056=ORIENTED_EDGE('',*,*,#35037,.T.);
#47057=ORIENTED_EDGE('',*,*,#35038,.T.);
#47058=ORIENTED_EDGE('',*,*,#35034,.F.);
#47059=ORIENTED_EDGE('',*,*,#35039,.T.);
#47060=ORIENTED_EDGE('',*,*,#35007,.T.);
#47061=ORIENTED_EDGE('',*,*,#35040,.T.);
#47062=ORIENTED_EDGE('',*,*,#35037,.F.);
#47063=ORIENTED_EDGE('',*,*,#35018,.F.);
#47064=ORIENTED_EDGE('',*,*,#35041,.F.);
#47065=ORIENTED_EDGE('',*,*,#35042,.F.);
#47066=ORIENTED_EDGE('',*,*,#35043,.T.);
#47067=ORIENTED_EDGE('',*,*,#34909,.T.);
#47068=ORIENTED_EDGE('',*,*,#34941,.T.);
#47069=ORIENTED_EDGE('',*,*,#34933,.T.);
#47070=ORIENTED_EDGE('',*,*,#34929,.T.);
#47071=ORIENTED_EDGE('',*,*,#35024,.F.);
#47072=ORIENTED_EDGE('',*,*,#35044,.T.);
#47073=ORIENTED_EDGE('',*,*,#35045,.F.);
#47074=ORIENTED_EDGE('',*,*,#35041,.T.);
#47075=ORIENTED_EDGE('',*,*,#35027,.F.);
#47076=ORIENTED_EDGE('',*,*,#35046,.F.);
#47077=ORIENTED_EDGE('',*,*,#35047,.F.);
#47078=ORIENTED_EDGE('',*,*,#35044,.F.);
#47079=ORIENTED_EDGE('',*,*,#35029,.F.);
#47080=ORIENTED_EDGE('',*,*,#34956,.T.);
#47081=ORIENTED_EDGE('',*,*,#35048,.F.);
#47082=ORIENTED_EDGE('',*,*,#35046,.T.);
#47083=ORIENTED_EDGE('',*,*,#35032,.F.);
#47084=ORIENTED_EDGE('',*,*,#35049,.T.);
#47085=ORIENTED_EDGE('',*,*,#35050,.F.);
#47086=ORIENTED_EDGE('',*,*,#34901,.T.);
#47087=ORIENTED_EDGE('',*,*,#35035,.F.);
#47088=ORIENTED_EDGE('',*,*,#35051,.F.);
#47089=ORIENTED_EDGE('',*,*,#35052,.F.);
#47090=ORIENTED_EDGE('',*,*,#35049,.F.);
#47091=ORIENTED_EDGE('',*,*,#30526,.T.);
#47092=ORIENTED_EDGE('',*,*,#30560,.T.);
#47093=ORIENTED_EDGE('',*,*,#30557,.T.);
#47094=ORIENTED_EDGE('',*,*,#30554,.T.);
#47095=ORIENTED_EDGE('',*,*,#30551,.T.);
#47096=ORIENTED_EDGE('',*,*,#30548,.T.);
#47097=ORIENTED_EDGE('',*,*,#30545,.T.);
#47098=ORIENTED_EDGE('',*,*,#30542,.T.);
#47099=ORIENTED_EDGE('',*,*,#30539,.T.);
#47100=ORIENTED_EDGE('',*,*,#30536,.T.);
#47101=ORIENTED_EDGE('',*,*,#30533,.T.);
#47102=ORIENTED_EDGE('',*,*,#30530,.T.);
#47103=ORIENTED_EDGE('',*,*,#30613,.T.);
#47104=ORIENTED_EDGE('',*,*,#30659,.T.);
#47105=ORIENTED_EDGE('',*,*,#30656,.T.);
#47106=ORIENTED_EDGE('',*,*,#30653,.T.);
#47107=ORIENTED_EDGE('',*,*,#30650,.T.);
#47108=ORIENTED_EDGE('',*,*,#30647,.T.);
#47109=ORIENTED_EDGE('',*,*,#30644,.T.);
#47110=ORIENTED_EDGE('',*,*,#30641,.T.);
#47111=ORIENTED_EDGE('',*,*,#30638,.T.);
#47112=ORIENTED_EDGE('',*,*,#30635,.T.);
#47113=ORIENTED_EDGE('',*,*,#30632,.T.);
#47114=ORIENTED_EDGE('',*,*,#30629,.T.);
#47115=ORIENTED_EDGE('',*,*,#30626,.T.);
#47116=ORIENTED_EDGE('',*,*,#30623,.T.);
#47117=ORIENTED_EDGE('',*,*,#30620,.T.);
#47118=ORIENTED_EDGE('',*,*,#30617,.T.);
#47119=ORIENTED_EDGE('',*,*,#30778,.T.);
#47120=ORIENTED_EDGE('',*,*,#30812,.T.);
#47121=ORIENTED_EDGE('',*,*,#30809,.T.);
#47122=ORIENTED_EDGE('',*,*,#30806,.T.);
#47123=ORIENTED_EDGE('',*,*,#30803,.T.);
#47124=ORIENTED_EDGE('',*,*,#30800,.T.);
#47125=ORIENTED_EDGE('',*,*,#30797,.T.);
#47126=ORIENTED_EDGE('',*,*,#30794,.T.);
#47127=ORIENTED_EDGE('',*,*,#30791,.T.);
#47128=ORIENTED_EDGE('',*,*,#30788,.T.);
#47129=ORIENTED_EDGE('',*,*,#30785,.T.);
#47130=ORIENTED_EDGE('',*,*,#30782,.T.);
#47131=ORIENTED_EDGE('',*,*,#30841,.T.);
#47132=ORIENTED_EDGE('',*,*,#30896,.T.);
#47133=ORIENTED_EDGE('',*,*,#30893,.T.);
#47134=ORIENTED_EDGE('',*,*,#30890,.T.);
#47135=ORIENTED_EDGE('',*,*,#30887,.T.);
#47136=ORIENTED_EDGE('',*,*,#30884,.T.);
#47137=ORIENTED_EDGE('',*,*,#30881,.T.);
#47138=ORIENTED_EDGE('',*,*,#30878,.T.);
#47139=ORIENTED_EDGE('',*,*,#30875,.T.);
#47140=ORIENTED_EDGE('',*,*,#30872,.T.);
#47141=ORIENTED_EDGE('',*,*,#30869,.T.);
#47142=ORIENTED_EDGE('',*,*,#30866,.T.);
#47143=ORIENTED_EDGE('',*,*,#30863,.T.);
#47144=ORIENTED_EDGE('',*,*,#30860,.T.);
#47145=ORIENTED_EDGE('',*,*,#30857,.T.);
#47146=ORIENTED_EDGE('',*,*,#30854,.T.);
#47147=ORIENTED_EDGE('',*,*,#30851,.T.);
#47148=ORIENTED_EDGE('',*,*,#30848,.T.);
#47149=ORIENTED_EDGE('',*,*,#30845,.T.);
#47150=ORIENTED_EDGE('',*,*,#31048,.T.);
#47151=ORIENTED_EDGE('',*,*,#31082,.T.);
#47152=ORIENTED_EDGE('',*,*,#31079,.T.);
#47153=ORIENTED_EDGE('',*,*,#31076,.T.);
#47154=ORIENTED_EDGE('',*,*,#31073,.T.);
#47155=ORIENTED_EDGE('',*,*,#31070,.T.);
#47156=ORIENTED_EDGE('',*,*,#31067,.T.);
#47157=ORIENTED_EDGE('',*,*,#31064,.T.);
#47158=ORIENTED_EDGE('',*,*,#31061,.T.);
#47159=ORIENTED_EDGE('',*,*,#31058,.T.);
#47160=ORIENTED_EDGE('',*,*,#31055,.T.);
#47161=ORIENTED_EDGE('',*,*,#31052,.T.);
#47162=ORIENTED_EDGE('',*,*,#31093,.T.);
#47163=ORIENTED_EDGE('',*,*,#31124,.T.);
#47164=ORIENTED_EDGE('',*,*,#31121,.T.);
#47165=ORIENTED_EDGE('',*,*,#31118,.T.);
#47166=ORIENTED_EDGE('',*,*,#31115,.T.);
#47167=ORIENTED_EDGE('',*,*,#31112,.T.);
#47168=ORIENTED_EDGE('',*,*,#31109,.T.);
#47169=ORIENTED_EDGE('',*,*,#31106,.T.);
#47170=ORIENTED_EDGE('',*,*,#31103,.T.);
#47171=ORIENTED_EDGE('',*,*,#31100,.T.);
#47172=ORIENTED_EDGE('',*,*,#31097,.T.);
#47173=ORIENTED_EDGE('',*,*,#31300,.T.);
#47174=ORIENTED_EDGE('',*,*,#31334,.T.);
#47175=ORIENTED_EDGE('',*,*,#31331,.T.);
#47176=ORIENTED_EDGE('',*,*,#31328,.T.);
#47177=ORIENTED_EDGE('',*,*,#31325,.T.);
#47178=ORIENTED_EDGE('',*,*,#31322,.T.);
#47179=ORIENTED_EDGE('',*,*,#31319,.T.);
#47180=ORIENTED_EDGE('',*,*,#31316,.T.);
#47181=ORIENTED_EDGE('',*,*,#31313,.T.);
#47182=ORIENTED_EDGE('',*,*,#31310,.T.);
#47183=ORIENTED_EDGE('',*,*,#31307,.T.);
#47184=ORIENTED_EDGE('',*,*,#31304,.T.);
#47185=ORIENTED_EDGE('',*,*,#31336,.T.);
#47186=ORIENTED_EDGE('',*,*,#31400,.T.);
#47187=ORIENTED_EDGE('',*,*,#31397,.T.);
#47188=ORIENTED_EDGE('',*,*,#31394,.T.);
#47189=ORIENTED_EDGE('',*,*,#31391,.T.);
#47190=ORIENTED_EDGE('',*,*,#31388,.T.);
#47191=ORIENTED_EDGE('',*,*,#31385,.T.);
#47192=ORIENTED_EDGE('',*,*,#31382,.T.);
#47193=ORIENTED_EDGE('',*,*,#31379,.T.);
#47194=ORIENTED_EDGE('',*,*,#31376,.T.);
#47195=ORIENTED_EDGE('',*,*,#31373,.T.);
#47196=ORIENTED_EDGE('',*,*,#31370,.T.);
#47197=ORIENTED_EDGE('',*,*,#31367,.T.);
#47198=ORIENTED_EDGE('',*,*,#31364,.T.);
#47199=ORIENTED_EDGE('',*,*,#31361,.T.);
#47200=ORIENTED_EDGE('',*,*,#31358,.T.);
#47201=ORIENTED_EDGE('',*,*,#31355,.T.);
#47202=ORIENTED_EDGE('',*,*,#31352,.T.);
#47203=ORIENTED_EDGE('',*,*,#31349,.T.);
#47204=ORIENTED_EDGE('',*,*,#31346,.T.);
#47205=ORIENTED_EDGE('',*,*,#31343,.T.);
#47206=ORIENTED_EDGE('',*,*,#31340,.T.);
#47207=ORIENTED_EDGE('',*,*,#31513,.T.);
#47208=ORIENTED_EDGE('',*,*,#31547,.T.);
#47209=ORIENTED_EDGE('',*,*,#31544,.T.);
#47210=ORIENTED_EDGE('',*,*,#31541,.T.);
#47211=ORIENTED_EDGE('',*,*,#31538,.T.);
#47212=ORIENTED_EDGE('',*,*,#31535,.T.);
#47213=ORIENTED_EDGE('',*,*,#31532,.T.);
#47214=ORIENTED_EDGE('',*,*,#31529,.T.);
#47215=ORIENTED_EDGE('',*,*,#31526,.T.);
#47216=ORIENTED_EDGE('',*,*,#31523,.T.);
#47217=ORIENTED_EDGE('',*,*,#31520,.T.);
#47218=ORIENTED_EDGE('',*,*,#31517,.T.);
#47219=ORIENTED_EDGE('',*,*,#31660,.T.);
#47220=ORIENTED_EDGE('',*,*,#31694,.T.);
#47221=ORIENTED_EDGE('',*,*,#31691,.T.);
#47222=ORIENTED_EDGE('',*,*,#31688,.T.);
#47223=ORIENTED_EDGE('',*,*,#31685,.T.);
#47224=ORIENTED_EDGE('',*,*,#31682,.T.);
#47225=ORIENTED_EDGE('',*,*,#31679,.T.);
#47226=ORIENTED_EDGE('',*,*,#31676,.T.);
#47227=ORIENTED_EDGE('',*,*,#31673,.T.);
#47228=ORIENTED_EDGE('',*,*,#31670,.T.);
#47229=ORIENTED_EDGE('',*,*,#31667,.T.);
#47230=ORIENTED_EDGE('',*,*,#31664,.T.);
#47231=ORIENTED_EDGE('',*,*,#31696,.T.);
#47232=ORIENTED_EDGE('',*,*,#31760,.T.);
#47233=ORIENTED_EDGE('',*,*,#31757,.T.);
#47234=ORIENTED_EDGE('',*,*,#31754,.T.);
#47235=ORIENTED_EDGE('',*,*,#31751,.T.);
#47236=ORIENTED_EDGE('',*,*,#31748,.T.);
#47237=ORIENTED_EDGE('',*,*,#31745,.T.);
#47238=ORIENTED_EDGE('',*,*,#31742,.T.);
#47239=ORIENTED_EDGE('',*,*,#31739,.T.);
#47240=ORIENTED_EDGE('',*,*,#31736,.T.);
#47241=ORIENTED_EDGE('',*,*,#31733,.T.);
#47242=ORIENTED_EDGE('',*,*,#31730,.T.);
#47243=ORIENTED_EDGE('',*,*,#31727,.T.);
#47244=ORIENTED_EDGE('',*,*,#31724,.T.);
#47245=ORIENTED_EDGE('',*,*,#31721,.T.);
#47246=ORIENTED_EDGE('',*,*,#31718,.T.);
#47247=ORIENTED_EDGE('',*,*,#31715,.T.);
#47248=ORIENTED_EDGE('',*,*,#31712,.T.);
#47249=ORIENTED_EDGE('',*,*,#31709,.T.);
#47250=ORIENTED_EDGE('',*,*,#31706,.T.);
#47251=ORIENTED_EDGE('',*,*,#31703,.T.);
#47252=ORIENTED_EDGE('',*,*,#31700,.T.);
#47253=ORIENTED_EDGE('',*,*,#31936,.T.);
#47254=ORIENTED_EDGE('',*,*,#31970,.T.);
#47255=ORIENTED_EDGE('',*,*,#31967,.T.);
#47256=ORIENTED_EDGE('',*,*,#31964,.T.);
#47257=ORIENTED_EDGE('',*,*,#31961,.T.);
#47258=ORIENTED_EDGE('',*,*,#31958,.T.);
#47259=ORIENTED_EDGE('',*,*,#31955,.T.);
#47260=ORIENTED_EDGE('',*,*,#31952,.T.);
#47261=ORIENTED_EDGE('',*,*,#31949,.T.);
#47262=ORIENTED_EDGE('',*,*,#31946,.T.);
#47263=ORIENTED_EDGE('',*,*,#31943,.T.);
#47264=ORIENTED_EDGE('',*,*,#31940,.T.);
#47265=ORIENTED_EDGE('',*,*,#31981,.T.);
#47266=ORIENTED_EDGE('',*,*,#32012,.T.);
#47267=ORIENTED_EDGE('',*,*,#32009,.T.);
#47268=ORIENTED_EDGE('',*,*,#32006,.T.);
#47269=ORIENTED_EDGE('',*,*,#32003,.T.);
#47270=ORIENTED_EDGE('',*,*,#32000,.T.);
#47271=ORIENTED_EDGE('',*,*,#31997,.T.);
#47272=ORIENTED_EDGE('',*,*,#31994,.T.);
#47273=ORIENTED_EDGE('',*,*,#31991,.T.);
#47274=ORIENTED_EDGE('',*,*,#31988,.T.);
#47275=ORIENTED_EDGE('',*,*,#31985,.T.);
#47276=ORIENTED_EDGE('',*,*,#32164,.T.);
#47277=ORIENTED_EDGE('',*,*,#32198,.T.);
#47278=ORIENTED_EDGE('',*,*,#32195,.T.);
#47279=ORIENTED_EDGE('',*,*,#32192,.T.);
#47280=ORIENTED_EDGE('',*,*,#32189,.T.);
#47281=ORIENTED_EDGE('',*,*,#32186,.T.);
#47282=ORIENTED_EDGE('',*,*,#32183,.T.);
#47283=ORIENTED_EDGE('',*,*,#32180,.T.);
#47284=ORIENTED_EDGE('',*,*,#32177,.T.);
#47285=ORIENTED_EDGE('',*,*,#32174,.T.);
#47286=ORIENTED_EDGE('',*,*,#32171,.T.);
#47287=ORIENTED_EDGE('',*,*,#32168,.T.);
#47288=ORIENTED_EDGE('',*,*,#32227,.T.);
#47289=ORIENTED_EDGE('',*,*,#32282,.T.);
#47290=ORIENTED_EDGE('',*,*,#32279,.T.);
#47291=ORIENTED_EDGE('',*,*,#32276,.T.);
#47292=ORIENTED_EDGE('',*,*,#32273,.T.);
#47293=ORIENTED_EDGE('',*,*,#32270,.T.);
#47294=ORIENTED_EDGE('',*,*,#32267,.T.);
#47295=ORIENTED_EDGE('',*,*,#32264,.T.);
#47296=ORIENTED_EDGE('',*,*,#32261,.T.);
#47297=ORIENTED_EDGE('',*,*,#32258,.T.);
#47298=ORIENTED_EDGE('',*,*,#32255,.T.);
#47299=ORIENTED_EDGE('',*,*,#32252,.T.);
#47300=ORIENTED_EDGE('',*,*,#32249,.T.);
#47301=ORIENTED_EDGE('',*,*,#32246,.T.);
#47302=ORIENTED_EDGE('',*,*,#32243,.T.);
#47303=ORIENTED_EDGE('',*,*,#32240,.T.);
#47304=ORIENTED_EDGE('',*,*,#32237,.T.);
#47305=ORIENTED_EDGE('',*,*,#32234,.T.);
#47306=ORIENTED_EDGE('',*,*,#32231,.T.);
#47307=ORIENTED_EDGE('',*,*,#32401,.T.);
#47308=ORIENTED_EDGE('',*,*,#32435,.T.);
#47309=ORIENTED_EDGE('',*,*,#32432,.T.);
#47310=ORIENTED_EDGE('',*,*,#32429,.T.);
#47311=ORIENTED_EDGE('',*,*,#32426,.T.);
#47312=ORIENTED_EDGE('',*,*,#32423,.T.);
#47313=ORIENTED_EDGE('',*,*,#32420,.T.);
#47314=ORIENTED_EDGE('',*,*,#32417,.T.);
#47315=ORIENTED_EDGE('',*,*,#32414,.T.);
#47316=ORIENTED_EDGE('',*,*,#32411,.T.);
#47317=ORIENTED_EDGE('',*,*,#32408,.T.);
#47318=ORIENTED_EDGE('',*,*,#32405,.T.);
#47319=ORIENTED_EDGE('',*,*,#32488,.T.);
#47320=ORIENTED_EDGE('',*,*,#32534,.T.);
#47321=ORIENTED_EDGE('',*,*,#32531,.T.);
#47322=ORIENTED_EDGE('',*,*,#32528,.T.);
#47323=ORIENTED_EDGE('',*,*,#32525,.T.);
#47324=ORIENTED_EDGE('',*,*,#32522,.T.);
#47325=ORIENTED_EDGE('',*,*,#32519,.T.);
#47326=ORIENTED_EDGE('',*,*,#32516,.T.);
#47327=ORIENTED_EDGE('',*,*,#32513,.T.);
#47328=ORIENTED_EDGE('',*,*,#32510,.T.);
#47329=ORIENTED_EDGE('',*,*,#32507,.T.);
#47330=ORIENTED_EDGE('',*,*,#32504,.T.);
#47331=ORIENTED_EDGE('',*,*,#32501,.T.);
#47332=ORIENTED_EDGE('',*,*,#32498,.T.);
#47333=ORIENTED_EDGE('',*,*,#32495,.T.);
#47334=ORIENTED_EDGE('',*,*,#32492,.T.);
#47335=ORIENTED_EDGE('',*,*,#32686,.T.);
#47336=ORIENTED_EDGE('',*,*,#32696,.T.);
#47337=ORIENTED_EDGE('',*,*,#32693,.T.);
#47338=ORIENTED_EDGE('',*,*,#32690,.T.);
#47339=ORIENTED_EDGE('',*,*,#32698,.T.);
#47340=ORIENTED_EDGE('',*,*,#32708,.T.);
#47341=ORIENTED_EDGE('',*,*,#32705,.T.);
#47342=ORIENTED_EDGE('',*,*,#32702,.T.);
#47343=ORIENTED_EDGE('',*,*,#32710,.T.);
#47344=ORIENTED_EDGE('',*,*,#32720,.T.);
#47345=ORIENTED_EDGE('',*,*,#32717,.T.);
#47346=ORIENTED_EDGE('',*,*,#32714,.T.);
#47347=ORIENTED_EDGE('',*,*,#32722,.T.);
#47348=ORIENTED_EDGE('',*,*,#32732,.T.);
#47349=ORIENTED_EDGE('',*,*,#32729,.T.);
#47350=ORIENTED_EDGE('',*,*,#32726,.T.);
#47351=ORIENTED_EDGE('',*,*,#32734,.T.);
#47352=ORIENTED_EDGE('',*,*,#32744,.T.);
#47353=ORIENTED_EDGE('',*,*,#32741,.T.);
#47354=ORIENTED_EDGE('',*,*,#32738,.T.);
#47355=ORIENTED_EDGE('',*,*,#32746,.T.);
#47356=ORIENTED_EDGE('',*,*,#32756,.T.);
#47357=ORIENTED_EDGE('',*,*,#32753,.T.);
#47358=ORIENTED_EDGE('',*,*,#32750,.T.);
#47359=ORIENTED_EDGE('',*,*,#32758,.T.);
#47360=ORIENTED_EDGE('',*,*,#32768,.T.);
#47361=ORIENTED_EDGE('',*,*,#32765,.T.);
#47362=ORIENTED_EDGE('',*,*,#32762,.T.);
#47363=ORIENTED_EDGE('',*,*,#32770,.T.);
#47364=ORIENTED_EDGE('',*,*,#32780,.T.);
#47365=ORIENTED_EDGE('',*,*,#32777,.T.);
#47366=ORIENTED_EDGE('',*,*,#32774,.T.);
#47367=ORIENTED_EDGE('',*,*,#32782,.T.);
#47368=ORIENTED_EDGE('',*,*,#32792,.T.);
#47369=ORIENTED_EDGE('',*,*,#32789,.T.);
#47370=ORIENTED_EDGE('',*,*,#32786,.T.);
#47371=ORIENTED_EDGE('',*,*,#32794,.T.);
#47372=ORIENTED_EDGE('',*,*,#32804,.T.);
#47373=ORIENTED_EDGE('',*,*,#32801,.T.);
#47374=ORIENTED_EDGE('',*,*,#32798,.T.);
#47375=ORIENTED_EDGE('',*,*,#32806,.T.);
#47376=ORIENTED_EDGE('',*,*,#32816,.T.);
#47377=ORIENTED_EDGE('',*,*,#32813,.T.);
#47378=ORIENTED_EDGE('',*,*,#32810,.T.);
#47379=ORIENTED_EDGE('',*,*,#32818,.T.);
#47380=ORIENTED_EDGE('',*,*,#32828,.T.);
#47381=ORIENTED_EDGE('',*,*,#32825,.T.);
#47382=ORIENTED_EDGE('',*,*,#32822,.T.);
#47383=ORIENTED_EDGE('',*,*,#32830,.T.);
#47384=ORIENTED_EDGE('',*,*,#32840,.T.);
#47385=ORIENTED_EDGE('',*,*,#32837,.T.);
#47386=ORIENTED_EDGE('',*,*,#32834,.T.);
#47387=ORIENTED_EDGE('',*,*,#32842,.T.);
#47388=ORIENTED_EDGE('',*,*,#32852,.T.);
#47389=ORIENTED_EDGE('',*,*,#32849,.T.);
#47390=ORIENTED_EDGE('',*,*,#32846,.T.);
#47391=ORIENTED_EDGE('',*,*,#32854,.T.);
#47392=ORIENTED_EDGE('',*,*,#32864,.T.);
#47393=ORIENTED_EDGE('',*,*,#32861,.T.);
#47394=ORIENTED_EDGE('',*,*,#32858,.T.);
#47395=ORIENTED_EDGE('',*,*,#32866,.T.);
#47396=ORIENTED_EDGE('',*,*,#32876,.T.);
#47397=ORIENTED_EDGE('',*,*,#32873,.T.);
#47398=ORIENTED_EDGE('',*,*,#32870,.T.);
#47399=ORIENTED_EDGE('',*,*,#32878,.T.);
#47400=ORIENTED_EDGE('',*,*,#32888,.T.);
#47401=ORIENTED_EDGE('',*,*,#32885,.T.);
#47402=ORIENTED_EDGE('',*,*,#32882,.T.);
#47403=ORIENTED_EDGE('',*,*,#32890,.T.);
#47404=ORIENTED_EDGE('',*,*,#32900,.T.);
#47405=ORIENTED_EDGE('',*,*,#32897,.T.);
#47406=ORIENTED_EDGE('',*,*,#32894,.T.);
#47407=ORIENTED_EDGE('',*,*,#32902,.T.);
#47408=ORIENTED_EDGE('',*,*,#32912,.T.);
#47409=ORIENTED_EDGE('',*,*,#32909,.T.);
#47410=ORIENTED_EDGE('',*,*,#32906,.T.);
#47411=ORIENTED_EDGE('',*,*,#32914,.T.);
#47412=ORIENTED_EDGE('',*,*,#32924,.T.);
#47413=ORIENTED_EDGE('',*,*,#32921,.T.);
#47414=ORIENTED_EDGE('',*,*,#32918,.T.);
#47415=ORIENTED_EDGE('',*,*,#32926,.T.);
#47416=ORIENTED_EDGE('',*,*,#32936,.T.);
#47417=ORIENTED_EDGE('',*,*,#32933,.T.);
#47418=ORIENTED_EDGE('',*,*,#32930,.T.);
#47419=ORIENTED_EDGE('',*,*,#32938,.T.);
#47420=ORIENTED_EDGE('',*,*,#32948,.T.);
#47421=ORIENTED_EDGE('',*,*,#32945,.T.);
#47422=ORIENTED_EDGE('',*,*,#32942,.T.);
#47423=ORIENTED_EDGE('',*,*,#32950,.T.);
#47424=ORIENTED_EDGE('',*,*,#32960,.T.);
#47425=ORIENTED_EDGE('',*,*,#32957,.T.);
#47426=ORIENTED_EDGE('',*,*,#32954,.T.);
#47427=ORIENTED_EDGE('',*,*,#32962,.T.);
#47428=ORIENTED_EDGE('',*,*,#32972,.T.);
#47429=ORIENTED_EDGE('',*,*,#32969,.T.);
#47430=ORIENTED_EDGE('',*,*,#32966,.T.);
#47431=ORIENTED_EDGE('',*,*,#32974,.T.);
#47432=ORIENTED_EDGE('',*,*,#32984,.T.);
#47433=ORIENTED_EDGE('',*,*,#32981,.T.);
#47434=ORIENTED_EDGE('',*,*,#32978,.T.);
#47435=ORIENTED_EDGE('',*,*,#32986,.T.);
#47436=ORIENTED_EDGE('',*,*,#32996,.T.);
#47437=ORIENTED_EDGE('',*,*,#32993,.T.);
#47438=ORIENTED_EDGE('',*,*,#32990,.T.);
#47439=ORIENTED_EDGE('',*,*,#32998,.T.);
#47440=ORIENTED_EDGE('',*,*,#33008,.T.);
#47441=ORIENTED_EDGE('',*,*,#33005,.T.);
#47442=ORIENTED_EDGE('',*,*,#33002,.T.);
#47443=ORIENTED_EDGE('',*,*,#33010,.T.);
#47444=ORIENTED_EDGE('',*,*,#33020,.T.);
#47445=ORIENTED_EDGE('',*,*,#33017,.T.);
#47446=ORIENTED_EDGE('',*,*,#33014,.T.);
#47447=ORIENTED_EDGE('',*,*,#33022,.T.);
#47448=ORIENTED_EDGE('',*,*,#33032,.T.);
#47449=ORIENTED_EDGE('',*,*,#33029,.T.);
#47450=ORIENTED_EDGE('',*,*,#33026,.T.);
#47451=ORIENTED_EDGE('',*,*,#33034,.T.);
#47452=ORIENTED_EDGE('',*,*,#33044,.T.);
#47453=ORIENTED_EDGE('',*,*,#33041,.T.);
#47454=ORIENTED_EDGE('',*,*,#33038,.T.);
#47455=ORIENTED_EDGE('',*,*,#33046,.T.);
#47456=ORIENTED_EDGE('',*,*,#33056,.T.);
#47457=ORIENTED_EDGE('',*,*,#33053,.T.);
#47458=ORIENTED_EDGE('',*,*,#33050,.T.);
#47459=ORIENTED_EDGE('',*,*,#33058,.T.);
#47460=ORIENTED_EDGE('',*,*,#33068,.T.);
#47461=ORIENTED_EDGE('',*,*,#33065,.T.);
#47462=ORIENTED_EDGE('',*,*,#33062,.T.);
#47463=ORIENTED_EDGE('',*,*,#33070,.T.);
#47464=ORIENTED_EDGE('',*,*,#33080,.T.);
#47465=ORIENTED_EDGE('',*,*,#33077,.T.);
#47466=ORIENTED_EDGE('',*,*,#33074,.T.);
#47467=ORIENTED_EDGE('',*,*,#33082,.T.);
#47468=ORIENTED_EDGE('',*,*,#33092,.T.);
#47469=ORIENTED_EDGE('',*,*,#33089,.T.);
#47470=ORIENTED_EDGE('',*,*,#33086,.T.);
#47471=ORIENTED_EDGE('',*,*,#33094,.T.);
#47472=ORIENTED_EDGE('',*,*,#33104,.T.);
#47473=ORIENTED_EDGE('',*,*,#33101,.T.);
#47474=ORIENTED_EDGE('',*,*,#33098,.T.);
#47475=ORIENTED_EDGE('',*,*,#33106,.T.);
#47476=ORIENTED_EDGE('',*,*,#33116,.T.);
#47477=ORIENTED_EDGE('',*,*,#33113,.T.);
#47478=ORIENTED_EDGE('',*,*,#33110,.T.);
#47479=ORIENTED_EDGE('',*,*,#33118,.T.);
#47480=ORIENTED_EDGE('',*,*,#33128,.T.);
#47481=ORIENTED_EDGE('',*,*,#33125,.T.);
#47482=ORIENTED_EDGE('',*,*,#33122,.T.);
#47483=ORIENTED_EDGE('',*,*,#33130,.T.);
#47484=ORIENTED_EDGE('',*,*,#33140,.T.);
#47485=ORIENTED_EDGE('',*,*,#33137,.T.);
#47486=ORIENTED_EDGE('',*,*,#33134,.T.);
#47487=ORIENTED_EDGE('',*,*,#33142,.T.);
#47488=ORIENTED_EDGE('',*,*,#33152,.T.);
#47489=ORIENTED_EDGE('',*,*,#33149,.T.);
#47490=ORIENTED_EDGE('',*,*,#33146,.T.);
#47491=ORIENTED_EDGE('',*,*,#33154,.T.);
#47492=ORIENTED_EDGE('',*,*,#33164,.T.);
#47493=ORIENTED_EDGE('',*,*,#33161,.T.);
#47494=ORIENTED_EDGE('',*,*,#33158,.T.);
#47495=ORIENTED_EDGE('',*,*,#33166,.T.);
#47496=ORIENTED_EDGE('',*,*,#33176,.T.);
#47497=ORIENTED_EDGE('',*,*,#33173,.T.);
#47498=ORIENTED_EDGE('',*,*,#33170,.T.);
#47499=ORIENTED_EDGE('',*,*,#33178,.T.);
#47500=ORIENTED_EDGE('',*,*,#33188,.T.);
#47501=ORIENTED_EDGE('',*,*,#33185,.T.);
#47502=ORIENTED_EDGE('',*,*,#33182,.T.);
#47503=ORIENTED_EDGE('',*,*,#33190,.T.);
#47504=ORIENTED_EDGE('',*,*,#33200,.T.);
#47505=ORIENTED_EDGE('',*,*,#33197,.T.);
#47506=ORIENTED_EDGE('',*,*,#33194,.T.);
#47507=ORIENTED_EDGE('',*,*,#33202,.T.);
#47508=ORIENTED_EDGE('',*,*,#33212,.T.);
#47509=ORIENTED_EDGE('',*,*,#33209,.T.);
#47510=ORIENTED_EDGE('',*,*,#33206,.T.);
#47511=ORIENTED_EDGE('',*,*,#33214,.T.);
#47512=ORIENTED_EDGE('',*,*,#33224,.T.);
#47513=ORIENTED_EDGE('',*,*,#33221,.T.);
#47514=ORIENTED_EDGE('',*,*,#33218,.T.);
#47515=ORIENTED_EDGE('',*,*,#33226,.T.);
#47516=ORIENTED_EDGE('',*,*,#33236,.T.);
#47517=ORIENTED_EDGE('',*,*,#33233,.T.);
#47518=ORIENTED_EDGE('',*,*,#33230,.T.);
#47519=ORIENTED_EDGE('',*,*,#33238,.T.);
#47520=ORIENTED_EDGE('',*,*,#33248,.T.);
#47521=ORIENTED_EDGE('',*,*,#33245,.T.);
#47522=ORIENTED_EDGE('',*,*,#33242,.T.);
#47523=ORIENTED_EDGE('',*,*,#33250,.T.);
#47524=ORIENTED_EDGE('',*,*,#33260,.T.);
#47525=ORIENTED_EDGE('',*,*,#33257,.T.);
#47526=ORIENTED_EDGE('',*,*,#33254,.T.);
#47527=ORIENTED_EDGE('',*,*,#33262,.T.);
#47528=ORIENTED_EDGE('',*,*,#33272,.T.);
#47529=ORIENTED_EDGE('',*,*,#33269,.T.);
#47530=ORIENTED_EDGE('',*,*,#33266,.T.);
#47531=ORIENTED_EDGE('',*,*,#33274,.T.);
#47532=ORIENTED_EDGE('',*,*,#33284,.T.);
#47533=ORIENTED_EDGE('',*,*,#33281,.T.);
#47534=ORIENTED_EDGE('',*,*,#33278,.T.);
#47535=ORIENTED_EDGE('',*,*,#33286,.T.);
#47536=ORIENTED_EDGE('',*,*,#33296,.T.);
#47537=ORIENTED_EDGE('',*,*,#33293,.T.);
#47538=ORIENTED_EDGE('',*,*,#33290,.T.);
#47539=ORIENTED_EDGE('',*,*,#33298,.T.);
#47540=ORIENTED_EDGE('',*,*,#33308,.T.);
#47541=ORIENTED_EDGE('',*,*,#33305,.T.);
#47542=ORIENTED_EDGE('',*,*,#33302,.T.);
#47543=ORIENTED_EDGE('',*,*,#33310,.T.);
#47544=ORIENTED_EDGE('',*,*,#33320,.T.);
#47545=ORIENTED_EDGE('',*,*,#33317,.T.);
#47546=ORIENTED_EDGE('',*,*,#33314,.T.);
#47547=ORIENTED_EDGE('',*,*,#33322,.T.);
#47548=ORIENTED_EDGE('',*,*,#33332,.T.);
#47549=ORIENTED_EDGE('',*,*,#33329,.T.);
#47550=ORIENTED_EDGE('',*,*,#33326,.T.);
#47551=ORIENTED_EDGE('',*,*,#33334,.T.);
#47552=ORIENTED_EDGE('',*,*,#33344,.T.);
#47553=ORIENTED_EDGE('',*,*,#33341,.T.);
#47554=ORIENTED_EDGE('',*,*,#33338,.T.);
#47555=ORIENTED_EDGE('',*,*,#33346,.T.);
#47556=ORIENTED_EDGE('',*,*,#33356,.T.);
#47557=ORIENTED_EDGE('',*,*,#33353,.T.);
#47558=ORIENTED_EDGE('',*,*,#33350,.T.);
#47559=ORIENTED_EDGE('',*,*,#33358,.T.);
#47560=ORIENTED_EDGE('',*,*,#33368,.T.);
#47561=ORIENTED_EDGE('',*,*,#33365,.T.);
#47562=ORIENTED_EDGE('',*,*,#33362,.T.);
#47563=ORIENTED_EDGE('',*,*,#33370,.T.);
#47564=ORIENTED_EDGE('',*,*,#33380,.T.);
#47565=ORIENTED_EDGE('',*,*,#33377,.T.);
#47566=ORIENTED_EDGE('',*,*,#33374,.T.);
#47567=ORIENTED_EDGE('',*,*,#33382,.T.);
#47568=ORIENTED_EDGE('',*,*,#33392,.T.);
#47569=ORIENTED_EDGE('',*,*,#33389,.T.);
#47570=ORIENTED_EDGE('',*,*,#33386,.T.);
#47571=ORIENTED_EDGE('',*,*,#33394,.T.);
#47572=ORIENTED_EDGE('',*,*,#33404,.T.);
#47573=ORIENTED_EDGE('',*,*,#33401,.T.);
#47574=ORIENTED_EDGE('',*,*,#33398,.T.);
#47575=ORIENTED_EDGE('',*,*,#33406,.T.);
#47576=ORIENTED_EDGE('',*,*,#33416,.T.);
#47577=ORIENTED_EDGE('',*,*,#33413,.T.);
#47578=ORIENTED_EDGE('',*,*,#33410,.T.);
#47579=ORIENTED_EDGE('',*,*,#33418,.T.);
#47580=ORIENTED_EDGE('',*,*,#33428,.T.);
#47581=ORIENTED_EDGE('',*,*,#33425,.T.);
#47582=ORIENTED_EDGE('',*,*,#33422,.T.);
#47583=ORIENTED_EDGE('',*,*,#33430,.T.);
#47584=ORIENTED_EDGE('',*,*,#33440,.T.);
#47585=ORIENTED_EDGE('',*,*,#33437,.T.);
#47586=ORIENTED_EDGE('',*,*,#33434,.T.);
#47587=ORIENTED_EDGE('',*,*,#33442,.T.);
#47588=ORIENTED_EDGE('',*,*,#33452,.T.);
#47589=ORIENTED_EDGE('',*,*,#33449,.T.);
#47590=ORIENTED_EDGE('',*,*,#33446,.T.);
#47591=ORIENTED_EDGE('',*,*,#33454,.T.);
#47592=ORIENTED_EDGE('',*,*,#33464,.T.);
#47593=ORIENTED_EDGE('',*,*,#33461,.T.);
#47594=ORIENTED_EDGE('',*,*,#33458,.T.);
#47595=ORIENTED_EDGE('',*,*,#33466,.T.);
#47596=ORIENTED_EDGE('',*,*,#33476,.T.);
#47597=ORIENTED_EDGE('',*,*,#33473,.T.);
#47598=ORIENTED_EDGE('',*,*,#33470,.T.);
#47599=ORIENTED_EDGE('',*,*,#33478,.T.);
#47600=ORIENTED_EDGE('',*,*,#33488,.T.);
#47601=ORIENTED_EDGE('',*,*,#33485,.T.);
#47602=ORIENTED_EDGE('',*,*,#33482,.T.);
#47603=ORIENTED_EDGE('',*,*,#33490,.T.);
#47604=ORIENTED_EDGE('',*,*,#33500,.T.);
#47605=ORIENTED_EDGE('',*,*,#33497,.T.);
#47606=ORIENTED_EDGE('',*,*,#33494,.T.);
#47607=ORIENTED_EDGE('',*,*,#33502,.T.);
#47608=ORIENTED_EDGE('',*,*,#33512,.T.);
#47609=ORIENTED_EDGE('',*,*,#33509,.T.);
#47610=ORIENTED_EDGE('',*,*,#33506,.T.);
#47611=ORIENTED_EDGE('',*,*,#33514,.T.);
#47612=ORIENTED_EDGE('',*,*,#33524,.T.);
#47613=ORIENTED_EDGE('',*,*,#33521,.T.);
#47614=ORIENTED_EDGE('',*,*,#33518,.T.);
#47615=ORIENTED_EDGE('',*,*,#33526,.T.);
#47616=ORIENTED_EDGE('',*,*,#33536,.T.);
#47617=ORIENTED_EDGE('',*,*,#33533,.T.);
#47618=ORIENTED_EDGE('',*,*,#33530,.T.);
#47619=ORIENTED_EDGE('',*,*,#33538,.T.);
#47620=ORIENTED_EDGE('',*,*,#33548,.T.);
#47621=ORIENTED_EDGE('',*,*,#33545,.T.);
#47622=ORIENTED_EDGE('',*,*,#33542,.T.);
#47623=ORIENTED_EDGE('',*,*,#33550,.T.);
#47624=ORIENTED_EDGE('',*,*,#33560,.T.);
#47625=ORIENTED_EDGE('',*,*,#33557,.T.);
#47626=ORIENTED_EDGE('',*,*,#33554,.T.);
#47627=ORIENTED_EDGE('',*,*,#33562,.T.);
#47628=ORIENTED_EDGE('',*,*,#33572,.T.);
#47629=ORIENTED_EDGE('',*,*,#33569,.T.);
#47630=ORIENTED_EDGE('',*,*,#33566,.T.);
#47631=ORIENTED_EDGE('',*,*,#33574,.T.);
#47632=ORIENTED_EDGE('',*,*,#33584,.T.);
#47633=ORIENTED_EDGE('',*,*,#33581,.T.);
#47634=ORIENTED_EDGE('',*,*,#33578,.T.);
#47635=ORIENTED_EDGE('',*,*,#33586,.T.);
#47636=ORIENTED_EDGE('',*,*,#33596,.T.);
#47637=ORIENTED_EDGE('',*,*,#33593,.T.);
#47638=ORIENTED_EDGE('',*,*,#33590,.T.);
#47639=ORIENTED_EDGE('',*,*,#33598,.T.);
#47640=ORIENTED_EDGE('',*,*,#33608,.T.);
#47641=ORIENTED_EDGE('',*,*,#33605,.T.);
#47642=ORIENTED_EDGE('',*,*,#33602,.T.);
#47643=ORIENTED_EDGE('',*,*,#33610,.T.);
#47644=ORIENTED_EDGE('',*,*,#33620,.T.);
#47645=ORIENTED_EDGE('',*,*,#33617,.T.);
#47646=ORIENTED_EDGE('',*,*,#33614,.T.);
#47647=ORIENTED_EDGE('',*,*,#33622,.T.);
#47648=ORIENTED_EDGE('',*,*,#33632,.T.);
#47649=ORIENTED_EDGE('',*,*,#33629,.T.);
#47650=ORIENTED_EDGE('',*,*,#33626,.T.);
#47651=ORIENTED_EDGE('',*,*,#33634,.T.);
#47652=ORIENTED_EDGE('',*,*,#33644,.T.);
#47653=ORIENTED_EDGE('',*,*,#33641,.T.);
#47654=ORIENTED_EDGE('',*,*,#33638,.T.);
#47655=ORIENTED_EDGE('',*,*,#33646,.T.);
#47656=ORIENTED_EDGE('',*,*,#33656,.T.);
#47657=ORIENTED_EDGE('',*,*,#33653,.T.);
#47658=ORIENTED_EDGE('',*,*,#33650,.T.);
#47659=ORIENTED_EDGE('',*,*,#33658,.T.);
#47660=ORIENTED_EDGE('',*,*,#33668,.T.);
#47661=ORIENTED_EDGE('',*,*,#33665,.T.);
#47662=ORIENTED_EDGE('',*,*,#33662,.T.);
#47663=ORIENTED_EDGE('',*,*,#33670,.T.);
#47664=ORIENTED_EDGE('',*,*,#33680,.T.);
#47665=ORIENTED_EDGE('',*,*,#33677,.T.);
#47666=ORIENTED_EDGE('',*,*,#33674,.T.);
#47667=ORIENTED_EDGE('',*,*,#33682,.T.);
#47668=ORIENTED_EDGE('',*,*,#33692,.T.);
#47669=ORIENTED_EDGE('',*,*,#33689,.T.);
#47670=ORIENTED_EDGE('',*,*,#33686,.T.);
#47671=ORIENTED_EDGE('',*,*,#33694,.T.);
#47672=ORIENTED_EDGE('',*,*,#33704,.T.);
#47673=ORIENTED_EDGE('',*,*,#33701,.T.);
#47674=ORIENTED_EDGE('',*,*,#33698,.T.);
#47675=ORIENTED_EDGE('',*,*,#33706,.T.);
#47676=ORIENTED_EDGE('',*,*,#33716,.T.);
#47677=ORIENTED_EDGE('',*,*,#33713,.T.);
#47678=ORIENTED_EDGE('',*,*,#33710,.T.);
#47679=ORIENTED_EDGE('',*,*,#33718,.T.);
#47680=ORIENTED_EDGE('',*,*,#33728,.T.);
#47681=ORIENTED_EDGE('',*,*,#33725,.T.);
#47682=ORIENTED_EDGE('',*,*,#33722,.T.);
#47683=ORIENTED_EDGE('',*,*,#33730,.T.);
#47684=ORIENTED_EDGE('',*,*,#33740,.T.);
#47685=ORIENTED_EDGE('',*,*,#33737,.T.);
#47686=ORIENTED_EDGE('',*,*,#33734,.T.);
#47687=ORIENTED_EDGE('',*,*,#33742,.T.);
#47688=ORIENTED_EDGE('',*,*,#33752,.T.);
#47689=ORIENTED_EDGE('',*,*,#33749,.T.);
#47690=ORIENTED_EDGE('',*,*,#33746,.T.);
#47691=ORIENTED_EDGE('',*,*,#33754,.T.);
#47692=ORIENTED_EDGE('',*,*,#33764,.T.);
#47693=ORIENTED_EDGE('',*,*,#33761,.T.);
#47694=ORIENTED_EDGE('',*,*,#33758,.T.);
#47695=ORIENTED_EDGE('',*,*,#33766,.T.);
#47696=ORIENTED_EDGE('',*,*,#33776,.T.);
#47697=ORIENTED_EDGE('',*,*,#33773,.T.);
#47698=ORIENTED_EDGE('',*,*,#33770,.T.);
#47699=ORIENTED_EDGE('',*,*,#33778,.T.);
#47700=ORIENTED_EDGE('',*,*,#33788,.T.);
#47701=ORIENTED_EDGE('',*,*,#33785,.T.);
#47702=ORIENTED_EDGE('',*,*,#33782,.T.);
#47703=ORIENTED_EDGE('',*,*,#33790,.T.);
#47704=ORIENTED_EDGE('',*,*,#33800,.T.);
#47705=ORIENTED_EDGE('',*,*,#33797,.T.);
#47706=ORIENTED_EDGE('',*,*,#33794,.T.);
#47707=ORIENTED_EDGE('',*,*,#33802,.T.);
#47708=ORIENTED_EDGE('',*,*,#33812,.T.);
#47709=ORIENTED_EDGE('',*,*,#33809,.T.);
#47710=ORIENTED_EDGE('',*,*,#33806,.T.);
#47711=ORIENTED_EDGE('',*,*,#33814,.T.);
#47712=ORIENTED_EDGE('',*,*,#33824,.T.);
#47713=ORIENTED_EDGE('',*,*,#33821,.T.);
#47714=ORIENTED_EDGE('',*,*,#33818,.T.);
#47715=ORIENTED_EDGE('',*,*,#33826,.T.);
#47716=ORIENTED_EDGE('',*,*,#33836,.T.);
#47717=ORIENTED_EDGE('',*,*,#33833,.T.);
#47718=ORIENTED_EDGE('',*,*,#33830,.T.);
#47719=ORIENTED_EDGE('',*,*,#33838,.T.);
#47720=ORIENTED_EDGE('',*,*,#33848,.T.);
#47721=ORIENTED_EDGE('',*,*,#33845,.T.);
#47722=ORIENTED_EDGE('',*,*,#33842,.T.);
#47723=ORIENTED_EDGE('',*,*,#33850,.T.);
#47724=ORIENTED_EDGE('',*,*,#33860,.T.);
#47725=ORIENTED_EDGE('',*,*,#33857,.T.);
#47726=ORIENTED_EDGE('',*,*,#33854,.T.);
#47727=ORIENTED_EDGE('',*,*,#33862,.T.);
#47728=ORIENTED_EDGE('',*,*,#33872,.T.);
#47729=ORIENTED_EDGE('',*,*,#33869,.T.);
#47730=ORIENTED_EDGE('',*,*,#33866,.T.);
#47731=ORIENTED_EDGE('',*,*,#33874,.T.);
#47732=ORIENTED_EDGE('',*,*,#33884,.T.);
#47733=ORIENTED_EDGE('',*,*,#33881,.T.);
#47734=ORIENTED_EDGE('',*,*,#33878,.T.);
#47735=ORIENTED_EDGE('',*,*,#33886,.T.);
#47736=ORIENTED_EDGE('',*,*,#33896,.T.);
#47737=ORIENTED_EDGE('',*,*,#33893,.T.);
#47738=ORIENTED_EDGE('',*,*,#33890,.T.);
#47739=ORIENTED_EDGE('',*,*,#33898,.T.);
#47740=ORIENTED_EDGE('',*,*,#33908,.T.);
#47741=ORIENTED_EDGE('',*,*,#33905,.T.);
#47742=ORIENTED_EDGE('',*,*,#33902,.T.);
#47743=ORIENTED_EDGE('',*,*,#33910,.T.);
#47744=ORIENTED_EDGE('',*,*,#33920,.T.);
#47745=ORIENTED_EDGE('',*,*,#33917,.T.);
#47746=ORIENTED_EDGE('',*,*,#33914,.T.);
#47747=ORIENTED_EDGE('',*,*,#33922,.T.);
#47748=ORIENTED_EDGE('',*,*,#33932,.T.);
#47749=ORIENTED_EDGE('',*,*,#33929,.T.);
#47750=ORIENTED_EDGE('',*,*,#33926,.T.);
#47751=ORIENTED_EDGE('',*,*,#33934,.T.);
#47752=ORIENTED_EDGE('',*,*,#33944,.T.);
#47753=ORIENTED_EDGE('',*,*,#33941,.T.);
#47754=ORIENTED_EDGE('',*,*,#33938,.T.);
#47755=ORIENTED_EDGE('',*,*,#33946,.T.);
#47756=ORIENTED_EDGE('',*,*,#33956,.T.);
#47757=ORIENTED_EDGE('',*,*,#33953,.T.);
#47758=ORIENTED_EDGE('',*,*,#33950,.T.);
#47759=ORIENTED_EDGE('',*,*,#33958,.T.);
#47760=ORIENTED_EDGE('',*,*,#33968,.T.);
#47761=ORIENTED_EDGE('',*,*,#33965,.T.);
#47762=ORIENTED_EDGE('',*,*,#33962,.T.);
#47763=ORIENTED_EDGE('',*,*,#33970,.T.);
#47764=ORIENTED_EDGE('',*,*,#33980,.T.);
#47765=ORIENTED_EDGE('',*,*,#33977,.T.);
#47766=ORIENTED_EDGE('',*,*,#33974,.T.);
#47767=ORIENTED_EDGE('',*,*,#33982,.T.);
#47768=ORIENTED_EDGE('',*,*,#33992,.T.);
#47769=ORIENTED_EDGE('',*,*,#33989,.T.);
#47770=ORIENTED_EDGE('',*,*,#33986,.T.);
#47771=ORIENTED_EDGE('',*,*,#33994,.T.);
#47772=ORIENTED_EDGE('',*,*,#34004,.T.);
#47773=ORIENTED_EDGE('',*,*,#34001,.T.);
#47774=ORIENTED_EDGE('',*,*,#33998,.T.);
#47775=ORIENTED_EDGE('',*,*,#34006,.T.);
#47776=ORIENTED_EDGE('',*,*,#34016,.T.);
#47777=ORIENTED_EDGE('',*,*,#34013,.T.);
#47778=ORIENTED_EDGE('',*,*,#34010,.T.);
#47779=ORIENTED_EDGE('',*,*,#34018,.T.);
#47780=ORIENTED_EDGE('',*,*,#34028,.T.);
#47781=ORIENTED_EDGE('',*,*,#34025,.T.);
#47782=ORIENTED_EDGE('',*,*,#34022,.T.);
#47783=ORIENTED_EDGE('',*,*,#34030,.T.);
#47784=ORIENTED_EDGE('',*,*,#34040,.T.);
#47785=ORIENTED_EDGE('',*,*,#34037,.T.);
#47786=ORIENTED_EDGE('',*,*,#34034,.T.);
#47787=ORIENTED_EDGE('',*,*,#34042,.T.);
#47788=ORIENTED_EDGE('',*,*,#34052,.T.);
#47789=ORIENTED_EDGE('',*,*,#34049,.T.);
#47790=ORIENTED_EDGE('',*,*,#34046,.T.);
#47791=ORIENTED_EDGE('',*,*,#34054,.T.);
#47792=ORIENTED_EDGE('',*,*,#34064,.T.);
#47793=ORIENTED_EDGE('',*,*,#34061,.T.);
#47794=ORIENTED_EDGE('',*,*,#34058,.T.);
#47795=ORIENTED_EDGE('',*,*,#34066,.T.);
#47796=ORIENTED_EDGE('',*,*,#34076,.T.);
#47797=ORIENTED_EDGE('',*,*,#34073,.T.);
#47798=ORIENTED_EDGE('',*,*,#34070,.T.);
#47799=ORIENTED_EDGE('',*,*,#34078,.T.);
#47800=ORIENTED_EDGE('',*,*,#34088,.T.);
#47801=ORIENTED_EDGE('',*,*,#34085,.T.);
#47802=ORIENTED_EDGE('',*,*,#34082,.T.);
#47803=ORIENTED_EDGE('',*,*,#34090,.T.);
#47804=ORIENTED_EDGE('',*,*,#34100,.T.);
#47805=ORIENTED_EDGE('',*,*,#34097,.T.);
#47806=ORIENTED_EDGE('',*,*,#34094,.T.);
#47807=ORIENTED_EDGE('',*,*,#34102,.T.);
#47808=ORIENTED_EDGE('',*,*,#34112,.T.);
#47809=ORIENTED_EDGE('',*,*,#34109,.T.);
#47810=ORIENTED_EDGE('',*,*,#34106,.T.);
#47811=ORIENTED_EDGE('',*,*,#34114,.T.);
#47812=ORIENTED_EDGE('',*,*,#34124,.T.);
#47813=ORIENTED_EDGE('',*,*,#34121,.T.);
#47814=ORIENTED_EDGE('',*,*,#34118,.T.);
#47815=ORIENTED_EDGE('',*,*,#34126,.T.);
#47816=ORIENTED_EDGE('',*,*,#34136,.T.);
#47817=ORIENTED_EDGE('',*,*,#34133,.T.);
#47818=ORIENTED_EDGE('',*,*,#34130,.T.);
#47819=ORIENTED_EDGE('',*,*,#34138,.T.);
#47820=ORIENTED_EDGE('',*,*,#34148,.T.);
#47821=ORIENTED_EDGE('',*,*,#34145,.T.);
#47822=ORIENTED_EDGE('',*,*,#34142,.T.);
#47823=ORIENTED_EDGE('',*,*,#34150,.T.);
#47824=ORIENTED_EDGE('',*,*,#34160,.T.);
#47825=ORIENTED_EDGE('',*,*,#34157,.T.);
#47826=ORIENTED_EDGE('',*,*,#34154,.T.);
#47827=ORIENTED_EDGE('',*,*,#34162,.T.);
#47828=ORIENTED_EDGE('',*,*,#34172,.T.);
#47829=ORIENTED_EDGE('',*,*,#34169,.T.);
#47830=ORIENTED_EDGE('',*,*,#34166,.T.);
#47831=ORIENTED_EDGE('',*,*,#34174,.T.);
#47832=ORIENTED_EDGE('',*,*,#34184,.T.);
#47833=ORIENTED_EDGE('',*,*,#34181,.T.);
#47834=ORIENTED_EDGE('',*,*,#34178,.T.);
#47835=ORIENTED_EDGE('',*,*,#34186,.T.);
#47836=ORIENTED_EDGE('',*,*,#34196,.T.);
#47837=ORIENTED_EDGE('',*,*,#34193,.T.);
#47838=ORIENTED_EDGE('',*,*,#34190,.T.);
#47839=ORIENTED_EDGE('',*,*,#34198,.T.);
#47840=ORIENTED_EDGE('',*,*,#34208,.T.);
#47841=ORIENTED_EDGE('',*,*,#34205,.T.);
#47842=ORIENTED_EDGE('',*,*,#34202,.T.);
#47843=ORIENTED_EDGE('',*,*,#34210,.T.);
#47844=ORIENTED_EDGE('',*,*,#34220,.T.);
#47845=ORIENTED_EDGE('',*,*,#34217,.T.);
#47846=ORIENTED_EDGE('',*,*,#34214,.T.);
#47847=ORIENTED_EDGE('',*,*,#34222,.T.);
#47848=ORIENTED_EDGE('',*,*,#34232,.T.);
#47849=ORIENTED_EDGE('',*,*,#34229,.T.);
#47850=ORIENTED_EDGE('',*,*,#34226,.T.);
#47851=ORIENTED_EDGE('',*,*,#34234,.T.);
#47852=ORIENTED_EDGE('',*,*,#34244,.T.);
#47853=ORIENTED_EDGE('',*,*,#34241,.T.);
#47854=ORIENTED_EDGE('',*,*,#34238,.T.);
#47855=ORIENTED_EDGE('',*,*,#34246,.T.);
#47856=ORIENTED_EDGE('',*,*,#34256,.T.);
#47857=ORIENTED_EDGE('',*,*,#34253,.T.);
#47858=ORIENTED_EDGE('',*,*,#34250,.T.);
#47859=ORIENTED_EDGE('',*,*,#34258,.T.);
#47860=ORIENTED_EDGE('',*,*,#34268,.T.);
#47861=ORIENTED_EDGE('',*,*,#34265,.T.);
#47862=ORIENTED_EDGE('',*,*,#34262,.T.);
#47863=ORIENTED_EDGE('',*,*,#34270,.T.);
#47864=ORIENTED_EDGE('',*,*,#34280,.T.);
#47865=ORIENTED_EDGE('',*,*,#34277,.T.);
#47866=ORIENTED_EDGE('',*,*,#34274,.T.);
#47867=ORIENTED_EDGE('',*,*,#34282,.T.);
#47868=ORIENTED_EDGE('',*,*,#34292,.T.);
#47869=ORIENTED_EDGE('',*,*,#34289,.T.);
#47870=ORIENTED_EDGE('',*,*,#34286,.T.);
#47871=ORIENTED_EDGE('',*,*,#34294,.T.);
#47872=ORIENTED_EDGE('',*,*,#34304,.T.);
#47873=ORIENTED_EDGE('',*,*,#34301,.T.);
#47874=ORIENTED_EDGE('',*,*,#34298,.T.);
#47875=ORIENTED_EDGE('',*,*,#34306,.T.);
#47876=ORIENTED_EDGE('',*,*,#34316,.T.);
#47877=ORIENTED_EDGE('',*,*,#34313,.T.);
#47878=ORIENTED_EDGE('',*,*,#34310,.T.);
#47879=ORIENTED_EDGE('',*,*,#34318,.T.);
#47880=ORIENTED_EDGE('',*,*,#34328,.T.);
#47881=ORIENTED_EDGE('',*,*,#34325,.T.);
#47882=ORIENTED_EDGE('',*,*,#34322,.T.);
#47883=ORIENTED_EDGE('',*,*,#34330,.T.);
#47884=ORIENTED_EDGE('',*,*,#34340,.T.);
#47885=ORIENTED_EDGE('',*,*,#34337,.T.);
#47886=ORIENTED_EDGE('',*,*,#34334,.T.);
#47887=ORIENTED_EDGE('',*,*,#34342,.T.);
#47888=ORIENTED_EDGE('',*,*,#34352,.T.);
#47889=ORIENTED_EDGE('',*,*,#34349,.T.);
#47890=ORIENTED_EDGE('',*,*,#34346,.T.);
#47891=ORIENTED_EDGE('',*,*,#34354,.T.);
#47892=ORIENTED_EDGE('',*,*,#34364,.T.);
#47893=ORIENTED_EDGE('',*,*,#34361,.T.);
#47894=ORIENTED_EDGE('',*,*,#34358,.T.);
#47895=ORIENTED_EDGE('',*,*,#34366,.T.);
#47896=ORIENTED_EDGE('',*,*,#34376,.T.);
#47897=ORIENTED_EDGE('',*,*,#34373,.T.);
#47898=ORIENTED_EDGE('',*,*,#34370,.T.);
#47899=ORIENTED_EDGE('',*,*,#34378,.T.);
#47900=ORIENTED_EDGE('',*,*,#34388,.T.);
#47901=ORIENTED_EDGE('',*,*,#34385,.T.);
#47902=ORIENTED_EDGE('',*,*,#34382,.T.);
#47903=ORIENTED_EDGE('',*,*,#34390,.T.);
#47904=ORIENTED_EDGE('',*,*,#34400,.T.);
#47905=ORIENTED_EDGE('',*,*,#34397,.T.);
#47906=ORIENTED_EDGE('',*,*,#34394,.T.);
#47907=ORIENTED_EDGE('',*,*,#34402,.T.);
#47908=ORIENTED_EDGE('',*,*,#34412,.T.);
#47909=ORIENTED_EDGE('',*,*,#34409,.T.);
#47910=ORIENTED_EDGE('',*,*,#34406,.T.);
#47911=ORIENTED_EDGE('',*,*,#34414,.T.);
#47912=ORIENTED_EDGE('',*,*,#34424,.T.);
#47913=ORIENTED_EDGE('',*,*,#34421,.T.);
#47914=ORIENTED_EDGE('',*,*,#34418,.T.);
#47915=ORIENTED_EDGE('',*,*,#34426,.T.);
#47916=ORIENTED_EDGE('',*,*,#34436,.T.);
#47917=ORIENTED_EDGE('',*,*,#34433,.T.);
#47918=ORIENTED_EDGE('',*,*,#34430,.T.);
#47919=ORIENTED_EDGE('',*,*,#34438,.T.);
#47920=ORIENTED_EDGE('',*,*,#34448,.T.);
#47921=ORIENTED_EDGE('',*,*,#34445,.T.);
#47922=ORIENTED_EDGE('',*,*,#34442,.T.);
#47923=ORIENTED_EDGE('',*,*,#34450,.T.);
#47924=ORIENTED_EDGE('',*,*,#34460,.T.);
#47925=ORIENTED_EDGE('',*,*,#34457,.T.);
#47926=ORIENTED_EDGE('',*,*,#34454,.T.);
#47927=ORIENTED_EDGE('',*,*,#34462,.T.);
#47928=ORIENTED_EDGE('',*,*,#34472,.T.);
#47929=ORIENTED_EDGE('',*,*,#34469,.T.);
#47930=ORIENTED_EDGE('',*,*,#34466,.T.);
#47931=ORIENTED_EDGE('',*,*,#34474,.T.);
#47932=ORIENTED_EDGE('',*,*,#34484,.T.);
#47933=ORIENTED_EDGE('',*,*,#34481,.T.);
#47934=ORIENTED_EDGE('',*,*,#34478,.T.);
#47935=ORIENTED_EDGE('',*,*,#34486,.T.);
#47936=ORIENTED_EDGE('',*,*,#34496,.T.);
#47937=ORIENTED_EDGE('',*,*,#34493,.T.);
#47938=ORIENTED_EDGE('',*,*,#34490,.T.);
#47939=ORIENTED_EDGE('',*,*,#34498,.T.);
#47940=ORIENTED_EDGE('',*,*,#34508,.T.);
#47941=ORIENTED_EDGE('',*,*,#34505,.T.);
#47942=ORIENTED_EDGE('',*,*,#34502,.T.);
#47943=ORIENTED_EDGE('',*,*,#34510,.T.);
#47944=ORIENTED_EDGE('',*,*,#34520,.T.);
#47945=ORIENTED_EDGE('',*,*,#34517,.T.);
#47946=ORIENTED_EDGE('',*,*,#34514,.T.);
#47947=ORIENTED_EDGE('',*,*,#34522,.T.);
#47948=ORIENTED_EDGE('',*,*,#34532,.T.);
#47949=ORIENTED_EDGE('',*,*,#34529,.T.);
#47950=ORIENTED_EDGE('',*,*,#34526,.T.);
#47951=ORIENTED_EDGE('',*,*,#34534,.T.);
#47952=ORIENTED_EDGE('',*,*,#34544,.T.);
#47953=ORIENTED_EDGE('',*,*,#34541,.T.);
#47954=ORIENTED_EDGE('',*,*,#34538,.T.);
#47955=ORIENTED_EDGE('',*,*,#34546,.T.);
#47956=ORIENTED_EDGE('',*,*,#34556,.T.);
#47957=ORIENTED_EDGE('',*,*,#34553,.T.);
#47958=ORIENTED_EDGE('',*,*,#34550,.T.);
#47959=ORIENTED_EDGE('',*,*,#34558,.T.);
#47960=ORIENTED_EDGE('',*,*,#34568,.T.);
#47961=ORIENTED_EDGE('',*,*,#34565,.T.);
#47962=ORIENTED_EDGE('',*,*,#34562,.T.);
#47963=ORIENTED_EDGE('',*,*,#34570,.T.);
#47964=ORIENTED_EDGE('',*,*,#34580,.T.);
#47965=ORIENTED_EDGE('',*,*,#34577,.T.);
#47966=ORIENTED_EDGE('',*,*,#34574,.T.);
#47967=ORIENTED_EDGE('',*,*,#34582,.T.);
#47968=ORIENTED_EDGE('',*,*,#34592,.T.);
#47969=ORIENTED_EDGE('',*,*,#34589,.T.);
#47970=ORIENTED_EDGE('',*,*,#34586,.T.);
#47971=ORIENTED_EDGE('',*,*,#34594,.T.);
#47972=ORIENTED_EDGE('',*,*,#34604,.T.);
#47973=ORIENTED_EDGE('',*,*,#34601,.T.);
#47974=ORIENTED_EDGE('',*,*,#34598,.T.);
#47975=ORIENTED_EDGE('',*,*,#34606,.T.);
#47976=ORIENTED_EDGE('',*,*,#34616,.T.);
#47977=ORIENTED_EDGE('',*,*,#34613,.T.);
#47978=ORIENTED_EDGE('',*,*,#34610,.T.);
#47979=ORIENTED_EDGE('',*,*,#34618,.T.);
#47980=ORIENTED_EDGE('',*,*,#34628,.T.);
#47981=ORIENTED_EDGE('',*,*,#34625,.T.);
#47982=ORIENTED_EDGE('',*,*,#34622,.T.);
#47983=ORIENTED_EDGE('',*,*,#34630,.T.);
#47984=ORIENTED_EDGE('',*,*,#34640,.T.);
#47985=ORIENTED_EDGE('',*,*,#34637,.T.);
#47986=ORIENTED_EDGE('',*,*,#34634,.T.);
#47987=ORIENTED_EDGE('',*,*,#34642,.T.);
#47988=ORIENTED_EDGE('',*,*,#34652,.T.);
#47989=ORIENTED_EDGE('',*,*,#34649,.T.);
#47990=ORIENTED_EDGE('',*,*,#34646,.T.);
#47991=ORIENTED_EDGE('',*,*,#34654,.T.);
#47992=ORIENTED_EDGE('',*,*,#34664,.T.);
#47993=ORIENTED_EDGE('',*,*,#34661,.T.);
#47994=ORIENTED_EDGE('',*,*,#34658,.T.);
#47995=ORIENTED_EDGE('',*,*,#34666,.T.);
#47996=ORIENTED_EDGE('',*,*,#34676,.T.);
#47997=ORIENTED_EDGE('',*,*,#34673,.T.);
#47998=ORIENTED_EDGE('',*,*,#34670,.T.);
#47999=ORIENTED_EDGE('',*,*,#34678,.T.);
#48000=ORIENTED_EDGE('',*,*,#34688,.T.);
#48001=ORIENTED_EDGE('',*,*,#34685,.T.);
#48002=ORIENTED_EDGE('',*,*,#34682,.T.);
#48003=ORIENTED_EDGE('',*,*,#34690,.T.);
#48004=ORIENTED_EDGE('',*,*,#34700,.T.);
#48005=ORIENTED_EDGE('',*,*,#34697,.T.);
#48006=ORIENTED_EDGE('',*,*,#34694,.T.);
#48007=ORIENTED_EDGE('',*,*,#34702,.T.);
#48008=ORIENTED_EDGE('',*,*,#34712,.T.);
#48009=ORIENTED_EDGE('',*,*,#34709,.T.);
#48010=ORIENTED_EDGE('',*,*,#34706,.T.);
#48011=ORIENTED_EDGE('',*,*,#34714,.T.);
#48012=ORIENTED_EDGE('',*,*,#34724,.T.);
#48013=ORIENTED_EDGE('',*,*,#34721,.T.);
#48014=ORIENTED_EDGE('',*,*,#34718,.T.);
#48015=ORIENTED_EDGE('',*,*,#34726,.T.);
#48016=ORIENTED_EDGE('',*,*,#34736,.T.);
#48017=ORIENTED_EDGE('',*,*,#34733,.T.);
#48018=ORIENTED_EDGE('',*,*,#34730,.T.);
#48019=ORIENTED_EDGE('',*,*,#34738,.T.);
#48020=ORIENTED_EDGE('',*,*,#34748,.T.);
#48021=ORIENTED_EDGE('',*,*,#34745,.T.);
#48022=ORIENTED_EDGE('',*,*,#34742,.T.);
#48023=ORIENTED_EDGE('',*,*,#34750,.T.);
#48024=ORIENTED_EDGE('',*,*,#34760,.T.);
#48025=ORIENTED_EDGE('',*,*,#34757,.T.);
#48026=ORIENTED_EDGE('',*,*,#34754,.T.);
#48027=ORIENTED_EDGE('',*,*,#34762,.T.);
#48028=ORIENTED_EDGE('',*,*,#34772,.T.);
#48029=ORIENTED_EDGE('',*,*,#34769,.T.);
#48030=ORIENTED_EDGE('',*,*,#34766,.T.);
#48031=ORIENTED_EDGE('',*,*,#34774,.T.);
#48032=ORIENTED_EDGE('',*,*,#34784,.T.);
#48033=ORIENTED_EDGE('',*,*,#34781,.T.);
#48034=ORIENTED_EDGE('',*,*,#34778,.T.);
#48035=ORIENTED_EDGE('',*,*,#34786,.T.);
#48036=ORIENTED_EDGE('',*,*,#34796,.T.);
#48037=ORIENTED_EDGE('',*,*,#34793,.T.);
#48038=ORIENTED_EDGE('',*,*,#34790,.T.);
#48039=ORIENTED_EDGE('',*,*,#34798,.T.);
#48040=ORIENTED_EDGE('',*,*,#34808,.T.);
#48041=ORIENTED_EDGE('',*,*,#34805,.T.);
#48042=ORIENTED_EDGE('',*,*,#34802,.T.);
#48043=ORIENTED_EDGE('',*,*,#34810,.T.);
#48044=ORIENTED_EDGE('',*,*,#34820,.T.);
#48045=ORIENTED_EDGE('',*,*,#34817,.T.);
#48046=ORIENTED_EDGE('',*,*,#34814,.T.);
#48047=ORIENTED_EDGE('',*,*,#34822,.T.);
#48048=ORIENTED_EDGE('',*,*,#34832,.T.);
#48049=ORIENTED_EDGE('',*,*,#34829,.T.);
#48050=ORIENTED_EDGE('',*,*,#34826,.T.);
#48051=ORIENTED_EDGE('',*,*,#34834,.T.);
#48052=ORIENTED_EDGE('',*,*,#34844,.T.);
#48053=ORIENTED_EDGE('',*,*,#34841,.T.);
#48054=ORIENTED_EDGE('',*,*,#34838,.T.);
#48055=ORIENTED_EDGE('',*,*,#34846,.T.);
#48056=ORIENTED_EDGE('',*,*,#34856,.T.);
#48057=ORIENTED_EDGE('',*,*,#34853,.T.);
#48058=ORIENTED_EDGE('',*,*,#34850,.T.);
#48059=ORIENTED_EDGE('',*,*,#32620,.T.);
#48060=ORIENTED_EDGE('',*,*,#32684,.T.);
#48061=ORIENTED_EDGE('',*,*,#32681,.T.);
#48062=ORIENTED_EDGE('',*,*,#32678,.T.);
#48063=ORIENTED_EDGE('',*,*,#32675,.T.);
#48064=ORIENTED_EDGE('',*,*,#32672,.T.);
#48065=ORIENTED_EDGE('',*,*,#32669,.T.);
#48066=ORIENTED_EDGE('',*,*,#32666,.T.);
#48067=ORIENTED_EDGE('',*,*,#32663,.T.);
#48068=ORIENTED_EDGE('',*,*,#32660,.T.);
#48069=ORIENTED_EDGE('',*,*,#32657,.T.);
#48070=ORIENTED_EDGE('',*,*,#32654,.T.);
#48071=ORIENTED_EDGE('',*,*,#32651,.T.);
#48072=ORIENTED_EDGE('',*,*,#32648,.T.);
#48073=ORIENTED_EDGE('',*,*,#32645,.T.);
#48074=ORIENTED_EDGE('',*,*,#32642,.T.);
#48075=ORIENTED_EDGE('',*,*,#32639,.T.);
#48076=ORIENTED_EDGE('',*,*,#32636,.T.);
#48077=ORIENTED_EDGE('',*,*,#32633,.T.);
#48078=ORIENTED_EDGE('',*,*,#32630,.T.);
#48079=ORIENTED_EDGE('',*,*,#32627,.T.);
#48080=ORIENTED_EDGE('',*,*,#32624,.T.);
#48081=ORIENTED_EDGE('',*,*,#32560,.T.);
#48082=ORIENTED_EDGE('',*,*,#32594,.T.);
#48083=ORIENTED_EDGE('',*,*,#32591,.T.);
#48084=ORIENTED_EDGE('',*,*,#32588,.T.);
#48085=ORIENTED_EDGE('',*,*,#32585,.T.);
#48086=ORIENTED_EDGE('',*,*,#32582,.T.);
#48087=ORIENTED_EDGE('',*,*,#32579,.T.);
#48088=ORIENTED_EDGE('',*,*,#32576,.T.);
#48089=ORIENTED_EDGE('',*,*,#32573,.T.);
#48090=ORIENTED_EDGE('',*,*,#32570,.T.);
#48091=ORIENTED_EDGE('',*,*,#32567,.T.);
#48092=ORIENTED_EDGE('',*,*,#32564,.T.);
#48093=ORIENTED_EDGE('',*,*,#32344,.T.);
#48094=ORIENTED_EDGE('',*,*,#32375,.T.);
#48095=ORIENTED_EDGE('',*,*,#32372,.T.);
#48096=ORIENTED_EDGE('',*,*,#32369,.T.);
#48097=ORIENTED_EDGE('',*,*,#32366,.T.);
#48098=ORIENTED_EDGE('',*,*,#32363,.T.);
#48099=ORIENTED_EDGE('',*,*,#32360,.T.);
#48100=ORIENTED_EDGE('',*,*,#32357,.T.);
#48101=ORIENTED_EDGE('',*,*,#32354,.T.);
#48102=ORIENTED_EDGE('',*,*,#32351,.T.);
#48103=ORIENTED_EDGE('',*,*,#32348,.T.);
#48104=ORIENTED_EDGE('',*,*,#32308,.T.);
#48105=ORIENTED_EDGE('',*,*,#32342,.T.);
#48106=ORIENTED_EDGE('',*,*,#32339,.T.);
#48107=ORIENTED_EDGE('',*,*,#32336,.T.);
#48108=ORIENTED_EDGE('',*,*,#32333,.T.);
#48109=ORIENTED_EDGE('',*,*,#32330,.T.);
#48110=ORIENTED_EDGE('',*,*,#32327,.T.);
#48111=ORIENTED_EDGE('',*,*,#32324,.T.);
#48112=ORIENTED_EDGE('',*,*,#32321,.T.);
#48113=ORIENTED_EDGE('',*,*,#32318,.T.);
#48114=ORIENTED_EDGE('',*,*,#32315,.T.);
#48115=ORIENTED_EDGE('',*,*,#32312,.T.);
#48116=ORIENTED_EDGE('',*,*,#32074,.T.);
#48117=ORIENTED_EDGE('',*,*,#32138,.T.);
#48118=ORIENTED_EDGE('',*,*,#32135,.T.);
#48119=ORIENTED_EDGE('',*,*,#32132,.T.);
#48120=ORIENTED_EDGE('',*,*,#32129,.T.);
#48121=ORIENTED_EDGE('',*,*,#32126,.T.);
#48122=ORIENTED_EDGE('',*,*,#32123,.T.);
#48123=ORIENTED_EDGE('',*,*,#32120,.T.);
#48124=ORIENTED_EDGE('',*,*,#32117,.T.);
#48125=ORIENTED_EDGE('',*,*,#32114,.T.);
#48126=ORIENTED_EDGE('',*,*,#32111,.T.);
#48127=ORIENTED_EDGE('',*,*,#32108,.T.);
#48128=ORIENTED_EDGE('',*,*,#32105,.T.);
#48129=ORIENTED_EDGE('',*,*,#32102,.T.);
#48130=ORIENTED_EDGE('',*,*,#32099,.T.);
#48131=ORIENTED_EDGE('',*,*,#32096,.T.);
#48132=ORIENTED_EDGE('',*,*,#32093,.T.);
#48133=ORIENTED_EDGE('',*,*,#32090,.T.);
#48134=ORIENTED_EDGE('',*,*,#32087,.T.);
#48135=ORIENTED_EDGE('',*,*,#32084,.T.);
#48136=ORIENTED_EDGE('',*,*,#32081,.T.);
#48137=ORIENTED_EDGE('',*,*,#32078,.T.);
#48138=ORIENTED_EDGE('',*,*,#32038,.T.);
#48139=ORIENTED_EDGE('',*,*,#32072,.T.);
#48140=ORIENTED_EDGE('',*,*,#32069,.T.);
#48141=ORIENTED_EDGE('',*,*,#32066,.T.);
#48142=ORIENTED_EDGE('',*,*,#32063,.T.);
#48143=ORIENTED_EDGE('',*,*,#32060,.T.);
#48144=ORIENTED_EDGE('',*,*,#32057,.T.);
#48145=ORIENTED_EDGE('',*,*,#32054,.T.);
#48146=ORIENTED_EDGE('',*,*,#32051,.T.);
#48147=ORIENTED_EDGE('',*,*,#32048,.T.);
#48148=ORIENTED_EDGE('',*,*,#32045,.T.);
#48149=ORIENTED_EDGE('',*,*,#32042,.T.);
#48150=ORIENTED_EDGE('',*,*,#31822,.T.);
#48151=ORIENTED_EDGE('',*,*,#31910,.T.);
#48152=ORIENTED_EDGE('',*,*,#31907,.T.);
#48153=ORIENTED_EDGE('',*,*,#31904,.T.);
#48154=ORIENTED_EDGE('',*,*,#31901,.T.);
#48155=ORIENTED_EDGE('',*,*,#31898,.T.);
#48156=ORIENTED_EDGE('',*,*,#31895,.T.);
#48157=ORIENTED_EDGE('',*,*,#31892,.T.);
#48158=ORIENTED_EDGE('',*,*,#31889,.T.);
#48159=ORIENTED_EDGE('',*,*,#31886,.T.);
#48160=ORIENTED_EDGE('',*,*,#31883,.T.);
#48161=ORIENTED_EDGE('',*,*,#31880,.T.);
#48162=ORIENTED_EDGE('',*,*,#31877,.T.);
#48163=ORIENTED_EDGE('',*,*,#31874,.T.);
#48164=ORIENTED_EDGE('',*,*,#31871,.T.);
#48165=ORIENTED_EDGE('',*,*,#31868,.T.);
#48166=ORIENTED_EDGE('',*,*,#31865,.T.);
#48167=ORIENTED_EDGE('',*,*,#31862,.T.);
#48168=ORIENTED_EDGE('',*,*,#31859,.T.);
#48169=ORIENTED_EDGE('',*,*,#31856,.T.);
#48170=ORIENTED_EDGE('',*,*,#31853,.T.);
#48171=ORIENTED_EDGE('',*,*,#31850,.T.);
#48172=ORIENTED_EDGE('',*,*,#31847,.T.);
#48173=ORIENTED_EDGE('',*,*,#31844,.T.);
#48174=ORIENTED_EDGE('',*,*,#31841,.T.);
#48175=ORIENTED_EDGE('',*,*,#31838,.T.);
#48176=ORIENTED_EDGE('',*,*,#31835,.T.);
#48177=ORIENTED_EDGE('',*,*,#31832,.T.);
#48178=ORIENTED_EDGE('',*,*,#31829,.T.);
#48179=ORIENTED_EDGE('',*,*,#31826,.T.);
#48180=ORIENTED_EDGE('',*,*,#31786,.T.);
#48181=ORIENTED_EDGE('',*,*,#31820,.T.);
#48182=ORIENTED_EDGE('',*,*,#31817,.T.);
#48183=ORIENTED_EDGE('',*,*,#31814,.T.);
#48184=ORIENTED_EDGE('',*,*,#31811,.T.);
#48185=ORIENTED_EDGE('',*,*,#31808,.T.);
#48186=ORIENTED_EDGE('',*,*,#31805,.T.);
#48187=ORIENTED_EDGE('',*,*,#31802,.T.);
#48188=ORIENTED_EDGE('',*,*,#31799,.T.);
#48189=ORIENTED_EDGE('',*,*,#31796,.T.);
#48190=ORIENTED_EDGE('',*,*,#31793,.T.);
#48191=ORIENTED_EDGE('',*,*,#31790,.T.);
#48192=ORIENTED_EDGE('',*,*,#31609,.T.);
#48193=ORIENTED_EDGE('',*,*,#31634,.T.);
#48194=ORIENTED_EDGE('',*,*,#31631,.T.);
#48195=ORIENTED_EDGE('',*,*,#31628,.T.);
#48196=ORIENTED_EDGE('',*,*,#31625,.T.);
#48197=ORIENTED_EDGE('',*,*,#31622,.T.);
#48198=ORIENTED_EDGE('',*,*,#31619,.T.);
#48199=ORIENTED_EDGE('',*,*,#31616,.T.);
#48200=ORIENTED_EDGE('',*,*,#31613,.T.);
#48201=ORIENTED_EDGE('',*,*,#31573,.T.);
#48202=ORIENTED_EDGE('',*,*,#31607,.T.);
#48203=ORIENTED_EDGE('',*,*,#31604,.T.);
#48204=ORIENTED_EDGE('',*,*,#31601,.T.);
#48205=ORIENTED_EDGE('',*,*,#31598,.T.);
#48206=ORIENTED_EDGE('',*,*,#31595,.T.);
#48207=ORIENTED_EDGE('',*,*,#31592,.T.);
#48208=ORIENTED_EDGE('',*,*,#31589,.T.);
#48209=ORIENTED_EDGE('',*,*,#31586,.T.);
#48210=ORIENTED_EDGE('',*,*,#31583,.T.);
#48211=ORIENTED_EDGE('',*,*,#31580,.T.);
#48212=ORIENTED_EDGE('',*,*,#31577,.T.);
#48213=ORIENTED_EDGE('',*,*,#31462,.T.);
#48214=ORIENTED_EDGE('',*,*,#31487,.T.);
#48215=ORIENTED_EDGE('',*,*,#31484,.T.);
#48216=ORIENTED_EDGE('',*,*,#31481,.T.);
#48217=ORIENTED_EDGE('',*,*,#31478,.T.);
#48218=ORIENTED_EDGE('',*,*,#31475,.T.);
#48219=ORIENTED_EDGE('',*,*,#31472,.T.);
#48220=ORIENTED_EDGE('',*,*,#31469,.T.);
#48221=ORIENTED_EDGE('',*,*,#31466,.T.);
#48222=ORIENTED_EDGE('',*,*,#31426,.T.);
#48223=ORIENTED_EDGE('',*,*,#31460,.T.);
#48224=ORIENTED_EDGE('',*,*,#31457,.T.);
#48225=ORIENTED_EDGE('',*,*,#31454,.T.);
#48226=ORIENTED_EDGE('',*,*,#31451,.T.);
#48227=ORIENTED_EDGE('',*,*,#31448,.T.);
#48228=ORIENTED_EDGE('',*,*,#31445,.T.);
#48229=ORIENTED_EDGE('',*,*,#31442,.T.);
#48230=ORIENTED_EDGE('',*,*,#31439,.T.);
#48231=ORIENTED_EDGE('',*,*,#31436,.T.);
#48232=ORIENTED_EDGE('',*,*,#31433,.T.);
#48233=ORIENTED_EDGE('',*,*,#31430,.T.);
#48234=ORIENTED_EDGE('',*,*,#31186,.T.);
#48235=ORIENTED_EDGE('',*,*,#31274,.T.);
#48236=ORIENTED_EDGE('',*,*,#31271,.T.);
#48237=ORIENTED_EDGE('',*,*,#31268,.T.);
#48238=ORIENTED_EDGE('',*,*,#31265,.T.);
#48239=ORIENTED_EDGE('',*,*,#31262,.T.);
#48240=ORIENTED_EDGE('',*,*,#31259,.T.);
#48241=ORIENTED_EDGE('',*,*,#31256,.T.);
#48242=ORIENTED_EDGE('',*,*,#31253,.T.);
#48243=ORIENTED_EDGE('',*,*,#31250,.T.);
#48244=ORIENTED_EDGE('',*,*,#31247,.T.);
#48245=ORIENTED_EDGE('',*,*,#31244,.T.);
#48246=ORIENTED_EDGE('',*,*,#31241,.T.);
#48247=ORIENTED_EDGE('',*,*,#31238,.T.);
#48248=ORIENTED_EDGE('',*,*,#31235,.T.);
#48249=ORIENTED_EDGE('',*,*,#31232,.T.);
#48250=ORIENTED_EDGE('',*,*,#31229,.T.);
#48251=ORIENTED_EDGE('',*,*,#31226,.T.);
#48252=ORIENTED_EDGE('',*,*,#31223,.T.);
#48253=ORIENTED_EDGE('',*,*,#31220,.T.);
#48254=ORIENTED_EDGE('',*,*,#31217,.T.);
#48255=ORIENTED_EDGE('',*,*,#31214,.T.);
#48256=ORIENTED_EDGE('',*,*,#31211,.T.);
#48257=ORIENTED_EDGE('',*,*,#31208,.T.);
#48258=ORIENTED_EDGE('',*,*,#31205,.T.);
#48259=ORIENTED_EDGE('',*,*,#31202,.T.);
#48260=ORIENTED_EDGE('',*,*,#31199,.T.);
#48261=ORIENTED_EDGE('',*,*,#31196,.T.);
#48262=ORIENTED_EDGE('',*,*,#31193,.T.);
#48263=ORIENTED_EDGE('',*,*,#31190,.T.);
#48264=ORIENTED_EDGE('',*,*,#31150,.T.);
#48265=ORIENTED_EDGE('',*,*,#31184,.T.);
#48266=ORIENTED_EDGE('',*,*,#31181,.T.);
#48267=ORIENTED_EDGE('',*,*,#31178,.T.);
#48268=ORIENTED_EDGE('',*,*,#31175,.T.);
#48269=ORIENTED_EDGE('',*,*,#31172,.T.);
#48270=ORIENTED_EDGE('',*,*,#31169,.T.);
#48271=ORIENTED_EDGE('',*,*,#31166,.T.);
#48272=ORIENTED_EDGE('',*,*,#31163,.T.);
#48273=ORIENTED_EDGE('',*,*,#31160,.T.);
#48274=ORIENTED_EDGE('',*,*,#31157,.T.);
#48275=ORIENTED_EDGE('',*,*,#31154,.T.);
#48276=ORIENTED_EDGE('',*,*,#30958,.T.);
#48277=ORIENTED_EDGE('',*,*,#31022,.T.);
#48278=ORIENTED_EDGE('',*,*,#31019,.T.);
#48279=ORIENTED_EDGE('',*,*,#31016,.T.);
#48280=ORIENTED_EDGE('',*,*,#31013,.T.);
#48281=ORIENTED_EDGE('',*,*,#31010,.T.);
#48282=ORIENTED_EDGE('',*,*,#31007,.T.);
#48283=ORIENTED_EDGE('',*,*,#31004,.T.);
#48284=ORIENTED_EDGE('',*,*,#31001,.T.);
#48285=ORIENTED_EDGE('',*,*,#30998,.T.);
#48286=ORIENTED_EDGE('',*,*,#30995,.T.);
#48287=ORIENTED_EDGE('',*,*,#30992,.T.);
#48288=ORIENTED_EDGE('',*,*,#30989,.T.);
#48289=ORIENTED_EDGE('',*,*,#30986,.T.);
#48290=ORIENTED_EDGE('',*,*,#30983,.T.);
#48291=ORIENTED_EDGE('',*,*,#30980,.T.);
#48292=ORIENTED_EDGE('',*,*,#30977,.T.);
#48293=ORIENTED_EDGE('',*,*,#30974,.T.);
#48294=ORIENTED_EDGE('',*,*,#30971,.T.);
#48295=ORIENTED_EDGE('',*,*,#30968,.T.);
#48296=ORIENTED_EDGE('',*,*,#30965,.T.);
#48297=ORIENTED_EDGE('',*,*,#30962,.T.);
#48298=ORIENTED_EDGE('',*,*,#30922,.T.);
#48299=ORIENTED_EDGE('',*,*,#30956,.T.);
#48300=ORIENTED_EDGE('',*,*,#30953,.T.);
#48301=ORIENTED_EDGE('',*,*,#30950,.T.);
#48302=ORIENTED_EDGE('',*,*,#30947,.T.);
#48303=ORIENTED_EDGE('',*,*,#30944,.T.);
#48304=ORIENTED_EDGE('',*,*,#30941,.T.);
#48305=ORIENTED_EDGE('',*,*,#30938,.T.);
#48306=ORIENTED_EDGE('',*,*,#30935,.T.);
#48307=ORIENTED_EDGE('',*,*,#30932,.T.);
#48308=ORIENTED_EDGE('',*,*,#30929,.T.);
#48309=ORIENTED_EDGE('',*,*,#30926,.T.);
#48310=ORIENTED_EDGE('',*,*,#30721,.T.);
#48311=ORIENTED_EDGE('',*,*,#30752,.T.);
#48312=ORIENTED_EDGE('',*,*,#30749,.T.);
#48313=ORIENTED_EDGE('',*,*,#30746,.T.);
#48314=ORIENTED_EDGE('',*,*,#30743,.T.);
#48315=ORIENTED_EDGE('',*,*,#30740,.T.);
#48316=ORIENTED_EDGE('',*,*,#30737,.T.);
#48317=ORIENTED_EDGE('',*,*,#30734,.T.);
#48318=ORIENTED_EDGE('',*,*,#30731,.T.);
#48319=ORIENTED_EDGE('',*,*,#30728,.T.);
#48320=ORIENTED_EDGE('',*,*,#30725,.T.);
#48321=ORIENTED_EDGE('',*,*,#30685,.T.);
#48322=ORIENTED_EDGE('',*,*,#30719,.T.);
#48323=ORIENTED_EDGE('',*,*,#30716,.T.);
#48324=ORIENTED_EDGE('',*,*,#30713,.T.);
#48325=ORIENTED_EDGE('',*,*,#30710,.T.);
#48326=ORIENTED_EDGE('',*,*,#30707,.T.);
#48327=ORIENTED_EDGE('',*,*,#30704,.T.);
#48328=ORIENTED_EDGE('',*,*,#30701,.T.);
#48329=ORIENTED_EDGE('',*,*,#30698,.T.);
#48330=ORIENTED_EDGE('',*,*,#30695,.T.);
#48331=ORIENTED_EDGE('',*,*,#30692,.T.);
#48332=ORIENTED_EDGE('',*,*,#30689,.T.);
#48333=ORIENTED_EDGE('',*,*,#30436,.T.);
#48334=ORIENTED_EDGE('',*,*,#30500,.T.);
#48335=ORIENTED_EDGE('',*,*,#30497,.T.);
#48336=ORIENTED_EDGE('',*,*,#30494,.T.);
#48337=ORIENTED_EDGE('',*,*,#30491,.T.);
#48338=ORIENTED_EDGE('',*,*,#30488,.T.);
#48339=ORIENTED_EDGE('',*,*,#30485,.T.);
#48340=ORIENTED_EDGE('',*,*,#30482,.T.);
#48341=ORIENTED_EDGE('',*,*,#30479,.T.);
#48342=ORIENTED_EDGE('',*,*,#30476,.T.);
#48343=ORIENTED_EDGE('',*,*,#30473,.T.);
#48344=ORIENTED_EDGE('',*,*,#30470,.T.);
#48345=ORIENTED_EDGE('',*,*,#30467,.T.);
#48346=ORIENTED_EDGE('',*,*,#30464,.T.);
#48347=ORIENTED_EDGE('',*,*,#30461,.T.);
#48348=ORIENTED_EDGE('',*,*,#30458,.T.);
#48349=ORIENTED_EDGE('',*,*,#30455,.T.);
#48350=ORIENTED_EDGE('',*,*,#30452,.T.);
#48351=ORIENTED_EDGE('',*,*,#30449,.T.);
#48352=ORIENTED_EDGE('',*,*,#30446,.T.);
#48353=ORIENTED_EDGE('',*,*,#30443,.T.);
#48354=ORIENTED_EDGE('',*,*,#30440,.T.);
#48355=ORIENTED_EDGE('',*,*,#30376,.T.);
#48356=ORIENTED_EDGE('',*,*,#30410,.T.);
#48357=ORIENTED_EDGE('',*,*,#30407,.T.);
#48358=ORIENTED_EDGE('',*,*,#30404,.T.);
#48359=ORIENTED_EDGE('',*,*,#30401,.T.);
#48360=ORIENTED_EDGE('',*,*,#30398,.T.);
#48361=ORIENTED_EDGE('',*,*,#30395,.T.);
#48362=ORIENTED_EDGE('',*,*,#30392,.T.);
#48363=ORIENTED_EDGE('',*,*,#30389,.T.);
#48364=ORIENTED_EDGE('',*,*,#30386,.T.);
#48365=ORIENTED_EDGE('',*,*,#30383,.T.);
#48366=ORIENTED_EDGE('',*,*,#30380,.T.);
#48367=ORIENTED_EDGE('',*,*,#35038,.F.);
#48368=ORIENTED_EDGE('',*,*,#35053,.T.);
#48369=ORIENTED_EDGE('',*,*,#35054,.F.);
#48370=ORIENTED_EDGE('',*,*,#35051,.T.);
#48371=ORIENTED_EDGE('',*,*,#35040,.F.);
#48372=ORIENTED_EDGE('',*,*,#35006,.T.);
#48373=ORIENTED_EDGE('',*,*,#35055,.F.);
#48374=ORIENTED_EDGE('',*,*,#35053,.F.);
#48375=ORIENTED_EDGE('',*,*,#34911,.T.);
#48376=ORIENTED_EDGE('',*,*,#34949,.T.);
#48377=ORIENTED_EDGE('',*,*,#34945,.T.);
#48378=ORIENTED_EDGE('',*,*,#34937,.T.);
#48379=ORIENTED_EDGE('',*,*,#35056,.T.);
#48380=ORIENTED_EDGE('',*,*,#35057,.T.);
#48381=ORIENTED_EDGE('',*,*,#34886,.T.);
#48382=ORIENTED_EDGE('',*,*,#35058,.T.);
#48383=ORIENTED_EDGE('',*,*,#34885,.T.);
#48384=ORIENTED_EDGE('',*,*,#35059,.T.);
#48385=ORIENTED_EDGE('',*,*,#35060,.T.);
#48386=ORIENTED_EDGE('',*,*,#35058,.F.);
#48387=ORIENTED_EDGE('',*,*,#34884,.T.);
#48388=ORIENTED_EDGE('',*,*,#35061,.T.);
#48389=ORIENTED_EDGE('',*,*,#35062,.T.);
#48390=ORIENTED_EDGE('',*,*,#35059,.F.);
#48391=ORIENTED_EDGE('',*,*,#34883,.T.);
#48392=ORIENTED_EDGE('',*,*,#35063,.T.);
#48393=ORIENTED_EDGE('',*,*,#35017,.T.);
#48394=ORIENTED_EDGE('',*,*,#35061,.F.);
#48395=ORIENTED_EDGE('',*,*,#34882,.T.);
#48396=ORIENTED_EDGE('',*,*,#35064,.T.);
#48397=ORIENTED_EDGE('',*,*,#34920,.T.);
#48398=ORIENTED_EDGE('',*,*,#35063,.F.);
#48399=ORIENTED_EDGE('',*,*,#34881,.T.);
#48400=ORIENTED_EDGE('',*,*,#35065,.T.);
#48401=ORIENTED_EDGE('',*,*,#35015,.T.);
#48402=ORIENTED_EDGE('',*,*,#35064,.F.);
#48403=ORIENTED_EDGE('',*,*,#34880,.T.);
#48404=ORIENTED_EDGE('',*,*,#35066,.T.);
#48405=ORIENTED_EDGE('',*,*,#35014,.T.);
#48406=ORIENTED_EDGE('',*,*,#35065,.F.);
#48407=ORIENTED_EDGE('',*,*,#34879,.T.);
#48408=ORIENTED_EDGE('',*,*,#35067,.T.);
#48409=ORIENTED_EDGE('',*,*,#35012,.T.);
#48410=ORIENTED_EDGE('',*,*,#35066,.F.);
#48411=ORIENTED_EDGE('',*,*,#34878,.T.);
#48412=ORIENTED_EDGE('',*,*,#35004,.T.);
#48413=ORIENTED_EDGE('',*,*,#35010,.T.);
#48414=ORIENTED_EDGE('',*,*,#35067,.F.);
#48415=ORIENTED_EDGE('',*,*,#35055,.T.);
#48416=ORIENTED_EDGE('',*,*,#35005,.T.);
#48417=ORIENTED_EDGE('',*,*,#34876,.T.);
#48418=ORIENTED_EDGE('',*,*,#35068,.T.);
#48419=ORIENTED_EDGE('',*,*,#34875,.T.);
#48420=ORIENTED_EDGE('',*,*,#35069,.T.);
#48421=ORIENTED_EDGE('',*,*,#35054,.T.);
#48422=ORIENTED_EDGE('',*,*,#35068,.F.);
#48423=ORIENTED_EDGE('',*,*,#34874,.T.);
#48424=ORIENTED_EDGE('',*,*,#35070,.T.);
#48425=ORIENTED_EDGE('',*,*,#35052,.T.);
#48426=ORIENTED_EDGE('',*,*,#35069,.F.);
#48427=ORIENTED_EDGE('',*,*,#35050,.T.);
#48428=ORIENTED_EDGE('',*,*,#35070,.F.);
#48429=ORIENTED_EDGE('',*,*,#34873,.T.);
#48430=ORIENTED_EDGE('',*,*,#34900,.T.);
#48431=ORIENTED_EDGE('',*,*,#34862,.T.);
#48432=ORIENTED_EDGE('',*,*,#34892,.T.);
#48433=ORIENTED_EDGE('',*,*,#35071,.T.);
#48434=ORIENTED_EDGE('',*,*,#34955,.T.);
#48435=ORIENTED_EDGE('',*,*,#35048,.T.);
#48436=ORIENTED_EDGE('',*,*,#35071,.F.);
#48437=ORIENTED_EDGE('',*,*,#34891,.T.);
#48438=ORIENTED_EDGE('',*,*,#35072,.T.);
#48439=ORIENTED_EDGE('',*,*,#35047,.T.);
#48440=ORIENTED_EDGE('',*,*,#35072,.F.);
#48441=ORIENTED_EDGE('',*,*,#34890,.T.);
#48442=ORIENTED_EDGE('',*,*,#35073,.T.);
#48443=ORIENTED_EDGE('',*,*,#35045,.T.);
#48444=ORIENTED_EDGE('',*,*,#35073,.F.);
#48445=ORIENTED_EDGE('',*,*,#34889,.T.);
#48446=ORIENTED_EDGE('',*,*,#35074,.T.);
#48447=ORIENTED_EDGE('',*,*,#34888,.T.);
#48448=ORIENTED_EDGE('',*,*,#35075,.T.);
#48449=ORIENTED_EDGE('',*,*,#35042,.T.);
#48450=ORIENTED_EDGE('',*,*,#35074,.F.);
#48451=ORIENTED_EDGE('',*,*,#34859,.T.);
#48452=ORIENTED_EDGE('',*,*,#34898,.F.);
#48453=ORIENTED_EDGE('',*,*,#35028,.F.);
#48454=ORIENTED_EDGE('',*,*,#35025,.F.);
#48455=ORIENTED_EDGE('',*,*,#35022,.F.);
#48456=ORIENTED_EDGE('',*,*,#35020,.F.);
#48457=ORIENTED_EDGE('',*,*,#35076,.T.);
#48458=ORIENTED_EDGE('',*,*,#34996,.F.);
#48459=ORIENTED_EDGE('',*,*,#34993,.F.);
#48460=ORIENTED_EDGE('',*,*,#34990,.F.);
#48461=ORIENTED_EDGE('',*,*,#34986,.F.);
#48462=ORIENTED_EDGE('',*,*,#34999,.F.);
#48463=ORIENTED_EDGE('',*,*,#35001,.F.);
#48464=ORIENTED_EDGE('',*,*,#34983,.F.);
#48465=ORIENTED_EDGE('',*,*,#34980,.F.);
#48466=ORIENTED_EDGE('',*,*,#34978,.F.);
#48467=ORIENTED_EDGE('',*,*,#35008,.T.);
#48468=ORIENTED_EDGE('',*,*,#35039,.F.);
#48469=ORIENTED_EDGE('',*,*,#35036,.F.);
#48470=ORIENTED_EDGE('',*,*,#35033,.F.);
#48471=ORIENTED_EDGE('',*,*,#35030,.F.);
#48472=ORIENTED_EDGE('',*,*,#34893,.F.);
#48473=ORIENTED_EDGE('',*,*,#34869,.T.);
#48474=ORIENTED_EDGE('',*,*,#34871,.T.);
#48475=ORIENTED_EDGE('',*,*,#34992,.F.);
#48476=ORIENTED_EDGE('',*,*,#35077,.F.);
#48477=ORIENTED_EDGE('',*,*,#35062,.F.);
#48478=ORIENTED_EDGE('',*,*,#35016,.T.);
#48479=ORIENTED_EDGE('',*,*,#34997,.F.);
#48480=ORIENTED_EDGE('',*,*,#35076,.F.);
#48481=ORIENTED_EDGE('',*,*,#35019,.F.);
#48482=ORIENTED_EDGE('',*,*,#35043,.F.);
#48483=ORIENTED_EDGE('',*,*,#35075,.F.);
#48484=ORIENTED_EDGE('',*,*,#34887,.F.);
#48485=ORIENTED_EDGE('',*,*,#35057,.F.);
#48486=ORIENTED_EDGE('',*,*,#35078,.F.);
#48487=ORIENTED_EDGE('',*,*,#34995,.F.);
#48488=ORIENTED_EDGE('',*,*,#35079,.T.);
#48489=ORIENTED_EDGE('',*,*,#35060,.F.);
#48490=ORIENTED_EDGE('',*,*,#35077,.T.);
#48491=ORIENTED_EDGE('',*,*,#34998,.F.);
#48492=ORIENTED_EDGE('',*,*,#35078,.T.);
#48493=ORIENTED_EDGE('',*,*,#35056,.F.);
#48494=ORIENTED_EDGE('',*,*,#35079,.F.);
#48495=ORIENTED_EDGE('',*,*,#35080,.F.);
#48496=ORIENTED_EDGE('',*,*,#35081,.T.);
#48497=ORIENTED_EDGE('',*,*,#35082,.T.);
#48498=ORIENTED_EDGE('',*,*,#35083,.T.);
#48499=ORIENTED_EDGE('',*,*,#35084,.T.);
#48500=ORIENTED_EDGE('',*,*,#35085,.T.);
#48501=ORIENTED_EDGE('',*,*,#35086,.T.);
#48502=ORIENTED_EDGE('',*,*,#35085,.F.);
#48503=ORIENTED_EDGE('',*,*,#35087,.T.);
#48504=ORIENTED_EDGE('',*,*,#35088,.F.);
#48505=ORIENTED_EDGE('',*,*,#35089,.F.);
#48506=ORIENTED_EDGE('',*,*,#35090,.F.);
#48507=ORIENTED_EDGE('',*,*,#35091,.F.);
#48508=ORIENTED_EDGE('',*,*,#35092,.F.);
#48509=ORIENTED_EDGE('',*,*,#35087,.F.);
#48510=ORIENTED_EDGE('',*,*,#35084,.F.);
#48511=ORIENTED_EDGE('',*,*,#35093,.F.);
#48512=ORIENTED_EDGE('',*,*,#35094,.F.);
#48513=ORIENTED_EDGE('',*,*,#35095,.F.);
#48514=ORIENTED_EDGE('',*,*,#35096,.F.);
#48515=ORIENTED_EDGE('',*,*,#35086,.F.);
#48516=ORIENTED_EDGE('',*,*,#35097,.T.);
#48517=ORIENTED_EDGE('',*,*,#35098,.T.);
#48518=ORIENTED_EDGE('',*,*,#35097,.F.);
#48519=ORIENTED_EDGE('',*,*,#35091,.T.);
#48520=ORIENTED_EDGE('',*,*,#35099,.T.);
#48521=ORIENTED_EDGE('',*,*,#35100,.T.);
#48522=ORIENTED_EDGE('',*,*,#35099,.F.);
#48523=ORIENTED_EDGE('',*,*,#35090,.T.);
#48524=ORIENTED_EDGE('',*,*,#35100,.F.);
#48525=ORIENTED_EDGE('',*,*,#35101,.T.);
#48526=ORIENTED_EDGE('',*,*,#35102,.T.);
#48527=ORIENTED_EDGE('',*,*,#35101,.F.);
#48528=ORIENTED_EDGE('',*,*,#35103,.T.);
#48529=ORIENTED_EDGE('',*,*,#35098,.F.);
#48530=ORIENTED_EDGE('',*,*,#35103,.F.);
#48531=ORIENTED_EDGE('',*,*,#35104,.T.);
#48532=ORIENTED_EDGE('',*,*,#35102,.F.);
#48533=ORIENTED_EDGE('',*,*,#35104,.F.);
#48534=ORIENTED_EDGE('',*,*,#35105,.T.);
#48535=ORIENTED_EDGE('',*,*,#35106,.T.);
#48536=ORIENTED_EDGE('',*,*,#35107,.T.);
#48537=ORIENTED_EDGE('',*,*,#35108,.T.);
#48538=ORIENTED_EDGE('',*,*,#35107,.F.);
#48539=ORIENTED_EDGE('',*,*,#35109,.T.);
#48540=ORIENTED_EDGE('',*,*,#35105,.F.);
#48541=ORIENTED_EDGE('',*,*,#35110,.T.);
#48542=ORIENTED_EDGE('',*,*,#35111,.T.);
#48543=ORIENTED_EDGE('',*,*,#35112,.T.);
#48544=ORIENTED_EDGE('',*,*,#35113,.T.);
#48545=ORIENTED_EDGE('',*,*,#35114,.T.);
#48546=ORIENTED_EDGE('',*,*,#35115,.F.);
#48547=ORIENTED_EDGE('',*,*,#35116,.T.);
#48548=ORIENTED_EDGE('',*,*,#35117,.F.);
#48549=ORIENTED_EDGE('',*,*,#35082,.F.);
#48550=ORIENTED_EDGE('',*,*,#35118,.T.);
#48551=ORIENTED_EDGE('',*,*,#35108,.F.);
#48552=ORIENTED_EDGE('',*,*,#35119,.T.);
#48553=ORIENTED_EDGE('',*,*,#35120,.F.);
#48554=ORIENTED_EDGE('',*,*,#35119,.F.);
#48555=ORIENTED_EDGE('',*,*,#35115,.T.);
#48556=ORIENTED_EDGE('',*,*,#35121,.T.);
#48557=ORIENTED_EDGE('',*,*,#35122,.T.);
#48558=ORIENTED_EDGE('',*,*,#35123,.T.);
#48559=ORIENTED_EDGE('',*,*,#35122,.F.);
#48560=ORIENTED_EDGE('',*,*,#35124,.T.);
#48561=ORIENTED_EDGE('',*,*,#35123,.F.);
#48562=ORIENTED_EDGE('',*,*,#35125,.T.);
#48563=ORIENTED_EDGE('',*,*,#35126,.F.);
#48564=ORIENTED_EDGE('',*,*,#35125,.F.);
#48565=ORIENTED_EDGE('',*,*,#35080,.T.);
#48566=ORIENTED_EDGE('',*,*,#35127,.T.);
#48567=ORIENTED_EDGE('',*,*,#35117,.T.);
#48568=ORIENTED_EDGE('',*,*,#35128,.T.);
#48569=ORIENTED_EDGE('',*,*,#35083,.F.);
#48570=ORIENTED_EDGE('',*,*,#35127,.F.);
#48571=ORIENTED_EDGE('',*,*,#35129,.T.);
#48572=ORIENTED_EDGE('',*,*,#35130,.F.);
#48573=ORIENTED_EDGE('',*,*,#35129,.F.);
#48574=ORIENTED_EDGE('',*,*,#35106,.F.);
#48575=ORIENTED_EDGE('',*,*,#35118,.F.);
#48576=ORIENTED_EDGE('',*,*,#35081,.F.);
#48577=ORIENTED_EDGE('',*,*,#35128,.F.);
#48578=ORIENTED_EDGE('',*,*,#35116,.F.);
#48579=ORIENTED_EDGE('',*,*,#35124,.F.);
#48580=ORIENTED_EDGE('',*,*,#35121,.F.);
#48581=ORIENTED_EDGE('',*,*,#35114,.F.);
#48582=ORIENTED_EDGE('',*,*,#35131,.F.);
#48583=ORIENTED_EDGE('',*,*,#35132,.F.);
#48584=ORIENTED_EDGE('',*,*,#35133,.F.);
#48585=ORIENTED_EDGE('',*,*,#35110,.F.);
#48586=ORIENTED_EDGE('',*,*,#35109,.F.);
#48587=ORIENTED_EDGE('',*,*,#35134,.T.);
#48588=ORIENTED_EDGE('',*,*,#35135,.T.);
#48589=ORIENTED_EDGE('',*,*,#35136,.T.);
#48590=ORIENTED_EDGE('',*,*,#35137,.T.);
#48591=ORIENTED_EDGE('',*,*,#35136,.F.);
#48592=ORIENTED_EDGE('',*,*,#35138,.T.);
#48593=ORIENTED_EDGE('',*,*,#35134,.F.);
#48594=ORIENTED_EDGE('',*,*,#35139,.T.);
#48595=ORIENTED_EDGE('',*,*,#35140,.T.);
#48596=ORIENTED_EDGE('',*,*,#35095,.T.);
#48597=ORIENTED_EDGE('',*,*,#35141,.T.);
#48598=ORIENTED_EDGE('',*,*,#35142,.T.);
#48599=ORIENTED_EDGE('',*,*,#35137,.F.);
#48600=ORIENTED_EDGE('',*,*,#35143,.T.);
#48601=ORIENTED_EDGE('',*,*,#35144,.T.);
#48602=ORIENTED_EDGE('',*,*,#35145,.T.);
#48603=ORIENTED_EDGE('',*,*,#35146,.T.);
#48604=ORIENTED_EDGE('',*,*,#35143,.F.);
#48605=ORIENTED_EDGE('',*,*,#35147,.T.);
#48606=ORIENTED_EDGE('',*,*,#35148,.T.);
#48607=ORIENTED_EDGE('',*,*,#35149,.T.);
#48608=ORIENTED_EDGE('',*,*,#35148,.F.);
#48609=ORIENTED_EDGE('',*,*,#35135,.F.);
#48610=ORIENTED_EDGE('',*,*,#35142,.F.);
#48611=ORIENTED_EDGE('',*,*,#35150,.F.);
#48612=ORIENTED_EDGE('',*,*,#35151,.F.);
#48613=ORIENTED_EDGE('',*,*,#35152,.F.);
#48614=ORIENTED_EDGE('',*,*,#35139,.F.);
#48615=ORIENTED_EDGE('',*,*,#35138,.F.);
#48616=ORIENTED_EDGE('',*,*,#35153,.F.);
#48617=ORIENTED_EDGE('',*,*,#35154,.F.);
#48618=ORIENTED_EDGE('',*,*,#35155,.F.);
#48619=ORIENTED_EDGE('',*,*,#35156,.F.);
#48620=ORIENTED_EDGE('',*,*,#35157,.F.);
#48621=ORIENTED_EDGE('',*,*,#35147,.F.);
#48622=ORIENTED_EDGE('',*,*,#35149,.F.);
#48623=ORIENTED_EDGE('',*,*,#35158,.T.);
#48624=ORIENTED_EDGE('',*,*,#35159,.T.);
#48625=ORIENTED_EDGE('',*,*,#35160,.T.);
#48626=ORIENTED_EDGE('',*,*,#35161,.T.);
#48627=ORIENTED_EDGE('',*,*,#35158,.F.);
#48628=ORIENTED_EDGE('',*,*,#35153,.T.);
#48629=ORIENTED_EDGE('',*,*,#35162,.T.);
#48630=ORIENTED_EDGE('',*,*,#35163,.T.);
#48631=ORIENTED_EDGE('',*,*,#35162,.F.);
#48632=ORIENTED_EDGE('',*,*,#35163,.F.);
#48633=ORIENTED_EDGE('',*,*,#35164,.T.);
#48634=ORIENTED_EDGE('',*,*,#35165,.T.);
#48635=ORIENTED_EDGE('',*,*,#35166,.T.);
#48636=ORIENTED_EDGE('',*,*,#35167,.T.);
#48637=ORIENTED_EDGE('',*,*,#35164,.F.);
#48638=ORIENTED_EDGE('',*,*,#35168,.T.);
#48639=ORIENTED_EDGE('',*,*,#35166,.F.);
#48640=ORIENTED_EDGE('',*,*,#35169,.F.);
#48641=ORIENTED_EDGE('',*,*,#35165,.F.);
#48642=ORIENTED_EDGE('',*,*,#35167,.F.);
#48643=ORIENTED_EDGE('',*,*,#35170,.T.);
#48644=ORIENTED_EDGE('',*,*,#35160,.F.);
#48645=ORIENTED_EDGE('',*,*,#35171,.F.);
#48646=ORIENTED_EDGE('',*,*,#35159,.F.);
#48647=ORIENTED_EDGE('',*,*,#35161,.F.);
#48648=ORIENTED_EDGE('',*,*,#35172,.T.);
#48649=ORIENTED_EDGE('',*,*,#35145,.F.);
#48650=ORIENTED_EDGE('',*,*,#35173,.F.);
#48651=ORIENTED_EDGE('',*,*,#35144,.F.);
#48652=ORIENTED_EDGE('',*,*,#35146,.F.);
#48653=ORIENTED_EDGE('',*,*,#35154,.T.);
#48654=ORIENTED_EDGE('',*,*,#35174,.T.);
#48655=ORIENTED_EDGE('',*,*,#35175,.T.);
#48656=ORIENTED_EDGE('',*,*,#35174,.F.);
#48657=ORIENTED_EDGE('',*,*,#35175,.F.);
#48658=ORIENTED_EDGE('',*,*,#35176,.T.);
#48659=ORIENTED_EDGE('',*,*,#35177,.T.);
#48660=ORIENTED_EDGE('',*,*,#35176,.F.);
#48661=ORIENTED_EDGE('',*,*,#35157,.T.);
#48662=ORIENTED_EDGE('',*,*,#35178,.T.);
#48663=ORIENTED_EDGE('',*,*,#35179,.T.);
#48664=ORIENTED_EDGE('',*,*,#35178,.F.);
#48665=ORIENTED_EDGE('',*,*,#35179,.F.);
#48666=ORIENTED_EDGE('',*,*,#35180,.T.);
#48667=ORIENTED_EDGE('',*,*,#35181,.T.);
#48668=ORIENTED_EDGE('',*,*,#35180,.F.);
#48669=ORIENTED_EDGE('',*,*,#35155,.T.);
#48670=ORIENTED_EDGE('',*,*,#35182,.T.);
#48671=ORIENTED_EDGE('',*,*,#35183,.T.);
#48672=ORIENTED_EDGE('',*,*,#35182,.F.);
#48673=ORIENTED_EDGE('',*,*,#35183,.F.);
#48674=ORIENTED_EDGE('',*,*,#35184,.T.);
#48675=ORIENTED_EDGE('',*,*,#35185,.T.);
#48676=ORIENTED_EDGE('',*,*,#35184,.F.);
#48677=ORIENTED_EDGE('',*,*,#35156,.T.);
#48678=ORIENTED_EDGE('',*,*,#35186,.T.);
#48679=ORIENTED_EDGE('',*,*,#35187,.T.);
#48680=ORIENTED_EDGE('',*,*,#35186,.F.);
#48681=ORIENTED_EDGE('',*,*,#35187,.F.);
#48682=ORIENTED_EDGE('',*,*,#35188,.T.);
#48683=ORIENTED_EDGE('',*,*,#35189,.T.);
#48684=ORIENTED_EDGE('',*,*,#35188,.F.);
#48685=ORIENTED_EDGE('',*,*,#35177,.F.);
#48686=ORIENTED_EDGE('',*,*,#35190,.T.);
#48687=ORIENTED_EDGE('',*,*,#35190,.F.);
#48688=ORIENTED_EDGE('',*,*,#35189,.F.);
#48689=ORIENTED_EDGE('',*,*,#35191,.T.);
#48690=ORIENTED_EDGE('',*,*,#35191,.F.);
#48691=ORIENTED_EDGE('',*,*,#35185,.F.);
#48692=ORIENTED_EDGE('',*,*,#35192,.T.);
#48693=ORIENTED_EDGE('',*,*,#35192,.F.);
#48694=ORIENTED_EDGE('',*,*,#35181,.F.);
#48695=ORIENTED_EDGE('',*,*,#35193,.T.);
#48696=ORIENTED_EDGE('',*,*,#35193,.F.);
#48697=ORIENTED_EDGE('',*,*,#35096,.T.);
#48698=ORIENTED_EDGE('',*,*,#35194,.T.);
#48699=ORIENTED_EDGE('',*,*,#35195,.T.);
#48700=ORIENTED_EDGE('',*,*,#35196,.T.);
#48701=ORIENTED_EDGE('',*,*,#35194,.F.);
#48702=ORIENTED_EDGE('',*,*,#35195,.F.);
#48703=ORIENTED_EDGE('',*,*,#35196,.F.);
#48704=ORIENTED_EDGE('',*,*,#35197,.T.);
#48705=ORIENTED_EDGE('',*,*,#35172,.F.);
#48706=ORIENTED_EDGE('',*,*,#35198,.T.);
#48707=ORIENTED_EDGE('',*,*,#35170,.F.);
#48708=ORIENTED_EDGE('',*,*,#35199,.T.);
#48709=ORIENTED_EDGE('',*,*,#35168,.F.);
#48710=ORIENTED_EDGE('',*,*,#35200,.T.);
#48711=ORIENTED_EDGE('',*,*,#35201,.T.);
#48712=ORIENTED_EDGE('',*,*,#35202,.F.);
#48713=ORIENTED_EDGE('',*,*,#35203,.F.);
#48714=ORIENTED_EDGE('',*,*,#35204,.F.);
#48715=ORIENTED_EDGE('',*,*,#35205,.T.);
#48716=ORIENTED_EDGE('',*,*,#35200,.F.);
#48717=ORIENTED_EDGE('',*,*,#35169,.T.);
#48718=ORIENTED_EDGE('',*,*,#35199,.F.);
#48719=ORIENTED_EDGE('',*,*,#35171,.T.);
#48720=ORIENTED_EDGE('',*,*,#35198,.F.);
#48721=ORIENTED_EDGE('',*,*,#35173,.T.);
#48722=ORIENTED_EDGE('',*,*,#35197,.F.);
#48723=ORIENTED_EDGE('',*,*,#35206,.T.);
#48724=ORIENTED_EDGE('',*,*,#35207,.F.);
#48725=ORIENTED_EDGE('',*,*,#35206,.F.);
#48726=ORIENTED_EDGE('',*,*,#35208,.F.);
#48727=ORIENTED_EDGE('',*,*,#35209,.T.);
#48728=ORIENTED_EDGE('',*,*,#35207,.T.);
#48729=ORIENTED_EDGE('',*,*,#35209,.F.);
#48730=ORIENTED_EDGE('',*,*,#35210,.F.);
#48731=ORIENTED_EDGE('',*,*,#35201,.F.);
#48732=ORIENTED_EDGE('',*,*,#35205,.F.);
#48733=ORIENTED_EDGE('',*,*,#35208,.T.);
#48734=ORIENTED_EDGE('',*,*,#35202,.T.);
#48735=ORIENTED_EDGE('',*,*,#35210,.T.);
#48736=ORIENTED_EDGE('',*,*,#35204,.T.);
#48737=ORIENTED_EDGE('',*,*,#35211,.F.);
#48738=ORIENTED_EDGE('',*,*,#35212,.F.);
#48739=ORIENTED_EDGE('',*,*,#35213,.T.);
#48740=ORIENTED_EDGE('',*,*,#35214,.F.);
#48741=ORIENTED_EDGE('',*,*,#35215,.F.);
#48742=ORIENTED_EDGE('',*,*,#35216,.F.);
#48743=ORIENTED_EDGE('',*,*,#35217,.F.);
#48744=ORIENTED_EDGE('',*,*,#35213,.F.);
#48745=ORIENTED_EDGE('',*,*,#35218,.F.);
#48746=ORIENTED_EDGE('',*,*,#35203,.T.);
#48747=ORIENTED_EDGE('',*,*,#35215,.T.);
#48748=ORIENTED_EDGE('',*,*,#35219,.F.);
#48749=ORIENTED_EDGE('',*,*,#35220,.F.);
#48750=ORIENTED_EDGE('',*,*,#35221,.F.);
#48751=ORIENTED_EDGE('',*,*,#35211,.T.);
#48752=ORIENTED_EDGE('',*,*,#35218,.T.);
#48753=ORIENTED_EDGE('',*,*,#35212,.T.);
#48754=ORIENTED_EDGE('',*,*,#35221,.T.);
#48755=ORIENTED_EDGE('',*,*,#35222,.T.);
#48756=ORIENTED_EDGE('',*,*,#35223,.T.);
#48757=ORIENTED_EDGE('',*,*,#35224,.F.);
#48758=ORIENTED_EDGE('',*,*,#35225,.F.);
#48759=ORIENTED_EDGE('',*,*,#35226,.F.);
#48760=ORIENTED_EDGE('',*,*,#35227,.F.);
#48761=ORIENTED_EDGE('',*,*,#35228,.F.);
#48762=ORIENTED_EDGE('',*,*,#35229,.T.);
#48763=ORIENTED_EDGE('',*,*,#35230,.T.);
#48764=ORIENTED_EDGE('',*,*,#35220,.T.);
#48765=ORIENTED_EDGE('',*,*,#35231,.F.);
#48766=ORIENTED_EDGE('',*,*,#35232,.F.);
#48767=ORIENTED_EDGE('',*,*,#35222,.F.);
#48768=ORIENTED_EDGE('',*,*,#35233,.F.);
#48769=ORIENTED_EDGE('',*,*,#35223,.F.);
#48770=ORIENTED_EDGE('',*,*,#35232,.T.);
#48771=ORIENTED_EDGE('',*,*,#35234,.F.);
#48772=ORIENTED_EDGE('',*,*,#35235,.F.);
#48773=ORIENTED_EDGE('',*,*,#35236,.F.);
#48774=ORIENTED_EDGE('',*,*,#35237,.F.);
#48775=ORIENTED_EDGE('',*,*,#35238,.F.);
#48776=ORIENTED_EDGE('',*,*,#35239,.F.);
#48777=ORIENTED_EDGE('',*,*,#35240,.F.);
#48778=ORIENTED_EDGE('',*,*,#35241,.F.);
#48779=ORIENTED_EDGE('',*,*,#35229,.F.);
#48780=ORIENTED_EDGE('',*,*,#35126,.T.);
#48781=ORIENTED_EDGE('',*,*,#35120,.T.);
#48782=ORIENTED_EDGE('',*,*,#35130,.T.);
#48783=ORIENTED_EDGE('',*,*,#35216,.T.);
#48784=ORIENTED_EDGE('',*,*,#35230,.F.);
#48785=ORIENTED_EDGE('',*,*,#35241,.T.);
#48786=ORIENTED_EDGE('',*,*,#35242,.F.);
#48787=ORIENTED_EDGE('',*,*,#35233,.T.);
#48788=ORIENTED_EDGE('',*,*,#35243,.T.);
#48789=ORIENTED_EDGE('',*,*,#35244,.T.);
#48790=ORIENTED_EDGE('',*,*,#35224,.T.);
#48791=ORIENTED_EDGE('',*,*,#35237,.T.);
#48792=ORIENTED_EDGE('',*,*,#35228,.T.);
#48793=ORIENTED_EDGE('',*,*,#35245,.T.);
#48794=ORIENTED_EDGE('',*,*,#35246,.T.);
#48795=ORIENTED_EDGE('',*,*,#35236,.T.);
#48796=ORIENTED_EDGE('',*,*,#35247,.F.);
#48797=ORIENTED_EDGE('',*,*,#35248,.F.);
#48798=ORIENTED_EDGE('',*,*,#35243,.F.);
#48799=ORIENTED_EDGE('',*,*,#35235,.T.);
#48800=ORIENTED_EDGE('',*,*,#35249,.T.);
#48801=ORIENTED_EDGE('',*,*,#35250,.T.);
#48802=ORIENTED_EDGE('',*,*,#35247,.T.);
#48803=ORIENTED_EDGE('',*,*,#35251,.F.);
#48804=ORIENTED_EDGE('',*,*,#35252,.F.);
#48805=ORIENTED_EDGE('',*,*,#35250,.F.);
#48806=ORIENTED_EDGE('',*,*,#35253,.F.);
#48807=ORIENTED_EDGE('',*,*,#35141,.F.);
#48808=ORIENTED_EDGE('',*,*,#35254,.F.);
#48809=ORIENTED_EDGE('',*,*,#35255,.F.);
#48810=ORIENTED_EDGE('',*,*,#35256,.F.);
#48811=ORIENTED_EDGE('',*,*,#35244,.F.);
#48812=ORIENTED_EDGE('',*,*,#35257,.F.);
#48813=ORIENTED_EDGE('',*,*,#35111,.F.);
#48814=ORIENTED_EDGE('',*,*,#35258,.F.);
#48815=ORIENTED_EDGE('',*,*,#35140,.F.);
#48816=ORIENTED_EDGE('',*,*,#35259,.F.);
#48817=ORIENTED_EDGE('',*,*,#35260,.F.);
#48818=ORIENTED_EDGE('',*,*,#35261,.F.);
#48819=ORIENTED_EDGE('',*,*,#35262,.F.);
#48820=ORIENTED_EDGE('',*,*,#35263,.F.);
#48821=ORIENTED_EDGE('',*,*,#35113,.F.);
#48822=ORIENTED_EDGE('',*,*,#35245,.F.);
#48823=ORIENTED_EDGE('',*,*,#35264,.F.);
#48824=ORIENTED_EDGE('',*,*,#35265,.F.);
#48825=ORIENTED_EDGE('',*,*,#35266,.F.);
#48826=ORIENTED_EDGE('',*,*,#35267,.F.);
#48827=ORIENTED_EDGE('',*,*,#35266,.T.);
#48828=ORIENTED_EDGE('',*,*,#35226,.T.);
#48829=ORIENTED_EDGE('',*,*,#35259,.T.);
#48830=ORIENTED_EDGE('',*,*,#35152,.T.);
#48831=ORIENTED_EDGE('',*,*,#35262,.T.);
#48832=ORIENTED_EDGE('',*,*,#35132,.T.);
#48833=ORIENTED_EDGE('',*,*,#35267,.T.);
#48834=ORIENTED_EDGE('',*,*,#35151,.T.);
#48835=ORIENTED_EDGE('',*,*,#35264,.T.);
#48836=ORIENTED_EDGE('',*,*,#35227,.T.);
#48837=ORIENTED_EDGE('',*,*,#35265,.T.);
#48838=ORIENTED_EDGE('',*,*,#35131,.T.);
#48839=ORIENTED_EDGE('',*,*,#35253,.T.);
#48840=ORIENTED_EDGE('',*,*,#35268,.T.);
#48841=ORIENTED_EDGE('',*,*,#35263,.T.);
#48842=ORIENTED_EDGE('',*,*,#35150,.T.);
#48843=ORIENTED_EDGE('',*,*,#35261,.T.);
#48844=ORIENTED_EDGE('',*,*,#35269,.T.);
#48845=ORIENTED_EDGE('',*,*,#35258,.T.);
#48846=ORIENTED_EDGE('',*,*,#35133,.T.);
#48847=ORIENTED_EDGE('',*,*,#35260,.T.);
#48848=ORIENTED_EDGE('',*,*,#35225,.T.);
#48849=ORIENTED_EDGE('',*,*,#35256,.T.);
#48850=ORIENTED_EDGE('',*,*,#35088,.T.);
#48851=ORIENTED_EDGE('',*,*,#35239,.T.);
#48852=ORIENTED_EDGE('',*,*,#35270,.T.);
#48853=ORIENTED_EDGE('',*,*,#35257,.T.);
#48854=ORIENTED_EDGE('',*,*,#35271,.T.);
#48855=ORIENTED_EDGE('',*,*,#35252,.T.);
#48856=ORIENTED_EDGE('',*,*,#35093,.T.);
#48857=ORIENTED_EDGE('',*,*,#35092,.T.);
#48858=ORIENTED_EDGE('',*,*,#35089,.T.);
#48859=ORIENTED_EDGE('',*,*,#35255,.T.);
#48860=ORIENTED_EDGE('',*,*,#35248,.T.);
#48861=ORIENTED_EDGE('',*,*,#35251,.T.);
#48862=ORIENTED_EDGE('',*,*,#35272,.T.);
#48863=ORIENTED_EDGE('',*,*,#35254,.T.);
#48864=ORIENTED_EDGE('',*,*,#35094,.T.);
#48865=ORIENTED_EDGE('',*,*,#35238,.T.);
#48866=ORIENTED_EDGE('',*,*,#35246,.F.);
#48867=ORIENTED_EDGE('',*,*,#35112,.F.);
#48868=ORIENTED_EDGE('',*,*,#35270,.F.);
#48869=ORIENTED_EDGE('',*,*,#35217,.T.);
#48870=ORIENTED_EDGE('',*,*,#35242,.T.);
#48871=ORIENTED_EDGE('',*,*,#35240,.T.);
#48872=ORIENTED_EDGE('',*,*,#35271,.F.);
#48873=ORIENTED_EDGE('',*,*,#35269,.F.);
#48874=ORIENTED_EDGE('',*,*,#35268,.F.);
#48875=ORIENTED_EDGE('',*,*,#35272,.F.);
#48876=ORIENTED_EDGE('',*,*,#35249,.F.);
#48877=ORIENTED_EDGE('',*,*,#35234,.T.);
#48878=ORIENTED_EDGE('',*,*,#35231,.T.);
#48879=ORIENTED_EDGE('',*,*,#35219,.T.);
#48880=ORIENTED_EDGE('',*,*,#35214,.T.);
#48881=ORIENTED_EDGE('',*,*,#35273,.F.);
#48882=ORIENTED_EDGE('',*,*,#35274,.T.);
#48883=ORIENTED_EDGE('',*,*,#35274,.F.);
#48884=ORIENTED_EDGE('',*,*,#35275,.F.);
#48885=ORIENTED_EDGE('',*,*,#35276,.T.);
#48886=ORIENTED_EDGE('',*,*,#35276,.F.);
#48887=ORIENTED_EDGE('',*,*,#35277,.F.);
#48888=ORIENTED_EDGE('',*,*,#35278,.T.);
#48889=ORIENTED_EDGE('',*,*,#35278,.F.);
#48890=ORIENTED_EDGE('',*,*,#35279,.T.);
#48891=ORIENTED_EDGE('',*,*,#35280,.T.);
#48892=ORIENTED_EDGE('',*,*,#35281,.T.);
#48893=ORIENTED_EDGE('',*,*,#35282,.F.);
#48894=ORIENTED_EDGE('',*,*,#35283,.T.);
#48895=ORIENTED_EDGE('',*,*,#35284,.T.);
#48896=ORIENTED_EDGE('',*,*,#35285,.T.);
#48897=ORIENTED_EDGE('',*,*,#35280,.F.);
#48898=ORIENTED_EDGE('',*,*,#35286,.T.);
#48899=ORIENTED_EDGE('',*,*,#35287,.T.);
#48900=ORIENTED_EDGE('',*,*,#35288,.T.);
#48901=ORIENTED_EDGE('',*,*,#35284,.F.);
#48902=ORIENTED_EDGE('',*,*,#35289,.T.);
#48903=ORIENTED_EDGE('',*,*,#35287,.F.);
#48904=ORIENTED_EDGE('',*,*,#35290,.T.);
#48905=ORIENTED_EDGE('',*,*,#35282,.T.);
#48906=ORIENTED_EDGE('',*,*,#35289,.F.);
#48907=ORIENTED_EDGE('',*,*,#35291,.F.);
#48908=ORIENTED_EDGE('',*,*,#35292,.F.);
#48909=ORIENTED_EDGE('',*,*,#35293,.T.);
#48910=ORIENTED_EDGE('',*,*,#35281,.F.);
#48911=ORIENTED_EDGE('',*,*,#35294,.F.);
#48912=ORIENTED_EDGE('',*,*,#35295,.F.);
#48913=ORIENTED_EDGE('',*,*,#35291,.T.);
#48914=ORIENTED_EDGE('',*,*,#35279,.F.);
#48915=ORIENTED_EDGE('',*,*,#35290,.F.);
#48916=ORIENTED_EDGE('',*,*,#35286,.F.);
#48917=ORIENTED_EDGE('',*,*,#35283,.F.);
#48918=ORIENTED_EDGE('',*,*,#35296,.T.);
#48919=ORIENTED_EDGE('',*,*,#35297,.T.);
#48920=ORIENTED_EDGE('',*,*,#35295,.T.);
#48921=ORIENTED_EDGE('',*,*,#35298,.F.);
#48922=ORIENTED_EDGE('',*,*,#35299,.T.);
#48923=ORIENTED_EDGE('',*,*,#35300,.T.);
#48924=ORIENTED_EDGE('',*,*,#35292,.T.);
#48925=ORIENTED_EDGE('',*,*,#35297,.F.);
#48926=ORIENTED_EDGE('',*,*,#35301,.T.);
#48927=ORIENTED_EDGE('',*,*,#35302,.T.);
#48928=ORIENTED_EDGE('',*,*,#35303,.T.);
#48929=ORIENTED_EDGE('',*,*,#35298,.T.);
#48930=ORIENTED_EDGE('',*,*,#35304,.T.);
#48931=ORIENTED_EDGE('',*,*,#35302,.F.);
#48932=ORIENTED_EDGE('',*,*,#35305,.T.);
#48933=ORIENTED_EDGE('',*,*,#35300,.F.);
#48934=ORIENTED_EDGE('',*,*,#35285,.F.);
#48935=ORIENTED_EDGE('',*,*,#35306,.F.);
#48936=ORIENTED_EDGE('',*,*,#35301,.F.);
#48937=ORIENTED_EDGE('',*,*,#35294,.T.);
#48938=ORIENTED_EDGE('',*,*,#35273,.T.);
#48939=ORIENTED_EDGE('',*,*,#35275,.T.);
#48940=ORIENTED_EDGE('',*,*,#35277,.T.);
#48941=ORIENTED_EDGE('',*,*,#35296,.F.);
#48942=ORIENTED_EDGE('',*,*,#35303,.F.);
#48943=ORIENTED_EDGE('',*,*,#35304,.F.);
#48944=ORIENTED_EDGE('',*,*,#35299,.F.);
#48945=ORIENTED_EDGE('',*,*,#35288,.F.);
#48946=ORIENTED_EDGE('',*,*,#35293,.F.);
#48947=ORIENTED_EDGE('',*,*,#35305,.F.);
#48948=ORIENTED_EDGE('',*,*,#35306,.T.);
#48949=ORIENTED_EDGE('',*,*,#35307,.F.);
#48950=ORIENTED_EDGE('',*,*,#35308,.T.);
#48951=ORIENTED_EDGE('',*,*,#35309,.F.);
#48952=ORIENTED_EDGE('',*,*,#35310,.T.);
#48953=ORIENTED_EDGE('',*,*,#35311,.F.);
#48954=ORIENTED_EDGE('',*,*,#35310,.F.);
#48955=ORIENTED_EDGE('',*,*,#35312,.F.);
#48956=ORIENTED_EDGE('',*,*,#35308,.F.);
#48957=ORIENTED_EDGE('',*,*,#35313,.F.);
#48958=ORIENTED_EDGE('',*,*,#35314,.T.);
#48959=ORIENTED_EDGE('',*,*,#35315,.F.);
#48960=ORIENTED_EDGE('',*,*,#35316,.T.);
#48961=ORIENTED_EDGE('',*,*,#35317,.F.);
#48962=ORIENTED_EDGE('',*,*,#35316,.F.);
#48963=ORIENTED_EDGE('',*,*,#35318,.F.);
#48964=ORIENTED_EDGE('',*,*,#35314,.F.);
#48965=ORIENTED_EDGE('',*,*,#35319,.F.);
#48966=ORIENTED_EDGE('',*,*,#35320,.F.);
#48967=ORIENTED_EDGE('',*,*,#35321,.T.);
#48968=ORIENTED_EDGE('',*,*,#35319,.T.);
#48969=ORIENTED_EDGE('',*,*,#35321,.F.);
#48970=ORIENTED_EDGE('',*,*,#35322,.F.);
#48971=ORIENTED_EDGE('',*,*,#35323,.T.);
#48972=ORIENTED_EDGE('',*,*,#35320,.T.);
#48973=ORIENTED_EDGE('',*,*,#35323,.F.);
#48974=ORIENTED_EDGE('',*,*,#35309,.T.);
#48975=ORIENTED_EDGE('',*,*,#35311,.T.);
#48976=ORIENTED_EDGE('',*,*,#35307,.T.);
#48977=ORIENTED_EDGE('',*,*,#35312,.T.);
#48978=ORIENTED_EDGE('',*,*,#35315,.T.);
#48979=ORIENTED_EDGE('',*,*,#35317,.T.);
#48980=ORIENTED_EDGE('',*,*,#35313,.T.);
#48981=ORIENTED_EDGE('',*,*,#35318,.T.);
#48982=ORIENTED_EDGE('',*,*,#35324,.F.);
#48983=ORIENTED_EDGE('',*,*,#35325,.T.);
#48984=ORIENTED_EDGE('',*,*,#35322,.T.);
#48985=ORIENTED_EDGE('',*,*,#35325,.F.);
#48986=ORIENTED_EDGE('',*,*,#35324,.T.);
#48987=ORIENTED_EDGE('',*,*,#35326,.F.);
#48988=ORIENTED_EDGE('',*,*,#35327,.F.);
#48989=ORIENTED_EDGE('',*,*,#35328,.F.);
#48990=ORIENTED_EDGE('',*,*,#35329,.F.);
#48991=ORIENTED_EDGE('',*,*,#35330,.F.);
#48992=ORIENTED_EDGE('',*,*,#35331,.T.);
#48993=ORIENTED_EDGE('',*,*,#35332,.T.);
#48994=ORIENTED_EDGE('',*,*,#35333,.F.);
#48995=ORIENTED_EDGE('',*,*,#35327,.T.);
#48996=ORIENTED_EDGE('',*,*,#35334,.F.);
#48997=ORIENTED_EDGE('',*,*,#35335,.T.);
#48998=ORIENTED_EDGE('',*,*,#35331,.F.);
#48999=ORIENTED_EDGE('',*,*,#35336,.F.);
#49000=ORIENTED_EDGE('',*,*,#35332,.F.);
#49001=ORIENTED_EDGE('',*,*,#35335,.F.);
#49002=ORIENTED_EDGE('',*,*,#35337,.F.);
#49003=ORIENTED_EDGE('',*,*,#35338,.F.);
#49004=ORIENTED_EDGE('',*,*,#35339,.T.);
#49005=ORIENTED_EDGE('',*,*,#35340,.F.);
#49006=ORIENTED_EDGE('',*,*,#35341,.F.);
#49007=ORIENTED_EDGE('',*,*,#35342,.F.);
#49008=ORIENTED_EDGE('',*,*,#35343,.F.);
#49009=ORIENTED_EDGE('',*,*,#35344,.F.);
#49010=ORIENTED_EDGE('',*,*,#35345,.F.);
#49011=ORIENTED_EDGE('',*,*,#35343,.T.);
#49012=ORIENTED_EDGE('',*,*,#35346,.F.);
#49013=ORIENTED_EDGE('',*,*,#35347,.F.);
#49014=ORIENTED_EDGE('',*,*,#35348,.F.);
#49015=ORIENTED_EDGE('',*,*,#35347,.T.);
#49016=ORIENTED_EDGE('',*,*,#35349,.F.);
#49017=ORIENTED_EDGE('',*,*,#35350,.F.);
#49018=ORIENTED_EDGE('',*,*,#35351,.T.);
#49019=ORIENTED_EDGE('',*,*,#35350,.T.);
#49020=ORIENTED_EDGE('',*,*,#35352,.F.);
#49021=ORIENTED_EDGE('',*,*,#35339,.F.);
#49022=ORIENTED_EDGE('',*,*,#35353,.F.);
#49023=ORIENTED_EDGE('',*,*,#35344,.T.);
#49024=ORIENTED_EDGE('',*,*,#35345,.T.);
#49025=ORIENTED_EDGE('',*,*,#35348,.T.);
#49026=ORIENTED_EDGE('',*,*,#35351,.F.);
#49027=ORIENTED_EDGE('',*,*,#35338,.T.);
#49028=ORIENTED_EDGE('',*,*,#35354,.F.);
#49029=ORIENTED_EDGE('',*,*,#35355,.T.);
#49030=ORIENTED_EDGE('',*,*,#35356,.T.);
#49031=ORIENTED_EDGE('',*,*,#35357,.T.);
#49032=ORIENTED_EDGE('',*,*,#35358,.T.);
#49033=ORIENTED_EDGE('',*,*,#35359,.T.);
#49034=ORIENTED_EDGE('',*,*,#35360,.T.);
#49035=ORIENTED_EDGE('',*,*,#35361,.T.);
#49036=ORIENTED_EDGE('',*,*,#35362,.T.);
#49037=ORIENTED_EDGE('',*,*,#35363,.T.);
#49038=ORIENTED_EDGE('',*,*,#35364,.T.);
#49039=ORIENTED_EDGE('',*,*,#35365,.T.);
#49040=ORIENTED_EDGE('',*,*,#35366,.T.);
#49041=ORIENTED_EDGE('',*,*,#35341,.T.);
#49042=ORIENTED_EDGE('',*,*,#35353,.T.);
#49043=ORIENTED_EDGE('',*,*,#35337,.T.);
#49044=ORIENTED_EDGE('',*,*,#35367,.T.);
#49045=ORIENTED_EDGE('',*,*,#35368,.T.);
#49046=ORIENTED_EDGE('',*,*,#35369,.T.);
#49047=ORIENTED_EDGE('',*,*,#35370,.T.);
#49048=ORIENTED_EDGE('',*,*,#35371,.T.);
#49049=ORIENTED_EDGE('',*,*,#35372,.T.);
#49050=ORIENTED_EDGE('',*,*,#35373,.T.);
#49051=ORIENTED_EDGE('',*,*,#35374,.T.);
#49052=ORIENTED_EDGE('',*,*,#35375,.T.);
#49053=ORIENTED_EDGE('',*,*,#35376,.T.);
#49054=ORIENTED_EDGE('',*,*,#35377,.T.);
#49055=ORIENTED_EDGE('',*,*,#35378,.T.);
#49056=ORIENTED_EDGE('',*,*,#35379,.T.);
#49057=ORIENTED_EDGE('',*,*,#35380,.T.);
#49058=ORIENTED_EDGE('',*,*,#35381,.T.);
#49059=ORIENTED_EDGE('',*,*,#35382,.T.);
#49060=ORIENTED_EDGE('',*,*,#35383,.T.);
#49061=ORIENTED_EDGE('',*,*,#35384,.T.);
#49062=ORIENTED_EDGE('',*,*,#35385,.T.);
#49063=ORIENTED_EDGE('',*,*,#35386,.T.);
#49064=ORIENTED_EDGE('',*,*,#35387,.T.);
#49065=ORIENTED_EDGE('',*,*,#35388,.T.);
#49066=ORIENTED_EDGE('',*,*,#35389,.T.);
#49067=ORIENTED_EDGE('',*,*,#35390,.T.);
#49068=ORIENTED_EDGE('',*,*,#35391,.T.);
#49069=ORIENTED_EDGE('',*,*,#35392,.T.);
#49070=ORIENTED_EDGE('',*,*,#35393,.T.);
#49071=ORIENTED_EDGE('',*,*,#35394,.T.);
#49072=ORIENTED_EDGE('',*,*,#35395,.T.);
#49073=ORIENTED_EDGE('',*,*,#35396,.T.);
#49074=ORIENTED_EDGE('',*,*,#35397,.T.);
#49075=ORIENTED_EDGE('',*,*,#35398,.T.);
#49076=ORIENTED_EDGE('',*,*,#35399,.T.);
#49077=ORIENTED_EDGE('',*,*,#35400,.T.);
#49078=ORIENTED_EDGE('',*,*,#35401,.T.);
#49079=ORIENTED_EDGE('',*,*,#35402,.T.);
#49080=ORIENTED_EDGE('',*,*,#35403,.T.);
#49081=ORIENTED_EDGE('',*,*,#35404,.T.);
#49082=ORIENTED_EDGE('',*,*,#35405,.T.);
#49083=ORIENTED_EDGE('',*,*,#35406,.T.);
#49084=ORIENTED_EDGE('',*,*,#35407,.T.);
#49085=ORIENTED_EDGE('',*,*,#35408,.T.);
#49086=ORIENTED_EDGE('',*,*,#35409,.T.);
#49087=ORIENTED_EDGE('',*,*,#35410,.T.);
#49088=ORIENTED_EDGE('',*,*,#35411,.T.);
#49089=ORIENTED_EDGE('',*,*,#35412,.T.);
#49090=ORIENTED_EDGE('',*,*,#35413,.T.);
#49091=ORIENTED_EDGE('',*,*,#35414,.T.);
#49092=ORIENTED_EDGE('',*,*,#35415,.T.);
#49093=ORIENTED_EDGE('',*,*,#35416,.T.);
#49094=ORIENTED_EDGE('',*,*,#35417,.T.);
#49095=ORIENTED_EDGE('',*,*,#35355,.F.);
#49096=ORIENTED_EDGE('',*,*,#35365,.F.);
#49097=ORIENTED_EDGE('',*,*,#35418,.F.);
#49098=ORIENTED_EDGE('',*,*,#35419,.T.);
#49099=ORIENTED_EDGE('',*,*,#35420,.F.);
#49100=ORIENTED_EDGE('',*,*,#35363,.F.);
#49101=ORIENTED_EDGE('',*,*,#35421,.F.);
#49102=ORIENTED_EDGE('',*,*,#35422,.F.);
#49103=ORIENTED_EDGE('',*,*,#35423,.F.);
#49104=ORIENTED_EDGE('',*,*,#35424,.F.);
#49105=ORIENTED_EDGE('',*,*,#35422,.T.);
#49106=ORIENTED_EDGE('',*,*,#35425,.F.);
#49107=ORIENTED_EDGE('',*,*,#35426,.F.);
#49108=ORIENTED_EDGE('',*,*,#35427,.F.);
#49109=ORIENTED_EDGE('',*,*,#35426,.T.);
#49110=ORIENTED_EDGE('',*,*,#35428,.F.);
#49111=ORIENTED_EDGE('',*,*,#35429,.F.);
#49112=ORIENTED_EDGE('',*,*,#35430,.T.);
#49113=ORIENTED_EDGE('',*,*,#35429,.T.);
#49114=ORIENTED_EDGE('',*,*,#35431,.F.);
#49115=ORIENTED_EDGE('',*,*,#35419,.F.);
#49116=ORIENTED_EDGE('',*,*,#35364,.F.);
#49117=ORIENTED_EDGE('',*,*,#35423,.T.);
#49118=ORIENTED_EDGE('',*,*,#35424,.T.);
#49119=ORIENTED_EDGE('',*,*,#35427,.T.);
#49120=ORIENTED_EDGE('',*,*,#35430,.F.);
#49121=ORIENTED_EDGE('',*,*,#35418,.T.);
#49122=ORIENTED_EDGE('',*,*,#35361,.F.);
#49123=ORIENTED_EDGE('',*,*,#35432,.F.);
#49124=ORIENTED_EDGE('',*,*,#35433,.T.);
#49125=ORIENTED_EDGE('',*,*,#35434,.F.);
#49126=ORIENTED_EDGE('',*,*,#35359,.F.);
#49127=ORIENTED_EDGE('',*,*,#35435,.F.);
#49128=ORIENTED_EDGE('',*,*,#35436,.F.);
#49129=ORIENTED_EDGE('',*,*,#35437,.F.);
#49130=ORIENTED_EDGE('',*,*,#35438,.F.);
#49131=ORIENTED_EDGE('',*,*,#35436,.T.);
#49132=ORIENTED_EDGE('',*,*,#35439,.F.);
#49133=ORIENTED_EDGE('',*,*,#35440,.F.);
#49134=ORIENTED_EDGE('',*,*,#35441,.F.);
#49135=ORIENTED_EDGE('',*,*,#35440,.T.);
#49136=ORIENTED_EDGE('',*,*,#35442,.F.);
#49137=ORIENTED_EDGE('',*,*,#35443,.F.);
#49138=ORIENTED_EDGE('',*,*,#35444,.T.);
#49139=ORIENTED_EDGE('',*,*,#35443,.T.);
#49140=ORIENTED_EDGE('',*,*,#35445,.F.);
#49141=ORIENTED_EDGE('',*,*,#35433,.F.);
#49142=ORIENTED_EDGE('',*,*,#35360,.F.);
#49143=ORIENTED_EDGE('',*,*,#35437,.T.);
#49144=ORIENTED_EDGE('',*,*,#35438,.T.);
#49145=ORIENTED_EDGE('',*,*,#35441,.T.);
#49146=ORIENTED_EDGE('',*,*,#35444,.F.);
#49147=ORIENTED_EDGE('',*,*,#35432,.T.);
#49148=ORIENTED_EDGE('',*,*,#35357,.F.);
#49149=ORIENTED_EDGE('',*,*,#35446,.F.);
#49150=ORIENTED_EDGE('',*,*,#35447,.T.);
#49151=ORIENTED_EDGE('',*,*,#35448,.F.);
#49152=ORIENTED_EDGE('',*,*,#35416,.F.);
#49153=ORIENTED_EDGE('',*,*,#35449,.F.);
#49154=ORIENTED_EDGE('',*,*,#35450,.F.);
#49155=ORIENTED_EDGE('',*,*,#35451,.F.);
#49156=ORIENTED_EDGE('',*,*,#35452,.F.);
#49157=ORIENTED_EDGE('',*,*,#35450,.T.);
#49158=ORIENTED_EDGE('',*,*,#35453,.F.);
#49159=ORIENTED_EDGE('',*,*,#35454,.F.);
#49160=ORIENTED_EDGE('',*,*,#35455,.F.);
#49161=ORIENTED_EDGE('',*,*,#35454,.T.);
#49162=ORIENTED_EDGE('',*,*,#35456,.F.);
#49163=ORIENTED_EDGE('',*,*,#35457,.F.);
#49164=ORIENTED_EDGE('',*,*,#35458,.T.);
#49165=ORIENTED_EDGE('',*,*,#35457,.T.);
#49166=ORIENTED_EDGE('',*,*,#35459,.F.);
#49167=ORIENTED_EDGE('',*,*,#35447,.F.);
#49168=ORIENTED_EDGE('',*,*,#35417,.F.);
#49169=ORIENTED_EDGE('',*,*,#35451,.T.);
#49170=ORIENTED_EDGE('',*,*,#35452,.T.);
#49171=ORIENTED_EDGE('',*,*,#35455,.T.);
#49172=ORIENTED_EDGE('',*,*,#35458,.F.);
#49173=ORIENTED_EDGE('',*,*,#35446,.T.);
#49174=ORIENTED_EDGE('',*,*,#35356,.F.);
#49175=ORIENTED_EDGE('',*,*,#35414,.F.);
#49176=ORIENTED_EDGE('',*,*,#35460,.F.);
#49177=ORIENTED_EDGE('',*,*,#35461,.T.);
#49178=ORIENTED_EDGE('',*,*,#35462,.F.);
#49179=ORIENTED_EDGE('',*,*,#35412,.F.);
#49180=ORIENTED_EDGE('',*,*,#35463,.F.);
#49181=ORIENTED_EDGE('',*,*,#35464,.F.);
#49182=ORIENTED_EDGE('',*,*,#35465,.F.);
#49183=ORIENTED_EDGE('',*,*,#35466,.F.);
#49184=ORIENTED_EDGE('',*,*,#35464,.T.);
#49185=ORIENTED_EDGE('',*,*,#35467,.F.);
#49186=ORIENTED_EDGE('',*,*,#35468,.F.);
#49187=ORIENTED_EDGE('',*,*,#35469,.F.);
#49188=ORIENTED_EDGE('',*,*,#35468,.T.);
#49189=ORIENTED_EDGE('',*,*,#35470,.F.);
#49190=ORIENTED_EDGE('',*,*,#35471,.F.);
#49191=ORIENTED_EDGE('',*,*,#35472,.T.);
#49192=ORIENTED_EDGE('',*,*,#35471,.T.);
#49193=ORIENTED_EDGE('',*,*,#35473,.F.);
#49194=ORIENTED_EDGE('',*,*,#35461,.F.);
#49195=ORIENTED_EDGE('',*,*,#35413,.F.);
#49196=ORIENTED_EDGE('',*,*,#35465,.T.);
#49197=ORIENTED_EDGE('',*,*,#35466,.T.);
#49198=ORIENTED_EDGE('',*,*,#35469,.T.);
#49199=ORIENTED_EDGE('',*,*,#35472,.F.);
#49200=ORIENTED_EDGE('',*,*,#35460,.T.);
#49201=ORIENTED_EDGE('',*,*,#35410,.F.);
#49202=ORIENTED_EDGE('',*,*,#35474,.F.);
#49203=ORIENTED_EDGE('',*,*,#35475,.T.);
#49204=ORIENTED_EDGE('',*,*,#35476,.F.);
#49205=ORIENTED_EDGE('',*,*,#35408,.F.);
#49206=ORIENTED_EDGE('',*,*,#35477,.F.);
#49207=ORIENTED_EDGE('',*,*,#35478,.F.);
#49208=ORIENTED_EDGE('',*,*,#35479,.F.);
#49209=ORIENTED_EDGE('',*,*,#35480,.F.);
#49210=ORIENTED_EDGE('',*,*,#35478,.T.);
#49211=ORIENTED_EDGE('',*,*,#35481,.F.);
#49212=ORIENTED_EDGE('',*,*,#35482,.F.);
#49213=ORIENTED_EDGE('',*,*,#35483,.F.);
#49214=ORIENTED_EDGE('',*,*,#35482,.T.);
#49215=ORIENTED_EDGE('',*,*,#35484,.F.);
#49216=ORIENTED_EDGE('',*,*,#35485,.F.);
#49217=ORIENTED_EDGE('',*,*,#35486,.T.);
#49218=ORIENTED_EDGE('',*,*,#35485,.T.);
#49219=ORIENTED_EDGE('',*,*,#35487,.F.);
#49220=ORIENTED_EDGE('',*,*,#35475,.F.);
#49221=ORIENTED_EDGE('',*,*,#35409,.F.);
#49222=ORIENTED_EDGE('',*,*,#35479,.T.);
#49223=ORIENTED_EDGE('',*,*,#35480,.T.);
#49224=ORIENTED_EDGE('',*,*,#35483,.T.);
#49225=ORIENTED_EDGE('',*,*,#35486,.F.);
#49226=ORIENTED_EDGE('',*,*,#35474,.T.);
#49227=ORIENTED_EDGE('',*,*,#35406,.F.);
#49228=ORIENTED_EDGE('',*,*,#35488,.F.);
#49229=ORIENTED_EDGE('',*,*,#35489,.T.);
#49230=ORIENTED_EDGE('',*,*,#35490,.F.);
#49231=ORIENTED_EDGE('',*,*,#35404,.F.);
#49232=ORIENTED_EDGE('',*,*,#35491,.F.);
#49233=ORIENTED_EDGE('',*,*,#35492,.F.);
#49234=ORIENTED_EDGE('',*,*,#35493,.F.);
#49235=ORIENTED_EDGE('',*,*,#35494,.F.);
#49236=ORIENTED_EDGE('',*,*,#35492,.T.);
#49237=ORIENTED_EDGE('',*,*,#35495,.F.);
#49238=ORIENTED_EDGE('',*,*,#35496,.F.);
#49239=ORIENTED_EDGE('',*,*,#35497,.F.);
#49240=ORIENTED_EDGE('',*,*,#35496,.T.);
#49241=ORIENTED_EDGE('',*,*,#35498,.F.);
#49242=ORIENTED_EDGE('',*,*,#35499,.F.);
#49243=ORIENTED_EDGE('',*,*,#35500,.T.);
#49244=ORIENTED_EDGE('',*,*,#35499,.T.);
#49245=ORIENTED_EDGE('',*,*,#35501,.F.);
#49246=ORIENTED_EDGE('',*,*,#35489,.F.);
#49247=ORIENTED_EDGE('',*,*,#35405,.F.);
#49248=ORIENTED_EDGE('',*,*,#35493,.T.);
#49249=ORIENTED_EDGE('',*,*,#35494,.T.);
#49250=ORIENTED_EDGE('',*,*,#35497,.T.);
#49251=ORIENTED_EDGE('',*,*,#35500,.F.);
#49252=ORIENTED_EDGE('',*,*,#35488,.T.);
#49253=ORIENTED_EDGE('',*,*,#35402,.F.);
#49254=ORIENTED_EDGE('',*,*,#35502,.F.);
#49255=ORIENTED_EDGE('',*,*,#35503,.T.);
#49256=ORIENTED_EDGE('',*,*,#35504,.F.);
#49257=ORIENTED_EDGE('',*,*,#35400,.F.);
#49258=ORIENTED_EDGE('',*,*,#35505,.F.);
#49259=ORIENTED_EDGE('',*,*,#35506,.F.);
#49260=ORIENTED_EDGE('',*,*,#35507,.F.);
#49261=ORIENTED_EDGE('',*,*,#35508,.F.);
#49262=ORIENTED_EDGE('',*,*,#35506,.T.);
#49263=ORIENTED_EDGE('',*,*,#35509,.F.);
#49264=ORIENTED_EDGE('',*,*,#35510,.F.);
#49265=ORIENTED_EDGE('',*,*,#35511,.F.);
#49266=ORIENTED_EDGE('',*,*,#35510,.T.);
#49267=ORIENTED_EDGE('',*,*,#35512,.F.);
#49268=ORIENTED_EDGE('',*,*,#35513,.F.);
#49269=ORIENTED_EDGE('',*,*,#35514,.T.);
#49270=ORIENTED_EDGE('',*,*,#35513,.T.);
#49271=ORIENTED_EDGE('',*,*,#35515,.F.);
#49272=ORIENTED_EDGE('',*,*,#35503,.F.);
#49273=ORIENTED_EDGE('',*,*,#35401,.F.);
#49274=ORIENTED_EDGE('',*,*,#35507,.T.);
#49275=ORIENTED_EDGE('',*,*,#35508,.T.);
#49276=ORIENTED_EDGE('',*,*,#35511,.T.);
#49277=ORIENTED_EDGE('',*,*,#35514,.F.);
#49278=ORIENTED_EDGE('',*,*,#35502,.T.);
#49279=ORIENTED_EDGE('',*,*,#35398,.F.);
#49280=ORIENTED_EDGE('',*,*,#35516,.F.);
#49281=ORIENTED_EDGE('',*,*,#35517,.T.);
#49282=ORIENTED_EDGE('',*,*,#35518,.F.);
#49283=ORIENTED_EDGE('',*,*,#35396,.F.);
#49284=ORIENTED_EDGE('',*,*,#35519,.F.);
#49285=ORIENTED_EDGE('',*,*,#35520,.F.);
#49286=ORIENTED_EDGE('',*,*,#35521,.F.);
#49287=ORIENTED_EDGE('',*,*,#35522,.F.);
#49288=ORIENTED_EDGE('',*,*,#35520,.T.);
#49289=ORIENTED_EDGE('',*,*,#35523,.F.);
#49290=ORIENTED_EDGE('',*,*,#35524,.F.);
#49291=ORIENTED_EDGE('',*,*,#35525,.F.);
#49292=ORIENTED_EDGE('',*,*,#35524,.T.);
#49293=ORIENTED_EDGE('',*,*,#35526,.F.);
#49294=ORIENTED_EDGE('',*,*,#35527,.F.);
#49295=ORIENTED_EDGE('',*,*,#35528,.T.);
#49296=ORIENTED_EDGE('',*,*,#35527,.T.);
#49297=ORIENTED_EDGE('',*,*,#35529,.F.);
#49298=ORIENTED_EDGE('',*,*,#35517,.F.);
#49299=ORIENTED_EDGE('',*,*,#35397,.F.);
#49300=ORIENTED_EDGE('',*,*,#35521,.T.);
#49301=ORIENTED_EDGE('',*,*,#35522,.T.);
#49302=ORIENTED_EDGE('',*,*,#35525,.T.);
#49303=ORIENTED_EDGE('',*,*,#35528,.F.);
#49304=ORIENTED_EDGE('',*,*,#35516,.T.);
#49305=ORIENTED_EDGE('',*,*,#35394,.F.);
#49306=ORIENTED_EDGE('',*,*,#35530,.F.);
#49307=ORIENTED_EDGE('',*,*,#35531,.T.);
#49308=ORIENTED_EDGE('',*,*,#35532,.F.);
#49309=ORIENTED_EDGE('',*,*,#35392,.F.);
#49310=ORIENTED_EDGE('',*,*,#35533,.F.);
#49311=ORIENTED_EDGE('',*,*,#35534,.F.);
#49312=ORIENTED_EDGE('',*,*,#35535,.F.);
#49313=ORIENTED_EDGE('',*,*,#35536,.F.);
#49314=ORIENTED_EDGE('',*,*,#35534,.T.);
#49315=ORIENTED_EDGE('',*,*,#35537,.F.);
#49316=ORIENTED_EDGE('',*,*,#35538,.F.);
#49317=ORIENTED_EDGE('',*,*,#35539,.F.);
#49318=ORIENTED_EDGE('',*,*,#35538,.T.);
#49319=ORIENTED_EDGE('',*,*,#35540,.F.);
#49320=ORIENTED_EDGE('',*,*,#35541,.F.);
#49321=ORIENTED_EDGE('',*,*,#35542,.T.);
#49322=ORIENTED_EDGE('',*,*,#35541,.T.);
#49323=ORIENTED_EDGE('',*,*,#35543,.F.);
#49324=ORIENTED_EDGE('',*,*,#35531,.F.);
#49325=ORIENTED_EDGE('',*,*,#35393,.F.);
#49326=ORIENTED_EDGE('',*,*,#35535,.T.);
#49327=ORIENTED_EDGE('',*,*,#35536,.T.);
#49328=ORIENTED_EDGE('',*,*,#35539,.T.);
#49329=ORIENTED_EDGE('',*,*,#35542,.F.);
#49330=ORIENTED_EDGE('',*,*,#35530,.T.);
#49331=ORIENTED_EDGE('',*,*,#35390,.F.);
#49332=ORIENTED_EDGE('',*,*,#35544,.F.);
#49333=ORIENTED_EDGE('',*,*,#35545,.T.);
#49334=ORIENTED_EDGE('',*,*,#35546,.F.);
#49335=ORIENTED_EDGE('',*,*,#35388,.F.);
#49336=ORIENTED_EDGE('',*,*,#35547,.F.);
#49337=ORIENTED_EDGE('',*,*,#35548,.F.);
#49338=ORIENTED_EDGE('',*,*,#35549,.F.);
#49339=ORIENTED_EDGE('',*,*,#35550,.F.);
#49340=ORIENTED_EDGE('',*,*,#35548,.T.);
#49341=ORIENTED_EDGE('',*,*,#35551,.F.);
#49342=ORIENTED_EDGE('',*,*,#35552,.F.);
#49343=ORIENTED_EDGE('',*,*,#35553,.F.);
#49344=ORIENTED_EDGE('',*,*,#35552,.T.);
#49345=ORIENTED_EDGE('',*,*,#35554,.F.);
#49346=ORIENTED_EDGE('',*,*,#35555,.F.);
#49347=ORIENTED_EDGE('',*,*,#35556,.T.);
#49348=ORIENTED_EDGE('',*,*,#35555,.T.);
#49349=ORIENTED_EDGE('',*,*,#35557,.F.);
#49350=ORIENTED_EDGE('',*,*,#35545,.F.);
#49351=ORIENTED_EDGE('',*,*,#35389,.F.);
#49352=ORIENTED_EDGE('',*,*,#35549,.T.);
#49353=ORIENTED_EDGE('',*,*,#35550,.T.);
#49354=ORIENTED_EDGE('',*,*,#35553,.T.);
#49355=ORIENTED_EDGE('',*,*,#35556,.F.);
#49356=ORIENTED_EDGE('',*,*,#35544,.T.);
#49357=ORIENTED_EDGE('',*,*,#35386,.F.);
#49358=ORIENTED_EDGE('',*,*,#35558,.F.);
#49359=ORIENTED_EDGE('',*,*,#35559,.T.);
#49360=ORIENTED_EDGE('',*,*,#35560,.F.);
#49361=ORIENTED_EDGE('',*,*,#35384,.F.);
#49362=ORIENTED_EDGE('',*,*,#35561,.F.);
#49363=ORIENTED_EDGE('',*,*,#35562,.F.);
#49364=ORIENTED_EDGE('',*,*,#35563,.F.);
#49365=ORIENTED_EDGE('',*,*,#35564,.F.);
#49366=ORIENTED_EDGE('',*,*,#35562,.T.);
#49367=ORIENTED_EDGE('',*,*,#35565,.F.);
#49368=ORIENTED_EDGE('',*,*,#35566,.F.);
#49369=ORIENTED_EDGE('',*,*,#35567,.F.);
#49370=ORIENTED_EDGE('',*,*,#35566,.T.);
#49371=ORIENTED_EDGE('',*,*,#35568,.F.);
#49372=ORIENTED_EDGE('',*,*,#35569,.F.);
#49373=ORIENTED_EDGE('',*,*,#35570,.T.);
#49374=ORIENTED_EDGE('',*,*,#35569,.T.);
#49375=ORIENTED_EDGE('',*,*,#35571,.F.);
#49376=ORIENTED_EDGE('',*,*,#35559,.F.);
#49377=ORIENTED_EDGE('',*,*,#35385,.F.);
#49378=ORIENTED_EDGE('',*,*,#35563,.T.);
#49379=ORIENTED_EDGE('',*,*,#35564,.T.);
#49380=ORIENTED_EDGE('',*,*,#35567,.T.);
#49381=ORIENTED_EDGE('',*,*,#35570,.F.);
#49382=ORIENTED_EDGE('',*,*,#35558,.T.);
#49383=ORIENTED_EDGE('',*,*,#35382,.F.);
#49384=ORIENTED_EDGE('',*,*,#35572,.F.);
#49385=ORIENTED_EDGE('',*,*,#35573,.T.);
#49386=ORIENTED_EDGE('',*,*,#35574,.F.);
#49387=ORIENTED_EDGE('',*,*,#35380,.F.);
#49388=ORIENTED_EDGE('',*,*,#35575,.F.);
#49389=ORIENTED_EDGE('',*,*,#35576,.F.);
#49390=ORIENTED_EDGE('',*,*,#35577,.F.);
#49391=ORIENTED_EDGE('',*,*,#35578,.F.);
#49392=ORIENTED_EDGE('',*,*,#35576,.T.);
#49393=ORIENTED_EDGE('',*,*,#35579,.F.);
#49394=ORIENTED_EDGE('',*,*,#35580,.F.);
#49395=ORIENTED_EDGE('',*,*,#35581,.F.);
#49396=ORIENTED_EDGE('',*,*,#35580,.T.);
#49397=ORIENTED_EDGE('',*,*,#35582,.F.);
#49398=ORIENTED_EDGE('',*,*,#35583,.F.);
#49399=ORIENTED_EDGE('',*,*,#35584,.T.);
#49400=ORIENTED_EDGE('',*,*,#35583,.T.);
#49401=ORIENTED_EDGE('',*,*,#35585,.F.);
#49402=ORIENTED_EDGE('',*,*,#35573,.F.);
#49403=ORIENTED_EDGE('',*,*,#35381,.F.);
#49404=ORIENTED_EDGE('',*,*,#35577,.T.);
#49405=ORIENTED_EDGE('',*,*,#35578,.T.);
#49406=ORIENTED_EDGE('',*,*,#35581,.T.);
#49407=ORIENTED_EDGE('',*,*,#35584,.F.);
#49408=ORIENTED_EDGE('',*,*,#35572,.T.);
#49409=ORIENTED_EDGE('',*,*,#35378,.F.);
#49410=ORIENTED_EDGE('',*,*,#35586,.F.);
#49411=ORIENTED_EDGE('',*,*,#35587,.T.);
#49412=ORIENTED_EDGE('',*,*,#35588,.F.);
#49413=ORIENTED_EDGE('',*,*,#35376,.F.);
#49414=ORIENTED_EDGE('',*,*,#35589,.F.);
#49415=ORIENTED_EDGE('',*,*,#35590,.F.);
#49416=ORIENTED_EDGE('',*,*,#35591,.F.);
#49417=ORIENTED_EDGE('',*,*,#35592,.F.);
#49418=ORIENTED_EDGE('',*,*,#35590,.T.);
#49419=ORIENTED_EDGE('',*,*,#35593,.F.);
#49420=ORIENTED_EDGE('',*,*,#35594,.F.);
#49421=ORIENTED_EDGE('',*,*,#35595,.F.);
#49422=ORIENTED_EDGE('',*,*,#35594,.T.);
#49423=ORIENTED_EDGE('',*,*,#35596,.F.);
#49424=ORIENTED_EDGE('',*,*,#35597,.F.);
#49425=ORIENTED_EDGE('',*,*,#35598,.T.);
#49426=ORIENTED_EDGE('',*,*,#35597,.T.);
#49427=ORIENTED_EDGE('',*,*,#35599,.F.);
#49428=ORIENTED_EDGE('',*,*,#35587,.F.);
#49429=ORIENTED_EDGE('',*,*,#35377,.F.);
#49430=ORIENTED_EDGE('',*,*,#35591,.T.);
#49431=ORIENTED_EDGE('',*,*,#35592,.T.);
#49432=ORIENTED_EDGE('',*,*,#35595,.T.);
#49433=ORIENTED_EDGE('',*,*,#35598,.F.);
#49434=ORIENTED_EDGE('',*,*,#35586,.T.);
#49435=ORIENTED_EDGE('',*,*,#35374,.F.);
#49436=ORIENTED_EDGE('',*,*,#35600,.F.);
#49437=ORIENTED_EDGE('',*,*,#35601,.T.);
#49438=ORIENTED_EDGE('',*,*,#35602,.F.);
#49439=ORIENTED_EDGE('',*,*,#35372,.F.);
#49440=ORIENTED_EDGE('',*,*,#35603,.F.);
#49441=ORIENTED_EDGE('',*,*,#35604,.F.);
#49442=ORIENTED_EDGE('',*,*,#35605,.F.);
#49443=ORIENTED_EDGE('',*,*,#35606,.F.);
#49444=ORIENTED_EDGE('',*,*,#35604,.T.);
#49445=ORIENTED_EDGE('',*,*,#35607,.F.);
#49446=ORIENTED_EDGE('',*,*,#35608,.F.);
#49447=ORIENTED_EDGE('',*,*,#35609,.F.);
#49448=ORIENTED_EDGE('',*,*,#35608,.T.);
#49449=ORIENTED_EDGE('',*,*,#35610,.F.);
#49450=ORIENTED_EDGE('',*,*,#35611,.F.);
#49451=ORIENTED_EDGE('',*,*,#35612,.T.);
#49452=ORIENTED_EDGE('',*,*,#35611,.T.);
#49453=ORIENTED_EDGE('',*,*,#35613,.F.);
#49454=ORIENTED_EDGE('',*,*,#35601,.F.);
#49455=ORIENTED_EDGE('',*,*,#35373,.F.);
#49456=ORIENTED_EDGE('',*,*,#35605,.T.);
#49457=ORIENTED_EDGE('',*,*,#35606,.T.);
#49458=ORIENTED_EDGE('',*,*,#35609,.T.);
#49459=ORIENTED_EDGE('',*,*,#35612,.F.);
#49460=ORIENTED_EDGE('',*,*,#35600,.T.);
#49461=ORIENTED_EDGE('',*,*,#35368,.F.);
#49462=ORIENTED_EDGE('',*,*,#35614,.F.);
#49463=ORIENTED_EDGE('',*,*,#35615,.F.);
#49464=ORIENTED_EDGE('',*,*,#35616,.F.);
#49465=ORIENTED_EDGE('',*,*,#35617,.F.);
#49466=ORIENTED_EDGE('',*,*,#35615,.T.);
#49467=ORIENTED_EDGE('',*,*,#35618,.F.);
#49468=ORIENTED_EDGE('',*,*,#35619,.F.);
#49469=ORIENTED_EDGE('',*,*,#35620,.F.);
#49470=ORIENTED_EDGE('',*,*,#35619,.T.);
#49471=ORIENTED_EDGE('',*,*,#35621,.F.);
#49472=ORIENTED_EDGE('',*,*,#35622,.F.);
#49473=ORIENTED_EDGE('',*,*,#35623,.T.);
#49474=ORIENTED_EDGE('',*,*,#35622,.T.);
#49475=ORIENTED_EDGE('',*,*,#35624,.F.);
#49476=ORIENTED_EDGE('',*,*,#35625,.F.);
#49477=ORIENTED_EDGE('',*,*,#35370,.F.);
#49478=ORIENTED_EDGE('',*,*,#35626,.F.);
#49479=ORIENTED_EDGE('',*,*,#35625,.T.);
#49480=ORIENTED_EDGE('',*,*,#35627,.F.);
#49481=ORIENTED_EDGE('',*,*,#35369,.F.);
#49482=ORIENTED_EDGE('',*,*,#35616,.T.);
#49483=ORIENTED_EDGE('',*,*,#35617,.T.);
#49484=ORIENTED_EDGE('',*,*,#35620,.T.);
#49485=ORIENTED_EDGE('',*,*,#35623,.F.);
#49486=ORIENTED_EDGE('',*,*,#35626,.T.);
#49487=ORIENTED_EDGE('',*,*,#35628,.T.);
#49488=ORIENTED_EDGE('',*,*,#35629,.T.);
#49489=ORIENTED_EDGE('',*,*,#35630,.F.);
#49490=ORIENTED_EDGE('',*,*,#35629,.F.);
#49491=ORIENTED_EDGE('',*,*,#35333,.T.);
#49492=ORIENTED_EDGE('',*,*,#35336,.T.);
#49493=ORIENTED_EDGE('',*,*,#35334,.T.);
#49494=ORIENTED_EDGE('',*,*,#35326,.T.);
#49495=ORIENTED_EDGE('',*,*,#35366,.F.);
#49496=ORIENTED_EDGE('',*,*,#35420,.T.);
#49497=ORIENTED_EDGE('',*,*,#35431,.T.);
#49498=ORIENTED_EDGE('',*,*,#35428,.T.);
#49499=ORIENTED_EDGE('',*,*,#35425,.T.);
#49500=ORIENTED_EDGE('',*,*,#35421,.T.);
#49501=ORIENTED_EDGE('',*,*,#35362,.F.);
#49502=ORIENTED_EDGE('',*,*,#35434,.T.);
#49503=ORIENTED_EDGE('',*,*,#35445,.T.);
#49504=ORIENTED_EDGE('',*,*,#35442,.T.);
#49505=ORIENTED_EDGE('',*,*,#35439,.T.);
#49506=ORIENTED_EDGE('',*,*,#35435,.T.);
#49507=ORIENTED_EDGE('',*,*,#35358,.F.);
#49508=ORIENTED_EDGE('',*,*,#35448,.T.);
#49509=ORIENTED_EDGE('',*,*,#35459,.T.);
#49510=ORIENTED_EDGE('',*,*,#35456,.T.);
#49511=ORIENTED_EDGE('',*,*,#35453,.T.);
#49512=ORIENTED_EDGE('',*,*,#35449,.T.);
#49513=ORIENTED_EDGE('',*,*,#35415,.F.);
#49514=ORIENTED_EDGE('',*,*,#35462,.T.);
#49515=ORIENTED_EDGE('',*,*,#35473,.T.);
#49516=ORIENTED_EDGE('',*,*,#35470,.T.);
#49517=ORIENTED_EDGE('',*,*,#35467,.T.);
#49518=ORIENTED_EDGE('',*,*,#35463,.T.);
#49519=ORIENTED_EDGE('',*,*,#35411,.F.);
#49520=ORIENTED_EDGE('',*,*,#35476,.T.);
#49521=ORIENTED_EDGE('',*,*,#35487,.T.);
#49522=ORIENTED_EDGE('',*,*,#35484,.T.);
#49523=ORIENTED_EDGE('',*,*,#35481,.T.);
#49524=ORIENTED_EDGE('',*,*,#35477,.T.);
#49525=ORIENTED_EDGE('',*,*,#35407,.F.);
#49526=ORIENTED_EDGE('',*,*,#35490,.T.);
#49527=ORIENTED_EDGE('',*,*,#35501,.T.);
#49528=ORIENTED_EDGE('',*,*,#35498,.T.);
#49529=ORIENTED_EDGE('',*,*,#35495,.T.);
#49530=ORIENTED_EDGE('',*,*,#35491,.T.);
#49531=ORIENTED_EDGE('',*,*,#35403,.F.);
#49532=ORIENTED_EDGE('',*,*,#35504,.T.);
#49533=ORIENTED_EDGE('',*,*,#35515,.T.);
#49534=ORIENTED_EDGE('',*,*,#35512,.T.);
#49535=ORIENTED_EDGE('',*,*,#35509,.T.);
#49536=ORIENTED_EDGE('',*,*,#35505,.T.);
#49537=ORIENTED_EDGE('',*,*,#35399,.F.);
#49538=ORIENTED_EDGE('',*,*,#35518,.T.);
#49539=ORIENTED_EDGE('',*,*,#35529,.T.);
#49540=ORIENTED_EDGE('',*,*,#35526,.T.);
#49541=ORIENTED_EDGE('',*,*,#35523,.T.);
#49542=ORIENTED_EDGE('',*,*,#35519,.T.);
#49543=ORIENTED_EDGE('',*,*,#35395,.F.);
#49544=ORIENTED_EDGE('',*,*,#35532,.T.);
#49545=ORIENTED_EDGE('',*,*,#35543,.T.);
#49546=ORIENTED_EDGE('',*,*,#35540,.T.);
#49547=ORIENTED_EDGE('',*,*,#35537,.T.);
#49548=ORIENTED_EDGE('',*,*,#35533,.T.);
#49549=ORIENTED_EDGE('',*,*,#35391,.F.);
#49550=ORIENTED_EDGE('',*,*,#35546,.T.);
#49551=ORIENTED_EDGE('',*,*,#35557,.T.);
#49552=ORIENTED_EDGE('',*,*,#35554,.T.);
#49553=ORIENTED_EDGE('',*,*,#35551,.T.);
#49554=ORIENTED_EDGE('',*,*,#35547,.T.);
#49555=ORIENTED_EDGE('',*,*,#35387,.F.);
#49556=ORIENTED_EDGE('',*,*,#35560,.T.);
#49557=ORIENTED_EDGE('',*,*,#35571,.T.);
#49558=ORIENTED_EDGE('',*,*,#35568,.T.);
#49559=ORIENTED_EDGE('',*,*,#35565,.T.);
#49560=ORIENTED_EDGE('',*,*,#35561,.T.);
#49561=ORIENTED_EDGE('',*,*,#35383,.F.);
#49562=ORIENTED_EDGE('',*,*,#35574,.T.);
#49563=ORIENTED_EDGE('',*,*,#35585,.T.);
#49564=ORIENTED_EDGE('',*,*,#35582,.T.);
#49565=ORIENTED_EDGE('',*,*,#35579,.T.);
#49566=ORIENTED_EDGE('',*,*,#35575,.T.);
#49567=ORIENTED_EDGE('',*,*,#35379,.F.);
#49568=ORIENTED_EDGE('',*,*,#35588,.T.);
#49569=ORIENTED_EDGE('',*,*,#35599,.T.);
#49570=ORIENTED_EDGE('',*,*,#35596,.T.);
#49571=ORIENTED_EDGE('',*,*,#35593,.T.);
#49572=ORIENTED_EDGE('',*,*,#35589,.T.);
#49573=ORIENTED_EDGE('',*,*,#35375,.F.);
#49574=ORIENTED_EDGE('',*,*,#35602,.T.);
#49575=ORIENTED_EDGE('',*,*,#35613,.T.);
#49576=ORIENTED_EDGE('',*,*,#35610,.T.);
#49577=ORIENTED_EDGE('',*,*,#35607,.T.);
#49578=ORIENTED_EDGE('',*,*,#35603,.T.);
#49579=ORIENTED_EDGE('',*,*,#35371,.F.);
#49580=ORIENTED_EDGE('',*,*,#35627,.T.);
#49581=ORIENTED_EDGE('',*,*,#35624,.T.);
#49582=ORIENTED_EDGE('',*,*,#35621,.T.);
#49583=ORIENTED_EDGE('',*,*,#35618,.T.);
#49584=ORIENTED_EDGE('',*,*,#35614,.T.);
#49585=ORIENTED_EDGE('',*,*,#35367,.F.);
#49586=ORIENTED_EDGE('',*,*,#35340,.T.);
#49587=ORIENTED_EDGE('',*,*,#35352,.T.);
#49588=ORIENTED_EDGE('',*,*,#35349,.T.);
#49589=ORIENTED_EDGE('',*,*,#35346,.T.);
#49590=ORIENTED_EDGE('',*,*,#35342,.T.);
#49591=ORIENTED_EDGE('',*,*,#35630,.T.);
#49592=ORIENTED_EDGE('',*,*,#35631,.F.);
#49593=ORIENTED_EDGE('',*,*,#35354,.T.);
#49594=ORIENTED_EDGE('',*,*,#35632,.F.);
#49595=ORIENTED_EDGE('',*,*,#35633,.T.);
#49596=ORIENTED_EDGE('',*,*,#35631,.T.);
#49597=ORIENTED_EDGE('',*,*,#35633,.F.);
#49598=ORIENTED_EDGE('',*,*,#35328,.T.);
#49599=ORIENTED_EDGE('',*,*,#35330,.T.);
#49600=ORIENTED_EDGE('',*,*,#35329,.T.);
#49601=ORIENTED_EDGE('',*,*,#35634,.F.);
#49602=ORIENTED_EDGE('',*,*,#35635,.T.);
#49603=ORIENTED_EDGE('',*,*,#35632,.T.);
#49604=ORIENTED_EDGE('',*,*,#35635,.F.);
#49605=ORIENTED_EDGE('',*,*,#35634,.T.);
#49606=ORIENTED_EDGE('',*,*,#35628,.F.);
#49607=ORIENTED_EDGE('',*,*,#35636,.F.);
#49608=ORIENTED_EDGE('',*,*,#35637,.F.);
#49609=ORIENTED_EDGE('',*,*,#35638,.F.);
#49610=ORIENTED_EDGE('',*,*,#35639,.F.);
#49611=ORIENTED_EDGE('',*,*,#35640,.F.);
#49612=ORIENTED_EDGE('',*,*,#35641,.F.);
#49613=ORIENTED_EDGE('',*,*,#35642,.T.);
#49614=ORIENTED_EDGE('',*,*,#35637,.T.);
#49615=ORIENTED_EDGE('',*,*,#35643,.F.);
#49616=ORIENTED_EDGE('',*,*,#35644,.T.);
#49617=ORIENTED_EDGE('',*,*,#35645,.F.);
#49618=ORIENTED_EDGE('',*,*,#35638,.T.);
#49619=ORIENTED_EDGE('',*,*,#35642,.F.);
#49620=ORIENTED_EDGE('',*,*,#35646,.F.);
#49621=ORIENTED_EDGE('',*,*,#35644,.F.);
#49622=ORIENTED_EDGE('',*,*,#35647,.F.);
#49623=ORIENTED_EDGE('',*,*,#35648,.T.);
#49624=ORIENTED_EDGE('',*,*,#35649,.F.);
#49625=ORIENTED_EDGE('',*,*,#35650,.F.);
#49626=ORIENTED_EDGE('',*,*,#35651,.F.);
#49627=ORIENTED_EDGE('',*,*,#35652,.F.);
#49628=ORIENTED_EDGE('',*,*,#35653,.F.);
#49629=ORIENTED_EDGE('',*,*,#35648,.F.);
#49630=ORIENTED_EDGE('',*,*,#35649,.T.);
#49631=ORIENTED_EDGE('',*,*,#35653,.T.);
#49632=ORIENTED_EDGE('',*,*,#35654,.F.);
#49633=ORIENTED_EDGE('',*,*,#35655,.T.);
#49634=ORIENTED_EDGE('',*,*,#35656,.T.);
#49635=ORIENTED_EDGE('',*,*,#35657,.F.);
#49636=ORIENTED_EDGE('',*,*,#35658,.T.);
#49637=ORIENTED_EDGE('',*,*,#35659,.T.);
#49638=ORIENTED_EDGE('',*,*,#35660,.F.);
#49639=ORIENTED_EDGE('',*,*,#35661,.T.);
#49640=ORIENTED_EDGE('',*,*,#35662,.T.);
#49641=ORIENTED_EDGE('',*,*,#35663,.F.);
#49642=ORIENTED_EDGE('',*,*,#35664,.T.);
#49643=ORIENTED_EDGE('',*,*,#35665,.T.);
#49644=ORIENTED_EDGE('',*,*,#35666,.F.);
#49645=ORIENTED_EDGE('',*,*,#35667,.T.);
#49646=ORIENTED_EDGE('',*,*,#35668,.T.);
#49647=ORIENTED_EDGE('',*,*,#35669,.F.);
#49648=ORIENTED_EDGE('',*,*,#35670,.T.);
#49649=ORIENTED_EDGE('',*,*,#35671,.T.);
#49650=ORIENTED_EDGE('',*,*,#35672,.F.);
#49651=ORIENTED_EDGE('',*,*,#35673,.T.);
#49652=ORIENTED_EDGE('',*,*,#35674,.T.);
#49653=ORIENTED_EDGE('',*,*,#35675,.F.);
#49654=ORIENTED_EDGE('',*,*,#35676,.T.);
#49655=ORIENTED_EDGE('',*,*,#35677,.T.);
#49656=ORIENTED_EDGE('',*,*,#35678,.F.);
#49657=ORIENTED_EDGE('',*,*,#35679,.T.);
#49658=ORIENTED_EDGE('',*,*,#35680,.T.);
#49659=ORIENTED_EDGE('',*,*,#35681,.F.);
#49660=ORIENTED_EDGE('',*,*,#35682,.T.);
#49661=ORIENTED_EDGE('',*,*,#35683,.T.);
#49662=ORIENTED_EDGE('',*,*,#35684,.F.);
#49663=ORIENTED_EDGE('',*,*,#35685,.T.);
#49664=ORIENTED_EDGE('',*,*,#35686,.T.);
#49665=ORIENTED_EDGE('',*,*,#35687,.F.);
#49666=ORIENTED_EDGE('',*,*,#35688,.T.);
#49667=ORIENTED_EDGE('',*,*,#35689,.T.);
#49668=ORIENTED_EDGE('',*,*,#35690,.F.);
#49669=ORIENTED_EDGE('',*,*,#35691,.T.);
#49670=ORIENTED_EDGE('',*,*,#35692,.T.);
#49671=ORIENTED_EDGE('',*,*,#35693,.F.);
#49672=ORIENTED_EDGE('',*,*,#35694,.T.);
#49673=ORIENTED_EDGE('',*,*,#35695,.T.);
#49674=ORIENTED_EDGE('',*,*,#35696,.F.);
#49675=ORIENTED_EDGE('',*,*,#35697,.T.);
#49676=ORIENTED_EDGE('',*,*,#35698,.T.);
#49677=ORIENTED_EDGE('',*,*,#35699,.F.);
#49678=ORIENTED_EDGE('',*,*,#35700,.T.);
#49679=ORIENTED_EDGE('',*,*,#35701,.T.);
#49680=ORIENTED_EDGE('',*,*,#35702,.F.);
#49681=ORIENTED_EDGE('',*,*,#35703,.T.);
#49682=ORIENTED_EDGE('',*,*,#35704,.T.);
#49683=ORIENTED_EDGE('',*,*,#35705,.F.);
#49684=ORIENTED_EDGE('',*,*,#35706,.T.);
#49685=ORIENTED_EDGE('',*,*,#35707,.T.);
#49686=ORIENTED_EDGE('',*,*,#35708,.F.);
#49687=ORIENTED_EDGE('',*,*,#35709,.T.);
#49688=ORIENTED_EDGE('',*,*,#35710,.T.);
#49689=ORIENTED_EDGE('',*,*,#35711,.T.);
#49690=ORIENTED_EDGE('',*,*,#35710,.F.);
#49691=ORIENTED_EDGE('',*,*,#35712,.T.);
#49692=ORIENTED_EDGE('',*,*,#35713,.F.);
#49693=ORIENTED_EDGE('',*,*,#35714,.T.);
#49694=ORIENTED_EDGE('',*,*,#35715,.T.);
#49695=ORIENTED_EDGE('',*,*,#35716,.F.);
#49696=ORIENTED_EDGE('',*,*,#35717,.T.);
#49697=ORIENTED_EDGE('',*,*,#35718,.T.);
#49698=ORIENTED_EDGE('',*,*,#35719,.F.);
#49699=ORIENTED_EDGE('',*,*,#35720,.T.);
#49700=ORIENTED_EDGE('',*,*,#35721,.T.);
#49701=ORIENTED_EDGE('',*,*,#35722,.F.);
#49702=ORIENTED_EDGE('',*,*,#35723,.T.);
#49703=ORIENTED_EDGE('',*,*,#35724,.T.);
#49704=ORIENTED_EDGE('',*,*,#35725,.F.);
#49705=ORIENTED_EDGE('',*,*,#35726,.T.);
#49706=ORIENTED_EDGE('',*,*,#35727,.T.);
#49707=ORIENTED_EDGE('',*,*,#35728,.F.);
#49708=ORIENTED_EDGE('',*,*,#35729,.T.);
#49709=ORIENTED_EDGE('',*,*,#35730,.T.);
#49710=ORIENTED_EDGE('',*,*,#35731,.F.);
#49711=ORIENTED_EDGE('',*,*,#35732,.T.);
#49712=ORIENTED_EDGE('',*,*,#35733,.T.);
#49713=ORIENTED_EDGE('',*,*,#35734,.F.);
#49714=ORIENTED_EDGE('',*,*,#35735,.T.);
#49715=ORIENTED_EDGE('',*,*,#35736,.T.);
#49716=ORIENTED_EDGE('',*,*,#35737,.F.);
#49717=ORIENTED_EDGE('',*,*,#35738,.T.);
#49718=ORIENTED_EDGE('',*,*,#35739,.T.);
#49719=ORIENTED_EDGE('',*,*,#35740,.F.);
#49720=ORIENTED_EDGE('',*,*,#35741,.T.);
#49721=ORIENTED_EDGE('',*,*,#35742,.T.);
#49722=ORIENTED_EDGE('',*,*,#35743,.F.);
#49723=ORIENTED_EDGE('',*,*,#35744,.T.);
#49724=ORIENTED_EDGE('',*,*,#35745,.T.);
#49725=ORIENTED_EDGE('',*,*,#35746,.F.);
#49726=ORIENTED_EDGE('',*,*,#35747,.T.);
#49727=ORIENTED_EDGE('',*,*,#35748,.T.);
#49728=ORIENTED_EDGE('',*,*,#35749,.F.);
#49729=ORIENTED_EDGE('',*,*,#35750,.T.);
#49730=ORIENTED_EDGE('',*,*,#35751,.T.);
#49731=ORIENTED_EDGE('',*,*,#35752,.F.);
#49732=ORIENTED_EDGE('',*,*,#35753,.T.);
#49733=ORIENTED_EDGE('',*,*,#35754,.T.);
#49734=ORIENTED_EDGE('',*,*,#35755,.F.);
#49735=ORIENTED_EDGE('',*,*,#35756,.T.);
#49736=ORIENTED_EDGE('',*,*,#35757,.T.);
#49737=ORIENTED_EDGE('',*,*,#35758,.F.);
#49738=ORIENTED_EDGE('',*,*,#35759,.T.);
#49739=ORIENTED_EDGE('',*,*,#35760,.T.);
#49740=ORIENTED_EDGE('',*,*,#35761,.F.);
#49741=ORIENTED_EDGE('',*,*,#35762,.T.);
#49742=ORIENTED_EDGE('',*,*,#35763,.T.);
#49743=ORIENTED_EDGE('',*,*,#35764,.F.);
#49744=ORIENTED_EDGE('',*,*,#35765,.T.);
#49745=ORIENTED_EDGE('',*,*,#35766,.T.);
#49746=ORIENTED_EDGE('',*,*,#35767,.F.);
#49747=ORIENTED_EDGE('',*,*,#35768,.T.);
#49748=ORIENTED_EDGE('',*,*,#35769,.T.);
#49749=ORIENTED_EDGE('',*,*,#35770,.F.);
#49750=ORIENTED_EDGE('',*,*,#35771,.T.);
#49751=ORIENTED_EDGE('',*,*,#35772,.T.);
#49752=ORIENTED_EDGE('',*,*,#35773,.F.);
#49753=ORIENTED_EDGE('',*,*,#35652,.T.);
#49754=ORIENTED_EDGE('',*,*,#35774,.F.);
#49755=ORIENTED_EDGE('',*,*,#35775,.T.);
#49756=ORIENTED_EDGE('',*,*,#35654,.T.);
#49757=ORIENTED_EDGE('',*,*,#35650,.T.);
#49758=ORIENTED_EDGE('',*,*,#35773,.T.);
#49759=ORIENTED_EDGE('',*,*,#35776,.T.);
#49760=ORIENTED_EDGE('',*,*,#35777,.F.);
#49761=ORIENTED_EDGE('',*,*,#35656,.F.);
#49762=ORIENTED_EDGE('',*,*,#35778,.F.);
#49763=ORIENTED_EDGE('',*,*,#35779,.F.);
#49764=ORIENTED_EDGE('',*,*,#35780,.F.);
#49765=ORIENTED_EDGE('',*,*,#35655,.F.);
#49766=ORIENTED_EDGE('',*,*,#35775,.F.);
#49767=ORIENTED_EDGE('',*,*,#35781,.F.);
#49768=ORIENTED_EDGE('',*,*,#35778,.T.);
#49769=ORIENTED_EDGE('',*,*,#35780,.T.);
#49770=ORIENTED_EDGE('',*,*,#35782,.F.);
#49771=ORIENTED_EDGE('',*,*,#35783,.T.);
#49772=ORIENTED_EDGE('',*,*,#35657,.T.);
#49773=ORIENTED_EDGE('',*,*,#35784,.F.);
#49774=ORIENTED_EDGE('',*,*,#35785,.T.);
#49775=ORIENTED_EDGE('',*,*,#35786,.T.);
#49776=ORIENTED_EDGE('',*,*,#35787,.T.);
#49777=ORIENTED_EDGE('',*,*,#35788,.T.);
#49778=ORIENTED_EDGE('',*,*,#35789,.T.);
#49779=ORIENTED_EDGE('',*,*,#35790,.T.);
#49780=ORIENTED_EDGE('',*,*,#35791,.T.);
#49781=ORIENTED_EDGE('',*,*,#35792,.T.);
#49782=ORIENTED_EDGE('',*,*,#35793,.T.);
#49783=ORIENTED_EDGE('',*,*,#35794,.T.);
#49784=ORIENTED_EDGE('',*,*,#35795,.T.);
#49785=ORIENTED_EDGE('',*,*,#35796,.T.);
#49786=ORIENTED_EDGE('',*,*,#35797,.T.);
#49787=ORIENTED_EDGE('',*,*,#35798,.T.);
#49788=ORIENTED_EDGE('',*,*,#35799,.T.);
#49789=ORIENTED_EDGE('',*,*,#35800,.T.);
#49790=ORIENTED_EDGE('',*,*,#35801,.T.);
#49791=ORIENTED_EDGE('',*,*,#35802,.T.);
#49792=ORIENTED_EDGE('',*,*,#35803,.T.);
#49793=ORIENTED_EDGE('',*,*,#35804,.T.);
#49794=ORIENTED_EDGE('',*,*,#35805,.T.);
#49795=ORIENTED_EDGE('',*,*,#35806,.T.);
#49796=ORIENTED_EDGE('',*,*,#35807,.T.);
#49797=ORIENTED_EDGE('',*,*,#35808,.T.);
#49798=ORIENTED_EDGE('',*,*,#35809,.T.);
#49799=ORIENTED_EDGE('',*,*,#35810,.T.);
#49800=ORIENTED_EDGE('',*,*,#35811,.T.);
#49801=ORIENTED_EDGE('',*,*,#35812,.T.);
#49802=ORIENTED_EDGE('',*,*,#35813,.T.);
#49803=ORIENTED_EDGE('',*,*,#35814,.T.);
#49804=ORIENTED_EDGE('',*,*,#35815,.T.);
#49805=ORIENTED_EDGE('',*,*,#35816,.T.);
#49806=ORIENTED_EDGE('',*,*,#35817,.T.);
#49807=ORIENTED_EDGE('',*,*,#35818,.T.);
#49808=ORIENTED_EDGE('',*,*,#35819,.T.);
#49809=ORIENTED_EDGE('',*,*,#35820,.T.);
#49810=ORIENTED_EDGE('',*,*,#35821,.T.);
#49811=ORIENTED_EDGE('',*,*,#35822,.T.);
#49812=ORIENTED_EDGE('',*,*,#35823,.T.);
#49813=ORIENTED_EDGE('',*,*,#35824,.T.);
#49814=ORIENTED_EDGE('',*,*,#35825,.T.);
#49815=ORIENTED_EDGE('',*,*,#35826,.T.);
#49816=ORIENTED_EDGE('',*,*,#35827,.T.);
#49817=ORIENTED_EDGE('',*,*,#35828,.T.);
#49818=ORIENTED_EDGE('',*,*,#35829,.T.);
#49819=ORIENTED_EDGE('',*,*,#35830,.T.);
#49820=ORIENTED_EDGE('',*,*,#35831,.T.);
#49821=ORIENTED_EDGE('',*,*,#35832,.T.);
#49822=ORIENTED_EDGE('',*,*,#35833,.T.);
#49823=ORIENTED_EDGE('',*,*,#35834,.T.);
#49824=ORIENTED_EDGE('',*,*,#35835,.T.);
#49825=ORIENTED_EDGE('',*,*,#35836,.T.);
#49826=ORIENTED_EDGE('',*,*,#35837,.T.);
#49827=ORIENTED_EDGE('',*,*,#35782,.T.);
#49828=ORIENTED_EDGE('',*,*,#35779,.T.);
#49829=ORIENTED_EDGE('',*,*,#35781,.T.);
#49830=ORIENTED_EDGE('',*,*,#35774,.T.);
#49831=ORIENTED_EDGE('',*,*,#35651,.T.);
#49832=ORIENTED_EDGE('',*,*,#35647,.T.);
#49833=ORIENTED_EDGE('',*,*,#35777,.T.);
#49834=ORIENTED_EDGE('',*,*,#35838,.T.);
#49835=ORIENTED_EDGE('',*,*,#35839,.T.);
#49836=ORIENTED_EDGE('',*,*,#35840,.T.);
#49837=ORIENTED_EDGE('',*,*,#35841,.T.);
#49838=ORIENTED_EDGE('',*,*,#35842,.T.);
#49839=ORIENTED_EDGE('',*,*,#35843,.T.);
#49840=ORIENTED_EDGE('',*,*,#35844,.T.);
#49841=ORIENTED_EDGE('',*,*,#35845,.T.);
#49842=ORIENTED_EDGE('',*,*,#35846,.T.);
#49843=ORIENTED_EDGE('',*,*,#35847,.T.);
#49844=ORIENTED_EDGE('',*,*,#35848,.T.);
#49845=ORIENTED_EDGE('',*,*,#35849,.T.);
#49846=ORIENTED_EDGE('',*,*,#35850,.T.);
#49847=ORIENTED_EDGE('',*,*,#35851,.T.);
#49848=ORIENTED_EDGE('',*,*,#35852,.T.);
#49849=ORIENTED_EDGE('',*,*,#35853,.T.);
#49850=ORIENTED_EDGE('',*,*,#35854,.T.);
#49851=ORIENTED_EDGE('',*,*,#35855,.T.);
#49852=ORIENTED_EDGE('',*,*,#35856,.T.);
#49853=ORIENTED_EDGE('',*,*,#35857,.T.);
#49854=ORIENTED_EDGE('',*,*,#35858,.T.);
#49855=ORIENTED_EDGE('',*,*,#35859,.T.);
#49856=ORIENTED_EDGE('',*,*,#35860,.T.);
#49857=ORIENTED_EDGE('',*,*,#35861,.T.);
#49858=ORIENTED_EDGE('',*,*,#35862,.T.);
#49859=ORIENTED_EDGE('',*,*,#35863,.T.);
#49860=ORIENTED_EDGE('',*,*,#35864,.T.);
#49861=ORIENTED_EDGE('',*,*,#35865,.T.);
#49862=ORIENTED_EDGE('',*,*,#35866,.T.);
#49863=ORIENTED_EDGE('',*,*,#35867,.T.);
#49864=ORIENTED_EDGE('',*,*,#35868,.T.);
#49865=ORIENTED_EDGE('',*,*,#35869,.T.);
#49866=ORIENTED_EDGE('',*,*,#35870,.T.);
#49867=ORIENTED_EDGE('',*,*,#35871,.T.);
#49868=ORIENTED_EDGE('',*,*,#35872,.T.);
#49869=ORIENTED_EDGE('',*,*,#35873,.T.);
#49870=ORIENTED_EDGE('',*,*,#35874,.T.);
#49871=ORIENTED_EDGE('',*,*,#35875,.T.);
#49872=ORIENTED_EDGE('',*,*,#35876,.T.);
#49873=ORIENTED_EDGE('',*,*,#35877,.T.);
#49874=ORIENTED_EDGE('',*,*,#35878,.T.);
#49875=ORIENTED_EDGE('',*,*,#35879,.T.);
#49876=ORIENTED_EDGE('',*,*,#35880,.T.);
#49877=ORIENTED_EDGE('',*,*,#35881,.T.);
#49878=ORIENTED_EDGE('',*,*,#35882,.T.);
#49879=ORIENTED_EDGE('',*,*,#35883,.T.);
#49880=ORIENTED_EDGE('',*,*,#35884,.T.);
#49881=ORIENTED_EDGE('',*,*,#35885,.T.);
#49882=ORIENTED_EDGE('',*,*,#35886,.T.);
#49883=ORIENTED_EDGE('',*,*,#35887,.T.);
#49884=ORIENTED_EDGE('',*,*,#35888,.T.);
#49885=ORIENTED_EDGE('',*,*,#35889,.T.);
#49886=ORIENTED_EDGE('',*,*,#35890,.T.);
#49887=ORIENTED_EDGE('',*,*,#35891,.T.);
#49888=ORIENTED_EDGE('',*,*,#35892,.T.);
#49889=ORIENTED_EDGE('',*,*,#35893,.T.);
#49890=ORIENTED_EDGE('',*,*,#35894,.T.);
#49891=ORIENTED_EDGE('',*,*,#35895,.T.);
#49892=ORIENTED_EDGE('',*,*,#35896,.T.);
#49893=ORIENTED_EDGE('',*,*,#35897,.T.);
#49894=ORIENTED_EDGE('',*,*,#35898,.T.);
#49895=ORIENTED_EDGE('',*,*,#35785,.F.);
#49896=ORIENTED_EDGE('',*,*,#35837,.F.);
#49897=ORIENTED_EDGE('',*,*,#35899,.T.);
#49898=ORIENTED_EDGE('',*,*,#35658,.F.);
#49899=ORIENTED_EDGE('',*,*,#35783,.F.);
#49900=ORIENTED_EDGE('',*,*,#35836,.F.);
#49901=ORIENTED_EDGE('',*,*,#35900,.F.);
#49902=ORIENTED_EDGE('',*,*,#35659,.F.);
#49903=ORIENTED_EDGE('',*,*,#35899,.F.);
#49904=ORIENTED_EDGE('',*,*,#35834,.F.);
#49905=ORIENTED_EDGE('',*,*,#35901,.T.);
#49906=ORIENTED_EDGE('',*,*,#35661,.F.);
#49907=ORIENTED_EDGE('',*,*,#35902,.F.);
#49908=ORIENTED_EDGE('',*,*,#35833,.F.);
#49909=ORIENTED_EDGE('',*,*,#35903,.F.);
#49910=ORIENTED_EDGE('',*,*,#35662,.F.);
#49911=ORIENTED_EDGE('',*,*,#35901,.F.);
#49912=ORIENTED_EDGE('',*,*,#35903,.T.);
#49913=ORIENTED_EDGE('',*,*,#35832,.F.);
#49914=ORIENTED_EDGE('',*,*,#35904,.T.);
#49915=ORIENTED_EDGE('',*,*,#35663,.T.);
#49916=ORIENTED_EDGE('',*,*,#35900,.T.);
#49917=ORIENTED_EDGE('',*,*,#35835,.F.);
#49918=ORIENTED_EDGE('',*,*,#35902,.T.);
#49919=ORIENTED_EDGE('',*,*,#35660,.T.);
#49920=ORIENTED_EDGE('',*,*,#35665,.F.);
#49921=ORIENTED_EDGE('',*,*,#35905,.F.);
#49922=ORIENTED_EDGE('',*,*,#35830,.F.);
#49923=ORIENTED_EDGE('',*,*,#35906,.F.);
#49924=ORIENTED_EDGE('',*,*,#35664,.F.);
#49925=ORIENTED_EDGE('',*,*,#35904,.F.);
#49926=ORIENTED_EDGE('',*,*,#35831,.F.);
#49927=ORIENTED_EDGE('',*,*,#35905,.T.);
#49928=ORIENTED_EDGE('',*,*,#35906,.T.);
#49929=ORIENTED_EDGE('',*,*,#35829,.F.);
#49930=ORIENTED_EDGE('',*,*,#35907,.T.);
#49931=ORIENTED_EDGE('',*,*,#35666,.T.);
#49932=ORIENTED_EDGE('',*,*,#35828,.F.);
#49933=ORIENTED_EDGE('',*,*,#35908,.T.);
#49934=ORIENTED_EDGE('',*,*,#35667,.F.);
#49935=ORIENTED_EDGE('',*,*,#35907,.F.);
#49936=ORIENTED_EDGE('',*,*,#35827,.F.);
#49937=ORIENTED_EDGE('',*,*,#35909,.F.);
#49938=ORIENTED_EDGE('',*,*,#35668,.F.);
#49939=ORIENTED_EDGE('',*,*,#35908,.F.);
#49940=ORIENTED_EDGE('',*,*,#35825,.F.);
#49941=ORIENTED_EDGE('',*,*,#35910,.T.);
#49942=ORIENTED_EDGE('',*,*,#35670,.F.);
#49943=ORIENTED_EDGE('',*,*,#35911,.F.);
#49944=ORIENTED_EDGE('',*,*,#35824,.F.);
#49945=ORIENTED_EDGE('',*,*,#35912,.F.);
#49946=ORIENTED_EDGE('',*,*,#35671,.F.);
#49947=ORIENTED_EDGE('',*,*,#35910,.F.);
#49948=ORIENTED_EDGE('',*,*,#35912,.T.);
#49949=ORIENTED_EDGE('',*,*,#35823,.F.);
#49950=ORIENTED_EDGE('',*,*,#35913,.T.);
#49951=ORIENTED_EDGE('',*,*,#35672,.T.);
#49952=ORIENTED_EDGE('',*,*,#35909,.T.);
#49953=ORIENTED_EDGE('',*,*,#35826,.F.);
#49954=ORIENTED_EDGE('',*,*,#35911,.T.);
#49955=ORIENTED_EDGE('',*,*,#35669,.T.);
#49956=ORIENTED_EDGE('',*,*,#35674,.F.);
#49957=ORIENTED_EDGE('',*,*,#35914,.F.);
#49958=ORIENTED_EDGE('',*,*,#35821,.F.);
#49959=ORIENTED_EDGE('',*,*,#35915,.F.);
#49960=ORIENTED_EDGE('',*,*,#35673,.F.);
#49961=ORIENTED_EDGE('',*,*,#35913,.F.);
#49962=ORIENTED_EDGE('',*,*,#35822,.F.);
#49963=ORIENTED_EDGE('',*,*,#35914,.T.);
#49964=ORIENTED_EDGE('',*,*,#35915,.T.);
#49965=ORIENTED_EDGE('',*,*,#35820,.F.);
#49966=ORIENTED_EDGE('',*,*,#35916,.T.);
#49967=ORIENTED_EDGE('',*,*,#35675,.T.);
#49968=ORIENTED_EDGE('',*,*,#35819,.F.);
#49969=ORIENTED_EDGE('',*,*,#35917,.T.);
#49970=ORIENTED_EDGE('',*,*,#35676,.F.);
#49971=ORIENTED_EDGE('',*,*,#35916,.F.);
#49972=ORIENTED_EDGE('',*,*,#35818,.F.);
#49973=ORIENTED_EDGE('',*,*,#35918,.F.);
#49974=ORIENTED_EDGE('',*,*,#35677,.F.);
#49975=ORIENTED_EDGE('',*,*,#35917,.F.);
#49976=ORIENTED_EDGE('',*,*,#35816,.F.);
#49977=ORIENTED_EDGE('',*,*,#35919,.T.);
#49978=ORIENTED_EDGE('',*,*,#35679,.F.);
#49979=ORIENTED_EDGE('',*,*,#35920,.F.);
#49980=ORIENTED_EDGE('',*,*,#35815,.F.);
#49981=ORIENTED_EDGE('',*,*,#35921,.F.);
#49982=ORIENTED_EDGE('',*,*,#35680,.F.);
#49983=ORIENTED_EDGE('',*,*,#35919,.F.);
#49984=ORIENTED_EDGE('',*,*,#35921,.T.);
#49985=ORIENTED_EDGE('',*,*,#35814,.F.);
#49986=ORIENTED_EDGE('',*,*,#35922,.T.);
#49987=ORIENTED_EDGE('',*,*,#35681,.T.);
#49988=ORIENTED_EDGE('',*,*,#35918,.T.);
#49989=ORIENTED_EDGE('',*,*,#35817,.F.);
#49990=ORIENTED_EDGE('',*,*,#35920,.T.);
#49991=ORIENTED_EDGE('',*,*,#35678,.T.);
#49992=ORIENTED_EDGE('',*,*,#35683,.F.);
#49993=ORIENTED_EDGE('',*,*,#35923,.F.);
#49994=ORIENTED_EDGE('',*,*,#35812,.F.);
#49995=ORIENTED_EDGE('',*,*,#35924,.F.);
#49996=ORIENTED_EDGE('',*,*,#35682,.F.);
#49997=ORIENTED_EDGE('',*,*,#35922,.F.);
#49998=ORIENTED_EDGE('',*,*,#35813,.F.);
#49999=ORIENTED_EDGE('',*,*,#35923,.T.);
#50000=ORIENTED_EDGE('',*,*,#35924,.T.);
#50001=ORIENTED_EDGE('',*,*,#35811,.F.);
#50002=ORIENTED_EDGE('',*,*,#35925,.T.);
#50003=ORIENTED_EDGE('',*,*,#35684,.T.);
#50004=ORIENTED_EDGE('',*,*,#35810,.F.);
#50005=ORIENTED_EDGE('',*,*,#35926,.T.);
#50006=ORIENTED_EDGE('',*,*,#35685,.F.);
#50007=ORIENTED_EDGE('',*,*,#35925,.F.);
#50008=ORIENTED_EDGE('',*,*,#35809,.F.);
#50009=ORIENTED_EDGE('',*,*,#35927,.F.);
#50010=ORIENTED_EDGE('',*,*,#35686,.F.);
#50011=ORIENTED_EDGE('',*,*,#35926,.F.);
#50012=ORIENTED_EDGE('',*,*,#35807,.F.);
#50013=ORIENTED_EDGE('',*,*,#35928,.T.);
#50014=ORIENTED_EDGE('',*,*,#35688,.F.);
#50015=ORIENTED_EDGE('',*,*,#35929,.F.);
#50016=ORIENTED_EDGE('',*,*,#35806,.F.);
#50017=ORIENTED_EDGE('',*,*,#35930,.F.);
#50018=ORIENTED_EDGE('',*,*,#35689,.F.);
#50019=ORIENTED_EDGE('',*,*,#35928,.F.);
#50020=ORIENTED_EDGE('',*,*,#35930,.T.);
#50021=ORIENTED_EDGE('',*,*,#35805,.F.);
#50022=ORIENTED_EDGE('',*,*,#35931,.T.);
#50023=ORIENTED_EDGE('',*,*,#35690,.T.);
#50024=ORIENTED_EDGE('',*,*,#35927,.T.);
#50025=ORIENTED_EDGE('',*,*,#35808,.F.);
#50026=ORIENTED_EDGE('',*,*,#35929,.T.);
#50027=ORIENTED_EDGE('',*,*,#35687,.T.);
#50028=ORIENTED_EDGE('',*,*,#35692,.F.);
#50029=ORIENTED_EDGE('',*,*,#35932,.F.);
#50030=ORIENTED_EDGE('',*,*,#35803,.F.);
#50031=ORIENTED_EDGE('',*,*,#35933,.F.);
#50032=ORIENTED_EDGE('',*,*,#35691,.F.);
#50033=ORIENTED_EDGE('',*,*,#35931,.F.);
#50034=ORIENTED_EDGE('',*,*,#35804,.F.);
#50035=ORIENTED_EDGE('',*,*,#35932,.T.);
#50036=ORIENTED_EDGE('',*,*,#35933,.T.);
#50037=ORIENTED_EDGE('',*,*,#35802,.F.);
#50038=ORIENTED_EDGE('',*,*,#35934,.T.);
#50039=ORIENTED_EDGE('',*,*,#35693,.T.);
#50040=ORIENTED_EDGE('',*,*,#35801,.F.);
#50041=ORIENTED_EDGE('',*,*,#35935,.T.);
#50042=ORIENTED_EDGE('',*,*,#35694,.F.);
#50043=ORIENTED_EDGE('',*,*,#35934,.F.);
#50044=ORIENTED_EDGE('',*,*,#35800,.F.);
#50045=ORIENTED_EDGE('',*,*,#35936,.F.);
#50046=ORIENTED_EDGE('',*,*,#35695,.F.);
#50047=ORIENTED_EDGE('',*,*,#35935,.F.);
#50048=ORIENTED_EDGE('',*,*,#35798,.F.);
#50049=ORIENTED_EDGE('',*,*,#35937,.T.);
#50050=ORIENTED_EDGE('',*,*,#35697,.F.);
#50051=ORIENTED_EDGE('',*,*,#35938,.F.);
#50052=ORIENTED_EDGE('',*,*,#35797,.F.);
#50053=ORIENTED_EDGE('',*,*,#35939,.F.);
#50054=ORIENTED_EDGE('',*,*,#35698,.F.);
#50055=ORIENTED_EDGE('',*,*,#35937,.F.);
#50056=ORIENTED_EDGE('',*,*,#35939,.T.);
#50057=ORIENTED_EDGE('',*,*,#35796,.F.);
#50058=ORIENTED_EDGE('',*,*,#35940,.T.);
#50059=ORIENTED_EDGE('',*,*,#35699,.T.);
#50060=ORIENTED_EDGE('',*,*,#35936,.T.);
#50061=ORIENTED_EDGE('',*,*,#35799,.F.);
#50062=ORIENTED_EDGE('',*,*,#35938,.T.);
#50063=ORIENTED_EDGE('',*,*,#35696,.T.);
#50064=ORIENTED_EDGE('',*,*,#35701,.F.);
#50065=ORIENTED_EDGE('',*,*,#35941,.F.);
#50066=ORIENTED_EDGE('',*,*,#35794,.F.);
#50067=ORIENTED_EDGE('',*,*,#35942,.F.);
#50068=ORIENTED_EDGE('',*,*,#35700,.F.);
#50069=ORIENTED_EDGE('',*,*,#35940,.F.);
#50070=ORIENTED_EDGE('',*,*,#35795,.F.);
#50071=ORIENTED_EDGE('',*,*,#35941,.T.);
#50072=ORIENTED_EDGE('',*,*,#35942,.T.);
#50073=ORIENTED_EDGE('',*,*,#35793,.F.);
#50074=ORIENTED_EDGE('',*,*,#35943,.T.);
#50075=ORIENTED_EDGE('',*,*,#35702,.T.);
#50076=ORIENTED_EDGE('',*,*,#35792,.F.);
#50077=ORIENTED_EDGE('',*,*,#35944,.T.);
#50078=ORIENTED_EDGE('',*,*,#35703,.F.);
#50079=ORIENTED_EDGE('',*,*,#35943,.F.);
#50080=ORIENTED_EDGE('',*,*,#35791,.F.);
#50081=ORIENTED_EDGE('',*,*,#35945,.F.);
#50082=ORIENTED_EDGE('',*,*,#35704,.F.);
#50083=ORIENTED_EDGE('',*,*,#35944,.F.);
#50084=ORIENTED_EDGE('',*,*,#35789,.F.);
#50085=ORIENTED_EDGE('',*,*,#35946,.T.);
#50086=ORIENTED_EDGE('',*,*,#35706,.F.);
#50087=ORIENTED_EDGE('',*,*,#35947,.F.);
#50088=ORIENTED_EDGE('',*,*,#35788,.F.);
#50089=ORIENTED_EDGE('',*,*,#35948,.F.);
#50090=ORIENTED_EDGE('',*,*,#35707,.F.);
#50091=ORIENTED_EDGE('',*,*,#35946,.F.);
#50092=ORIENTED_EDGE('',*,*,#35948,.T.);
#50093=ORIENTED_EDGE('',*,*,#35787,.F.);
#50094=ORIENTED_EDGE('',*,*,#35949,.T.);
#50095=ORIENTED_EDGE('',*,*,#35708,.T.);
#50096=ORIENTED_EDGE('',*,*,#35945,.T.);
#50097=ORIENTED_EDGE('',*,*,#35790,.F.);
#50098=ORIENTED_EDGE('',*,*,#35947,.T.);
#50099=ORIENTED_EDGE('',*,*,#35705,.T.);
#50100=ORIENTED_EDGE('',*,*,#35712,.F.);
#50101=ORIENTED_EDGE('',*,*,#35950,.F.);
#50102=ORIENTED_EDGE('',*,*,#35898,.F.);
#50103=ORIENTED_EDGE('',*,*,#35951,.F.);
#50104=ORIENTED_EDGE('',*,*,#35709,.F.);
#50105=ORIENTED_EDGE('',*,*,#35949,.F.);
#50106=ORIENTED_EDGE('',*,*,#35786,.F.);
#50107=ORIENTED_EDGE('',*,*,#35950,.T.);
#50108=ORIENTED_EDGE('',*,*,#35951,.T.);
#50109=ORIENTED_EDGE('',*,*,#35897,.F.);
#50110=ORIENTED_EDGE('',*,*,#35952,.T.);
#50111=ORIENTED_EDGE('',*,*,#35713,.T.);
#50112=ORIENTED_EDGE('',*,*,#35896,.F.);
#50113=ORIENTED_EDGE('',*,*,#35953,.T.);
#50114=ORIENTED_EDGE('',*,*,#35714,.F.);
#50115=ORIENTED_EDGE('',*,*,#35952,.F.);
#50116=ORIENTED_EDGE('',*,*,#35895,.F.);
#50117=ORIENTED_EDGE('',*,*,#35954,.F.);
#50118=ORIENTED_EDGE('',*,*,#35715,.F.);
#50119=ORIENTED_EDGE('',*,*,#35953,.F.);
#50120=ORIENTED_EDGE('',*,*,#35893,.F.);
#50121=ORIENTED_EDGE('',*,*,#35955,.T.);
#50122=ORIENTED_EDGE('',*,*,#35717,.F.);
#50123=ORIENTED_EDGE('',*,*,#35956,.F.);
#50124=ORIENTED_EDGE('',*,*,#35892,.F.);
#50125=ORIENTED_EDGE('',*,*,#35957,.F.);
#50126=ORIENTED_EDGE('',*,*,#35718,.F.);
#50127=ORIENTED_EDGE('',*,*,#35955,.F.);
#50128=ORIENTED_EDGE('',*,*,#35957,.T.);
#50129=ORIENTED_EDGE('',*,*,#35891,.F.);
#50130=ORIENTED_EDGE('',*,*,#35958,.T.);
#50131=ORIENTED_EDGE('',*,*,#35719,.T.);
#50132=ORIENTED_EDGE('',*,*,#35954,.T.);
#50133=ORIENTED_EDGE('',*,*,#35894,.F.);
#50134=ORIENTED_EDGE('',*,*,#35956,.T.);
#50135=ORIENTED_EDGE('',*,*,#35716,.T.);
#50136=ORIENTED_EDGE('',*,*,#35721,.F.);
#50137=ORIENTED_EDGE('',*,*,#35959,.F.);
#50138=ORIENTED_EDGE('',*,*,#35889,.F.);
#50139=ORIENTED_EDGE('',*,*,#35960,.F.);
#50140=ORIENTED_EDGE('',*,*,#35720,.F.);
#50141=ORIENTED_EDGE('',*,*,#35958,.F.);
#50142=ORIENTED_EDGE('',*,*,#35890,.F.);
#50143=ORIENTED_EDGE('',*,*,#35959,.T.);
#50144=ORIENTED_EDGE('',*,*,#35960,.T.);
#50145=ORIENTED_EDGE('',*,*,#35888,.F.);
#50146=ORIENTED_EDGE('',*,*,#35961,.T.);
#50147=ORIENTED_EDGE('',*,*,#35722,.T.);
#50148=ORIENTED_EDGE('',*,*,#35887,.F.);
#50149=ORIENTED_EDGE('',*,*,#35962,.T.);
#50150=ORIENTED_EDGE('',*,*,#35723,.F.);
#50151=ORIENTED_EDGE('',*,*,#35961,.F.);
#50152=ORIENTED_EDGE('',*,*,#35886,.F.);
#50153=ORIENTED_EDGE('',*,*,#35963,.F.);
#50154=ORIENTED_EDGE('',*,*,#35724,.F.);
#50155=ORIENTED_EDGE('',*,*,#35962,.F.);
#50156=ORIENTED_EDGE('',*,*,#35884,.F.);
#50157=ORIENTED_EDGE('',*,*,#35964,.T.);
#50158=ORIENTED_EDGE('',*,*,#35726,.F.);
#50159=ORIENTED_EDGE('',*,*,#35965,.F.);
#50160=ORIENTED_EDGE('',*,*,#35883,.F.);
#50161=ORIENTED_EDGE('',*,*,#35966,.F.);
#50162=ORIENTED_EDGE('',*,*,#35727,.F.);
#50163=ORIENTED_EDGE('',*,*,#35964,.F.);
#50164=ORIENTED_EDGE('',*,*,#35966,.T.);
#50165=ORIENTED_EDGE('',*,*,#35882,.F.);
#50166=ORIENTED_EDGE('',*,*,#35967,.T.);
#50167=ORIENTED_EDGE('',*,*,#35728,.T.);
#50168=ORIENTED_EDGE('',*,*,#35963,.T.);
#50169=ORIENTED_EDGE('',*,*,#35885,.F.);
#50170=ORIENTED_EDGE('',*,*,#35965,.T.);
#50171=ORIENTED_EDGE('',*,*,#35725,.T.);
#50172=ORIENTED_EDGE('',*,*,#35730,.F.);
#50173=ORIENTED_EDGE('',*,*,#35968,.F.);
#50174=ORIENTED_EDGE('',*,*,#35880,.F.);
#50175=ORIENTED_EDGE('',*,*,#35969,.F.);
#50176=ORIENTED_EDGE('',*,*,#35729,.F.);
#50177=ORIENTED_EDGE('',*,*,#35967,.F.);
#50178=ORIENTED_EDGE('',*,*,#35881,.F.);
#50179=ORIENTED_EDGE('',*,*,#35968,.T.);
#50180=ORIENTED_EDGE('',*,*,#35969,.T.);
#50181=ORIENTED_EDGE('',*,*,#35879,.F.);
#50182=ORIENTED_EDGE('',*,*,#35970,.T.);
#50183=ORIENTED_EDGE('',*,*,#35731,.T.);
#50184=ORIENTED_EDGE('',*,*,#35878,.F.);
#50185=ORIENTED_EDGE('',*,*,#35971,.T.);
#50186=ORIENTED_EDGE('',*,*,#35732,.F.);
#50187=ORIENTED_EDGE('',*,*,#35970,.F.);
#50188=ORIENTED_EDGE('',*,*,#35877,.F.);
#50189=ORIENTED_EDGE('',*,*,#35972,.F.);
#50190=ORIENTED_EDGE('',*,*,#35733,.F.);
#50191=ORIENTED_EDGE('',*,*,#35971,.F.);
#50192=ORIENTED_EDGE('',*,*,#35875,.F.);
#50193=ORIENTED_EDGE('',*,*,#35973,.T.);
#50194=ORIENTED_EDGE('',*,*,#35735,.F.);
#50195=ORIENTED_EDGE('',*,*,#35974,.F.);
#50196=ORIENTED_EDGE('',*,*,#35874,.F.);
#50197=ORIENTED_EDGE('',*,*,#35975,.F.);
#50198=ORIENTED_EDGE('',*,*,#35736,.F.);
#50199=ORIENTED_EDGE('',*,*,#35973,.F.);
#50200=ORIENTED_EDGE('',*,*,#35975,.T.);
#50201=ORIENTED_EDGE('',*,*,#35873,.F.);
#50202=ORIENTED_EDGE('',*,*,#35976,.T.);
#50203=ORIENTED_EDGE('',*,*,#35737,.T.);
#50204=ORIENTED_EDGE('',*,*,#35972,.T.);
#50205=ORIENTED_EDGE('',*,*,#35876,.F.);
#50206=ORIENTED_EDGE('',*,*,#35974,.T.);
#50207=ORIENTED_EDGE('',*,*,#35734,.T.);
#50208=ORIENTED_EDGE('',*,*,#35739,.F.);
#50209=ORIENTED_EDGE('',*,*,#35977,.F.);
#50210=ORIENTED_EDGE('',*,*,#35871,.F.);
#50211=ORIENTED_EDGE('',*,*,#35978,.F.);
#50212=ORIENTED_EDGE('',*,*,#35738,.F.);
#50213=ORIENTED_EDGE('',*,*,#35976,.F.);
#50214=ORIENTED_EDGE('',*,*,#35872,.F.);
#50215=ORIENTED_EDGE('',*,*,#35977,.T.);
#50216=ORIENTED_EDGE('',*,*,#35978,.T.);
#50217=ORIENTED_EDGE('',*,*,#35870,.F.);
#50218=ORIENTED_EDGE('',*,*,#35979,.T.);
#50219=ORIENTED_EDGE('',*,*,#35740,.T.);
#50220=ORIENTED_EDGE('',*,*,#35869,.F.);
#50221=ORIENTED_EDGE('',*,*,#35980,.T.);
#50222=ORIENTED_EDGE('',*,*,#35741,.F.);
#50223=ORIENTED_EDGE('',*,*,#35979,.F.);
#50224=ORIENTED_EDGE('',*,*,#35868,.F.);
#50225=ORIENTED_EDGE('',*,*,#35981,.F.);
#50226=ORIENTED_EDGE('',*,*,#35742,.F.);
#50227=ORIENTED_EDGE('',*,*,#35980,.F.);
#50228=ORIENTED_EDGE('',*,*,#35866,.F.);
#50229=ORIENTED_EDGE('',*,*,#35982,.T.);
#50230=ORIENTED_EDGE('',*,*,#35744,.F.);
#50231=ORIENTED_EDGE('',*,*,#35983,.F.);
#50232=ORIENTED_EDGE('',*,*,#35865,.F.);
#50233=ORIENTED_EDGE('',*,*,#35984,.F.);
#50234=ORIENTED_EDGE('',*,*,#35745,.F.);
#50235=ORIENTED_EDGE('',*,*,#35982,.F.);
#50236=ORIENTED_EDGE('',*,*,#35984,.T.);
#50237=ORIENTED_EDGE('',*,*,#35864,.F.);
#50238=ORIENTED_EDGE('',*,*,#35985,.T.);
#50239=ORIENTED_EDGE('',*,*,#35746,.T.);
#50240=ORIENTED_EDGE('',*,*,#35981,.T.);
#50241=ORIENTED_EDGE('',*,*,#35867,.F.);
#50242=ORIENTED_EDGE('',*,*,#35983,.T.);
#50243=ORIENTED_EDGE('',*,*,#35743,.T.);
#50244=ORIENTED_EDGE('',*,*,#35748,.F.);
#50245=ORIENTED_EDGE('',*,*,#35986,.F.);
#50246=ORIENTED_EDGE('',*,*,#35862,.F.);
#50247=ORIENTED_EDGE('',*,*,#35987,.F.);
#50248=ORIENTED_EDGE('',*,*,#35747,.F.);
#50249=ORIENTED_EDGE('',*,*,#35985,.F.);
#50250=ORIENTED_EDGE('',*,*,#35863,.F.);
#50251=ORIENTED_EDGE('',*,*,#35986,.T.);
#50252=ORIENTED_EDGE('',*,*,#35987,.T.);
#50253=ORIENTED_EDGE('',*,*,#35861,.F.);
#50254=ORIENTED_EDGE('',*,*,#35988,.T.);
#50255=ORIENTED_EDGE('',*,*,#35749,.T.);
#50256=ORIENTED_EDGE('',*,*,#35860,.F.);
#50257=ORIENTED_EDGE('',*,*,#35989,.T.);
#50258=ORIENTED_EDGE('',*,*,#35750,.F.);
#50259=ORIENTED_EDGE('',*,*,#35988,.F.);
#50260=ORIENTED_EDGE('',*,*,#35859,.F.);
#50261=ORIENTED_EDGE('',*,*,#35990,.F.);
#50262=ORIENTED_EDGE('',*,*,#35751,.F.);
#50263=ORIENTED_EDGE('',*,*,#35989,.F.);
#50264=ORIENTED_EDGE('',*,*,#35857,.F.);
#50265=ORIENTED_EDGE('',*,*,#35991,.T.);
#50266=ORIENTED_EDGE('',*,*,#35753,.F.);
#50267=ORIENTED_EDGE('',*,*,#35992,.F.);
#50268=ORIENTED_EDGE('',*,*,#35856,.F.);
#50269=ORIENTED_EDGE('',*,*,#35993,.F.);
#50270=ORIENTED_EDGE('',*,*,#35754,.F.);
#50271=ORIENTED_EDGE('',*,*,#35991,.F.);
#50272=ORIENTED_EDGE('',*,*,#35993,.T.);
#50273=ORIENTED_EDGE('',*,*,#35855,.F.);
#50274=ORIENTED_EDGE('',*,*,#35994,.T.);
#50275=ORIENTED_EDGE('',*,*,#35755,.T.);
#50276=ORIENTED_EDGE('',*,*,#35990,.T.);
#50277=ORIENTED_EDGE('',*,*,#35858,.F.);
#50278=ORIENTED_EDGE('',*,*,#35992,.T.);
#50279=ORIENTED_EDGE('',*,*,#35752,.T.);
#50280=ORIENTED_EDGE('',*,*,#35757,.F.);
#50281=ORIENTED_EDGE('',*,*,#35995,.F.);
#50282=ORIENTED_EDGE('',*,*,#35853,.F.);
#50283=ORIENTED_EDGE('',*,*,#35996,.F.);
#50284=ORIENTED_EDGE('',*,*,#35756,.F.);
#50285=ORIENTED_EDGE('',*,*,#35994,.F.);
#50286=ORIENTED_EDGE('',*,*,#35854,.F.);
#50287=ORIENTED_EDGE('',*,*,#35995,.T.);
#50288=ORIENTED_EDGE('',*,*,#35996,.T.);
#50289=ORIENTED_EDGE('',*,*,#35852,.F.);
#50290=ORIENTED_EDGE('',*,*,#35997,.T.);
#50291=ORIENTED_EDGE('',*,*,#35758,.T.);
#50292=ORIENTED_EDGE('',*,*,#35851,.F.);
#50293=ORIENTED_EDGE('',*,*,#35998,.T.);
#50294=ORIENTED_EDGE('',*,*,#35759,.F.);
#50295=ORIENTED_EDGE('',*,*,#35997,.F.);
#50296=ORIENTED_EDGE('',*,*,#35850,.F.);
#50297=ORIENTED_EDGE('',*,*,#35999,.F.);
#50298=ORIENTED_EDGE('',*,*,#35760,.F.);
#50299=ORIENTED_EDGE('',*,*,#35998,.F.);
#50300=ORIENTED_EDGE('',*,*,#35848,.F.);
#50301=ORIENTED_EDGE('',*,*,#36000,.T.);
#50302=ORIENTED_EDGE('',*,*,#35762,.F.);
#50303=ORIENTED_EDGE('',*,*,#36001,.F.);
#50304=ORIENTED_EDGE('',*,*,#35847,.F.);
#50305=ORIENTED_EDGE('',*,*,#36002,.F.);
#50306=ORIENTED_EDGE('',*,*,#35763,.F.);
#50307=ORIENTED_EDGE('',*,*,#36000,.F.);
#50308=ORIENTED_EDGE('',*,*,#36002,.T.);
#50309=ORIENTED_EDGE('',*,*,#35846,.F.);
#50310=ORIENTED_EDGE('',*,*,#36003,.T.);
#50311=ORIENTED_EDGE('',*,*,#35764,.T.);
#50312=ORIENTED_EDGE('',*,*,#35999,.T.);
#50313=ORIENTED_EDGE('',*,*,#35849,.F.);
#50314=ORIENTED_EDGE('',*,*,#36001,.T.);
#50315=ORIENTED_EDGE('',*,*,#35761,.T.);
#50316=ORIENTED_EDGE('',*,*,#35766,.F.);
#50317=ORIENTED_EDGE('',*,*,#36004,.F.);
#50318=ORIENTED_EDGE('',*,*,#35844,.F.);
#50319=ORIENTED_EDGE('',*,*,#36005,.F.);
#50320=ORIENTED_EDGE('',*,*,#35765,.F.);
#50321=ORIENTED_EDGE('',*,*,#36003,.F.);
#50322=ORIENTED_EDGE('',*,*,#35845,.F.);
#50323=ORIENTED_EDGE('',*,*,#36004,.T.);
#50324=ORIENTED_EDGE('',*,*,#36005,.T.);
#50325=ORIENTED_EDGE('',*,*,#35843,.F.);
#50326=ORIENTED_EDGE('',*,*,#36006,.T.);
#50327=ORIENTED_EDGE('',*,*,#35767,.T.);
#50328=ORIENTED_EDGE('',*,*,#35842,.F.);
#50329=ORIENTED_EDGE('',*,*,#36007,.T.);
#50330=ORIENTED_EDGE('',*,*,#35768,.F.);
#50331=ORIENTED_EDGE('',*,*,#36006,.F.);
#50332=ORIENTED_EDGE('',*,*,#35841,.F.);
#50333=ORIENTED_EDGE('',*,*,#36008,.F.);
#50334=ORIENTED_EDGE('',*,*,#35769,.F.);
#50335=ORIENTED_EDGE('',*,*,#36007,.F.);
#50336=ORIENTED_EDGE('',*,*,#35839,.F.);
#50337=ORIENTED_EDGE('',*,*,#36009,.T.);
#50338=ORIENTED_EDGE('',*,*,#35771,.F.);
#50339=ORIENTED_EDGE('',*,*,#36010,.F.);
#50340=ORIENTED_EDGE('',*,*,#35838,.F.);
#50341=ORIENTED_EDGE('',*,*,#35776,.F.);
#50342=ORIENTED_EDGE('',*,*,#35772,.F.);
#50343=ORIENTED_EDGE('',*,*,#36009,.F.);
#50344=ORIENTED_EDGE('',*,*,#36011,.T.);
#50345=ORIENTED_EDGE('',*,*,#36012,.T.);
#50346=ORIENTED_EDGE('',*,*,#36013,.F.);
#50347=ORIENTED_EDGE('',*,*,#36012,.F.);
#50348=ORIENTED_EDGE('',*,*,#36014,.F.);
#50349=ORIENTED_EDGE('',*,*,#36013,.T.);
#50350=ORIENTED_EDGE('',*,*,#36015,.F.);
#50351=ORIENTED_EDGE('',*,*,#36016,.T.);
#50352=ORIENTED_EDGE('',*,*,#36014,.T.);
#50353=ORIENTED_EDGE('',*,*,#36016,.F.);
#50354=ORIENTED_EDGE('',*,*,#36017,.F.);
#50355=ORIENTED_EDGE('',*,*,#36018,.T.);
#50356=ORIENTED_EDGE('',*,*,#36015,.T.);
#50357=ORIENTED_EDGE('',*,*,#36018,.F.);
#50358=ORIENTED_EDGE('',*,*,#36019,.F.);
#50359=ORIENTED_EDGE('',*,*,#36020,.T.);
#50360=ORIENTED_EDGE('',*,*,#36017,.T.);
#50361=ORIENTED_EDGE('',*,*,#36020,.F.);
#50362=ORIENTED_EDGE('',*,*,#36021,.F.);
#50363=ORIENTED_EDGE('',*,*,#36019,.T.);
#50364=ORIENTED_EDGE('',*,*,#36022,.F.);
#50365=ORIENTED_EDGE('',*,*,#36023,.T.);
#50366=ORIENTED_EDGE('',*,*,#36021,.T.);
#50367=ORIENTED_EDGE('',*,*,#36023,.F.);
#50368=ORIENTED_EDGE('',*,*,#35639,.T.);
#50369=ORIENTED_EDGE('',*,*,#35641,.T.);
#50370=ORIENTED_EDGE('',*,*,#35640,.T.);
#50371=ORIENTED_EDGE('',*,*,#36024,.F.);
#50372=ORIENTED_EDGE('',*,*,#36025,.T.);
#50373=ORIENTED_EDGE('',*,*,#36022,.T.);
#50374=ORIENTED_EDGE('',*,*,#36025,.F.);
#50375=ORIENTED_EDGE('',*,*,#35711,.F.);
#50376=ORIENTED_EDGE('',*,*,#36024,.T.);
#50377=ORIENTED_EDGE('',*,*,#36008,.T.);
#50378=ORIENTED_EDGE('',*,*,#35840,.F.);
#50379=ORIENTED_EDGE('',*,*,#36010,.T.);
#50380=ORIENTED_EDGE('',*,*,#35770,.T.);
#50381=ORIENTED_EDGE('',*,*,#35784,.T.);
#50382=ORIENTED_EDGE('',*,*,#36026,.F.);
#50383=ORIENTED_EDGE('',*,*,#36026,.T.);
#50384=ORIENTED_EDGE('',*,*,#36027,.T.);
#50385=ORIENTED_EDGE('',*,*,#36028,.F.);
#50386=ORIENTED_EDGE('',*,*,#36027,.F.);
#50387=ORIENTED_EDGE('',*,*,#36028,.T.);
#50388=ORIENTED_EDGE('',*,*,#36029,.T.);
#50389=ORIENTED_EDGE('',*,*,#36030,.F.);
#50390=ORIENTED_EDGE('',*,*,#36029,.F.);
#50391=ORIENTED_EDGE('',*,*,#36030,.T.);
#50392=ORIENTED_EDGE('',*,*,#36031,.T.);
#50393=ORIENTED_EDGE('',*,*,#36011,.F.);
#50394=ORIENTED_EDGE('',*,*,#36031,.F.);
#50395=ORIENTED_EDGE('',*,*,#35645,.T.);
#50396=ORIENTED_EDGE('',*,*,#35646,.T.);
#50397=ORIENTED_EDGE('',*,*,#35643,.T.);
#50398=ORIENTED_EDGE('',*,*,#35636,.T.);
#50399=ORIENTED_EDGE('',*,*,#36032,.T.);
#50400=ORIENTED_EDGE('',*,*,#36033,.T.);
#50401=ORIENTED_EDGE('',*,*,#36034,.F.);
#50402=ORIENTED_EDGE('',*,*,#36033,.F.);
#50403=ORIENTED_EDGE('',*,*,#36035,.F.);
#50404=ORIENTED_EDGE('',*,*,#36034,.T.);
#50405=ORIENTED_EDGE('',*,*,#36036,.F.);
#50406=ORIENTED_EDGE('',*,*,#36037,.T.);
#50407=ORIENTED_EDGE('',*,*,#36035,.T.);
#50408=ORIENTED_EDGE('',*,*,#36037,.F.);
#50409=ORIENTED_EDGE('',*,*,#36038,.F.);
#50410=ORIENTED_EDGE('',*,*,#36039,.T.);
#50411=ORIENTED_EDGE('',*,*,#36036,.T.);
#50412=ORIENTED_EDGE('',*,*,#36039,.F.);
#50413=ORIENTED_EDGE('',*,*,#36040,.F.);
#50414=ORIENTED_EDGE('',*,*,#36038,.T.);
#50415=ORIENTED_EDGE('',*,*,#36041,.F.);
#50416=ORIENTED_EDGE('',*,*,#36042,.T.);
#50417=ORIENTED_EDGE('',*,*,#36040,.T.);
#50418=ORIENTED_EDGE('',*,*,#36042,.F.);
#50419=ORIENTED_EDGE('',*,*,#36043,.F.);
#50420=ORIENTED_EDGE('',*,*,#36044,.T.);
#50421=ORIENTED_EDGE('',*,*,#36041,.T.);
#50422=ORIENTED_EDGE('',*,*,#36044,.F.);
#50423=ORIENTED_EDGE('',*,*,#36043,.T.);
#50424=ORIENTED_EDGE('',*,*,#36045,.F.);
#50425=ORIENTED_EDGE('',*,*,#36045,.T.);
#50426=ORIENTED_EDGE('',*,*,#36046,.T.);
#50427=ORIENTED_EDGE('',*,*,#36047,.F.);
#50428=ORIENTED_EDGE('',*,*,#36046,.F.);
#50429=ORIENTED_EDGE('',*,*,#36047,.T.);
#50430=ORIENTED_EDGE('',*,*,#36048,.T.);
#50431=ORIENTED_EDGE('',*,*,#36032,.F.);
#50432=ORIENTED_EDGE('',*,*,#36048,.F.);
#50433=ORIENTED_EDGE('',*,*,#36049,.T.);
#50434=ORIENTED_EDGE('',*,*,#36050,.T.);
#50435=ORIENTED_EDGE('',*,*,#36051,.T.);
#50436=ORIENTED_EDGE('',*,*,#36050,.F.);
#50437=ORIENTED_EDGE('',*,*,#36051,.F.);
#50438=ORIENTED_EDGE('',*,*,#36052,.T.);
#50439=ORIENTED_EDGE('',*,*,#36053,.T.);
#50440=ORIENTED_EDGE('',*,*,#36052,.F.);
#50441=ORIENTED_EDGE('',*,*,#36054,.T.);
#50442=ORIENTED_EDGE('',*,*,#36055,.T.);
#50443=ORIENTED_EDGE('',*,*,#36056,.F.);
#50444=ORIENTED_EDGE('',*,*,#36057,.F.);
#50445=ORIENTED_EDGE('',*,*,#36049,.F.);
#50446=ORIENTED_EDGE('',*,*,#36058,.T.);
#50447=ORIENTED_EDGE('',*,*,#36059,.T.);
#50448=ORIENTED_EDGE('',*,*,#36060,.T.);
#50449=ORIENTED_EDGE('',*,*,#36059,.F.);
#50450=ORIENTED_EDGE('',*,*,#36060,.F.);
#50451=ORIENTED_EDGE('',*,*,#36061,.T.);
#50452=ORIENTED_EDGE('',*,*,#36062,.T.);
#50453=ORIENTED_EDGE('',*,*,#36061,.F.);
#50454=ORIENTED_EDGE('',*,*,#36063,.T.);
#50455=ORIENTED_EDGE('',*,*,#36064,.T.);
#50456=ORIENTED_EDGE('',*,*,#36065,.F.);
#50457=ORIENTED_EDGE('',*,*,#36066,.F.);
#50458=ORIENTED_EDGE('',*,*,#36058,.F.);
#50459=ORIENTED_EDGE('',*,*,#36062,.F.);
#50460=ORIENTED_EDGE('',*,*,#36067,.F.);
#50461=ORIENTED_EDGE('',*,*,#36053,.F.);
#50462=ORIENTED_EDGE('',*,*,#36068,.F.);
#50463=ORIENTED_EDGE('',*,*,#36067,.T.);
#50464=ORIENTED_EDGE('',*,*,#36069,.T.);
#50465=ORIENTED_EDGE('',*,*,#36070,.F.);
#50466=ORIENTED_EDGE('',*,*,#36069,.F.);
#50467=ORIENTED_EDGE('',*,*,#36068,.T.);
#50468=ORIENTED_EDGE('',*,*,#36071,.T.);
#50469=ORIENTED_EDGE('',*,*,#36072,.F.);
#50470=ORIENTED_EDGE('',*,*,#36071,.F.);
#50471=ORIENTED_EDGE('',*,*,#36073,.T.);
#50472=ORIENTED_EDGE('',*,*,#36074,.T.);
#50473=ORIENTED_EDGE('',*,*,#36075,.T.);
#50474=ORIENTED_EDGE('',*,*,#36076,.T.);
#50475=ORIENTED_EDGE('',*,*,#36073,.F.);
#50476=ORIENTED_EDGE('',*,*,#36077,.F.);
#50477=ORIENTED_EDGE('',*,*,#36078,.F.);
#50478=ORIENTED_EDGE('',*,*,#36079,.T.);
#50479=ORIENTED_EDGE('',*,*,#36057,.T.);
#50480=ORIENTED_EDGE('',*,*,#36080,.F.);
#50481=ORIENTED_EDGE('',*,*,#36076,.F.);
#50482=ORIENTED_EDGE('',*,*,#36081,.F.);
#50483=ORIENTED_EDGE('',*,*,#36082,.F.);
#50484=ORIENTED_EDGE('',*,*,#36077,.T.);
#50485=ORIENTED_EDGE('',*,*,#36070,.T.);
#50486=ORIENTED_EDGE('',*,*,#36072,.T.);
#50487=ORIENTED_EDGE('',*,*,#36078,.T.);
#50488=ORIENTED_EDGE('',*,*,#36082,.T.);
#50489=ORIENTED_EDGE('',*,*,#36083,.T.);
#50490=ORIENTED_EDGE('',*,*,#36084,.T.);
#50491=ORIENTED_EDGE('',*,*,#36085,.T.);
#50492=ORIENTED_EDGE('',*,*,#36066,.T.);
#50493=ORIENTED_EDGE('',*,*,#36086,.F.);
#50494=ORIENTED_EDGE('',*,*,#36087,.F.);
#50495=ORIENTED_EDGE('',*,*,#36088,.T.);
#50496=ORIENTED_EDGE('',*,*,#36087,.T.);
#50497=ORIENTED_EDGE('',*,*,#36089,.F.);
#50498=ORIENTED_EDGE('',*,*,#36090,.F.);
#50499=ORIENTED_EDGE('',*,*,#36091,.T.);
#50500=ORIENTED_EDGE('',*,*,#36090,.T.);
#50501=ORIENTED_EDGE('',*,*,#36092,.F.);
#50502=ORIENTED_EDGE('',*,*,#36093,.F.);
#50503=ORIENTED_EDGE('',*,*,#36094,.T.);
#50504=ORIENTED_EDGE('',*,*,#36093,.T.);
#50505=ORIENTED_EDGE('',*,*,#36095,.F.);
#50506=ORIENTED_EDGE('',*,*,#36096,.F.);
#50507=ORIENTED_EDGE('',*,*,#36097,.T.);
#50508=ORIENTED_EDGE('',*,*,#36096,.T.);
#50509=ORIENTED_EDGE('',*,*,#36098,.F.);
#50510=ORIENTED_EDGE('',*,*,#36099,.F.);
#50511=ORIENTED_EDGE('',*,*,#36100,.T.);
#50512=ORIENTED_EDGE('',*,*,#36099,.T.);
#50513=ORIENTED_EDGE('',*,*,#36101,.F.);
#50514=ORIENTED_EDGE('',*,*,#36102,.F.);
#50515=ORIENTED_EDGE('',*,*,#36103,.T.);
#50516=ORIENTED_EDGE('',*,*,#36102,.T.);
#50517=ORIENTED_EDGE('',*,*,#36104,.F.);
#50518=ORIENTED_EDGE('',*,*,#36105,.F.);
#50519=ORIENTED_EDGE('',*,*,#36106,.T.);
#50520=ORIENTED_EDGE('',*,*,#36105,.T.);
#50521=ORIENTED_EDGE('',*,*,#36107,.F.);
#50522=ORIENTED_EDGE('',*,*,#36108,.F.);
#50523=ORIENTED_EDGE('',*,*,#36109,.T.);
#50524=ORIENTED_EDGE('',*,*,#36108,.T.);
#50525=ORIENTED_EDGE('',*,*,#36110,.F.);
#50526=ORIENTED_EDGE('',*,*,#36111,.F.);
#50527=ORIENTED_EDGE('',*,*,#36112,.T.);
#50528=ORIENTED_EDGE('',*,*,#36111,.T.);
#50529=ORIENTED_EDGE('',*,*,#36113,.F.);
#50530=ORIENTED_EDGE('',*,*,#36114,.F.);
#50531=ORIENTED_EDGE('',*,*,#36115,.T.);
#50532=ORIENTED_EDGE('',*,*,#36114,.T.);
#50533=ORIENTED_EDGE('',*,*,#36116,.F.);
#50534=ORIENTED_EDGE('',*,*,#36117,.F.);
#50535=ORIENTED_EDGE('',*,*,#36118,.T.);
#50536=ORIENTED_EDGE('',*,*,#36117,.T.);
#50537=ORIENTED_EDGE('',*,*,#36119,.F.);
#50538=ORIENTED_EDGE('',*,*,#36120,.F.);
#50539=ORIENTED_EDGE('',*,*,#36121,.T.);
#50540=ORIENTED_EDGE('',*,*,#36120,.T.);
#50541=ORIENTED_EDGE('',*,*,#36122,.F.);
#50542=ORIENTED_EDGE('',*,*,#36123,.F.);
#50543=ORIENTED_EDGE('',*,*,#36124,.T.);
#50544=ORIENTED_EDGE('',*,*,#36123,.T.);
#50545=ORIENTED_EDGE('',*,*,#36125,.F.);
#50546=ORIENTED_EDGE('',*,*,#36126,.F.);
#50547=ORIENTED_EDGE('',*,*,#36127,.T.);
#50548=ORIENTED_EDGE('',*,*,#36126,.T.);
#50549=ORIENTED_EDGE('',*,*,#36128,.F.);
#50550=ORIENTED_EDGE('',*,*,#36129,.F.);
#50551=ORIENTED_EDGE('',*,*,#36130,.T.);
#50552=ORIENTED_EDGE('',*,*,#36129,.T.);
#50553=ORIENTED_EDGE('',*,*,#36131,.F.);
#50554=ORIENTED_EDGE('',*,*,#36132,.F.);
#50555=ORIENTED_EDGE('',*,*,#36133,.T.);
#50556=ORIENTED_EDGE('',*,*,#36132,.T.);
#50557=ORIENTED_EDGE('',*,*,#36134,.F.);
#50558=ORIENTED_EDGE('',*,*,#36135,.F.);
#50559=ORIENTED_EDGE('',*,*,#36136,.T.);
#50560=ORIENTED_EDGE('',*,*,#36135,.T.);
#50561=ORIENTED_EDGE('',*,*,#36137,.F.);
#50562=ORIENTED_EDGE('',*,*,#36138,.F.);
#50563=ORIENTED_EDGE('',*,*,#36139,.T.);
#50564=ORIENTED_EDGE('',*,*,#36138,.T.);
#50565=ORIENTED_EDGE('',*,*,#36140,.F.);
#50566=ORIENTED_EDGE('',*,*,#36141,.F.);
#50567=ORIENTED_EDGE('',*,*,#36142,.T.);
#50568=ORIENTED_EDGE('',*,*,#36141,.T.);
#50569=ORIENTED_EDGE('',*,*,#36143,.F.);
#50570=ORIENTED_EDGE('',*,*,#36144,.F.);
#50571=ORIENTED_EDGE('',*,*,#36145,.T.);
#50572=ORIENTED_EDGE('',*,*,#36144,.T.);
#50573=ORIENTED_EDGE('',*,*,#36146,.F.);
#50574=ORIENTED_EDGE('',*,*,#36147,.F.);
#50575=ORIENTED_EDGE('',*,*,#36148,.T.);
#50576=ORIENTED_EDGE('',*,*,#36147,.T.);
#50577=ORIENTED_EDGE('',*,*,#36149,.F.);
#50578=ORIENTED_EDGE('',*,*,#36150,.F.);
#50579=ORIENTED_EDGE('',*,*,#36151,.T.);
#50580=ORIENTED_EDGE('',*,*,#36150,.T.);
#50581=ORIENTED_EDGE('',*,*,#36152,.F.);
#50582=ORIENTED_EDGE('',*,*,#36153,.F.);
#50583=ORIENTED_EDGE('',*,*,#36154,.T.);
#50584=ORIENTED_EDGE('',*,*,#36153,.T.);
#50585=ORIENTED_EDGE('',*,*,#36155,.F.);
#50586=ORIENTED_EDGE('',*,*,#36156,.F.);
#50587=ORIENTED_EDGE('',*,*,#36157,.T.);
#50588=ORIENTED_EDGE('',*,*,#36156,.T.);
#50589=ORIENTED_EDGE('',*,*,#36158,.F.);
#50590=ORIENTED_EDGE('',*,*,#36159,.F.);
#50591=ORIENTED_EDGE('',*,*,#36160,.T.);
#50592=ORIENTED_EDGE('',*,*,#36159,.T.);
#50593=ORIENTED_EDGE('',*,*,#36161,.F.);
#50594=ORIENTED_EDGE('',*,*,#36162,.F.);
#50595=ORIENTED_EDGE('',*,*,#36163,.T.);
#50596=ORIENTED_EDGE('',*,*,#36162,.T.);
#50597=ORIENTED_EDGE('',*,*,#36164,.F.);
#50598=ORIENTED_EDGE('',*,*,#36165,.F.);
#50599=ORIENTED_EDGE('',*,*,#36166,.T.);
#50600=ORIENTED_EDGE('',*,*,#36165,.T.);
#50601=ORIENTED_EDGE('',*,*,#36167,.F.);
#50602=ORIENTED_EDGE('',*,*,#36168,.F.);
#50603=ORIENTED_EDGE('',*,*,#36169,.T.);
#50604=ORIENTED_EDGE('',*,*,#36168,.T.);
#50605=ORIENTED_EDGE('',*,*,#36170,.F.);
#50606=ORIENTED_EDGE('',*,*,#36171,.F.);
#50607=ORIENTED_EDGE('',*,*,#36172,.T.);
#50608=ORIENTED_EDGE('',*,*,#36171,.T.);
#50609=ORIENTED_EDGE('',*,*,#36173,.F.);
#50610=ORIENTED_EDGE('',*,*,#36174,.F.);
#50611=ORIENTED_EDGE('',*,*,#36175,.T.);
#50612=ORIENTED_EDGE('',*,*,#36174,.T.);
#50613=ORIENTED_EDGE('',*,*,#36176,.F.);
#50614=ORIENTED_EDGE('',*,*,#36177,.F.);
#50615=ORIENTED_EDGE('',*,*,#36178,.T.);
#50616=ORIENTED_EDGE('',*,*,#36177,.T.);
#50617=ORIENTED_EDGE('',*,*,#36179,.F.);
#50618=ORIENTED_EDGE('',*,*,#36180,.F.);
#50619=ORIENTED_EDGE('',*,*,#36181,.T.);
#50620=ORIENTED_EDGE('',*,*,#36180,.T.);
#50621=ORIENTED_EDGE('',*,*,#36182,.F.);
#50622=ORIENTED_EDGE('',*,*,#36183,.F.);
#50623=ORIENTED_EDGE('',*,*,#36184,.T.);
#50624=ORIENTED_EDGE('',*,*,#36183,.T.);
#50625=ORIENTED_EDGE('',*,*,#36185,.F.);
#50626=ORIENTED_EDGE('',*,*,#36186,.F.);
#50627=ORIENTED_EDGE('',*,*,#36187,.T.);
#50628=ORIENTED_EDGE('',*,*,#36186,.T.);
#50629=ORIENTED_EDGE('',*,*,#36188,.F.);
#50630=ORIENTED_EDGE('',*,*,#36189,.F.);
#50631=ORIENTED_EDGE('',*,*,#36190,.T.);
#50632=ORIENTED_EDGE('',*,*,#36189,.T.);
#50633=ORIENTED_EDGE('',*,*,#36191,.F.);
#50634=ORIENTED_EDGE('',*,*,#36192,.F.);
#50635=ORIENTED_EDGE('',*,*,#36193,.T.);
#50636=ORIENTED_EDGE('',*,*,#36192,.T.);
#50637=ORIENTED_EDGE('',*,*,#36194,.F.);
#50638=ORIENTED_EDGE('',*,*,#36195,.F.);
#50639=ORIENTED_EDGE('',*,*,#36196,.T.);
#50640=ORIENTED_EDGE('',*,*,#36195,.T.);
#50641=ORIENTED_EDGE('',*,*,#36197,.F.);
#50642=ORIENTED_EDGE('',*,*,#36198,.F.);
#50643=ORIENTED_EDGE('',*,*,#36199,.T.);
#50644=ORIENTED_EDGE('',*,*,#36198,.T.);
#50645=ORIENTED_EDGE('',*,*,#36200,.F.);
#50646=ORIENTED_EDGE('',*,*,#36201,.F.);
#50647=ORIENTED_EDGE('',*,*,#36202,.T.);
#50648=ORIENTED_EDGE('',*,*,#36201,.T.);
#50649=ORIENTED_EDGE('',*,*,#36203,.F.);
#50650=ORIENTED_EDGE('',*,*,#36204,.F.);
#50651=ORIENTED_EDGE('',*,*,#36205,.T.);
#50652=ORIENTED_EDGE('',*,*,#36204,.T.);
#50653=ORIENTED_EDGE('',*,*,#36206,.F.);
#50654=ORIENTED_EDGE('',*,*,#36207,.F.);
#50655=ORIENTED_EDGE('',*,*,#36208,.T.);
#50656=ORIENTED_EDGE('',*,*,#36207,.T.);
#50657=ORIENTED_EDGE('',*,*,#36209,.F.);
#50658=ORIENTED_EDGE('',*,*,#36210,.F.);
#50659=ORIENTED_EDGE('',*,*,#36211,.T.);
#50660=ORIENTED_EDGE('',*,*,#36210,.T.);
#50661=ORIENTED_EDGE('',*,*,#36212,.F.);
#50662=ORIENTED_EDGE('',*,*,#36213,.F.);
#50663=ORIENTED_EDGE('',*,*,#36214,.T.);
#50664=ORIENTED_EDGE('',*,*,#36213,.T.);
#50665=ORIENTED_EDGE('',*,*,#36215,.F.);
#50666=ORIENTED_EDGE('',*,*,#36216,.F.);
#50667=ORIENTED_EDGE('',*,*,#36217,.T.);
#50668=ORIENTED_EDGE('',*,*,#36216,.T.);
#50669=ORIENTED_EDGE('',*,*,#36218,.F.);
#50670=ORIENTED_EDGE('',*,*,#36219,.F.);
#50671=ORIENTED_EDGE('',*,*,#36220,.T.);
#50672=ORIENTED_EDGE('',*,*,#36219,.T.);
#50673=ORIENTED_EDGE('',*,*,#36221,.F.);
#50674=ORIENTED_EDGE('',*,*,#36222,.F.);
#50675=ORIENTED_EDGE('',*,*,#36223,.T.);
#50676=ORIENTED_EDGE('',*,*,#36222,.T.);
#50677=ORIENTED_EDGE('',*,*,#36224,.F.);
#50678=ORIENTED_EDGE('',*,*,#36225,.F.);
#50679=ORIENTED_EDGE('',*,*,#36226,.T.);
#50680=ORIENTED_EDGE('',*,*,#36225,.T.);
#50681=ORIENTED_EDGE('',*,*,#36227,.F.);
#50682=ORIENTED_EDGE('',*,*,#36228,.F.);
#50683=ORIENTED_EDGE('',*,*,#36229,.T.);
#50684=ORIENTED_EDGE('',*,*,#36228,.T.);
#50685=ORIENTED_EDGE('',*,*,#36230,.F.);
#50686=ORIENTED_EDGE('',*,*,#36231,.F.);
#50687=ORIENTED_EDGE('',*,*,#36232,.T.);
#50688=ORIENTED_EDGE('',*,*,#36231,.T.);
#50689=ORIENTED_EDGE('',*,*,#36233,.F.);
#50690=ORIENTED_EDGE('',*,*,#36234,.F.);
#50691=ORIENTED_EDGE('',*,*,#36235,.T.);
#50692=ORIENTED_EDGE('',*,*,#36234,.T.);
#50693=ORIENTED_EDGE('',*,*,#36236,.F.);
#50694=ORIENTED_EDGE('',*,*,#36237,.F.);
#50695=ORIENTED_EDGE('',*,*,#36238,.T.);
#50696=ORIENTED_EDGE('',*,*,#36237,.T.);
#50697=ORIENTED_EDGE('',*,*,#36239,.F.);
#50698=ORIENTED_EDGE('',*,*,#36240,.F.);
#50699=ORIENTED_EDGE('',*,*,#36241,.T.);
#50700=ORIENTED_EDGE('',*,*,#36240,.T.);
#50701=ORIENTED_EDGE('',*,*,#36242,.F.);
#50702=ORIENTED_EDGE('',*,*,#36243,.F.);
#50703=ORIENTED_EDGE('',*,*,#36244,.T.);
#50704=ORIENTED_EDGE('',*,*,#36243,.T.);
#50705=ORIENTED_EDGE('',*,*,#36245,.F.);
#50706=ORIENTED_EDGE('',*,*,#36246,.F.);
#50707=ORIENTED_EDGE('',*,*,#36247,.T.);
#50708=ORIENTED_EDGE('',*,*,#36246,.T.);
#50709=ORIENTED_EDGE('',*,*,#36248,.F.);
#50710=ORIENTED_EDGE('',*,*,#36249,.F.);
#50711=ORIENTED_EDGE('',*,*,#36250,.T.);
#50712=ORIENTED_EDGE('',*,*,#36249,.T.);
#50713=ORIENTED_EDGE('',*,*,#36251,.F.);
#50714=ORIENTED_EDGE('',*,*,#36252,.F.);
#50715=ORIENTED_EDGE('',*,*,#36253,.T.);
#50716=ORIENTED_EDGE('',*,*,#36252,.T.);
#50717=ORIENTED_EDGE('',*,*,#36254,.F.);
#50718=ORIENTED_EDGE('',*,*,#36255,.F.);
#50719=ORIENTED_EDGE('',*,*,#36256,.T.);
#50720=ORIENTED_EDGE('',*,*,#36255,.T.);
#50721=ORIENTED_EDGE('',*,*,#36257,.F.);
#50722=ORIENTED_EDGE('',*,*,#36258,.F.);
#50723=ORIENTED_EDGE('',*,*,#36259,.T.);
#50724=ORIENTED_EDGE('',*,*,#36258,.T.);
#50725=ORIENTED_EDGE('',*,*,#36260,.F.);
#50726=ORIENTED_EDGE('',*,*,#36261,.F.);
#50727=ORIENTED_EDGE('',*,*,#36262,.T.);
#50728=ORIENTED_EDGE('',*,*,#36261,.T.);
#50729=ORIENTED_EDGE('',*,*,#36263,.F.);
#50730=ORIENTED_EDGE('',*,*,#36264,.F.);
#50731=ORIENTED_EDGE('',*,*,#36265,.T.);
#50732=ORIENTED_EDGE('',*,*,#36264,.T.);
#50733=ORIENTED_EDGE('',*,*,#36266,.F.);
#50734=ORIENTED_EDGE('',*,*,#36267,.F.);
#50735=ORIENTED_EDGE('',*,*,#36268,.T.);
#50736=ORIENTED_EDGE('',*,*,#36267,.T.);
#50737=ORIENTED_EDGE('',*,*,#36269,.F.);
#50738=ORIENTED_EDGE('',*,*,#36270,.F.);
#50739=ORIENTED_EDGE('',*,*,#36271,.T.);
#50740=ORIENTED_EDGE('',*,*,#36270,.T.);
#50741=ORIENTED_EDGE('',*,*,#36272,.F.);
#50742=ORIENTED_EDGE('',*,*,#36273,.F.);
#50743=ORIENTED_EDGE('',*,*,#36274,.T.);
#50744=ORIENTED_EDGE('',*,*,#36273,.T.);
#50745=ORIENTED_EDGE('',*,*,#36275,.F.);
#50746=ORIENTED_EDGE('',*,*,#36276,.F.);
#50747=ORIENTED_EDGE('',*,*,#36277,.T.);
#50748=ORIENTED_EDGE('',*,*,#36276,.T.);
#50749=ORIENTED_EDGE('',*,*,#36278,.F.);
#50750=ORIENTED_EDGE('',*,*,#36279,.F.);
#50751=ORIENTED_EDGE('',*,*,#36280,.T.);
#50752=ORIENTED_EDGE('',*,*,#36279,.T.);
#50753=ORIENTED_EDGE('',*,*,#36281,.F.);
#50754=ORIENTED_EDGE('',*,*,#36282,.F.);
#50755=ORIENTED_EDGE('',*,*,#36283,.T.);
#50756=ORIENTED_EDGE('',*,*,#36282,.T.);
#50757=ORIENTED_EDGE('',*,*,#36284,.F.);
#50758=ORIENTED_EDGE('',*,*,#36285,.F.);
#50759=ORIENTED_EDGE('',*,*,#36286,.T.);
#50760=ORIENTED_EDGE('',*,*,#36285,.T.);
#50761=ORIENTED_EDGE('',*,*,#36287,.F.);
#50762=ORIENTED_EDGE('',*,*,#36288,.F.);
#50763=ORIENTED_EDGE('',*,*,#36289,.T.);
#50764=ORIENTED_EDGE('',*,*,#36288,.T.);
#50765=ORIENTED_EDGE('',*,*,#36290,.F.);
#50766=ORIENTED_EDGE('',*,*,#36291,.F.);
#50767=ORIENTED_EDGE('',*,*,#36292,.T.);
#50768=ORIENTED_EDGE('',*,*,#36291,.T.);
#50769=ORIENTED_EDGE('',*,*,#36293,.F.);
#50770=ORIENTED_EDGE('',*,*,#36294,.F.);
#50771=ORIENTED_EDGE('',*,*,#36295,.T.);
#50772=ORIENTED_EDGE('',*,*,#36294,.T.);
#50773=ORIENTED_EDGE('',*,*,#36296,.F.);
#50774=ORIENTED_EDGE('',*,*,#36297,.F.);
#50775=ORIENTED_EDGE('',*,*,#36298,.T.);
#50776=ORIENTED_EDGE('',*,*,#36297,.T.);
#50777=ORIENTED_EDGE('',*,*,#36299,.F.);
#50778=ORIENTED_EDGE('',*,*,#36300,.F.);
#50779=ORIENTED_EDGE('',*,*,#36301,.T.);
#50780=ORIENTED_EDGE('',*,*,#36300,.T.);
#50781=ORIENTED_EDGE('',*,*,#36302,.F.);
#50782=ORIENTED_EDGE('',*,*,#36303,.F.);
#50783=ORIENTED_EDGE('',*,*,#36304,.T.);
#50784=ORIENTED_EDGE('',*,*,#36303,.T.);
#50785=ORIENTED_EDGE('',*,*,#36305,.F.);
#50786=ORIENTED_EDGE('',*,*,#36306,.F.);
#50787=ORIENTED_EDGE('',*,*,#36307,.T.);
#50788=ORIENTED_EDGE('',*,*,#36306,.T.);
#50789=ORIENTED_EDGE('',*,*,#36308,.F.);
#50790=ORIENTED_EDGE('',*,*,#36309,.F.);
#50791=ORIENTED_EDGE('',*,*,#36310,.T.);
#50792=ORIENTED_EDGE('',*,*,#36309,.T.);
#50793=ORIENTED_EDGE('',*,*,#36311,.F.);
#50794=ORIENTED_EDGE('',*,*,#36312,.F.);
#50795=ORIENTED_EDGE('',*,*,#36313,.T.);
#50796=ORIENTED_EDGE('',*,*,#36312,.T.);
#50797=ORIENTED_EDGE('',*,*,#36314,.F.);
#50798=ORIENTED_EDGE('',*,*,#36315,.F.);
#50799=ORIENTED_EDGE('',*,*,#36316,.T.);
#50800=ORIENTED_EDGE('',*,*,#36315,.T.);
#50801=ORIENTED_EDGE('',*,*,#36317,.F.);
#50802=ORIENTED_EDGE('',*,*,#36318,.F.);
#50803=ORIENTED_EDGE('',*,*,#36319,.T.);
#50804=ORIENTED_EDGE('',*,*,#36318,.T.);
#50805=ORIENTED_EDGE('',*,*,#36320,.F.);
#50806=ORIENTED_EDGE('',*,*,#36321,.F.);
#50807=ORIENTED_EDGE('',*,*,#36322,.T.);
#50808=ORIENTED_EDGE('',*,*,#36321,.T.);
#50809=ORIENTED_EDGE('',*,*,#36323,.F.);
#50810=ORIENTED_EDGE('',*,*,#36324,.F.);
#50811=ORIENTED_EDGE('',*,*,#36325,.T.);
#50812=ORIENTED_EDGE('',*,*,#36324,.T.);
#50813=ORIENTED_EDGE('',*,*,#36326,.F.);
#50814=ORIENTED_EDGE('',*,*,#36327,.F.);
#50815=ORIENTED_EDGE('',*,*,#36328,.T.);
#50816=ORIENTED_EDGE('',*,*,#36327,.T.);
#50817=ORIENTED_EDGE('',*,*,#36329,.F.);
#50818=ORIENTED_EDGE('',*,*,#36330,.F.);
#50819=ORIENTED_EDGE('',*,*,#36331,.T.);
#50820=ORIENTED_EDGE('',*,*,#36330,.T.);
#50821=ORIENTED_EDGE('',*,*,#36332,.F.);
#50822=ORIENTED_EDGE('',*,*,#36333,.F.);
#50823=ORIENTED_EDGE('',*,*,#36334,.T.);
#50824=ORIENTED_EDGE('',*,*,#36333,.T.);
#50825=ORIENTED_EDGE('',*,*,#36335,.F.);
#50826=ORIENTED_EDGE('',*,*,#36336,.F.);
#50827=ORIENTED_EDGE('',*,*,#36337,.T.);
#50828=ORIENTED_EDGE('',*,*,#36336,.T.);
#50829=ORIENTED_EDGE('',*,*,#36338,.F.);
#50830=ORIENTED_EDGE('',*,*,#36339,.F.);
#50831=ORIENTED_EDGE('',*,*,#36340,.T.);
#50832=ORIENTED_EDGE('',*,*,#36339,.T.);
#50833=ORIENTED_EDGE('',*,*,#36341,.F.);
#50834=ORIENTED_EDGE('',*,*,#36342,.F.);
#50835=ORIENTED_EDGE('',*,*,#36343,.T.);
#50836=ORIENTED_EDGE('',*,*,#36342,.T.);
#50837=ORIENTED_EDGE('',*,*,#36344,.F.);
#50838=ORIENTED_EDGE('',*,*,#36345,.F.);
#50839=ORIENTED_EDGE('',*,*,#36346,.T.);
#50840=ORIENTED_EDGE('',*,*,#36345,.T.);
#50841=ORIENTED_EDGE('',*,*,#36347,.F.);
#50842=ORIENTED_EDGE('',*,*,#36348,.F.);
#50843=ORIENTED_EDGE('',*,*,#36349,.T.);
#50844=ORIENTED_EDGE('',*,*,#36348,.T.);
#50845=ORIENTED_EDGE('',*,*,#36350,.F.);
#50846=ORIENTED_EDGE('',*,*,#36351,.F.);
#50847=ORIENTED_EDGE('',*,*,#36352,.T.);
#50848=ORIENTED_EDGE('',*,*,#36351,.T.);
#50849=ORIENTED_EDGE('',*,*,#36353,.F.);
#50850=ORIENTED_EDGE('',*,*,#36354,.F.);
#50851=ORIENTED_EDGE('',*,*,#36355,.T.);
#50852=ORIENTED_EDGE('',*,*,#36354,.T.);
#50853=ORIENTED_EDGE('',*,*,#36356,.F.);
#50854=ORIENTED_EDGE('',*,*,#36357,.F.);
#50855=ORIENTED_EDGE('',*,*,#36358,.T.);
#50856=ORIENTED_EDGE('',*,*,#36357,.T.);
#50857=ORIENTED_EDGE('',*,*,#36359,.F.);
#50858=ORIENTED_EDGE('',*,*,#36360,.F.);
#50859=ORIENTED_EDGE('',*,*,#36361,.T.);
#50860=ORIENTED_EDGE('',*,*,#36360,.T.);
#50861=ORIENTED_EDGE('',*,*,#36362,.F.);
#50862=ORIENTED_EDGE('',*,*,#36363,.F.);
#50863=ORIENTED_EDGE('',*,*,#36364,.T.);
#50864=ORIENTED_EDGE('',*,*,#36363,.T.);
#50865=ORIENTED_EDGE('',*,*,#36365,.F.);
#50866=ORIENTED_EDGE('',*,*,#36366,.F.);
#50867=ORIENTED_EDGE('',*,*,#36367,.T.);
#50868=ORIENTED_EDGE('',*,*,#36366,.T.);
#50869=ORIENTED_EDGE('',*,*,#36368,.F.);
#50870=ORIENTED_EDGE('',*,*,#36369,.F.);
#50871=ORIENTED_EDGE('',*,*,#36370,.T.);
#50872=ORIENTED_EDGE('',*,*,#36369,.T.);
#50873=ORIENTED_EDGE('',*,*,#36371,.F.);
#50874=ORIENTED_EDGE('',*,*,#36372,.F.);
#50875=ORIENTED_EDGE('',*,*,#36373,.T.);
#50876=ORIENTED_EDGE('',*,*,#36372,.T.);
#50877=ORIENTED_EDGE('',*,*,#36374,.F.);
#50878=ORIENTED_EDGE('',*,*,#36375,.F.);
#50879=ORIENTED_EDGE('',*,*,#36376,.T.);
#50880=ORIENTED_EDGE('',*,*,#36375,.T.);
#50881=ORIENTED_EDGE('',*,*,#36377,.F.);
#50882=ORIENTED_EDGE('',*,*,#36378,.F.);
#50883=ORIENTED_EDGE('',*,*,#36379,.T.);
#50884=ORIENTED_EDGE('',*,*,#36378,.T.);
#50885=ORIENTED_EDGE('',*,*,#36380,.F.);
#50886=ORIENTED_EDGE('',*,*,#36381,.F.);
#50887=ORIENTED_EDGE('',*,*,#36382,.T.);
#50888=ORIENTED_EDGE('',*,*,#36381,.T.);
#50889=ORIENTED_EDGE('',*,*,#36383,.F.);
#50890=ORIENTED_EDGE('',*,*,#36384,.F.);
#50891=ORIENTED_EDGE('',*,*,#36385,.T.);
#50892=ORIENTED_EDGE('',*,*,#36384,.T.);
#50893=ORIENTED_EDGE('',*,*,#36386,.F.);
#50894=ORIENTED_EDGE('',*,*,#36387,.F.);
#50895=ORIENTED_EDGE('',*,*,#36388,.T.);
#50896=ORIENTED_EDGE('',*,*,#36387,.T.);
#50897=ORIENTED_EDGE('',*,*,#36389,.F.);
#50898=ORIENTED_EDGE('',*,*,#36390,.F.);
#50899=ORIENTED_EDGE('',*,*,#36391,.T.);
#50900=ORIENTED_EDGE('',*,*,#36390,.T.);
#50901=ORIENTED_EDGE('',*,*,#36392,.F.);
#50902=ORIENTED_EDGE('',*,*,#36393,.F.);
#50903=ORIENTED_EDGE('',*,*,#36394,.T.);
#50904=ORIENTED_EDGE('',*,*,#36393,.T.);
#50905=ORIENTED_EDGE('',*,*,#36395,.F.);
#50906=ORIENTED_EDGE('',*,*,#36396,.F.);
#50907=ORIENTED_EDGE('',*,*,#36397,.T.);
#50908=ORIENTED_EDGE('',*,*,#36396,.T.);
#50909=ORIENTED_EDGE('',*,*,#36398,.F.);
#50910=ORIENTED_EDGE('',*,*,#36399,.F.);
#50911=ORIENTED_EDGE('',*,*,#36400,.T.);
#50912=ORIENTED_EDGE('',*,*,#36399,.T.);
#50913=ORIENTED_EDGE('',*,*,#36401,.F.);
#50914=ORIENTED_EDGE('',*,*,#36402,.F.);
#50915=ORIENTED_EDGE('',*,*,#36403,.T.);
#50916=ORIENTED_EDGE('',*,*,#36402,.T.);
#50917=ORIENTED_EDGE('',*,*,#36404,.F.);
#50918=ORIENTED_EDGE('',*,*,#36405,.F.);
#50919=ORIENTED_EDGE('',*,*,#36406,.T.);
#50920=ORIENTED_EDGE('',*,*,#36405,.T.);
#50921=ORIENTED_EDGE('',*,*,#36407,.F.);
#50922=ORIENTED_EDGE('',*,*,#36408,.F.);
#50923=ORIENTED_EDGE('',*,*,#36409,.T.);
#50924=ORIENTED_EDGE('',*,*,#36408,.T.);
#50925=ORIENTED_EDGE('',*,*,#36410,.F.);
#50926=ORIENTED_EDGE('',*,*,#36411,.F.);
#50927=ORIENTED_EDGE('',*,*,#36412,.T.);
#50928=ORIENTED_EDGE('',*,*,#36411,.T.);
#50929=ORIENTED_EDGE('',*,*,#36413,.F.);
#50930=ORIENTED_EDGE('',*,*,#36414,.F.);
#50931=ORIENTED_EDGE('',*,*,#36415,.T.);
#50932=ORIENTED_EDGE('',*,*,#36414,.T.);
#50933=ORIENTED_EDGE('',*,*,#36416,.F.);
#50934=ORIENTED_EDGE('',*,*,#36417,.F.);
#50935=ORIENTED_EDGE('',*,*,#36418,.T.);
#50936=ORIENTED_EDGE('',*,*,#36417,.T.);
#50937=ORIENTED_EDGE('',*,*,#36419,.F.);
#50938=ORIENTED_EDGE('',*,*,#36420,.F.);
#50939=ORIENTED_EDGE('',*,*,#36421,.T.);
#50940=ORIENTED_EDGE('',*,*,#36420,.T.);
#50941=ORIENTED_EDGE('',*,*,#36422,.F.);
#50942=ORIENTED_EDGE('',*,*,#36423,.F.);
#50943=ORIENTED_EDGE('',*,*,#36424,.T.);
#50944=ORIENTED_EDGE('',*,*,#36423,.T.);
#50945=ORIENTED_EDGE('',*,*,#36425,.F.);
#50946=ORIENTED_EDGE('',*,*,#36426,.F.);
#50947=ORIENTED_EDGE('',*,*,#36427,.T.);
#50948=ORIENTED_EDGE('',*,*,#36426,.T.);
#50949=ORIENTED_EDGE('',*,*,#36428,.F.);
#50950=ORIENTED_EDGE('',*,*,#36429,.F.);
#50951=ORIENTED_EDGE('',*,*,#36430,.T.);
#50952=ORIENTED_EDGE('',*,*,#36429,.T.);
#50953=ORIENTED_EDGE('',*,*,#36431,.F.);
#50954=ORIENTED_EDGE('',*,*,#36432,.F.);
#50955=ORIENTED_EDGE('',*,*,#36433,.T.);
#50956=ORIENTED_EDGE('',*,*,#36432,.T.);
#50957=ORIENTED_EDGE('',*,*,#36434,.F.);
#50958=ORIENTED_EDGE('',*,*,#36435,.F.);
#50959=ORIENTED_EDGE('',*,*,#36436,.T.);
#50960=ORIENTED_EDGE('',*,*,#36435,.T.);
#50961=ORIENTED_EDGE('',*,*,#36437,.F.);
#50962=ORIENTED_EDGE('',*,*,#36438,.F.);
#50963=ORIENTED_EDGE('',*,*,#36439,.T.);
#50964=ORIENTED_EDGE('',*,*,#36438,.T.);
#50965=ORIENTED_EDGE('',*,*,#36440,.F.);
#50966=ORIENTED_EDGE('',*,*,#36441,.F.);
#50967=ORIENTED_EDGE('',*,*,#36442,.T.);
#50968=ORIENTED_EDGE('',*,*,#36441,.T.);
#50969=ORIENTED_EDGE('',*,*,#36443,.F.);
#50970=ORIENTED_EDGE('',*,*,#36444,.F.);
#50971=ORIENTED_EDGE('',*,*,#36445,.T.);
#50972=ORIENTED_EDGE('',*,*,#36444,.T.);
#50973=ORIENTED_EDGE('',*,*,#36446,.F.);
#50974=ORIENTED_EDGE('',*,*,#36447,.F.);
#50975=ORIENTED_EDGE('',*,*,#36448,.T.);
#50976=ORIENTED_EDGE('',*,*,#36447,.T.);
#50977=ORIENTED_EDGE('',*,*,#36449,.F.);
#50978=ORIENTED_EDGE('',*,*,#36450,.F.);
#50979=ORIENTED_EDGE('',*,*,#36451,.T.);
#50980=ORIENTED_EDGE('',*,*,#36450,.T.);
#50981=ORIENTED_EDGE('',*,*,#36452,.F.);
#50982=ORIENTED_EDGE('',*,*,#36453,.F.);
#50983=ORIENTED_EDGE('',*,*,#36454,.T.);
#50984=ORIENTED_EDGE('',*,*,#36453,.T.);
#50985=ORIENTED_EDGE('',*,*,#36455,.F.);
#50986=ORIENTED_EDGE('',*,*,#36456,.F.);
#50987=ORIENTED_EDGE('',*,*,#36457,.T.);
#50988=ORIENTED_EDGE('',*,*,#36456,.T.);
#50989=ORIENTED_EDGE('',*,*,#36458,.F.);
#50990=ORIENTED_EDGE('',*,*,#36459,.F.);
#50991=ORIENTED_EDGE('',*,*,#36460,.T.);
#50992=ORIENTED_EDGE('',*,*,#36459,.T.);
#50993=ORIENTED_EDGE('',*,*,#36461,.F.);
#50994=ORIENTED_EDGE('',*,*,#36462,.F.);
#50995=ORIENTED_EDGE('',*,*,#36463,.T.);
#50996=ORIENTED_EDGE('',*,*,#36462,.T.);
#50997=ORIENTED_EDGE('',*,*,#36464,.F.);
#50998=ORIENTED_EDGE('',*,*,#36465,.F.);
#50999=ORIENTED_EDGE('',*,*,#36466,.T.);
#51000=ORIENTED_EDGE('',*,*,#36465,.T.);
#51001=ORIENTED_EDGE('',*,*,#36467,.F.);
#51002=ORIENTED_EDGE('',*,*,#36468,.F.);
#51003=ORIENTED_EDGE('',*,*,#36469,.T.);
#51004=ORIENTED_EDGE('',*,*,#36468,.T.);
#51005=ORIENTED_EDGE('',*,*,#36470,.F.);
#51006=ORIENTED_EDGE('',*,*,#36471,.F.);
#51007=ORIENTED_EDGE('',*,*,#36472,.T.);
#51008=ORIENTED_EDGE('',*,*,#36471,.T.);
#51009=ORIENTED_EDGE('',*,*,#36473,.F.);
#51010=ORIENTED_EDGE('',*,*,#36474,.F.);
#51011=ORIENTED_EDGE('',*,*,#36475,.T.);
#51012=ORIENTED_EDGE('',*,*,#36474,.T.);
#51013=ORIENTED_EDGE('',*,*,#36476,.F.);
#51014=ORIENTED_EDGE('',*,*,#36477,.F.);
#51015=ORIENTED_EDGE('',*,*,#36478,.T.);
#51016=ORIENTED_EDGE('',*,*,#36477,.T.);
#51017=ORIENTED_EDGE('',*,*,#36479,.F.);
#51018=ORIENTED_EDGE('',*,*,#36480,.F.);
#51019=ORIENTED_EDGE('',*,*,#36481,.T.);
#51020=ORIENTED_EDGE('',*,*,#36480,.T.);
#51021=ORIENTED_EDGE('',*,*,#36482,.F.);
#51022=ORIENTED_EDGE('',*,*,#36483,.F.);
#51023=ORIENTED_EDGE('',*,*,#36484,.T.);
#51024=ORIENTED_EDGE('',*,*,#36483,.T.);
#51025=ORIENTED_EDGE('',*,*,#36485,.F.);
#51026=ORIENTED_EDGE('',*,*,#36486,.F.);
#51027=ORIENTED_EDGE('',*,*,#36487,.T.);
#51028=ORIENTED_EDGE('',*,*,#36486,.T.);
#51029=ORIENTED_EDGE('',*,*,#36488,.F.);
#51030=ORIENTED_EDGE('',*,*,#36489,.F.);
#51031=ORIENTED_EDGE('',*,*,#36490,.T.);
#51032=ORIENTED_EDGE('',*,*,#36489,.T.);
#51033=ORIENTED_EDGE('',*,*,#36491,.F.);
#51034=ORIENTED_EDGE('',*,*,#36492,.F.);
#51035=ORIENTED_EDGE('',*,*,#36493,.T.);
#51036=ORIENTED_EDGE('',*,*,#36492,.T.);
#51037=ORIENTED_EDGE('',*,*,#36494,.F.);
#51038=ORIENTED_EDGE('',*,*,#36495,.F.);
#51039=ORIENTED_EDGE('',*,*,#36496,.T.);
#51040=ORIENTED_EDGE('',*,*,#36495,.T.);
#51041=ORIENTED_EDGE('',*,*,#36497,.F.);
#51042=ORIENTED_EDGE('',*,*,#36498,.F.);
#51043=ORIENTED_EDGE('',*,*,#36499,.T.);
#51044=ORIENTED_EDGE('',*,*,#36498,.T.);
#51045=ORIENTED_EDGE('',*,*,#36500,.F.);
#51046=ORIENTED_EDGE('',*,*,#36501,.F.);
#51047=ORIENTED_EDGE('',*,*,#36502,.T.);
#51048=ORIENTED_EDGE('',*,*,#36501,.T.);
#51049=ORIENTED_EDGE('',*,*,#36503,.F.);
#51050=ORIENTED_EDGE('',*,*,#36504,.F.);
#51051=ORIENTED_EDGE('',*,*,#36505,.T.);
#51052=ORIENTED_EDGE('',*,*,#36504,.T.);
#51053=ORIENTED_EDGE('',*,*,#36506,.F.);
#51054=ORIENTED_EDGE('',*,*,#36507,.F.);
#51055=ORIENTED_EDGE('',*,*,#36508,.T.);
#51056=ORIENTED_EDGE('',*,*,#36507,.T.);
#51057=ORIENTED_EDGE('',*,*,#36509,.F.);
#51058=ORIENTED_EDGE('',*,*,#36510,.F.);
#51059=ORIENTED_EDGE('',*,*,#36511,.T.);
#51060=ORIENTED_EDGE('',*,*,#36510,.T.);
#51061=ORIENTED_EDGE('',*,*,#36512,.F.);
#51062=ORIENTED_EDGE('',*,*,#36513,.F.);
#51063=ORIENTED_EDGE('',*,*,#36514,.T.);
#51064=ORIENTED_EDGE('',*,*,#36513,.T.);
#51065=ORIENTED_EDGE('',*,*,#36515,.F.);
#51066=ORIENTED_EDGE('',*,*,#36516,.F.);
#51067=ORIENTED_EDGE('',*,*,#36517,.T.);
#51068=ORIENTED_EDGE('',*,*,#36516,.T.);
#51069=ORIENTED_EDGE('',*,*,#36518,.F.);
#51070=ORIENTED_EDGE('',*,*,#36519,.F.);
#51071=ORIENTED_EDGE('',*,*,#36520,.T.);
#51072=ORIENTED_EDGE('',*,*,#36519,.T.);
#51073=ORIENTED_EDGE('',*,*,#36521,.F.);
#51074=ORIENTED_EDGE('',*,*,#36522,.F.);
#51075=ORIENTED_EDGE('',*,*,#36523,.T.);
#51076=ORIENTED_EDGE('',*,*,#36522,.T.);
#51077=ORIENTED_EDGE('',*,*,#36524,.F.);
#51078=ORIENTED_EDGE('',*,*,#36525,.F.);
#51079=ORIENTED_EDGE('',*,*,#36526,.T.);
#51080=ORIENTED_EDGE('',*,*,#36525,.T.);
#51081=ORIENTED_EDGE('',*,*,#36527,.F.);
#51082=ORIENTED_EDGE('',*,*,#36528,.F.);
#51083=ORIENTED_EDGE('',*,*,#36529,.T.);
#51084=ORIENTED_EDGE('',*,*,#36528,.T.);
#51085=ORIENTED_EDGE('',*,*,#36530,.F.);
#51086=ORIENTED_EDGE('',*,*,#36531,.F.);
#51087=ORIENTED_EDGE('',*,*,#36532,.T.);
#51088=ORIENTED_EDGE('',*,*,#36531,.T.);
#51089=ORIENTED_EDGE('',*,*,#36533,.F.);
#51090=ORIENTED_EDGE('',*,*,#36534,.F.);
#51091=ORIENTED_EDGE('',*,*,#36535,.T.);
#51092=ORIENTED_EDGE('',*,*,#36534,.T.);
#51093=ORIENTED_EDGE('',*,*,#36536,.F.);
#51094=ORIENTED_EDGE('',*,*,#36537,.F.);
#51095=ORIENTED_EDGE('',*,*,#36538,.T.);
#51096=ORIENTED_EDGE('',*,*,#36537,.T.);
#51097=ORIENTED_EDGE('',*,*,#36539,.F.);
#51098=ORIENTED_EDGE('',*,*,#36540,.F.);
#51099=ORIENTED_EDGE('',*,*,#36541,.T.);
#51100=ORIENTED_EDGE('',*,*,#36540,.T.);
#51101=ORIENTED_EDGE('',*,*,#36542,.F.);
#51102=ORIENTED_EDGE('',*,*,#36543,.F.);
#51103=ORIENTED_EDGE('',*,*,#36544,.T.);
#51104=ORIENTED_EDGE('',*,*,#36543,.T.);
#51105=ORIENTED_EDGE('',*,*,#36545,.F.);
#51106=ORIENTED_EDGE('',*,*,#36546,.F.);
#51107=ORIENTED_EDGE('',*,*,#36547,.T.);
#51108=ORIENTED_EDGE('',*,*,#36546,.T.);
#51109=ORIENTED_EDGE('',*,*,#36548,.F.);
#51110=ORIENTED_EDGE('',*,*,#36549,.F.);
#51111=ORIENTED_EDGE('',*,*,#36550,.T.);
#51112=ORIENTED_EDGE('',*,*,#36549,.T.);
#51113=ORIENTED_EDGE('',*,*,#36551,.F.);
#51114=ORIENTED_EDGE('',*,*,#36552,.F.);
#51115=ORIENTED_EDGE('',*,*,#36553,.T.);
#51116=ORIENTED_EDGE('',*,*,#36552,.T.);
#51117=ORIENTED_EDGE('',*,*,#36554,.F.);
#51118=ORIENTED_EDGE('',*,*,#36555,.F.);
#51119=ORIENTED_EDGE('',*,*,#36556,.T.);
#51120=ORIENTED_EDGE('',*,*,#36555,.T.);
#51121=ORIENTED_EDGE('',*,*,#36557,.F.);
#51122=ORIENTED_EDGE('',*,*,#36558,.F.);
#51123=ORIENTED_EDGE('',*,*,#36559,.T.);
#51124=ORIENTED_EDGE('',*,*,#36558,.T.);
#51125=ORIENTED_EDGE('',*,*,#36560,.F.);
#51126=ORIENTED_EDGE('',*,*,#36561,.F.);
#51127=ORIENTED_EDGE('',*,*,#36562,.T.);
#51128=ORIENTED_EDGE('',*,*,#36561,.T.);
#51129=ORIENTED_EDGE('',*,*,#36563,.F.);
#51130=ORIENTED_EDGE('',*,*,#36564,.F.);
#51131=ORIENTED_EDGE('',*,*,#36565,.T.);
#51132=ORIENTED_EDGE('',*,*,#36564,.T.);
#51133=ORIENTED_EDGE('',*,*,#36566,.F.);
#51134=ORIENTED_EDGE('',*,*,#36567,.F.);
#51135=ORIENTED_EDGE('',*,*,#36568,.T.);
#51136=ORIENTED_EDGE('',*,*,#36567,.T.);
#51137=ORIENTED_EDGE('',*,*,#36569,.F.);
#51138=ORIENTED_EDGE('',*,*,#36570,.F.);
#51139=ORIENTED_EDGE('',*,*,#36571,.T.);
#51140=ORIENTED_EDGE('',*,*,#36570,.T.);
#51141=ORIENTED_EDGE('',*,*,#36572,.F.);
#51142=ORIENTED_EDGE('',*,*,#36573,.F.);
#51143=ORIENTED_EDGE('',*,*,#36574,.T.);
#51144=ORIENTED_EDGE('',*,*,#36573,.T.);
#51145=ORIENTED_EDGE('',*,*,#36575,.F.);
#51146=ORIENTED_EDGE('',*,*,#36576,.F.);
#51147=ORIENTED_EDGE('',*,*,#36577,.T.);
#51148=ORIENTED_EDGE('',*,*,#36576,.T.);
#51149=ORIENTED_EDGE('',*,*,#36578,.F.);
#51150=ORIENTED_EDGE('',*,*,#36579,.F.);
#51151=ORIENTED_EDGE('',*,*,#36580,.T.);
#51152=ORIENTED_EDGE('',*,*,#36579,.T.);
#51153=ORIENTED_EDGE('',*,*,#36581,.F.);
#51154=ORIENTED_EDGE('',*,*,#36582,.F.);
#51155=ORIENTED_EDGE('',*,*,#36583,.T.);
#51156=ORIENTED_EDGE('',*,*,#36582,.T.);
#51157=ORIENTED_EDGE('',*,*,#36584,.F.);
#51158=ORIENTED_EDGE('',*,*,#36585,.F.);
#51159=ORIENTED_EDGE('',*,*,#36586,.T.);
#51160=ORIENTED_EDGE('',*,*,#36585,.T.);
#51161=ORIENTED_EDGE('',*,*,#36587,.F.);
#51162=ORIENTED_EDGE('',*,*,#36588,.F.);
#51163=ORIENTED_EDGE('',*,*,#36589,.T.);
#51164=ORIENTED_EDGE('',*,*,#36588,.T.);
#51165=ORIENTED_EDGE('',*,*,#36590,.F.);
#51166=ORIENTED_EDGE('',*,*,#36591,.F.);
#51167=ORIENTED_EDGE('',*,*,#36592,.T.);
#51168=ORIENTED_EDGE('',*,*,#36591,.T.);
#51169=ORIENTED_EDGE('',*,*,#36593,.F.);
#51170=ORIENTED_EDGE('',*,*,#36594,.F.);
#51171=ORIENTED_EDGE('',*,*,#36595,.T.);
#51172=ORIENTED_EDGE('',*,*,#36594,.T.);
#51173=ORIENTED_EDGE('',*,*,#36596,.F.);
#51174=ORIENTED_EDGE('',*,*,#36597,.F.);
#51175=ORIENTED_EDGE('',*,*,#36598,.T.);
#51176=ORIENTED_EDGE('',*,*,#36597,.T.);
#51177=ORIENTED_EDGE('',*,*,#36599,.F.);
#51178=ORIENTED_EDGE('',*,*,#36600,.F.);
#51179=ORIENTED_EDGE('',*,*,#36601,.T.);
#51180=ORIENTED_EDGE('',*,*,#36600,.T.);
#51181=ORIENTED_EDGE('',*,*,#36602,.F.);
#51182=ORIENTED_EDGE('',*,*,#36603,.F.);
#51183=ORIENTED_EDGE('',*,*,#36604,.T.);
#51184=ORIENTED_EDGE('',*,*,#36603,.T.);
#51185=ORIENTED_EDGE('',*,*,#36605,.F.);
#51186=ORIENTED_EDGE('',*,*,#36606,.F.);
#51187=ORIENTED_EDGE('',*,*,#36607,.T.);
#51188=ORIENTED_EDGE('',*,*,#36606,.T.);
#51189=ORIENTED_EDGE('',*,*,#36608,.F.);
#51190=ORIENTED_EDGE('',*,*,#36609,.F.);
#51191=ORIENTED_EDGE('',*,*,#36610,.T.);
#51192=ORIENTED_EDGE('',*,*,#36609,.T.);
#51193=ORIENTED_EDGE('',*,*,#36611,.F.);
#51194=ORIENTED_EDGE('',*,*,#36612,.F.);
#51195=ORIENTED_EDGE('',*,*,#36613,.T.);
#51196=ORIENTED_EDGE('',*,*,#36612,.T.);
#51197=ORIENTED_EDGE('',*,*,#36614,.F.);
#51198=ORIENTED_EDGE('',*,*,#36615,.F.);
#51199=ORIENTED_EDGE('',*,*,#36616,.T.);
#51200=ORIENTED_EDGE('',*,*,#36615,.T.);
#51201=ORIENTED_EDGE('',*,*,#36617,.F.);
#51202=ORIENTED_EDGE('',*,*,#36618,.F.);
#51203=ORIENTED_EDGE('',*,*,#36619,.T.);
#51204=ORIENTED_EDGE('',*,*,#36618,.T.);
#51205=ORIENTED_EDGE('',*,*,#36620,.F.);
#51206=ORIENTED_EDGE('',*,*,#36621,.F.);
#51207=ORIENTED_EDGE('',*,*,#36622,.T.);
#51208=ORIENTED_EDGE('',*,*,#36621,.T.);
#51209=ORIENTED_EDGE('',*,*,#36623,.F.);
#51210=ORIENTED_EDGE('',*,*,#36624,.F.);
#51211=ORIENTED_EDGE('',*,*,#36625,.T.);
#51212=ORIENTED_EDGE('',*,*,#36624,.T.);
#51213=ORIENTED_EDGE('',*,*,#36626,.F.);
#51214=ORIENTED_EDGE('',*,*,#36627,.F.);
#51215=ORIENTED_EDGE('',*,*,#36628,.T.);
#51216=ORIENTED_EDGE('',*,*,#36627,.T.);
#51217=ORIENTED_EDGE('',*,*,#36629,.F.);
#51218=ORIENTED_EDGE('',*,*,#36630,.F.);
#51219=ORIENTED_EDGE('',*,*,#36631,.T.);
#51220=ORIENTED_EDGE('',*,*,#36630,.T.);
#51221=ORIENTED_EDGE('',*,*,#36632,.F.);
#51222=ORIENTED_EDGE('',*,*,#36633,.F.);
#51223=ORIENTED_EDGE('',*,*,#36634,.T.);
#51224=ORIENTED_EDGE('',*,*,#36633,.T.);
#51225=ORIENTED_EDGE('',*,*,#36635,.F.);
#51226=ORIENTED_EDGE('',*,*,#36636,.F.);
#51227=ORIENTED_EDGE('',*,*,#36637,.T.);
#51228=ORIENTED_EDGE('',*,*,#36636,.T.);
#51229=ORIENTED_EDGE('',*,*,#36638,.F.);
#51230=ORIENTED_EDGE('',*,*,#36639,.F.);
#51231=ORIENTED_EDGE('',*,*,#36640,.T.);
#51232=ORIENTED_EDGE('',*,*,#36639,.T.);
#51233=ORIENTED_EDGE('',*,*,#36641,.F.);
#51234=ORIENTED_EDGE('',*,*,#36642,.F.);
#51235=ORIENTED_EDGE('',*,*,#36643,.T.);
#51236=ORIENTED_EDGE('',*,*,#36642,.T.);
#51237=ORIENTED_EDGE('',*,*,#36644,.F.);
#51238=ORIENTED_EDGE('',*,*,#36645,.F.);
#51239=ORIENTED_EDGE('',*,*,#36646,.T.);
#51240=ORIENTED_EDGE('',*,*,#36645,.T.);
#51241=ORIENTED_EDGE('',*,*,#36647,.F.);
#51242=ORIENTED_EDGE('',*,*,#36648,.F.);
#51243=ORIENTED_EDGE('',*,*,#36649,.T.);
#51244=ORIENTED_EDGE('',*,*,#36648,.T.);
#51245=ORIENTED_EDGE('',*,*,#36650,.F.);
#51246=ORIENTED_EDGE('',*,*,#36651,.F.);
#51247=ORIENTED_EDGE('',*,*,#36652,.T.);
#51248=ORIENTED_EDGE('',*,*,#36651,.T.);
#51249=ORIENTED_EDGE('',*,*,#36653,.F.);
#51250=ORIENTED_EDGE('',*,*,#36654,.F.);
#51251=ORIENTED_EDGE('',*,*,#36655,.T.);
#51252=ORIENTED_EDGE('',*,*,#36654,.T.);
#51253=ORIENTED_EDGE('',*,*,#36656,.F.);
#51254=ORIENTED_EDGE('',*,*,#36657,.F.);
#51255=ORIENTED_EDGE('',*,*,#36658,.T.);
#51256=ORIENTED_EDGE('',*,*,#36657,.T.);
#51257=ORIENTED_EDGE('',*,*,#36659,.F.);
#51258=ORIENTED_EDGE('',*,*,#36660,.F.);
#51259=ORIENTED_EDGE('',*,*,#36661,.T.);
#51260=ORIENTED_EDGE('',*,*,#36660,.T.);
#51261=ORIENTED_EDGE('',*,*,#36662,.F.);
#51262=ORIENTED_EDGE('',*,*,#36663,.F.);
#51263=ORIENTED_EDGE('',*,*,#36664,.T.);
#51264=ORIENTED_EDGE('',*,*,#36663,.T.);
#51265=ORIENTED_EDGE('',*,*,#36665,.F.);
#51266=ORIENTED_EDGE('',*,*,#36666,.F.);
#51267=ORIENTED_EDGE('',*,*,#36667,.T.);
#51268=ORIENTED_EDGE('',*,*,#36666,.T.);
#51269=ORIENTED_EDGE('',*,*,#36668,.F.);
#51270=ORIENTED_EDGE('',*,*,#36669,.F.);
#51271=ORIENTED_EDGE('',*,*,#36670,.T.);
#51272=ORIENTED_EDGE('',*,*,#36669,.T.);
#51273=ORIENTED_EDGE('',*,*,#36671,.F.);
#51274=ORIENTED_EDGE('',*,*,#36672,.F.);
#51275=ORIENTED_EDGE('',*,*,#36673,.T.);
#51276=ORIENTED_EDGE('',*,*,#36672,.T.);
#51277=ORIENTED_EDGE('',*,*,#36674,.F.);
#51278=ORIENTED_EDGE('',*,*,#36675,.F.);
#51279=ORIENTED_EDGE('',*,*,#36676,.T.);
#51280=ORIENTED_EDGE('',*,*,#36675,.T.);
#51281=ORIENTED_EDGE('',*,*,#36677,.F.);
#51282=ORIENTED_EDGE('',*,*,#36678,.F.);
#51283=ORIENTED_EDGE('',*,*,#36679,.T.);
#51284=ORIENTED_EDGE('',*,*,#36678,.T.);
#51285=ORIENTED_EDGE('',*,*,#36680,.F.);
#51286=ORIENTED_EDGE('',*,*,#36681,.F.);
#51287=ORIENTED_EDGE('',*,*,#36682,.T.);
#51288=ORIENTED_EDGE('',*,*,#36681,.T.);
#51289=ORIENTED_EDGE('',*,*,#36683,.F.);
#51290=ORIENTED_EDGE('',*,*,#36684,.F.);
#51291=ORIENTED_EDGE('',*,*,#36685,.T.);
#51292=ORIENTED_EDGE('',*,*,#36684,.T.);
#51293=ORIENTED_EDGE('',*,*,#36686,.F.);
#51294=ORIENTED_EDGE('',*,*,#36687,.F.);
#51295=ORIENTED_EDGE('',*,*,#36688,.T.);
#51296=ORIENTED_EDGE('',*,*,#36687,.T.);
#51297=ORIENTED_EDGE('',*,*,#36689,.F.);
#51298=ORIENTED_EDGE('',*,*,#36690,.F.);
#51299=ORIENTED_EDGE('',*,*,#36691,.T.);
#51300=ORIENTED_EDGE('',*,*,#36690,.T.);
#51301=ORIENTED_EDGE('',*,*,#36692,.F.);
#51302=ORIENTED_EDGE('',*,*,#36693,.F.);
#51303=ORIENTED_EDGE('',*,*,#36694,.T.);
#51304=ORIENTED_EDGE('',*,*,#36693,.T.);
#51305=ORIENTED_EDGE('',*,*,#36695,.F.);
#51306=ORIENTED_EDGE('',*,*,#36696,.F.);
#51307=ORIENTED_EDGE('',*,*,#36697,.T.);
#51308=ORIENTED_EDGE('',*,*,#36696,.T.);
#51309=ORIENTED_EDGE('',*,*,#36698,.F.);
#51310=ORIENTED_EDGE('',*,*,#36699,.F.);
#51311=ORIENTED_EDGE('',*,*,#36700,.T.);
#51312=ORIENTED_EDGE('',*,*,#36699,.T.);
#51313=ORIENTED_EDGE('',*,*,#36701,.F.);
#51314=ORIENTED_EDGE('',*,*,#36702,.F.);
#51315=ORIENTED_EDGE('',*,*,#36703,.T.);
#51316=ORIENTED_EDGE('',*,*,#36702,.T.);
#51317=ORIENTED_EDGE('',*,*,#36704,.F.);
#51318=ORIENTED_EDGE('',*,*,#36705,.F.);
#51319=ORIENTED_EDGE('',*,*,#36706,.T.);
#51320=ORIENTED_EDGE('',*,*,#36705,.T.);
#51321=ORIENTED_EDGE('',*,*,#36707,.F.);
#51322=ORIENTED_EDGE('',*,*,#36708,.F.);
#51323=ORIENTED_EDGE('',*,*,#36709,.T.);
#51324=ORIENTED_EDGE('',*,*,#36708,.T.);
#51325=ORIENTED_EDGE('',*,*,#36710,.F.);
#51326=ORIENTED_EDGE('',*,*,#36711,.F.);
#51327=ORIENTED_EDGE('',*,*,#36712,.T.);
#51328=ORIENTED_EDGE('',*,*,#36711,.T.);
#51329=ORIENTED_EDGE('',*,*,#36713,.F.);
#51330=ORIENTED_EDGE('',*,*,#36714,.F.);
#51331=ORIENTED_EDGE('',*,*,#36715,.T.);
#51332=ORIENTED_EDGE('',*,*,#36714,.T.);
#51333=ORIENTED_EDGE('',*,*,#36716,.F.);
#51334=ORIENTED_EDGE('',*,*,#36717,.F.);
#51335=ORIENTED_EDGE('',*,*,#36718,.T.);
#51336=ORIENTED_EDGE('',*,*,#36717,.T.);
#51337=ORIENTED_EDGE('',*,*,#36719,.F.);
#51338=ORIENTED_EDGE('',*,*,#36720,.F.);
#51339=ORIENTED_EDGE('',*,*,#36721,.T.);
#51340=ORIENTED_EDGE('',*,*,#36720,.T.);
#51341=ORIENTED_EDGE('',*,*,#36722,.F.);
#51342=ORIENTED_EDGE('',*,*,#36723,.F.);
#51343=ORIENTED_EDGE('',*,*,#36724,.T.);
#51344=ORIENTED_EDGE('',*,*,#36723,.T.);
#51345=ORIENTED_EDGE('',*,*,#36725,.F.);
#51346=ORIENTED_EDGE('',*,*,#36726,.F.);
#51347=ORIENTED_EDGE('',*,*,#36727,.T.);
#51348=ORIENTED_EDGE('',*,*,#36726,.T.);
#51349=ORIENTED_EDGE('',*,*,#36728,.F.);
#51350=ORIENTED_EDGE('',*,*,#36729,.F.);
#51351=ORIENTED_EDGE('',*,*,#36730,.T.);
#51352=ORIENTED_EDGE('',*,*,#36729,.T.);
#51353=ORIENTED_EDGE('',*,*,#36731,.F.);
#51354=ORIENTED_EDGE('',*,*,#36732,.F.);
#51355=ORIENTED_EDGE('',*,*,#36733,.T.);
#51356=ORIENTED_EDGE('',*,*,#36732,.T.);
#51357=ORIENTED_EDGE('',*,*,#36734,.F.);
#51358=ORIENTED_EDGE('',*,*,#36735,.F.);
#51359=ORIENTED_EDGE('',*,*,#36736,.T.);
#51360=ORIENTED_EDGE('',*,*,#36735,.T.);
#51361=ORIENTED_EDGE('',*,*,#36737,.F.);
#51362=ORIENTED_EDGE('',*,*,#36738,.F.);
#51363=ORIENTED_EDGE('',*,*,#36739,.T.);
#51364=ORIENTED_EDGE('',*,*,#36738,.T.);
#51365=ORIENTED_EDGE('',*,*,#36740,.F.);
#51366=ORIENTED_EDGE('',*,*,#36741,.F.);
#51367=ORIENTED_EDGE('',*,*,#36742,.T.);
#51368=ORIENTED_EDGE('',*,*,#36741,.T.);
#51369=ORIENTED_EDGE('',*,*,#36743,.F.);
#51370=ORIENTED_EDGE('',*,*,#36744,.F.);
#51371=ORIENTED_EDGE('',*,*,#36745,.T.);
#51372=ORIENTED_EDGE('',*,*,#36744,.T.);
#51373=ORIENTED_EDGE('',*,*,#36746,.F.);
#51374=ORIENTED_EDGE('',*,*,#36747,.F.);
#51375=ORIENTED_EDGE('',*,*,#36748,.T.);
#51376=ORIENTED_EDGE('',*,*,#36747,.T.);
#51377=ORIENTED_EDGE('',*,*,#36749,.F.);
#51378=ORIENTED_EDGE('',*,*,#36750,.F.);
#51379=ORIENTED_EDGE('',*,*,#36751,.T.);
#51380=ORIENTED_EDGE('',*,*,#36750,.T.);
#51381=ORIENTED_EDGE('',*,*,#36752,.F.);
#51382=ORIENTED_EDGE('',*,*,#36753,.F.);
#51383=ORIENTED_EDGE('',*,*,#36754,.T.);
#51384=ORIENTED_EDGE('',*,*,#36753,.T.);
#51385=ORIENTED_EDGE('',*,*,#36755,.F.);
#51386=ORIENTED_EDGE('',*,*,#36756,.F.);
#51387=ORIENTED_EDGE('',*,*,#36757,.T.);
#51388=ORIENTED_EDGE('',*,*,#36756,.T.);
#51389=ORIENTED_EDGE('',*,*,#36758,.F.);
#51390=ORIENTED_EDGE('',*,*,#36759,.F.);
#51391=ORIENTED_EDGE('',*,*,#36760,.T.);
#51392=ORIENTED_EDGE('',*,*,#36759,.T.);
#51393=ORIENTED_EDGE('',*,*,#36761,.F.);
#51394=ORIENTED_EDGE('',*,*,#36762,.F.);
#51395=ORIENTED_EDGE('',*,*,#36763,.T.);
#51396=ORIENTED_EDGE('',*,*,#36762,.T.);
#51397=ORIENTED_EDGE('',*,*,#36764,.F.);
#51398=ORIENTED_EDGE('',*,*,#36765,.F.);
#51399=ORIENTED_EDGE('',*,*,#36766,.T.);
#51400=ORIENTED_EDGE('',*,*,#36765,.T.);
#51401=ORIENTED_EDGE('',*,*,#36767,.F.);
#51402=ORIENTED_EDGE('',*,*,#36768,.F.);
#51403=ORIENTED_EDGE('',*,*,#36769,.T.);
#51404=ORIENTED_EDGE('',*,*,#36768,.T.);
#51405=ORIENTED_EDGE('',*,*,#36770,.F.);
#51406=ORIENTED_EDGE('',*,*,#36771,.F.);
#51407=ORIENTED_EDGE('',*,*,#36772,.T.);
#51408=ORIENTED_EDGE('',*,*,#36771,.T.);
#51409=ORIENTED_EDGE('',*,*,#36773,.F.);
#51410=ORIENTED_EDGE('',*,*,#36774,.F.);
#51411=ORIENTED_EDGE('',*,*,#36775,.T.);
#51412=ORIENTED_EDGE('',*,*,#36774,.T.);
#51413=ORIENTED_EDGE('',*,*,#36776,.F.);
#51414=ORIENTED_EDGE('',*,*,#36777,.F.);
#51415=ORIENTED_EDGE('',*,*,#36778,.T.);
#51416=ORIENTED_EDGE('',*,*,#36777,.T.);
#51417=ORIENTED_EDGE('',*,*,#36779,.F.);
#51418=ORIENTED_EDGE('',*,*,#36780,.F.);
#51419=ORIENTED_EDGE('',*,*,#36781,.T.);
#51420=ORIENTED_EDGE('',*,*,#36780,.T.);
#51421=ORIENTED_EDGE('',*,*,#36782,.F.);
#51422=ORIENTED_EDGE('',*,*,#36783,.F.);
#51423=ORIENTED_EDGE('',*,*,#36784,.T.);
#51424=ORIENTED_EDGE('',*,*,#36783,.T.);
#51425=ORIENTED_EDGE('',*,*,#36785,.F.);
#51426=ORIENTED_EDGE('',*,*,#36786,.F.);
#51427=ORIENTED_EDGE('',*,*,#36787,.T.);
#51428=ORIENTED_EDGE('',*,*,#36786,.T.);
#51429=ORIENTED_EDGE('',*,*,#36788,.F.);
#51430=ORIENTED_EDGE('',*,*,#36789,.F.);
#51431=ORIENTED_EDGE('',*,*,#36790,.T.);
#51432=ORIENTED_EDGE('',*,*,#36789,.T.);
#51433=ORIENTED_EDGE('',*,*,#36791,.F.);
#51434=ORIENTED_EDGE('',*,*,#36792,.F.);
#51435=ORIENTED_EDGE('',*,*,#36793,.T.);
#51436=ORIENTED_EDGE('',*,*,#36792,.T.);
#51437=ORIENTED_EDGE('',*,*,#36794,.F.);
#51438=ORIENTED_EDGE('',*,*,#36795,.F.);
#51439=ORIENTED_EDGE('',*,*,#36796,.T.);
#51440=ORIENTED_EDGE('',*,*,#36795,.T.);
#51441=ORIENTED_EDGE('',*,*,#36797,.F.);
#51442=ORIENTED_EDGE('',*,*,#36798,.F.);
#51443=ORIENTED_EDGE('',*,*,#36799,.T.);
#51444=ORIENTED_EDGE('',*,*,#36798,.T.);
#51445=ORIENTED_EDGE('',*,*,#36800,.F.);
#51446=ORIENTED_EDGE('',*,*,#36801,.F.);
#51447=ORIENTED_EDGE('',*,*,#36802,.T.);
#51448=ORIENTED_EDGE('',*,*,#36801,.T.);
#51449=ORIENTED_EDGE('',*,*,#36803,.F.);
#51450=ORIENTED_EDGE('',*,*,#36804,.F.);
#51451=ORIENTED_EDGE('',*,*,#36805,.T.);
#51452=ORIENTED_EDGE('',*,*,#36804,.T.);
#51453=ORIENTED_EDGE('',*,*,#36806,.F.);
#51454=ORIENTED_EDGE('',*,*,#36807,.F.);
#51455=ORIENTED_EDGE('',*,*,#36808,.T.);
#51456=ORIENTED_EDGE('',*,*,#36807,.T.);
#51457=ORIENTED_EDGE('',*,*,#36809,.F.);
#51458=ORIENTED_EDGE('',*,*,#36810,.F.);
#51459=ORIENTED_EDGE('',*,*,#36811,.T.);
#51460=ORIENTED_EDGE('',*,*,#36810,.T.);
#51461=ORIENTED_EDGE('',*,*,#36812,.F.);
#51462=ORIENTED_EDGE('',*,*,#36813,.F.);
#51463=ORIENTED_EDGE('',*,*,#36814,.T.);
#51464=ORIENTED_EDGE('',*,*,#36813,.T.);
#51465=ORIENTED_EDGE('',*,*,#36815,.F.);
#51466=ORIENTED_EDGE('',*,*,#36816,.F.);
#51467=ORIENTED_EDGE('',*,*,#36817,.T.);
#51468=ORIENTED_EDGE('',*,*,#36816,.T.);
#51469=ORIENTED_EDGE('',*,*,#36818,.F.);
#51470=ORIENTED_EDGE('',*,*,#36819,.F.);
#51471=ORIENTED_EDGE('',*,*,#36820,.T.);
#51472=ORIENTED_EDGE('',*,*,#36819,.T.);
#51473=ORIENTED_EDGE('',*,*,#36821,.F.);
#51474=ORIENTED_EDGE('',*,*,#36822,.F.);
#51475=ORIENTED_EDGE('',*,*,#36823,.T.);
#51476=ORIENTED_EDGE('',*,*,#36822,.T.);
#51477=ORIENTED_EDGE('',*,*,#36824,.F.);
#51478=ORIENTED_EDGE('',*,*,#36825,.F.);
#51479=ORIENTED_EDGE('',*,*,#36826,.T.);
#51480=ORIENTED_EDGE('',*,*,#36825,.T.);
#51481=ORIENTED_EDGE('',*,*,#36827,.F.);
#51482=ORIENTED_EDGE('',*,*,#36828,.F.);
#51483=ORIENTED_EDGE('',*,*,#36829,.T.);
#51484=ORIENTED_EDGE('',*,*,#36828,.T.);
#51485=ORIENTED_EDGE('',*,*,#36830,.F.);
#51486=ORIENTED_EDGE('',*,*,#36831,.F.);
#51487=ORIENTED_EDGE('',*,*,#36832,.T.);
#51488=ORIENTED_EDGE('',*,*,#36831,.T.);
#51489=ORIENTED_EDGE('',*,*,#36833,.F.);
#51490=ORIENTED_EDGE('',*,*,#36834,.F.);
#51491=ORIENTED_EDGE('',*,*,#36835,.T.);
#51492=ORIENTED_EDGE('',*,*,#36834,.T.);
#51493=ORIENTED_EDGE('',*,*,#36836,.F.);
#51494=ORIENTED_EDGE('',*,*,#36837,.F.);
#51495=ORIENTED_EDGE('',*,*,#36838,.T.);
#51496=ORIENTED_EDGE('',*,*,#36837,.T.);
#51497=ORIENTED_EDGE('',*,*,#36839,.F.);
#51498=ORIENTED_EDGE('',*,*,#36840,.F.);
#51499=ORIENTED_EDGE('',*,*,#36841,.T.);
#51500=ORIENTED_EDGE('',*,*,#36840,.T.);
#51501=ORIENTED_EDGE('',*,*,#36842,.F.);
#51502=ORIENTED_EDGE('',*,*,#36843,.F.);
#51503=ORIENTED_EDGE('',*,*,#36844,.T.);
#51504=ORIENTED_EDGE('',*,*,#36843,.T.);
#51505=ORIENTED_EDGE('',*,*,#36845,.F.);
#51506=ORIENTED_EDGE('',*,*,#36846,.F.);
#51507=ORIENTED_EDGE('',*,*,#36847,.T.);
#51508=ORIENTED_EDGE('',*,*,#36846,.T.);
#51509=ORIENTED_EDGE('',*,*,#36848,.F.);
#51510=ORIENTED_EDGE('',*,*,#36849,.F.);
#51511=ORIENTED_EDGE('',*,*,#36850,.T.);
#51512=ORIENTED_EDGE('',*,*,#36849,.T.);
#51513=ORIENTED_EDGE('',*,*,#36851,.F.);
#51514=ORIENTED_EDGE('',*,*,#36852,.F.);
#51515=ORIENTED_EDGE('',*,*,#36853,.T.);
#51516=ORIENTED_EDGE('',*,*,#36852,.T.);
#51517=ORIENTED_EDGE('',*,*,#36854,.F.);
#51518=ORIENTED_EDGE('',*,*,#36855,.F.);
#51519=ORIENTED_EDGE('',*,*,#36856,.T.);
#51520=ORIENTED_EDGE('',*,*,#36855,.T.);
#51521=ORIENTED_EDGE('',*,*,#36857,.F.);
#51522=ORIENTED_EDGE('',*,*,#36858,.F.);
#51523=ORIENTED_EDGE('',*,*,#36859,.T.);
#51524=ORIENTED_EDGE('',*,*,#36858,.T.);
#51525=ORIENTED_EDGE('',*,*,#36860,.F.);
#51526=ORIENTED_EDGE('',*,*,#36861,.F.);
#51527=ORIENTED_EDGE('',*,*,#36862,.T.);
#51528=ORIENTED_EDGE('',*,*,#36861,.T.);
#51529=ORIENTED_EDGE('',*,*,#36863,.F.);
#51530=ORIENTED_EDGE('',*,*,#36864,.F.);
#51531=ORIENTED_EDGE('',*,*,#36865,.T.);
#51532=ORIENTED_EDGE('',*,*,#36864,.T.);
#51533=ORIENTED_EDGE('',*,*,#36866,.F.);
#51534=ORIENTED_EDGE('',*,*,#36867,.F.);
#51535=ORIENTED_EDGE('',*,*,#36868,.T.);
#51536=ORIENTED_EDGE('',*,*,#36867,.T.);
#51537=ORIENTED_EDGE('',*,*,#36869,.F.);
#51538=ORIENTED_EDGE('',*,*,#36870,.F.);
#51539=ORIENTED_EDGE('',*,*,#36871,.T.);
#51540=ORIENTED_EDGE('',*,*,#36870,.T.);
#51541=ORIENTED_EDGE('',*,*,#36872,.F.);
#51542=ORIENTED_EDGE('',*,*,#36873,.F.);
#51543=ORIENTED_EDGE('',*,*,#36874,.T.);
#51544=ORIENTED_EDGE('',*,*,#36873,.T.);
#51545=ORIENTED_EDGE('',*,*,#36875,.F.);
#51546=ORIENTED_EDGE('',*,*,#36876,.F.);
#51547=ORIENTED_EDGE('',*,*,#36877,.T.);
#51548=ORIENTED_EDGE('',*,*,#36876,.T.);
#51549=ORIENTED_EDGE('',*,*,#36878,.F.);
#51550=ORIENTED_EDGE('',*,*,#36879,.F.);
#51551=ORIENTED_EDGE('',*,*,#36880,.T.);
#51552=ORIENTED_EDGE('',*,*,#36879,.T.);
#51553=ORIENTED_EDGE('',*,*,#36881,.F.);
#51554=ORIENTED_EDGE('',*,*,#36882,.F.);
#51555=ORIENTED_EDGE('',*,*,#36883,.T.);
#51556=ORIENTED_EDGE('',*,*,#36882,.T.);
#51557=ORIENTED_EDGE('',*,*,#36884,.F.);
#51558=ORIENTED_EDGE('',*,*,#36885,.F.);
#51559=ORIENTED_EDGE('',*,*,#36886,.T.);
#51560=ORIENTED_EDGE('',*,*,#36885,.T.);
#51561=ORIENTED_EDGE('',*,*,#36887,.F.);
#51562=ORIENTED_EDGE('',*,*,#36888,.F.);
#51563=ORIENTED_EDGE('',*,*,#36889,.T.);
#51564=ORIENTED_EDGE('',*,*,#36888,.T.);
#51565=ORIENTED_EDGE('',*,*,#36890,.F.);
#51566=ORIENTED_EDGE('',*,*,#36891,.F.);
#51567=ORIENTED_EDGE('',*,*,#36892,.T.);
#51568=ORIENTED_EDGE('',*,*,#36891,.T.);
#51569=ORIENTED_EDGE('',*,*,#36893,.F.);
#51570=ORIENTED_EDGE('',*,*,#36894,.F.);
#51571=ORIENTED_EDGE('',*,*,#36895,.T.);
#51572=ORIENTED_EDGE('',*,*,#36894,.T.);
#51573=ORIENTED_EDGE('',*,*,#36896,.F.);
#51574=ORIENTED_EDGE('',*,*,#36897,.F.);
#51575=ORIENTED_EDGE('',*,*,#36898,.T.);
#51576=ORIENTED_EDGE('',*,*,#36897,.T.);
#51577=ORIENTED_EDGE('',*,*,#36899,.F.);
#51578=ORIENTED_EDGE('',*,*,#36900,.F.);
#51579=ORIENTED_EDGE('',*,*,#36901,.T.);
#51580=ORIENTED_EDGE('',*,*,#36900,.T.);
#51581=ORIENTED_EDGE('',*,*,#36902,.F.);
#51582=ORIENTED_EDGE('',*,*,#36903,.F.);
#51583=ORIENTED_EDGE('',*,*,#36904,.T.);
#51584=ORIENTED_EDGE('',*,*,#36903,.T.);
#51585=ORIENTED_EDGE('',*,*,#36905,.F.);
#51586=ORIENTED_EDGE('',*,*,#36906,.F.);
#51587=ORIENTED_EDGE('',*,*,#36907,.T.);
#51588=ORIENTED_EDGE('',*,*,#36906,.T.);
#51589=ORIENTED_EDGE('',*,*,#36908,.F.);
#51590=ORIENTED_EDGE('',*,*,#36909,.F.);
#51591=ORIENTED_EDGE('',*,*,#36910,.T.);
#51592=ORIENTED_EDGE('',*,*,#36909,.T.);
#51593=ORIENTED_EDGE('',*,*,#36911,.F.);
#51594=ORIENTED_EDGE('',*,*,#36912,.F.);
#51595=ORIENTED_EDGE('',*,*,#36913,.T.);
#51596=ORIENTED_EDGE('',*,*,#36912,.T.);
#51597=ORIENTED_EDGE('',*,*,#36914,.F.);
#51598=ORIENTED_EDGE('',*,*,#36915,.F.);
#51599=ORIENTED_EDGE('',*,*,#36916,.T.);
#51600=ORIENTED_EDGE('',*,*,#36915,.T.);
#51601=ORIENTED_EDGE('',*,*,#36917,.F.);
#51602=ORIENTED_EDGE('',*,*,#36918,.F.);
#51603=ORIENTED_EDGE('',*,*,#36919,.T.);
#51604=ORIENTED_EDGE('',*,*,#36918,.T.);
#51605=ORIENTED_EDGE('',*,*,#36920,.F.);
#51606=ORIENTED_EDGE('',*,*,#36921,.F.);
#51607=ORIENTED_EDGE('',*,*,#36922,.T.);
#51608=ORIENTED_EDGE('',*,*,#36921,.T.);
#51609=ORIENTED_EDGE('',*,*,#36923,.F.);
#51610=ORIENTED_EDGE('',*,*,#36924,.F.);
#51611=ORIENTED_EDGE('',*,*,#36925,.T.);
#51612=ORIENTED_EDGE('',*,*,#36924,.T.);
#51613=ORIENTED_EDGE('',*,*,#36926,.F.);
#51614=ORIENTED_EDGE('',*,*,#36927,.F.);
#51615=ORIENTED_EDGE('',*,*,#36928,.T.);
#51616=ORIENTED_EDGE('',*,*,#36927,.T.);
#51617=ORIENTED_EDGE('',*,*,#36929,.F.);
#51618=ORIENTED_EDGE('',*,*,#36930,.F.);
#51619=ORIENTED_EDGE('',*,*,#36931,.T.);
#51620=ORIENTED_EDGE('',*,*,#36930,.T.);
#51621=ORIENTED_EDGE('',*,*,#36932,.F.);
#51622=ORIENTED_EDGE('',*,*,#36933,.F.);
#51623=ORIENTED_EDGE('',*,*,#36934,.T.);
#51624=ORIENTED_EDGE('',*,*,#36933,.T.);
#51625=ORIENTED_EDGE('',*,*,#36935,.F.);
#51626=ORIENTED_EDGE('',*,*,#36936,.F.);
#51627=ORIENTED_EDGE('',*,*,#36937,.T.);
#51628=ORIENTED_EDGE('',*,*,#36936,.T.);
#51629=ORIENTED_EDGE('',*,*,#36938,.F.);
#51630=ORIENTED_EDGE('',*,*,#36939,.F.);
#51631=ORIENTED_EDGE('',*,*,#36940,.T.);
#51632=ORIENTED_EDGE('',*,*,#36939,.T.);
#51633=ORIENTED_EDGE('',*,*,#36941,.F.);
#51634=ORIENTED_EDGE('',*,*,#36942,.F.);
#51635=ORIENTED_EDGE('',*,*,#36943,.T.);
#51636=ORIENTED_EDGE('',*,*,#36942,.T.);
#51637=ORIENTED_EDGE('',*,*,#36944,.F.);
#51638=ORIENTED_EDGE('',*,*,#36945,.F.);
#51639=ORIENTED_EDGE('',*,*,#36946,.T.);
#51640=ORIENTED_EDGE('',*,*,#36945,.T.);
#51641=ORIENTED_EDGE('',*,*,#36947,.F.);
#51642=ORIENTED_EDGE('',*,*,#36948,.F.);
#51643=ORIENTED_EDGE('',*,*,#36949,.T.);
#51644=ORIENTED_EDGE('',*,*,#36948,.T.);
#51645=ORIENTED_EDGE('',*,*,#36950,.F.);
#51646=ORIENTED_EDGE('',*,*,#36951,.F.);
#51647=ORIENTED_EDGE('',*,*,#36952,.T.);
#51648=ORIENTED_EDGE('',*,*,#36951,.T.);
#51649=ORIENTED_EDGE('',*,*,#36953,.F.);
#51650=ORIENTED_EDGE('',*,*,#36954,.F.);
#51651=ORIENTED_EDGE('',*,*,#36955,.T.);
#51652=ORIENTED_EDGE('',*,*,#36954,.T.);
#51653=ORIENTED_EDGE('',*,*,#36956,.F.);
#51654=ORIENTED_EDGE('',*,*,#36957,.F.);
#51655=ORIENTED_EDGE('',*,*,#36958,.T.);
#51656=ORIENTED_EDGE('',*,*,#36957,.T.);
#51657=ORIENTED_EDGE('',*,*,#36959,.F.);
#51658=ORIENTED_EDGE('',*,*,#36960,.F.);
#51659=ORIENTED_EDGE('',*,*,#36961,.T.);
#51660=ORIENTED_EDGE('',*,*,#36960,.T.);
#51661=ORIENTED_EDGE('',*,*,#36962,.F.);
#51662=ORIENTED_EDGE('',*,*,#36963,.F.);
#51663=ORIENTED_EDGE('',*,*,#36964,.T.);
#51664=ORIENTED_EDGE('',*,*,#36963,.T.);
#51665=ORIENTED_EDGE('',*,*,#36965,.F.);
#51666=ORIENTED_EDGE('',*,*,#36966,.F.);
#51667=ORIENTED_EDGE('',*,*,#36967,.T.);
#51668=ORIENTED_EDGE('',*,*,#36966,.T.);
#51669=ORIENTED_EDGE('',*,*,#36968,.F.);
#51670=ORIENTED_EDGE('',*,*,#36969,.F.);
#51671=ORIENTED_EDGE('',*,*,#36970,.T.);
#51672=ORIENTED_EDGE('',*,*,#36969,.T.);
#51673=ORIENTED_EDGE('',*,*,#36971,.F.);
#51674=ORIENTED_EDGE('',*,*,#36972,.F.);
#51675=ORIENTED_EDGE('',*,*,#36973,.T.);
#51676=ORIENTED_EDGE('',*,*,#36972,.T.);
#51677=ORIENTED_EDGE('',*,*,#36974,.F.);
#51678=ORIENTED_EDGE('',*,*,#36975,.F.);
#51679=ORIENTED_EDGE('',*,*,#36976,.T.);
#51680=ORIENTED_EDGE('',*,*,#36975,.T.);
#51681=ORIENTED_EDGE('',*,*,#36977,.F.);
#51682=ORIENTED_EDGE('',*,*,#36978,.F.);
#51683=ORIENTED_EDGE('',*,*,#36979,.T.);
#51684=ORIENTED_EDGE('',*,*,#36978,.T.);
#51685=ORIENTED_EDGE('',*,*,#36980,.F.);
#51686=ORIENTED_EDGE('',*,*,#36981,.F.);
#51687=ORIENTED_EDGE('',*,*,#36982,.T.);
#51688=ORIENTED_EDGE('',*,*,#36981,.T.);
#51689=ORIENTED_EDGE('',*,*,#36983,.F.);
#51690=ORIENTED_EDGE('',*,*,#36984,.F.);
#51691=ORIENTED_EDGE('',*,*,#36985,.T.);
#51692=ORIENTED_EDGE('',*,*,#36984,.T.);
#51693=ORIENTED_EDGE('',*,*,#36986,.F.);
#51694=ORIENTED_EDGE('',*,*,#36987,.F.);
#51695=ORIENTED_EDGE('',*,*,#36988,.T.);
#51696=ORIENTED_EDGE('',*,*,#36987,.T.);
#51697=ORIENTED_EDGE('',*,*,#36989,.F.);
#51698=ORIENTED_EDGE('',*,*,#36990,.F.);
#51699=ORIENTED_EDGE('',*,*,#36991,.T.);
#51700=ORIENTED_EDGE('',*,*,#36990,.T.);
#51701=ORIENTED_EDGE('',*,*,#36992,.F.);
#51702=ORIENTED_EDGE('',*,*,#36993,.F.);
#51703=ORIENTED_EDGE('',*,*,#36994,.T.);
#51704=ORIENTED_EDGE('',*,*,#36993,.T.);
#51705=ORIENTED_EDGE('',*,*,#36995,.F.);
#51706=ORIENTED_EDGE('',*,*,#36996,.F.);
#51707=ORIENTED_EDGE('',*,*,#36997,.T.);
#51708=ORIENTED_EDGE('',*,*,#36996,.T.);
#51709=ORIENTED_EDGE('',*,*,#36998,.F.);
#51710=ORIENTED_EDGE('',*,*,#36999,.F.);
#51711=ORIENTED_EDGE('',*,*,#37000,.T.);
#51712=ORIENTED_EDGE('',*,*,#36999,.T.);
#51713=ORIENTED_EDGE('',*,*,#37001,.F.);
#51714=ORIENTED_EDGE('',*,*,#37002,.F.);
#51715=ORIENTED_EDGE('',*,*,#37003,.T.);
#51716=ORIENTED_EDGE('',*,*,#37002,.T.);
#51717=ORIENTED_EDGE('',*,*,#37004,.F.);
#51718=ORIENTED_EDGE('',*,*,#37005,.F.);
#51719=ORIENTED_EDGE('',*,*,#37006,.T.);
#51720=ORIENTED_EDGE('',*,*,#37005,.T.);
#51721=ORIENTED_EDGE('',*,*,#37007,.F.);
#51722=ORIENTED_EDGE('',*,*,#37008,.F.);
#51723=ORIENTED_EDGE('',*,*,#37009,.T.);
#51724=ORIENTED_EDGE('',*,*,#37008,.T.);
#51725=ORIENTED_EDGE('',*,*,#37010,.F.);
#51726=ORIENTED_EDGE('',*,*,#37011,.F.);
#51727=ORIENTED_EDGE('',*,*,#37012,.T.);
#51728=ORIENTED_EDGE('',*,*,#37011,.T.);
#51729=ORIENTED_EDGE('',*,*,#37013,.F.);
#51730=ORIENTED_EDGE('',*,*,#37014,.F.);
#51731=ORIENTED_EDGE('',*,*,#37015,.T.);
#51732=ORIENTED_EDGE('',*,*,#37014,.T.);
#51733=ORIENTED_EDGE('',*,*,#37016,.F.);
#51734=ORIENTED_EDGE('',*,*,#37017,.F.);
#51735=ORIENTED_EDGE('',*,*,#37018,.T.);
#51736=ORIENTED_EDGE('',*,*,#37017,.T.);
#51737=ORIENTED_EDGE('',*,*,#37019,.F.);
#51738=ORIENTED_EDGE('',*,*,#37020,.F.);
#51739=ORIENTED_EDGE('',*,*,#37021,.T.);
#51740=ORIENTED_EDGE('',*,*,#37020,.T.);
#51741=ORIENTED_EDGE('',*,*,#37022,.F.);
#51742=ORIENTED_EDGE('',*,*,#37023,.F.);
#51743=ORIENTED_EDGE('',*,*,#37024,.T.);
#51744=ORIENTED_EDGE('',*,*,#37023,.T.);
#51745=ORIENTED_EDGE('',*,*,#37025,.F.);
#51746=ORIENTED_EDGE('',*,*,#37026,.F.);
#51747=ORIENTED_EDGE('',*,*,#37027,.T.);
#51748=ORIENTED_EDGE('',*,*,#37026,.T.);
#51749=ORIENTED_EDGE('',*,*,#37028,.F.);
#51750=ORIENTED_EDGE('',*,*,#37029,.F.);
#51751=ORIENTED_EDGE('',*,*,#37030,.T.);
#51752=ORIENTED_EDGE('',*,*,#37029,.T.);
#51753=ORIENTED_EDGE('',*,*,#37031,.F.);
#51754=ORIENTED_EDGE('',*,*,#37032,.F.);
#51755=ORIENTED_EDGE('',*,*,#37033,.T.);
#51756=ORIENTED_EDGE('',*,*,#37032,.T.);
#51757=ORIENTED_EDGE('',*,*,#37034,.F.);
#51758=ORIENTED_EDGE('',*,*,#37035,.F.);
#51759=ORIENTED_EDGE('',*,*,#37036,.T.);
#51760=ORIENTED_EDGE('',*,*,#37035,.T.);
#51761=ORIENTED_EDGE('',*,*,#37037,.F.);
#51762=ORIENTED_EDGE('',*,*,#37038,.F.);
#51763=ORIENTED_EDGE('',*,*,#37039,.T.);
#51764=ORIENTED_EDGE('',*,*,#37038,.T.);
#51765=ORIENTED_EDGE('',*,*,#37040,.F.);
#51766=ORIENTED_EDGE('',*,*,#37041,.F.);
#51767=ORIENTED_EDGE('',*,*,#37042,.T.);
#51768=ORIENTED_EDGE('',*,*,#37041,.T.);
#51769=ORIENTED_EDGE('',*,*,#37043,.F.);
#51770=ORIENTED_EDGE('',*,*,#37044,.F.);
#51771=ORIENTED_EDGE('',*,*,#37045,.T.);
#51772=ORIENTED_EDGE('',*,*,#37044,.T.);
#51773=ORIENTED_EDGE('',*,*,#37046,.F.);
#51774=ORIENTED_EDGE('',*,*,#37047,.F.);
#51775=ORIENTED_EDGE('',*,*,#37048,.T.);
#51776=ORIENTED_EDGE('',*,*,#37047,.T.);
#51777=ORIENTED_EDGE('',*,*,#37049,.F.);
#51778=ORIENTED_EDGE('',*,*,#37050,.F.);
#51779=ORIENTED_EDGE('',*,*,#37051,.T.);
#51780=ORIENTED_EDGE('',*,*,#37050,.T.);
#51781=ORIENTED_EDGE('',*,*,#37052,.F.);
#51782=ORIENTED_EDGE('',*,*,#37053,.F.);
#51783=ORIENTED_EDGE('',*,*,#37054,.T.);
#51784=ORIENTED_EDGE('',*,*,#37053,.T.);
#51785=ORIENTED_EDGE('',*,*,#37055,.F.);
#51786=ORIENTED_EDGE('',*,*,#37056,.F.);
#51787=ORIENTED_EDGE('',*,*,#37057,.T.);
#51788=ORIENTED_EDGE('',*,*,#37056,.T.);
#51789=ORIENTED_EDGE('',*,*,#37058,.F.);
#51790=ORIENTED_EDGE('',*,*,#37059,.F.);
#51791=ORIENTED_EDGE('',*,*,#37060,.T.);
#51792=ORIENTED_EDGE('',*,*,#37059,.T.);
#51793=ORIENTED_EDGE('',*,*,#37061,.F.);
#51794=ORIENTED_EDGE('',*,*,#37062,.F.);
#51795=ORIENTED_EDGE('',*,*,#37063,.T.);
#51796=ORIENTED_EDGE('',*,*,#37062,.T.);
#51797=ORIENTED_EDGE('',*,*,#37064,.F.);
#51798=ORIENTED_EDGE('',*,*,#37065,.F.);
#51799=ORIENTED_EDGE('',*,*,#37066,.T.);
#51800=ORIENTED_EDGE('',*,*,#37065,.T.);
#51801=ORIENTED_EDGE('',*,*,#37067,.F.);
#51802=ORIENTED_EDGE('',*,*,#37068,.F.);
#51803=ORIENTED_EDGE('',*,*,#37069,.T.);
#51804=ORIENTED_EDGE('',*,*,#37068,.T.);
#51805=ORIENTED_EDGE('',*,*,#37070,.F.);
#51806=ORIENTED_EDGE('',*,*,#37071,.F.);
#51807=ORIENTED_EDGE('',*,*,#37072,.T.);
#51808=ORIENTED_EDGE('',*,*,#37071,.T.);
#51809=ORIENTED_EDGE('',*,*,#37073,.F.);
#51810=ORIENTED_EDGE('',*,*,#37074,.F.);
#51811=ORIENTED_EDGE('',*,*,#37075,.T.);
#51812=ORIENTED_EDGE('',*,*,#37074,.T.);
#51813=ORIENTED_EDGE('',*,*,#37076,.F.);
#51814=ORIENTED_EDGE('',*,*,#37077,.F.);
#51815=ORIENTED_EDGE('',*,*,#37078,.T.);
#51816=ORIENTED_EDGE('',*,*,#37077,.T.);
#51817=ORIENTED_EDGE('',*,*,#37079,.F.);
#51818=ORIENTED_EDGE('',*,*,#37080,.F.);
#51819=ORIENTED_EDGE('',*,*,#37081,.T.);
#51820=ORIENTED_EDGE('',*,*,#37080,.T.);
#51821=ORIENTED_EDGE('',*,*,#37082,.F.);
#51822=ORIENTED_EDGE('',*,*,#37083,.F.);
#51823=ORIENTED_EDGE('',*,*,#37084,.T.);
#51824=ORIENTED_EDGE('',*,*,#37083,.T.);
#51825=ORIENTED_EDGE('',*,*,#37085,.F.);
#51826=ORIENTED_EDGE('',*,*,#37086,.F.);
#51827=ORIENTED_EDGE('',*,*,#37087,.T.);
#51828=ORIENTED_EDGE('',*,*,#37086,.T.);
#51829=ORIENTED_EDGE('',*,*,#37088,.F.);
#51830=ORIENTED_EDGE('',*,*,#37089,.F.);
#51831=ORIENTED_EDGE('',*,*,#37090,.T.);
#51832=ORIENTED_EDGE('',*,*,#37089,.T.);
#51833=ORIENTED_EDGE('',*,*,#37091,.F.);
#51834=ORIENTED_EDGE('',*,*,#37092,.F.);
#51835=ORIENTED_EDGE('',*,*,#37093,.T.);
#51836=ORIENTED_EDGE('',*,*,#37092,.T.);
#51837=ORIENTED_EDGE('',*,*,#37094,.F.);
#51838=ORIENTED_EDGE('',*,*,#37095,.F.);
#51839=ORIENTED_EDGE('',*,*,#37096,.T.);
#51840=ORIENTED_EDGE('',*,*,#37095,.T.);
#51841=ORIENTED_EDGE('',*,*,#37097,.F.);
#51842=ORIENTED_EDGE('',*,*,#37098,.F.);
#51843=ORIENTED_EDGE('',*,*,#37099,.T.);
#51844=ORIENTED_EDGE('',*,*,#37098,.T.);
#51845=ORIENTED_EDGE('',*,*,#37100,.F.);
#51846=ORIENTED_EDGE('',*,*,#37101,.F.);
#51847=ORIENTED_EDGE('',*,*,#37102,.T.);
#51848=ORIENTED_EDGE('',*,*,#37101,.T.);
#51849=ORIENTED_EDGE('',*,*,#37103,.F.);
#51850=ORIENTED_EDGE('',*,*,#37104,.F.);
#51851=ORIENTED_EDGE('',*,*,#37105,.T.);
#51852=ORIENTED_EDGE('',*,*,#37104,.T.);
#51853=ORIENTED_EDGE('',*,*,#37106,.F.);
#51854=ORIENTED_EDGE('',*,*,#37107,.F.);
#51855=ORIENTED_EDGE('',*,*,#37108,.T.);
#51856=ORIENTED_EDGE('',*,*,#37107,.T.);
#51857=ORIENTED_EDGE('',*,*,#37109,.F.);
#51858=ORIENTED_EDGE('',*,*,#37110,.F.);
#51859=ORIENTED_EDGE('',*,*,#37111,.T.);
#51860=ORIENTED_EDGE('',*,*,#37110,.T.);
#51861=ORIENTED_EDGE('',*,*,#37112,.F.);
#51862=ORIENTED_EDGE('',*,*,#37113,.F.);
#51863=ORIENTED_EDGE('',*,*,#37114,.T.);
#51864=ORIENTED_EDGE('',*,*,#37113,.T.);
#51865=ORIENTED_EDGE('',*,*,#37115,.F.);
#51866=ORIENTED_EDGE('',*,*,#37116,.F.);
#51867=ORIENTED_EDGE('',*,*,#37117,.T.);
#51868=ORIENTED_EDGE('',*,*,#37116,.T.);
#51869=ORIENTED_EDGE('',*,*,#37118,.F.);
#51870=ORIENTED_EDGE('',*,*,#37119,.F.);
#51871=ORIENTED_EDGE('',*,*,#37120,.T.);
#51872=ORIENTED_EDGE('',*,*,#37119,.T.);
#51873=ORIENTED_EDGE('',*,*,#37121,.F.);
#51874=ORIENTED_EDGE('',*,*,#37122,.F.);
#51875=ORIENTED_EDGE('',*,*,#37123,.T.);
#51876=ORIENTED_EDGE('',*,*,#37122,.T.);
#51877=ORIENTED_EDGE('',*,*,#37124,.F.);
#51878=ORIENTED_EDGE('',*,*,#37125,.F.);
#51879=ORIENTED_EDGE('',*,*,#37126,.T.);
#51880=ORIENTED_EDGE('',*,*,#37125,.T.);
#51881=ORIENTED_EDGE('',*,*,#37127,.F.);
#51882=ORIENTED_EDGE('',*,*,#37128,.F.);
#51883=ORIENTED_EDGE('',*,*,#37129,.T.);
#51884=ORIENTED_EDGE('',*,*,#37128,.T.);
#51885=ORIENTED_EDGE('',*,*,#37130,.F.);
#51886=ORIENTED_EDGE('',*,*,#37131,.F.);
#51887=ORIENTED_EDGE('',*,*,#37132,.T.);
#51888=ORIENTED_EDGE('',*,*,#37131,.T.);
#51889=ORIENTED_EDGE('',*,*,#37133,.F.);
#51890=ORIENTED_EDGE('',*,*,#37134,.F.);
#51891=ORIENTED_EDGE('',*,*,#37135,.T.);
#51892=ORIENTED_EDGE('',*,*,#37134,.T.);
#51893=ORIENTED_EDGE('',*,*,#37136,.F.);
#51894=ORIENTED_EDGE('',*,*,#37137,.F.);
#51895=ORIENTED_EDGE('',*,*,#37138,.T.);
#51896=ORIENTED_EDGE('',*,*,#37137,.T.);
#51897=ORIENTED_EDGE('',*,*,#37139,.F.);
#51898=ORIENTED_EDGE('',*,*,#37140,.F.);
#51899=ORIENTED_EDGE('',*,*,#37141,.T.);
#51900=ORIENTED_EDGE('',*,*,#37140,.T.);
#51901=ORIENTED_EDGE('',*,*,#37142,.F.);
#51902=ORIENTED_EDGE('',*,*,#37143,.F.);
#51903=ORIENTED_EDGE('',*,*,#37144,.T.);
#51904=ORIENTED_EDGE('',*,*,#37143,.T.);
#51905=ORIENTED_EDGE('',*,*,#37145,.F.);
#51906=ORIENTED_EDGE('',*,*,#37146,.F.);
#51907=ORIENTED_EDGE('',*,*,#37147,.T.);
#51908=ORIENTED_EDGE('',*,*,#37146,.T.);
#51909=ORIENTED_EDGE('',*,*,#37148,.F.);
#51910=ORIENTED_EDGE('',*,*,#37149,.F.);
#51911=ORIENTED_EDGE('',*,*,#37150,.T.);
#51912=ORIENTED_EDGE('',*,*,#37149,.T.);
#51913=ORIENTED_EDGE('',*,*,#37151,.F.);
#51914=ORIENTED_EDGE('',*,*,#37152,.F.);
#51915=ORIENTED_EDGE('',*,*,#37153,.T.);
#51916=ORIENTED_EDGE('',*,*,#37152,.T.);
#51917=ORIENTED_EDGE('',*,*,#37154,.F.);
#51918=ORIENTED_EDGE('',*,*,#37155,.F.);
#51919=ORIENTED_EDGE('',*,*,#37156,.T.);
#51920=ORIENTED_EDGE('',*,*,#37155,.T.);
#51921=ORIENTED_EDGE('',*,*,#37157,.F.);
#51922=ORIENTED_EDGE('',*,*,#37158,.F.);
#51923=ORIENTED_EDGE('',*,*,#37159,.T.);
#51924=ORIENTED_EDGE('',*,*,#37158,.T.);
#51925=ORIENTED_EDGE('',*,*,#37160,.F.);
#51926=ORIENTED_EDGE('',*,*,#37161,.F.);
#51927=ORIENTED_EDGE('',*,*,#37162,.T.);
#51928=ORIENTED_EDGE('',*,*,#37161,.T.);
#51929=ORIENTED_EDGE('',*,*,#37163,.F.);
#51930=ORIENTED_EDGE('',*,*,#37164,.F.);
#51931=ORIENTED_EDGE('',*,*,#37165,.T.);
#51932=ORIENTED_EDGE('',*,*,#37164,.T.);
#51933=ORIENTED_EDGE('',*,*,#37166,.F.);
#51934=ORIENTED_EDGE('',*,*,#37167,.F.);
#51935=ORIENTED_EDGE('',*,*,#37168,.T.);
#51936=ORIENTED_EDGE('',*,*,#37167,.T.);
#51937=ORIENTED_EDGE('',*,*,#37169,.F.);
#51938=ORIENTED_EDGE('',*,*,#37170,.F.);
#51939=ORIENTED_EDGE('',*,*,#37171,.T.);
#51940=ORIENTED_EDGE('',*,*,#37170,.T.);
#51941=ORIENTED_EDGE('',*,*,#37172,.F.);
#51942=ORIENTED_EDGE('',*,*,#37173,.F.);
#51943=ORIENTED_EDGE('',*,*,#37174,.T.);
#51944=ORIENTED_EDGE('',*,*,#37173,.T.);
#51945=ORIENTED_EDGE('',*,*,#37175,.F.);
#51946=ORIENTED_EDGE('',*,*,#37176,.F.);
#51947=ORIENTED_EDGE('',*,*,#37177,.T.);
#51948=ORIENTED_EDGE('',*,*,#37176,.T.);
#51949=ORIENTED_EDGE('',*,*,#37178,.F.);
#51950=ORIENTED_EDGE('',*,*,#37179,.F.);
#51951=ORIENTED_EDGE('',*,*,#37180,.T.);
#51952=ORIENTED_EDGE('',*,*,#37179,.T.);
#51953=ORIENTED_EDGE('',*,*,#37181,.F.);
#51954=ORIENTED_EDGE('',*,*,#37182,.F.);
#51955=ORIENTED_EDGE('',*,*,#37183,.T.);
#51956=ORIENTED_EDGE('',*,*,#37182,.T.);
#51957=ORIENTED_EDGE('',*,*,#37184,.F.);
#51958=ORIENTED_EDGE('',*,*,#37185,.F.);
#51959=ORIENTED_EDGE('',*,*,#37186,.T.);
#51960=ORIENTED_EDGE('',*,*,#37185,.T.);
#51961=ORIENTED_EDGE('',*,*,#37187,.F.);
#51962=ORIENTED_EDGE('',*,*,#37188,.F.);
#51963=ORIENTED_EDGE('',*,*,#37189,.T.);
#51964=ORIENTED_EDGE('',*,*,#37188,.T.);
#51965=ORIENTED_EDGE('',*,*,#37190,.F.);
#51966=ORIENTED_EDGE('',*,*,#37191,.F.);
#51967=ORIENTED_EDGE('',*,*,#37192,.T.);
#51968=ORIENTED_EDGE('',*,*,#37191,.T.);
#51969=ORIENTED_EDGE('',*,*,#37193,.F.);
#51970=ORIENTED_EDGE('',*,*,#37194,.F.);
#51971=ORIENTED_EDGE('',*,*,#37195,.T.);
#51972=ORIENTED_EDGE('',*,*,#37194,.T.);
#51973=ORIENTED_EDGE('',*,*,#37196,.F.);
#51974=ORIENTED_EDGE('',*,*,#37197,.F.);
#51975=ORIENTED_EDGE('',*,*,#37198,.T.);
#51976=ORIENTED_EDGE('',*,*,#37197,.T.);
#51977=ORIENTED_EDGE('',*,*,#37199,.F.);
#51978=ORIENTED_EDGE('',*,*,#37200,.F.);
#51979=ORIENTED_EDGE('',*,*,#37201,.T.);
#51980=ORIENTED_EDGE('',*,*,#37200,.T.);
#51981=ORIENTED_EDGE('',*,*,#37202,.F.);
#51982=ORIENTED_EDGE('',*,*,#37203,.F.);
#51983=ORIENTED_EDGE('',*,*,#37204,.T.);
#51984=ORIENTED_EDGE('',*,*,#37203,.T.);
#51985=ORIENTED_EDGE('',*,*,#37205,.F.);
#51986=ORIENTED_EDGE('',*,*,#37206,.F.);
#51987=ORIENTED_EDGE('',*,*,#37207,.T.);
#51988=ORIENTED_EDGE('',*,*,#37206,.T.);
#51989=ORIENTED_EDGE('',*,*,#37208,.F.);
#51990=ORIENTED_EDGE('',*,*,#37209,.F.);
#51991=ORIENTED_EDGE('',*,*,#37210,.T.);
#51992=ORIENTED_EDGE('',*,*,#37209,.T.);
#51993=ORIENTED_EDGE('',*,*,#37211,.F.);
#51994=ORIENTED_EDGE('',*,*,#37212,.F.);
#51995=ORIENTED_EDGE('',*,*,#37213,.T.);
#51996=ORIENTED_EDGE('',*,*,#37212,.T.);
#51997=ORIENTED_EDGE('',*,*,#37214,.F.);
#51998=ORIENTED_EDGE('',*,*,#37215,.F.);
#51999=ORIENTED_EDGE('',*,*,#37216,.T.);
#52000=ORIENTED_EDGE('',*,*,#37215,.T.);
#52001=ORIENTED_EDGE('',*,*,#37217,.F.);
#52002=ORIENTED_EDGE('',*,*,#37218,.F.);
#52003=ORIENTED_EDGE('',*,*,#37219,.T.);
#52004=ORIENTED_EDGE('',*,*,#37218,.T.);
#52005=ORIENTED_EDGE('',*,*,#37220,.F.);
#52006=ORIENTED_EDGE('',*,*,#37221,.F.);
#52007=ORIENTED_EDGE('',*,*,#37222,.T.);
#52008=ORIENTED_EDGE('',*,*,#37221,.T.);
#52009=ORIENTED_EDGE('',*,*,#37223,.F.);
#52010=ORIENTED_EDGE('',*,*,#37224,.F.);
#52011=ORIENTED_EDGE('',*,*,#37225,.T.);
#52012=ORIENTED_EDGE('',*,*,#37224,.T.);
#52013=ORIENTED_EDGE('',*,*,#37226,.F.);
#52014=ORIENTED_EDGE('',*,*,#37227,.F.);
#52015=ORIENTED_EDGE('',*,*,#37228,.T.);
#52016=ORIENTED_EDGE('',*,*,#37227,.T.);
#52017=ORIENTED_EDGE('',*,*,#37229,.F.);
#52018=ORIENTED_EDGE('',*,*,#37230,.F.);
#52019=ORIENTED_EDGE('',*,*,#37231,.T.);
#52020=ORIENTED_EDGE('',*,*,#37230,.T.);
#52021=ORIENTED_EDGE('',*,*,#37232,.F.);
#52022=ORIENTED_EDGE('',*,*,#37233,.F.);
#52023=ORIENTED_EDGE('',*,*,#37234,.T.);
#52024=ORIENTED_EDGE('',*,*,#37233,.T.);
#52025=ORIENTED_EDGE('',*,*,#37235,.F.);
#52026=ORIENTED_EDGE('',*,*,#37236,.F.);
#52027=ORIENTED_EDGE('',*,*,#37237,.T.);
#52028=ORIENTED_EDGE('',*,*,#37236,.T.);
#52029=ORIENTED_EDGE('',*,*,#37238,.F.);
#52030=ORIENTED_EDGE('',*,*,#37239,.F.);
#52031=ORIENTED_EDGE('',*,*,#37240,.T.);
#52032=ORIENTED_EDGE('',*,*,#37239,.T.);
#52033=ORIENTED_EDGE('',*,*,#37241,.F.);
#52034=ORIENTED_EDGE('',*,*,#37242,.F.);
#52035=ORIENTED_EDGE('',*,*,#37243,.T.);
#52036=ORIENTED_EDGE('',*,*,#37242,.T.);
#52037=ORIENTED_EDGE('',*,*,#37244,.F.);
#52038=ORIENTED_EDGE('',*,*,#37245,.F.);
#52039=ORIENTED_EDGE('',*,*,#37246,.T.);
#52040=ORIENTED_EDGE('',*,*,#37245,.T.);
#52041=ORIENTED_EDGE('',*,*,#37247,.F.);
#52042=ORIENTED_EDGE('',*,*,#37248,.F.);
#52043=ORIENTED_EDGE('',*,*,#37249,.T.);
#52044=ORIENTED_EDGE('',*,*,#37248,.T.);
#52045=ORIENTED_EDGE('',*,*,#37250,.F.);
#52046=ORIENTED_EDGE('',*,*,#37251,.F.);
#52047=ORIENTED_EDGE('',*,*,#37252,.T.);
#52048=ORIENTED_EDGE('',*,*,#37251,.T.);
#52049=ORIENTED_EDGE('',*,*,#37253,.F.);
#52050=ORIENTED_EDGE('',*,*,#37254,.F.);
#52051=ORIENTED_EDGE('',*,*,#37255,.T.);
#52052=ORIENTED_EDGE('',*,*,#37254,.T.);
#52053=ORIENTED_EDGE('',*,*,#37256,.F.);
#52054=ORIENTED_EDGE('',*,*,#37257,.F.);
#52055=ORIENTED_EDGE('',*,*,#37258,.T.);
#52056=ORIENTED_EDGE('',*,*,#37257,.T.);
#52057=ORIENTED_EDGE('',*,*,#37259,.F.);
#52058=ORIENTED_EDGE('',*,*,#37260,.F.);
#52059=ORIENTED_EDGE('',*,*,#37261,.T.);
#52060=ORIENTED_EDGE('',*,*,#37260,.T.);
#52061=ORIENTED_EDGE('',*,*,#37262,.F.);
#52062=ORIENTED_EDGE('',*,*,#37263,.F.);
#52063=ORIENTED_EDGE('',*,*,#37264,.T.);
#52064=ORIENTED_EDGE('',*,*,#37263,.T.);
#52065=ORIENTED_EDGE('',*,*,#37265,.F.);
#52066=ORIENTED_EDGE('',*,*,#37266,.F.);
#52067=ORIENTED_EDGE('',*,*,#37267,.T.);
#52068=ORIENTED_EDGE('',*,*,#37266,.T.);
#52069=ORIENTED_EDGE('',*,*,#37268,.F.);
#52070=ORIENTED_EDGE('',*,*,#37269,.F.);
#52071=ORIENTED_EDGE('',*,*,#37270,.T.);
#52072=ORIENTED_EDGE('',*,*,#37269,.T.);
#52073=ORIENTED_EDGE('',*,*,#37271,.F.);
#52074=ORIENTED_EDGE('',*,*,#37272,.F.);
#52075=ORIENTED_EDGE('',*,*,#37273,.T.);
#52076=ORIENTED_EDGE('',*,*,#37272,.T.);
#52077=ORIENTED_EDGE('',*,*,#37274,.F.);
#52078=ORIENTED_EDGE('',*,*,#37275,.F.);
#52079=ORIENTED_EDGE('',*,*,#37276,.T.);
#52080=ORIENTED_EDGE('',*,*,#37275,.T.);
#52081=ORIENTED_EDGE('',*,*,#37277,.F.);
#52082=ORIENTED_EDGE('',*,*,#37278,.F.);
#52083=ORIENTED_EDGE('',*,*,#37279,.T.);
#52084=ORIENTED_EDGE('',*,*,#37278,.T.);
#52085=ORIENTED_EDGE('',*,*,#37280,.F.);
#52086=ORIENTED_EDGE('',*,*,#37281,.F.);
#52087=ORIENTED_EDGE('',*,*,#37282,.T.);
#52088=ORIENTED_EDGE('',*,*,#37281,.T.);
#52089=ORIENTED_EDGE('',*,*,#37283,.F.);
#52090=ORIENTED_EDGE('',*,*,#37284,.F.);
#52091=ORIENTED_EDGE('',*,*,#37285,.T.);
#52092=ORIENTED_EDGE('',*,*,#37284,.T.);
#52093=ORIENTED_EDGE('',*,*,#37286,.F.);
#52094=ORIENTED_EDGE('',*,*,#37287,.F.);
#52095=ORIENTED_EDGE('',*,*,#37288,.T.);
#52096=ORIENTED_EDGE('',*,*,#37287,.T.);
#52097=ORIENTED_EDGE('',*,*,#37289,.F.);
#52098=ORIENTED_EDGE('',*,*,#37290,.F.);
#52099=ORIENTED_EDGE('',*,*,#37291,.T.);
#52100=ORIENTED_EDGE('',*,*,#37290,.T.);
#52101=ORIENTED_EDGE('',*,*,#37292,.F.);
#52102=ORIENTED_EDGE('',*,*,#37293,.F.);
#52103=ORIENTED_EDGE('',*,*,#37294,.T.);
#52104=ORIENTED_EDGE('',*,*,#37293,.T.);
#52105=ORIENTED_EDGE('',*,*,#37295,.F.);
#52106=ORIENTED_EDGE('',*,*,#37296,.F.);
#52107=ORIENTED_EDGE('',*,*,#37297,.T.);
#52108=ORIENTED_EDGE('',*,*,#37296,.T.);
#52109=ORIENTED_EDGE('',*,*,#37298,.F.);
#52110=ORIENTED_EDGE('',*,*,#37299,.F.);
#52111=ORIENTED_EDGE('',*,*,#37300,.T.);
#52112=ORIENTED_EDGE('',*,*,#37299,.T.);
#52113=ORIENTED_EDGE('',*,*,#37301,.F.);
#52114=ORIENTED_EDGE('',*,*,#37302,.F.);
#52115=ORIENTED_EDGE('',*,*,#37303,.T.);
#52116=ORIENTED_EDGE('',*,*,#37302,.T.);
#52117=ORIENTED_EDGE('',*,*,#37304,.F.);
#52118=ORIENTED_EDGE('',*,*,#37305,.F.);
#52119=ORIENTED_EDGE('',*,*,#37306,.T.);
#52120=ORIENTED_EDGE('',*,*,#37305,.T.);
#52121=ORIENTED_EDGE('',*,*,#37307,.F.);
#52122=ORIENTED_EDGE('',*,*,#37308,.F.);
#52123=ORIENTED_EDGE('',*,*,#37309,.T.);
#52124=ORIENTED_EDGE('',*,*,#37308,.T.);
#52125=ORIENTED_EDGE('',*,*,#37310,.F.);
#52126=ORIENTED_EDGE('',*,*,#37311,.F.);
#52127=ORIENTED_EDGE('',*,*,#37312,.T.);
#52128=ORIENTED_EDGE('',*,*,#37311,.T.);
#52129=ORIENTED_EDGE('',*,*,#37313,.F.);
#52130=ORIENTED_EDGE('',*,*,#37314,.F.);
#52131=ORIENTED_EDGE('',*,*,#37315,.T.);
#52132=ORIENTED_EDGE('',*,*,#37314,.T.);
#52133=ORIENTED_EDGE('',*,*,#37316,.F.);
#52134=ORIENTED_EDGE('',*,*,#37317,.F.);
#52135=ORIENTED_EDGE('',*,*,#37318,.T.);
#52136=ORIENTED_EDGE('',*,*,#37317,.T.);
#52137=ORIENTED_EDGE('',*,*,#37319,.F.);
#52138=ORIENTED_EDGE('',*,*,#37320,.F.);
#52139=ORIENTED_EDGE('',*,*,#37321,.T.);
#52140=ORIENTED_EDGE('',*,*,#37320,.T.);
#52141=ORIENTED_EDGE('',*,*,#37322,.F.);
#52142=ORIENTED_EDGE('',*,*,#37323,.F.);
#52143=ORIENTED_EDGE('',*,*,#37324,.T.);
#52144=ORIENTED_EDGE('',*,*,#37323,.T.);
#52145=ORIENTED_EDGE('',*,*,#37325,.F.);
#52146=ORIENTED_EDGE('',*,*,#37326,.F.);
#52147=ORIENTED_EDGE('',*,*,#37327,.T.);
#52148=ORIENTED_EDGE('',*,*,#37326,.T.);
#52149=ORIENTED_EDGE('',*,*,#37328,.F.);
#52150=ORIENTED_EDGE('',*,*,#37329,.F.);
#52151=ORIENTED_EDGE('',*,*,#37330,.T.);
#52152=ORIENTED_EDGE('',*,*,#37329,.T.);
#52153=ORIENTED_EDGE('',*,*,#37331,.F.);
#52154=ORIENTED_EDGE('',*,*,#37332,.F.);
#52155=ORIENTED_EDGE('',*,*,#37333,.T.);
#52156=ORIENTED_EDGE('',*,*,#37332,.T.);
#52157=ORIENTED_EDGE('',*,*,#37334,.F.);
#52158=ORIENTED_EDGE('',*,*,#37335,.F.);
#52159=ORIENTED_EDGE('',*,*,#37336,.T.);
#52160=ORIENTED_EDGE('',*,*,#37335,.T.);
#52161=ORIENTED_EDGE('',*,*,#37337,.F.);
#52162=ORIENTED_EDGE('',*,*,#37338,.F.);
#52163=ORIENTED_EDGE('',*,*,#37339,.T.);
#52164=ORIENTED_EDGE('',*,*,#37338,.T.);
#52165=ORIENTED_EDGE('',*,*,#37340,.F.);
#52166=ORIENTED_EDGE('',*,*,#37341,.F.);
#52167=ORIENTED_EDGE('',*,*,#37342,.T.);
#52168=ORIENTED_EDGE('',*,*,#37341,.T.);
#52169=ORIENTED_EDGE('',*,*,#37343,.F.);
#52170=ORIENTED_EDGE('',*,*,#37344,.F.);
#52171=ORIENTED_EDGE('',*,*,#37345,.T.);
#52172=ORIENTED_EDGE('',*,*,#37344,.T.);
#52173=ORIENTED_EDGE('',*,*,#37346,.F.);
#52174=ORIENTED_EDGE('',*,*,#37347,.F.);
#52175=ORIENTED_EDGE('',*,*,#37348,.T.);
#52176=ORIENTED_EDGE('',*,*,#37347,.T.);
#52177=ORIENTED_EDGE('',*,*,#37349,.F.);
#52178=ORIENTED_EDGE('',*,*,#37350,.F.);
#52179=ORIENTED_EDGE('',*,*,#37351,.T.);
#52180=ORIENTED_EDGE('',*,*,#37350,.T.);
#52181=ORIENTED_EDGE('',*,*,#37352,.F.);
#52182=ORIENTED_EDGE('',*,*,#37353,.F.);
#52183=ORIENTED_EDGE('',*,*,#37354,.T.);
#52184=ORIENTED_EDGE('',*,*,#37353,.T.);
#52185=ORIENTED_EDGE('',*,*,#37355,.F.);
#52186=ORIENTED_EDGE('',*,*,#37356,.F.);
#52187=ORIENTED_EDGE('',*,*,#37357,.T.);
#52188=ORIENTED_EDGE('',*,*,#37356,.T.);
#52189=ORIENTED_EDGE('',*,*,#37358,.F.);
#52190=ORIENTED_EDGE('',*,*,#37359,.F.);
#52191=ORIENTED_EDGE('',*,*,#37360,.T.);
#52192=ORIENTED_EDGE('',*,*,#37359,.T.);
#52193=ORIENTED_EDGE('',*,*,#37361,.F.);
#52194=ORIENTED_EDGE('',*,*,#37362,.F.);
#52195=ORIENTED_EDGE('',*,*,#37363,.T.);
#52196=ORIENTED_EDGE('',*,*,#37362,.T.);
#52197=ORIENTED_EDGE('',*,*,#37364,.F.);
#52198=ORIENTED_EDGE('',*,*,#37365,.F.);
#52199=ORIENTED_EDGE('',*,*,#37366,.T.);
#52200=ORIENTED_EDGE('',*,*,#37365,.T.);
#52201=ORIENTED_EDGE('',*,*,#37367,.F.);
#52202=ORIENTED_EDGE('',*,*,#37368,.F.);
#52203=ORIENTED_EDGE('',*,*,#37369,.T.);
#52204=ORIENTED_EDGE('',*,*,#37368,.T.);
#52205=ORIENTED_EDGE('',*,*,#37370,.F.);
#52206=ORIENTED_EDGE('',*,*,#37371,.F.);
#52207=ORIENTED_EDGE('',*,*,#37372,.T.);
#52208=ORIENTED_EDGE('',*,*,#37371,.T.);
#52209=ORIENTED_EDGE('',*,*,#37373,.F.);
#52210=ORIENTED_EDGE('',*,*,#37374,.F.);
#52211=ORIENTED_EDGE('',*,*,#37375,.T.);
#52212=ORIENTED_EDGE('',*,*,#37374,.T.);
#52213=ORIENTED_EDGE('',*,*,#37376,.F.);
#52214=ORIENTED_EDGE('',*,*,#37377,.F.);
#52215=ORIENTED_EDGE('',*,*,#37378,.T.);
#52216=ORIENTED_EDGE('',*,*,#37377,.T.);
#52217=ORIENTED_EDGE('',*,*,#37379,.F.);
#52218=ORIENTED_EDGE('',*,*,#37380,.F.);
#52219=ORIENTED_EDGE('',*,*,#37381,.T.);
#52220=ORIENTED_EDGE('',*,*,#37380,.T.);
#52221=ORIENTED_EDGE('',*,*,#37382,.F.);
#52222=ORIENTED_EDGE('',*,*,#37383,.F.);
#52223=ORIENTED_EDGE('',*,*,#37384,.T.);
#52224=ORIENTED_EDGE('',*,*,#37383,.T.);
#52225=ORIENTED_EDGE('',*,*,#37385,.F.);
#52226=ORIENTED_EDGE('',*,*,#37386,.F.);
#52227=ORIENTED_EDGE('',*,*,#37387,.T.);
#52228=ORIENTED_EDGE('',*,*,#37386,.T.);
#52229=ORIENTED_EDGE('',*,*,#37388,.F.);
#52230=ORIENTED_EDGE('',*,*,#37389,.F.);
#52231=ORIENTED_EDGE('',*,*,#37390,.T.);
#52232=ORIENTED_EDGE('',*,*,#37389,.T.);
#52233=ORIENTED_EDGE('',*,*,#37391,.F.);
#52234=ORIENTED_EDGE('',*,*,#37392,.F.);
#52235=ORIENTED_EDGE('',*,*,#37393,.T.);
#52236=ORIENTED_EDGE('',*,*,#37392,.T.);
#52237=ORIENTED_EDGE('',*,*,#37394,.F.);
#52238=ORIENTED_EDGE('',*,*,#37395,.F.);
#52239=ORIENTED_EDGE('',*,*,#37396,.T.);
#52240=ORIENTED_EDGE('',*,*,#37395,.T.);
#52241=ORIENTED_EDGE('',*,*,#37397,.F.);
#52242=ORIENTED_EDGE('',*,*,#37398,.F.);
#52243=ORIENTED_EDGE('',*,*,#37399,.T.);
#52244=ORIENTED_EDGE('',*,*,#37398,.T.);
#52245=ORIENTED_EDGE('',*,*,#37400,.F.);
#52246=ORIENTED_EDGE('',*,*,#37401,.F.);
#52247=ORIENTED_EDGE('',*,*,#37402,.T.);
#52248=ORIENTED_EDGE('',*,*,#37401,.T.);
#52249=ORIENTED_EDGE('',*,*,#37403,.F.);
#52250=ORIENTED_EDGE('',*,*,#37404,.F.);
#52251=ORIENTED_EDGE('',*,*,#37405,.T.);
#52252=ORIENTED_EDGE('',*,*,#37404,.T.);
#52253=ORIENTED_EDGE('',*,*,#37406,.F.);
#52254=ORIENTED_EDGE('',*,*,#37407,.F.);
#52255=ORIENTED_EDGE('',*,*,#37408,.T.);
#52256=ORIENTED_EDGE('',*,*,#37407,.T.);
#52257=ORIENTED_EDGE('',*,*,#37409,.F.);
#52258=ORIENTED_EDGE('',*,*,#37410,.F.);
#52259=ORIENTED_EDGE('',*,*,#37411,.T.);
#52260=ORIENTED_EDGE('',*,*,#37410,.T.);
#52261=ORIENTED_EDGE('',*,*,#37412,.F.);
#52262=ORIENTED_EDGE('',*,*,#37413,.F.);
#52263=ORIENTED_EDGE('',*,*,#37414,.T.);
#52264=ORIENTED_EDGE('',*,*,#37413,.T.);
#52265=ORIENTED_EDGE('',*,*,#37415,.F.);
#52266=ORIENTED_EDGE('',*,*,#37416,.F.);
#52267=ORIENTED_EDGE('',*,*,#37417,.T.);
#52268=ORIENTED_EDGE('',*,*,#37416,.T.);
#52269=ORIENTED_EDGE('',*,*,#37418,.F.);
#52270=ORIENTED_EDGE('',*,*,#37419,.F.);
#52271=ORIENTED_EDGE('',*,*,#37420,.T.);
#52272=ORIENTED_EDGE('',*,*,#37419,.T.);
#52273=ORIENTED_EDGE('',*,*,#37421,.F.);
#52274=ORIENTED_EDGE('',*,*,#37422,.F.);
#52275=ORIENTED_EDGE('',*,*,#37423,.T.);
#52276=ORIENTED_EDGE('',*,*,#37422,.T.);
#52277=ORIENTED_EDGE('',*,*,#37424,.F.);
#52278=ORIENTED_EDGE('',*,*,#37425,.F.);
#52279=ORIENTED_EDGE('',*,*,#37426,.T.);
#52280=ORIENTED_EDGE('',*,*,#37425,.T.);
#52281=ORIENTED_EDGE('',*,*,#37427,.F.);
#52282=ORIENTED_EDGE('',*,*,#37428,.F.);
#52283=ORIENTED_EDGE('',*,*,#37429,.T.);
#52284=ORIENTED_EDGE('',*,*,#37428,.T.);
#52285=ORIENTED_EDGE('',*,*,#37430,.F.);
#52286=ORIENTED_EDGE('',*,*,#37431,.F.);
#52287=ORIENTED_EDGE('',*,*,#37432,.T.);
#52288=ORIENTED_EDGE('',*,*,#37431,.T.);
#52289=ORIENTED_EDGE('',*,*,#37433,.F.);
#52290=ORIENTED_EDGE('',*,*,#37434,.F.);
#52291=ORIENTED_EDGE('',*,*,#37435,.T.);
#52292=ORIENTED_EDGE('',*,*,#37434,.T.);
#52293=ORIENTED_EDGE('',*,*,#37436,.F.);
#52294=ORIENTED_EDGE('',*,*,#37437,.F.);
#52295=ORIENTED_EDGE('',*,*,#37438,.T.);
#52296=ORIENTED_EDGE('',*,*,#37437,.T.);
#52297=ORIENTED_EDGE('',*,*,#37439,.F.);
#52298=ORIENTED_EDGE('',*,*,#37440,.F.);
#52299=ORIENTED_EDGE('',*,*,#37441,.T.);
#52300=ORIENTED_EDGE('',*,*,#37440,.T.);
#52301=ORIENTED_EDGE('',*,*,#37442,.F.);
#52302=ORIENTED_EDGE('',*,*,#37443,.F.);
#52303=ORIENTED_EDGE('',*,*,#37444,.T.);
#52304=ORIENTED_EDGE('',*,*,#37443,.T.);
#52305=ORIENTED_EDGE('',*,*,#37445,.F.);
#52306=ORIENTED_EDGE('',*,*,#37446,.F.);
#52307=ORIENTED_EDGE('',*,*,#37447,.T.);
#52308=ORIENTED_EDGE('',*,*,#37446,.T.);
#52309=ORIENTED_EDGE('',*,*,#37448,.F.);
#52310=ORIENTED_EDGE('',*,*,#37449,.F.);
#52311=ORIENTED_EDGE('',*,*,#37450,.T.);
#52312=ORIENTED_EDGE('',*,*,#37449,.T.);
#52313=ORIENTED_EDGE('',*,*,#37451,.F.);
#52314=ORIENTED_EDGE('',*,*,#37452,.F.);
#52315=ORIENTED_EDGE('',*,*,#37453,.T.);
#52316=ORIENTED_EDGE('',*,*,#37452,.T.);
#52317=ORIENTED_EDGE('',*,*,#37454,.F.);
#52318=ORIENTED_EDGE('',*,*,#37455,.F.);
#52319=ORIENTED_EDGE('',*,*,#37456,.T.);
#52320=ORIENTED_EDGE('',*,*,#37455,.T.);
#52321=ORIENTED_EDGE('',*,*,#37457,.F.);
#52322=ORIENTED_EDGE('',*,*,#37458,.F.);
#52323=ORIENTED_EDGE('',*,*,#37459,.T.);
#52324=ORIENTED_EDGE('',*,*,#37458,.T.);
#52325=ORIENTED_EDGE('',*,*,#37460,.F.);
#52326=ORIENTED_EDGE('',*,*,#37461,.F.);
#52327=ORIENTED_EDGE('',*,*,#37462,.T.);
#52328=ORIENTED_EDGE('',*,*,#37461,.T.);
#52329=ORIENTED_EDGE('',*,*,#37463,.F.);
#52330=ORIENTED_EDGE('',*,*,#37464,.F.);
#52331=ORIENTED_EDGE('',*,*,#37465,.T.);
#52332=ORIENTED_EDGE('',*,*,#37464,.T.);
#52333=ORIENTED_EDGE('',*,*,#37466,.F.);
#52334=ORIENTED_EDGE('',*,*,#37467,.F.);
#52335=ORIENTED_EDGE('',*,*,#37468,.T.);
#52336=ORIENTED_EDGE('',*,*,#37467,.T.);
#52337=ORIENTED_EDGE('',*,*,#37469,.F.);
#52338=ORIENTED_EDGE('',*,*,#37470,.F.);
#52339=ORIENTED_EDGE('',*,*,#37471,.T.);
#52340=ORIENTED_EDGE('',*,*,#37470,.T.);
#52341=ORIENTED_EDGE('',*,*,#37472,.F.);
#52342=ORIENTED_EDGE('',*,*,#37473,.F.);
#52343=ORIENTED_EDGE('',*,*,#37474,.T.);
#52344=ORIENTED_EDGE('',*,*,#37473,.T.);
#52345=ORIENTED_EDGE('',*,*,#37475,.F.);
#52346=ORIENTED_EDGE('',*,*,#37476,.F.);
#52347=ORIENTED_EDGE('',*,*,#37477,.T.);
#52348=ORIENTED_EDGE('',*,*,#37476,.T.);
#52349=ORIENTED_EDGE('',*,*,#37478,.F.);
#52350=ORIENTED_EDGE('',*,*,#37479,.F.);
#52351=ORIENTED_EDGE('',*,*,#37480,.T.);
#52352=ORIENTED_EDGE('',*,*,#37479,.T.);
#52353=ORIENTED_EDGE('',*,*,#37481,.F.);
#52354=ORIENTED_EDGE('',*,*,#37482,.F.);
#52355=ORIENTED_EDGE('',*,*,#37483,.T.);
#52356=ORIENTED_EDGE('',*,*,#37482,.T.);
#52357=ORIENTED_EDGE('',*,*,#37484,.F.);
#52358=ORIENTED_EDGE('',*,*,#37485,.F.);
#52359=ORIENTED_EDGE('',*,*,#37486,.T.);
#52360=ORIENTED_EDGE('',*,*,#37485,.T.);
#52361=ORIENTED_EDGE('',*,*,#37487,.F.);
#52362=ORIENTED_EDGE('',*,*,#37488,.F.);
#52363=ORIENTED_EDGE('',*,*,#37489,.T.);
#52364=ORIENTED_EDGE('',*,*,#37488,.T.);
#52365=ORIENTED_EDGE('',*,*,#37490,.F.);
#52366=ORIENTED_EDGE('',*,*,#37491,.F.);
#52367=ORIENTED_EDGE('',*,*,#37492,.T.);
#52368=ORIENTED_EDGE('',*,*,#37491,.T.);
#52369=ORIENTED_EDGE('',*,*,#37493,.F.);
#52370=ORIENTED_EDGE('',*,*,#37494,.F.);
#52371=ORIENTED_EDGE('',*,*,#37495,.T.);
#52372=ORIENTED_EDGE('',*,*,#37494,.T.);
#52373=ORIENTED_EDGE('',*,*,#37496,.F.);
#52374=ORIENTED_EDGE('',*,*,#37497,.F.);
#52375=ORIENTED_EDGE('',*,*,#37498,.T.);
#52376=ORIENTED_EDGE('',*,*,#37497,.T.);
#52377=ORIENTED_EDGE('',*,*,#37499,.F.);
#52378=ORIENTED_EDGE('',*,*,#37500,.F.);
#52379=ORIENTED_EDGE('',*,*,#37501,.T.);
#52380=ORIENTED_EDGE('',*,*,#37500,.T.);
#52381=ORIENTED_EDGE('',*,*,#37502,.F.);
#52382=ORIENTED_EDGE('',*,*,#37503,.F.);
#52383=ORIENTED_EDGE('',*,*,#37504,.T.);
#52384=ORIENTED_EDGE('',*,*,#37503,.T.);
#52385=ORIENTED_EDGE('',*,*,#37505,.F.);
#52386=ORIENTED_EDGE('',*,*,#37506,.F.);
#52387=ORIENTED_EDGE('',*,*,#37507,.T.);
#52388=ORIENTED_EDGE('',*,*,#37506,.T.);
#52389=ORIENTED_EDGE('',*,*,#37508,.F.);
#52390=ORIENTED_EDGE('',*,*,#37509,.F.);
#52391=ORIENTED_EDGE('',*,*,#37510,.T.);
#52392=ORIENTED_EDGE('',*,*,#37509,.T.);
#52393=ORIENTED_EDGE('',*,*,#37511,.F.);
#52394=ORIENTED_EDGE('',*,*,#37512,.F.);
#52395=ORIENTED_EDGE('',*,*,#37513,.T.);
#52396=ORIENTED_EDGE('',*,*,#37512,.T.);
#52397=ORIENTED_EDGE('',*,*,#37514,.F.);
#52398=ORIENTED_EDGE('',*,*,#37515,.F.);
#52399=ORIENTED_EDGE('',*,*,#37516,.T.);
#52400=ORIENTED_EDGE('',*,*,#37515,.T.);
#52401=ORIENTED_EDGE('',*,*,#37517,.F.);
#52402=ORIENTED_EDGE('',*,*,#37518,.F.);
#52403=ORIENTED_EDGE('',*,*,#37519,.T.);
#52404=ORIENTED_EDGE('',*,*,#37518,.T.);
#52405=ORIENTED_EDGE('',*,*,#37520,.F.);
#52406=ORIENTED_EDGE('',*,*,#37521,.F.);
#52407=ORIENTED_EDGE('',*,*,#37522,.T.);
#52408=ORIENTED_EDGE('',*,*,#37521,.T.);
#52409=ORIENTED_EDGE('',*,*,#37523,.F.);
#52410=ORIENTED_EDGE('',*,*,#37524,.F.);
#52411=ORIENTED_EDGE('',*,*,#37525,.T.);
#52412=ORIENTED_EDGE('',*,*,#37524,.T.);
#52413=ORIENTED_EDGE('',*,*,#37526,.F.);
#52414=ORIENTED_EDGE('',*,*,#37527,.F.);
#52415=ORIENTED_EDGE('',*,*,#37528,.T.);
#52416=ORIENTED_EDGE('',*,*,#37527,.T.);
#52417=ORIENTED_EDGE('',*,*,#37529,.F.);
#52418=ORIENTED_EDGE('',*,*,#37530,.F.);
#52419=ORIENTED_EDGE('',*,*,#37531,.T.);
#52420=ORIENTED_EDGE('',*,*,#37530,.T.);
#52421=ORIENTED_EDGE('',*,*,#37532,.F.);
#52422=ORIENTED_EDGE('',*,*,#37533,.F.);
#52423=ORIENTED_EDGE('',*,*,#37534,.T.);
#52424=ORIENTED_EDGE('',*,*,#37533,.T.);
#52425=ORIENTED_EDGE('',*,*,#37535,.F.);
#52426=ORIENTED_EDGE('',*,*,#37536,.F.);
#52427=ORIENTED_EDGE('',*,*,#37537,.T.);
#52428=ORIENTED_EDGE('',*,*,#37536,.T.);
#52429=ORIENTED_EDGE('',*,*,#37538,.F.);
#52430=ORIENTED_EDGE('',*,*,#37539,.F.);
#52431=ORIENTED_EDGE('',*,*,#37540,.T.);
#52432=ORIENTED_EDGE('',*,*,#37539,.T.);
#52433=ORIENTED_EDGE('',*,*,#37541,.F.);
#52434=ORIENTED_EDGE('',*,*,#37542,.F.);
#52435=ORIENTED_EDGE('',*,*,#37543,.T.);
#52436=ORIENTED_EDGE('',*,*,#37542,.T.);
#52437=ORIENTED_EDGE('',*,*,#37544,.F.);
#52438=ORIENTED_EDGE('',*,*,#37545,.F.);
#52439=ORIENTED_EDGE('',*,*,#37546,.T.);
#52440=ORIENTED_EDGE('',*,*,#37545,.T.);
#52441=ORIENTED_EDGE('',*,*,#37547,.F.);
#52442=ORIENTED_EDGE('',*,*,#37548,.F.);
#52443=ORIENTED_EDGE('',*,*,#37549,.T.);
#52444=ORIENTED_EDGE('',*,*,#37548,.T.);
#52445=ORIENTED_EDGE('',*,*,#37550,.F.);
#52446=ORIENTED_EDGE('',*,*,#37551,.F.);
#52447=ORIENTED_EDGE('',*,*,#37552,.T.);
#52448=ORIENTED_EDGE('',*,*,#37551,.T.);
#52449=ORIENTED_EDGE('',*,*,#37553,.F.);
#52450=ORIENTED_EDGE('',*,*,#37554,.F.);
#52451=ORIENTED_EDGE('',*,*,#37555,.T.);
#52452=ORIENTED_EDGE('',*,*,#37554,.T.);
#52453=ORIENTED_EDGE('',*,*,#37556,.F.);
#52454=ORIENTED_EDGE('',*,*,#37557,.F.);
#52455=ORIENTED_EDGE('',*,*,#37558,.T.);
#52456=ORIENTED_EDGE('',*,*,#37557,.T.);
#52457=ORIENTED_EDGE('',*,*,#37559,.F.);
#52458=ORIENTED_EDGE('',*,*,#37560,.F.);
#52459=ORIENTED_EDGE('',*,*,#37561,.T.);
#52460=ORIENTED_EDGE('',*,*,#37560,.T.);
#52461=ORIENTED_EDGE('',*,*,#37562,.F.);
#52462=ORIENTED_EDGE('',*,*,#37563,.F.);
#52463=ORIENTED_EDGE('',*,*,#37564,.T.);
#52464=ORIENTED_EDGE('',*,*,#37563,.T.);
#52465=ORIENTED_EDGE('',*,*,#37565,.F.);
#52466=ORIENTED_EDGE('',*,*,#37566,.F.);
#52467=ORIENTED_EDGE('',*,*,#37567,.T.);
#52468=ORIENTED_EDGE('',*,*,#37566,.T.);
#52469=ORIENTED_EDGE('',*,*,#37568,.F.);
#52470=ORIENTED_EDGE('',*,*,#37569,.F.);
#52471=ORIENTED_EDGE('',*,*,#37570,.T.);
#52472=ORIENTED_EDGE('',*,*,#37569,.T.);
#52473=ORIENTED_EDGE('',*,*,#37571,.F.);
#52474=ORIENTED_EDGE('',*,*,#37572,.F.);
#52475=ORIENTED_EDGE('',*,*,#37573,.T.);
#52476=ORIENTED_EDGE('',*,*,#37572,.T.);
#52477=ORIENTED_EDGE('',*,*,#37574,.F.);
#52478=ORIENTED_EDGE('',*,*,#37575,.F.);
#52479=ORIENTED_EDGE('',*,*,#37576,.T.);
#52480=ORIENTED_EDGE('',*,*,#37575,.T.);
#52481=ORIENTED_EDGE('',*,*,#37577,.F.);
#52482=ORIENTED_EDGE('',*,*,#37578,.F.);
#52483=ORIENTED_EDGE('',*,*,#37579,.T.);
#52484=ORIENTED_EDGE('',*,*,#37578,.T.);
#52485=ORIENTED_EDGE('',*,*,#37580,.F.);
#52486=ORIENTED_EDGE('',*,*,#36055,.F.);
#52487=ORIENTED_EDGE('',*,*,#36075,.F.);
#52488=ORIENTED_EDGE('',*,*,#37581,.F.);
#52489=ORIENTED_EDGE('',*,*,#36064,.F.);
#52490=ORIENTED_EDGE('',*,*,#37582,.T.);
#52491=ORIENTED_EDGE('',*,*,#36083,.F.);
#52492=ORIENTED_EDGE('',*,*,#36081,.T.);
#52493=ORIENTED_EDGE('',*,*,#36074,.F.);
#52494=ORIENTED_EDGE('',*,*,#36080,.T.);
#52495=ORIENTED_EDGE('',*,*,#36056,.T.);
#52496=ORIENTED_EDGE('',*,*,#37580,.T.);
#52497=ORIENTED_EDGE('',*,*,#37577,.T.);
#52498=ORIENTED_EDGE('',*,*,#37574,.T.);
#52499=ORIENTED_EDGE('',*,*,#37571,.T.);
#52500=ORIENTED_EDGE('',*,*,#37568,.T.);
#52501=ORIENTED_EDGE('',*,*,#37565,.T.);
#52502=ORIENTED_EDGE('',*,*,#37562,.T.);
#52503=ORIENTED_EDGE('',*,*,#37559,.T.);
#52504=ORIENTED_EDGE('',*,*,#37556,.T.);
#52505=ORIENTED_EDGE('',*,*,#37553,.T.);
#52506=ORIENTED_EDGE('',*,*,#37550,.T.);
#52507=ORIENTED_EDGE('',*,*,#37547,.T.);
#52508=ORIENTED_EDGE('',*,*,#37544,.T.);
#52509=ORIENTED_EDGE('',*,*,#37541,.T.);
#52510=ORIENTED_EDGE('',*,*,#37538,.T.);
#52511=ORIENTED_EDGE('',*,*,#37535,.T.);
#52512=ORIENTED_EDGE('',*,*,#37532,.T.);
#52513=ORIENTED_EDGE('',*,*,#37529,.T.);
#52514=ORIENTED_EDGE('',*,*,#37526,.T.);
#52515=ORIENTED_EDGE('',*,*,#37523,.T.);
#52516=ORIENTED_EDGE('',*,*,#37520,.T.);
#52517=ORIENTED_EDGE('',*,*,#37517,.T.);
#52518=ORIENTED_EDGE('',*,*,#37514,.T.);
#52519=ORIENTED_EDGE('',*,*,#37511,.T.);
#52520=ORIENTED_EDGE('',*,*,#37508,.T.);
#52521=ORIENTED_EDGE('',*,*,#37505,.T.);
#52522=ORIENTED_EDGE('',*,*,#37502,.T.);
#52523=ORIENTED_EDGE('',*,*,#37499,.T.);
#52524=ORIENTED_EDGE('',*,*,#37496,.T.);
#52525=ORIENTED_EDGE('',*,*,#37493,.T.);
#52526=ORIENTED_EDGE('',*,*,#37490,.T.);
#52527=ORIENTED_EDGE('',*,*,#37487,.T.);
#52528=ORIENTED_EDGE('',*,*,#37484,.T.);
#52529=ORIENTED_EDGE('',*,*,#37481,.T.);
#52530=ORIENTED_EDGE('',*,*,#37478,.T.);
#52531=ORIENTED_EDGE('',*,*,#37475,.T.);
#52532=ORIENTED_EDGE('',*,*,#37472,.T.);
#52533=ORIENTED_EDGE('',*,*,#37469,.T.);
#52534=ORIENTED_EDGE('',*,*,#37466,.T.);
#52535=ORIENTED_EDGE('',*,*,#37463,.T.);
#52536=ORIENTED_EDGE('',*,*,#37460,.T.);
#52537=ORIENTED_EDGE('',*,*,#37457,.T.);
#52538=ORIENTED_EDGE('',*,*,#37454,.T.);
#52539=ORIENTED_EDGE('',*,*,#37451,.T.);
#52540=ORIENTED_EDGE('',*,*,#37448,.T.);
#52541=ORIENTED_EDGE('',*,*,#37445,.T.);
#52542=ORIENTED_EDGE('',*,*,#37442,.T.);
#52543=ORIENTED_EDGE('',*,*,#37439,.T.);
#52544=ORIENTED_EDGE('',*,*,#37436,.T.);
#52545=ORIENTED_EDGE('',*,*,#37433,.T.);
#52546=ORIENTED_EDGE('',*,*,#37430,.T.);
#52547=ORIENTED_EDGE('',*,*,#37427,.T.);
#52548=ORIENTED_EDGE('',*,*,#37424,.T.);
#52549=ORIENTED_EDGE('',*,*,#37421,.T.);
#52550=ORIENTED_EDGE('',*,*,#37418,.T.);
#52551=ORIENTED_EDGE('',*,*,#37415,.T.);
#52552=ORIENTED_EDGE('',*,*,#37412,.T.);
#52553=ORIENTED_EDGE('',*,*,#37409,.T.);
#52554=ORIENTED_EDGE('',*,*,#37406,.T.);
#52555=ORIENTED_EDGE('',*,*,#37403,.T.);
#52556=ORIENTED_EDGE('',*,*,#37400,.T.);
#52557=ORIENTED_EDGE('',*,*,#37397,.T.);
#52558=ORIENTED_EDGE('',*,*,#37394,.T.);
#52559=ORIENTED_EDGE('',*,*,#37391,.T.);
#52560=ORIENTED_EDGE('',*,*,#37388,.T.);
#52561=ORIENTED_EDGE('',*,*,#37385,.T.);
#52562=ORIENTED_EDGE('',*,*,#37382,.T.);
#52563=ORIENTED_EDGE('',*,*,#37379,.T.);
#52564=ORIENTED_EDGE('',*,*,#37376,.T.);
#52565=ORIENTED_EDGE('',*,*,#37373,.T.);
#52566=ORIENTED_EDGE('',*,*,#37370,.T.);
#52567=ORIENTED_EDGE('',*,*,#37367,.T.);
#52568=ORIENTED_EDGE('',*,*,#37364,.T.);
#52569=ORIENTED_EDGE('',*,*,#37361,.T.);
#52570=ORIENTED_EDGE('',*,*,#37358,.T.);
#52571=ORIENTED_EDGE('',*,*,#37355,.T.);
#52572=ORIENTED_EDGE('',*,*,#37352,.T.);
#52573=ORIENTED_EDGE('',*,*,#37349,.T.);
#52574=ORIENTED_EDGE('',*,*,#37346,.T.);
#52575=ORIENTED_EDGE('',*,*,#37343,.T.);
#52576=ORIENTED_EDGE('',*,*,#37340,.T.);
#52577=ORIENTED_EDGE('',*,*,#37337,.T.);
#52578=ORIENTED_EDGE('',*,*,#37334,.T.);
#52579=ORIENTED_EDGE('',*,*,#37331,.T.);
#52580=ORIENTED_EDGE('',*,*,#37328,.T.);
#52581=ORIENTED_EDGE('',*,*,#37325,.T.);
#52582=ORIENTED_EDGE('',*,*,#37322,.T.);
#52583=ORIENTED_EDGE('',*,*,#37319,.T.);
#52584=ORIENTED_EDGE('',*,*,#37316,.T.);
#52585=ORIENTED_EDGE('',*,*,#37313,.T.);
#52586=ORIENTED_EDGE('',*,*,#37310,.T.);
#52587=ORIENTED_EDGE('',*,*,#37307,.T.);
#52588=ORIENTED_EDGE('',*,*,#37304,.T.);
#52589=ORIENTED_EDGE('',*,*,#37301,.T.);
#52590=ORIENTED_EDGE('',*,*,#37298,.T.);
#52591=ORIENTED_EDGE('',*,*,#37295,.T.);
#52592=ORIENTED_EDGE('',*,*,#37292,.T.);
#52593=ORIENTED_EDGE('',*,*,#37289,.T.);
#52594=ORIENTED_EDGE('',*,*,#37286,.T.);
#52595=ORIENTED_EDGE('',*,*,#37283,.T.);
#52596=ORIENTED_EDGE('',*,*,#37280,.T.);
#52597=ORIENTED_EDGE('',*,*,#37277,.T.);
#52598=ORIENTED_EDGE('',*,*,#37274,.T.);
#52599=ORIENTED_EDGE('',*,*,#37271,.T.);
#52600=ORIENTED_EDGE('',*,*,#37268,.T.);
#52601=ORIENTED_EDGE('',*,*,#37265,.T.);
#52602=ORIENTED_EDGE('',*,*,#37262,.T.);
#52603=ORIENTED_EDGE('',*,*,#37259,.T.);
#52604=ORIENTED_EDGE('',*,*,#37256,.T.);
#52605=ORIENTED_EDGE('',*,*,#37253,.T.);
#52606=ORIENTED_EDGE('',*,*,#37250,.T.);
#52607=ORIENTED_EDGE('',*,*,#37247,.T.);
#52608=ORIENTED_EDGE('',*,*,#37244,.T.);
#52609=ORIENTED_EDGE('',*,*,#37241,.T.);
#52610=ORIENTED_EDGE('',*,*,#37238,.T.);
#52611=ORIENTED_EDGE('',*,*,#37235,.T.);
#52612=ORIENTED_EDGE('',*,*,#37232,.T.);
#52613=ORIENTED_EDGE('',*,*,#37229,.T.);
#52614=ORIENTED_EDGE('',*,*,#37226,.T.);
#52615=ORIENTED_EDGE('',*,*,#37223,.T.);
#52616=ORIENTED_EDGE('',*,*,#37220,.T.);
#52617=ORIENTED_EDGE('',*,*,#37217,.T.);
#52618=ORIENTED_EDGE('',*,*,#37214,.T.);
#52619=ORIENTED_EDGE('',*,*,#37211,.T.);
#52620=ORIENTED_EDGE('',*,*,#37208,.T.);
#52621=ORIENTED_EDGE('',*,*,#37205,.T.);
#52622=ORIENTED_EDGE('',*,*,#37202,.T.);
#52623=ORIENTED_EDGE('',*,*,#37199,.T.);
#52624=ORIENTED_EDGE('',*,*,#37196,.T.);
#52625=ORIENTED_EDGE('',*,*,#37193,.T.);
#52626=ORIENTED_EDGE('',*,*,#37190,.T.);
#52627=ORIENTED_EDGE('',*,*,#37187,.T.);
#52628=ORIENTED_EDGE('',*,*,#37184,.T.);
#52629=ORIENTED_EDGE('',*,*,#37181,.T.);
#52630=ORIENTED_EDGE('',*,*,#37178,.T.);
#52631=ORIENTED_EDGE('',*,*,#37175,.T.);
#52632=ORIENTED_EDGE('',*,*,#37172,.T.);
#52633=ORIENTED_EDGE('',*,*,#37169,.T.);
#52634=ORIENTED_EDGE('',*,*,#37166,.T.);
#52635=ORIENTED_EDGE('',*,*,#37163,.T.);
#52636=ORIENTED_EDGE('',*,*,#37160,.T.);
#52637=ORIENTED_EDGE('',*,*,#37157,.T.);
#52638=ORIENTED_EDGE('',*,*,#37154,.T.);
#52639=ORIENTED_EDGE('',*,*,#37151,.T.);
#52640=ORIENTED_EDGE('',*,*,#37148,.T.);
#52641=ORIENTED_EDGE('',*,*,#37145,.T.);
#52642=ORIENTED_EDGE('',*,*,#37142,.T.);
#52643=ORIENTED_EDGE('',*,*,#37139,.T.);
#52644=ORIENTED_EDGE('',*,*,#37136,.T.);
#52645=ORIENTED_EDGE('',*,*,#37133,.T.);
#52646=ORIENTED_EDGE('',*,*,#37130,.T.);
#52647=ORIENTED_EDGE('',*,*,#37127,.T.);
#52648=ORIENTED_EDGE('',*,*,#37124,.T.);
#52649=ORIENTED_EDGE('',*,*,#37121,.T.);
#52650=ORIENTED_EDGE('',*,*,#37118,.T.);
#52651=ORIENTED_EDGE('',*,*,#37115,.T.);
#52652=ORIENTED_EDGE('',*,*,#37112,.T.);
#52653=ORIENTED_EDGE('',*,*,#37109,.T.);
#52654=ORIENTED_EDGE('',*,*,#37106,.T.);
#52655=ORIENTED_EDGE('',*,*,#37103,.T.);
#52656=ORIENTED_EDGE('',*,*,#37100,.T.);
#52657=ORIENTED_EDGE('',*,*,#37097,.T.);
#52658=ORIENTED_EDGE('',*,*,#37094,.T.);
#52659=ORIENTED_EDGE('',*,*,#37091,.T.);
#52660=ORIENTED_EDGE('',*,*,#37088,.T.);
#52661=ORIENTED_EDGE('',*,*,#37085,.T.);
#52662=ORIENTED_EDGE('',*,*,#37082,.T.);
#52663=ORIENTED_EDGE('',*,*,#37079,.T.);
#52664=ORIENTED_EDGE('',*,*,#37076,.T.);
#52665=ORIENTED_EDGE('',*,*,#37073,.T.);
#52666=ORIENTED_EDGE('',*,*,#37070,.T.);
#52667=ORIENTED_EDGE('',*,*,#37067,.T.);
#52668=ORIENTED_EDGE('',*,*,#37064,.T.);
#52669=ORIENTED_EDGE('',*,*,#37061,.T.);
#52670=ORIENTED_EDGE('',*,*,#37058,.T.);
#52671=ORIENTED_EDGE('',*,*,#37055,.T.);
#52672=ORIENTED_EDGE('',*,*,#37052,.T.);
#52673=ORIENTED_EDGE('',*,*,#37049,.T.);
#52674=ORIENTED_EDGE('',*,*,#37046,.T.);
#52675=ORIENTED_EDGE('',*,*,#37043,.T.);
#52676=ORIENTED_EDGE('',*,*,#37040,.T.);
#52677=ORIENTED_EDGE('',*,*,#37037,.T.);
#52678=ORIENTED_EDGE('',*,*,#37034,.T.);
#52679=ORIENTED_EDGE('',*,*,#37031,.T.);
#52680=ORIENTED_EDGE('',*,*,#37028,.T.);
#52681=ORIENTED_EDGE('',*,*,#37025,.T.);
#52682=ORIENTED_EDGE('',*,*,#37022,.T.);
#52683=ORIENTED_EDGE('',*,*,#37019,.T.);
#52684=ORIENTED_EDGE('',*,*,#37016,.T.);
#52685=ORIENTED_EDGE('',*,*,#37013,.T.);
#52686=ORIENTED_EDGE('',*,*,#37010,.T.);
#52687=ORIENTED_EDGE('',*,*,#37007,.T.);
#52688=ORIENTED_EDGE('',*,*,#37004,.T.);
#52689=ORIENTED_EDGE('',*,*,#37001,.T.);
#52690=ORIENTED_EDGE('',*,*,#36998,.T.);
#52691=ORIENTED_EDGE('',*,*,#36995,.T.);
#52692=ORIENTED_EDGE('',*,*,#36992,.T.);
#52693=ORIENTED_EDGE('',*,*,#36989,.T.);
#52694=ORIENTED_EDGE('',*,*,#36986,.T.);
#52695=ORIENTED_EDGE('',*,*,#36983,.T.);
#52696=ORIENTED_EDGE('',*,*,#36980,.T.);
#52697=ORIENTED_EDGE('',*,*,#36977,.T.);
#52698=ORIENTED_EDGE('',*,*,#36974,.T.);
#52699=ORIENTED_EDGE('',*,*,#36971,.T.);
#52700=ORIENTED_EDGE('',*,*,#36968,.T.);
#52701=ORIENTED_EDGE('',*,*,#36965,.T.);
#52702=ORIENTED_EDGE('',*,*,#36962,.T.);
#52703=ORIENTED_EDGE('',*,*,#36959,.T.);
#52704=ORIENTED_EDGE('',*,*,#36956,.T.);
#52705=ORIENTED_EDGE('',*,*,#36953,.T.);
#52706=ORIENTED_EDGE('',*,*,#36950,.T.);
#52707=ORIENTED_EDGE('',*,*,#36947,.T.);
#52708=ORIENTED_EDGE('',*,*,#36944,.T.);
#52709=ORIENTED_EDGE('',*,*,#36941,.T.);
#52710=ORIENTED_EDGE('',*,*,#36938,.T.);
#52711=ORIENTED_EDGE('',*,*,#36935,.T.);
#52712=ORIENTED_EDGE('',*,*,#36932,.T.);
#52713=ORIENTED_EDGE('',*,*,#36929,.T.);
#52714=ORIENTED_EDGE('',*,*,#36926,.T.);
#52715=ORIENTED_EDGE('',*,*,#36923,.T.);
#52716=ORIENTED_EDGE('',*,*,#36920,.T.);
#52717=ORIENTED_EDGE('',*,*,#36917,.T.);
#52718=ORIENTED_EDGE('',*,*,#36914,.T.);
#52719=ORIENTED_EDGE('',*,*,#36911,.T.);
#52720=ORIENTED_EDGE('',*,*,#36908,.T.);
#52721=ORIENTED_EDGE('',*,*,#36905,.T.);
#52722=ORIENTED_EDGE('',*,*,#36902,.T.);
#52723=ORIENTED_EDGE('',*,*,#36899,.T.);
#52724=ORIENTED_EDGE('',*,*,#36896,.T.);
#52725=ORIENTED_EDGE('',*,*,#36893,.T.);
#52726=ORIENTED_EDGE('',*,*,#36890,.T.);
#52727=ORIENTED_EDGE('',*,*,#36887,.T.);
#52728=ORIENTED_EDGE('',*,*,#36884,.T.);
#52729=ORIENTED_EDGE('',*,*,#36881,.T.);
#52730=ORIENTED_EDGE('',*,*,#36878,.T.);
#52731=ORIENTED_EDGE('',*,*,#36875,.T.);
#52732=ORIENTED_EDGE('',*,*,#36872,.T.);
#52733=ORIENTED_EDGE('',*,*,#36869,.T.);
#52734=ORIENTED_EDGE('',*,*,#36866,.T.);
#52735=ORIENTED_EDGE('',*,*,#36863,.T.);
#52736=ORIENTED_EDGE('',*,*,#36860,.T.);
#52737=ORIENTED_EDGE('',*,*,#36857,.T.);
#52738=ORIENTED_EDGE('',*,*,#36854,.T.);
#52739=ORIENTED_EDGE('',*,*,#36851,.T.);
#52740=ORIENTED_EDGE('',*,*,#36848,.T.);
#52741=ORIENTED_EDGE('',*,*,#36845,.T.);
#52742=ORIENTED_EDGE('',*,*,#36842,.T.);
#52743=ORIENTED_EDGE('',*,*,#36839,.T.);
#52744=ORIENTED_EDGE('',*,*,#36836,.T.);
#52745=ORIENTED_EDGE('',*,*,#36833,.T.);
#52746=ORIENTED_EDGE('',*,*,#36830,.T.);
#52747=ORIENTED_EDGE('',*,*,#36827,.T.);
#52748=ORIENTED_EDGE('',*,*,#36824,.T.);
#52749=ORIENTED_EDGE('',*,*,#36821,.T.);
#52750=ORIENTED_EDGE('',*,*,#36818,.T.);
#52751=ORIENTED_EDGE('',*,*,#36815,.T.);
#52752=ORIENTED_EDGE('',*,*,#36812,.T.);
#52753=ORIENTED_EDGE('',*,*,#36809,.T.);
#52754=ORIENTED_EDGE('',*,*,#36806,.T.);
#52755=ORIENTED_EDGE('',*,*,#36803,.T.);
#52756=ORIENTED_EDGE('',*,*,#36800,.T.);
#52757=ORIENTED_EDGE('',*,*,#36797,.T.);
#52758=ORIENTED_EDGE('',*,*,#36794,.T.);
#52759=ORIENTED_EDGE('',*,*,#36791,.T.);
#52760=ORIENTED_EDGE('',*,*,#36788,.T.);
#52761=ORIENTED_EDGE('',*,*,#36785,.T.);
#52762=ORIENTED_EDGE('',*,*,#36782,.T.);
#52763=ORIENTED_EDGE('',*,*,#36779,.T.);
#52764=ORIENTED_EDGE('',*,*,#36776,.T.);
#52765=ORIENTED_EDGE('',*,*,#36773,.T.);
#52766=ORIENTED_EDGE('',*,*,#36770,.T.);
#52767=ORIENTED_EDGE('',*,*,#36767,.T.);
#52768=ORIENTED_EDGE('',*,*,#36764,.T.);
#52769=ORIENTED_EDGE('',*,*,#36761,.T.);
#52770=ORIENTED_EDGE('',*,*,#36758,.T.);
#52771=ORIENTED_EDGE('',*,*,#36755,.T.);
#52772=ORIENTED_EDGE('',*,*,#36752,.T.);
#52773=ORIENTED_EDGE('',*,*,#36749,.T.);
#52774=ORIENTED_EDGE('',*,*,#36746,.T.);
#52775=ORIENTED_EDGE('',*,*,#36743,.T.);
#52776=ORIENTED_EDGE('',*,*,#36740,.T.);
#52777=ORIENTED_EDGE('',*,*,#36737,.T.);
#52778=ORIENTED_EDGE('',*,*,#36734,.T.);
#52779=ORIENTED_EDGE('',*,*,#36731,.T.);
#52780=ORIENTED_EDGE('',*,*,#36728,.T.);
#52781=ORIENTED_EDGE('',*,*,#36725,.T.);
#52782=ORIENTED_EDGE('',*,*,#36722,.T.);
#52783=ORIENTED_EDGE('',*,*,#36719,.T.);
#52784=ORIENTED_EDGE('',*,*,#36716,.T.);
#52785=ORIENTED_EDGE('',*,*,#36713,.T.);
#52786=ORIENTED_EDGE('',*,*,#36710,.T.);
#52787=ORIENTED_EDGE('',*,*,#36707,.T.);
#52788=ORIENTED_EDGE('',*,*,#36704,.T.);
#52789=ORIENTED_EDGE('',*,*,#36701,.T.);
#52790=ORIENTED_EDGE('',*,*,#36698,.T.);
#52791=ORIENTED_EDGE('',*,*,#36695,.T.);
#52792=ORIENTED_EDGE('',*,*,#36692,.T.);
#52793=ORIENTED_EDGE('',*,*,#36689,.T.);
#52794=ORIENTED_EDGE('',*,*,#36686,.T.);
#52795=ORIENTED_EDGE('',*,*,#36683,.T.);
#52796=ORIENTED_EDGE('',*,*,#36680,.T.);
#52797=ORIENTED_EDGE('',*,*,#36677,.T.);
#52798=ORIENTED_EDGE('',*,*,#36674,.T.);
#52799=ORIENTED_EDGE('',*,*,#36671,.T.);
#52800=ORIENTED_EDGE('',*,*,#36668,.T.);
#52801=ORIENTED_EDGE('',*,*,#36665,.T.);
#52802=ORIENTED_EDGE('',*,*,#36662,.T.);
#52803=ORIENTED_EDGE('',*,*,#36659,.T.);
#52804=ORIENTED_EDGE('',*,*,#36656,.T.);
#52805=ORIENTED_EDGE('',*,*,#36653,.T.);
#52806=ORIENTED_EDGE('',*,*,#36650,.T.);
#52807=ORIENTED_EDGE('',*,*,#36647,.T.);
#52808=ORIENTED_EDGE('',*,*,#36644,.T.);
#52809=ORIENTED_EDGE('',*,*,#36641,.T.);
#52810=ORIENTED_EDGE('',*,*,#36638,.T.);
#52811=ORIENTED_EDGE('',*,*,#36635,.T.);
#52812=ORIENTED_EDGE('',*,*,#36632,.T.);
#52813=ORIENTED_EDGE('',*,*,#36629,.T.);
#52814=ORIENTED_EDGE('',*,*,#36626,.T.);
#52815=ORIENTED_EDGE('',*,*,#36623,.T.);
#52816=ORIENTED_EDGE('',*,*,#36620,.T.);
#52817=ORIENTED_EDGE('',*,*,#36617,.T.);
#52818=ORIENTED_EDGE('',*,*,#36614,.T.);
#52819=ORIENTED_EDGE('',*,*,#36611,.T.);
#52820=ORIENTED_EDGE('',*,*,#36608,.T.);
#52821=ORIENTED_EDGE('',*,*,#36605,.T.);
#52822=ORIENTED_EDGE('',*,*,#36602,.T.);
#52823=ORIENTED_EDGE('',*,*,#36599,.T.);
#52824=ORIENTED_EDGE('',*,*,#36596,.T.);
#52825=ORIENTED_EDGE('',*,*,#36593,.T.);
#52826=ORIENTED_EDGE('',*,*,#36590,.T.);
#52827=ORIENTED_EDGE('',*,*,#36587,.T.);
#52828=ORIENTED_EDGE('',*,*,#36584,.T.);
#52829=ORIENTED_EDGE('',*,*,#36581,.T.);
#52830=ORIENTED_EDGE('',*,*,#36578,.T.);
#52831=ORIENTED_EDGE('',*,*,#36575,.T.);
#52832=ORIENTED_EDGE('',*,*,#36572,.T.);
#52833=ORIENTED_EDGE('',*,*,#36569,.T.);
#52834=ORIENTED_EDGE('',*,*,#36566,.T.);
#52835=ORIENTED_EDGE('',*,*,#36563,.T.);
#52836=ORIENTED_EDGE('',*,*,#36560,.T.);
#52837=ORIENTED_EDGE('',*,*,#36557,.T.);
#52838=ORIENTED_EDGE('',*,*,#36554,.T.);
#52839=ORIENTED_EDGE('',*,*,#36551,.T.);
#52840=ORIENTED_EDGE('',*,*,#36548,.T.);
#52841=ORIENTED_EDGE('',*,*,#36545,.T.);
#52842=ORIENTED_EDGE('',*,*,#36542,.T.);
#52843=ORIENTED_EDGE('',*,*,#36539,.T.);
#52844=ORIENTED_EDGE('',*,*,#36536,.T.);
#52845=ORIENTED_EDGE('',*,*,#36533,.T.);
#52846=ORIENTED_EDGE('',*,*,#36530,.T.);
#52847=ORIENTED_EDGE('',*,*,#36527,.T.);
#52848=ORIENTED_EDGE('',*,*,#36524,.T.);
#52849=ORIENTED_EDGE('',*,*,#36521,.T.);
#52850=ORIENTED_EDGE('',*,*,#36518,.T.);
#52851=ORIENTED_EDGE('',*,*,#36515,.T.);
#52852=ORIENTED_EDGE('',*,*,#36512,.T.);
#52853=ORIENTED_EDGE('',*,*,#36509,.T.);
#52854=ORIENTED_EDGE('',*,*,#36506,.T.);
#52855=ORIENTED_EDGE('',*,*,#36503,.T.);
#52856=ORIENTED_EDGE('',*,*,#36500,.T.);
#52857=ORIENTED_EDGE('',*,*,#36497,.T.);
#52858=ORIENTED_EDGE('',*,*,#36494,.T.);
#52859=ORIENTED_EDGE('',*,*,#36491,.T.);
#52860=ORIENTED_EDGE('',*,*,#36488,.T.);
#52861=ORIENTED_EDGE('',*,*,#36485,.T.);
#52862=ORIENTED_EDGE('',*,*,#36482,.T.);
#52863=ORIENTED_EDGE('',*,*,#36479,.T.);
#52864=ORIENTED_EDGE('',*,*,#36476,.T.);
#52865=ORIENTED_EDGE('',*,*,#36473,.T.);
#52866=ORIENTED_EDGE('',*,*,#36470,.T.);
#52867=ORIENTED_EDGE('',*,*,#36467,.T.);
#52868=ORIENTED_EDGE('',*,*,#36464,.T.);
#52869=ORIENTED_EDGE('',*,*,#36461,.T.);
#52870=ORIENTED_EDGE('',*,*,#36458,.T.);
#52871=ORIENTED_EDGE('',*,*,#36455,.T.);
#52872=ORIENTED_EDGE('',*,*,#36452,.T.);
#52873=ORIENTED_EDGE('',*,*,#36449,.T.);
#52874=ORIENTED_EDGE('',*,*,#36446,.T.);
#52875=ORIENTED_EDGE('',*,*,#36443,.T.);
#52876=ORIENTED_EDGE('',*,*,#36440,.T.);
#52877=ORIENTED_EDGE('',*,*,#36437,.T.);
#52878=ORIENTED_EDGE('',*,*,#36434,.T.);
#52879=ORIENTED_EDGE('',*,*,#36431,.T.);
#52880=ORIENTED_EDGE('',*,*,#36428,.T.);
#52881=ORIENTED_EDGE('',*,*,#36425,.T.);
#52882=ORIENTED_EDGE('',*,*,#36422,.T.);
#52883=ORIENTED_EDGE('',*,*,#36419,.T.);
#52884=ORIENTED_EDGE('',*,*,#36416,.T.);
#52885=ORIENTED_EDGE('',*,*,#36413,.T.);
#52886=ORIENTED_EDGE('',*,*,#36410,.T.);
#52887=ORIENTED_EDGE('',*,*,#36407,.T.);
#52888=ORIENTED_EDGE('',*,*,#36404,.T.);
#52889=ORIENTED_EDGE('',*,*,#36401,.T.);
#52890=ORIENTED_EDGE('',*,*,#36398,.T.);
#52891=ORIENTED_EDGE('',*,*,#36395,.T.);
#52892=ORIENTED_EDGE('',*,*,#36392,.T.);
#52893=ORIENTED_EDGE('',*,*,#36389,.T.);
#52894=ORIENTED_EDGE('',*,*,#36386,.T.);
#52895=ORIENTED_EDGE('',*,*,#36383,.T.);
#52896=ORIENTED_EDGE('',*,*,#36380,.T.);
#52897=ORIENTED_EDGE('',*,*,#36377,.T.);
#52898=ORIENTED_EDGE('',*,*,#36374,.T.);
#52899=ORIENTED_EDGE('',*,*,#36371,.T.);
#52900=ORIENTED_EDGE('',*,*,#36368,.T.);
#52901=ORIENTED_EDGE('',*,*,#36365,.T.);
#52902=ORIENTED_EDGE('',*,*,#36362,.T.);
#52903=ORIENTED_EDGE('',*,*,#36359,.T.);
#52904=ORIENTED_EDGE('',*,*,#36356,.T.);
#52905=ORIENTED_EDGE('',*,*,#36353,.T.);
#52906=ORIENTED_EDGE('',*,*,#36350,.T.);
#52907=ORIENTED_EDGE('',*,*,#36347,.T.);
#52908=ORIENTED_EDGE('',*,*,#36344,.T.);
#52909=ORIENTED_EDGE('',*,*,#36341,.T.);
#52910=ORIENTED_EDGE('',*,*,#36338,.T.);
#52911=ORIENTED_EDGE('',*,*,#36335,.T.);
#52912=ORIENTED_EDGE('',*,*,#36332,.T.);
#52913=ORIENTED_EDGE('',*,*,#36329,.T.);
#52914=ORIENTED_EDGE('',*,*,#36326,.T.);
#52915=ORIENTED_EDGE('',*,*,#36323,.T.);
#52916=ORIENTED_EDGE('',*,*,#36320,.T.);
#52917=ORIENTED_EDGE('',*,*,#36317,.T.);
#52918=ORIENTED_EDGE('',*,*,#36314,.T.);
#52919=ORIENTED_EDGE('',*,*,#36311,.T.);
#52920=ORIENTED_EDGE('',*,*,#36308,.T.);
#52921=ORIENTED_EDGE('',*,*,#36305,.T.);
#52922=ORIENTED_EDGE('',*,*,#36302,.T.);
#52923=ORIENTED_EDGE('',*,*,#36299,.T.);
#52924=ORIENTED_EDGE('',*,*,#36296,.T.);
#52925=ORIENTED_EDGE('',*,*,#36293,.T.);
#52926=ORIENTED_EDGE('',*,*,#36290,.T.);
#52927=ORIENTED_EDGE('',*,*,#36287,.T.);
#52928=ORIENTED_EDGE('',*,*,#36284,.T.);
#52929=ORIENTED_EDGE('',*,*,#36281,.T.);
#52930=ORIENTED_EDGE('',*,*,#36278,.T.);
#52931=ORIENTED_EDGE('',*,*,#36275,.T.);
#52932=ORIENTED_EDGE('',*,*,#36272,.T.);
#52933=ORIENTED_EDGE('',*,*,#36269,.T.);
#52934=ORIENTED_EDGE('',*,*,#36266,.T.);
#52935=ORIENTED_EDGE('',*,*,#36263,.T.);
#52936=ORIENTED_EDGE('',*,*,#36260,.T.);
#52937=ORIENTED_EDGE('',*,*,#36257,.T.);
#52938=ORIENTED_EDGE('',*,*,#36254,.T.);
#52939=ORIENTED_EDGE('',*,*,#36251,.T.);
#52940=ORIENTED_EDGE('',*,*,#36248,.T.);
#52941=ORIENTED_EDGE('',*,*,#36245,.T.);
#52942=ORIENTED_EDGE('',*,*,#36242,.T.);
#52943=ORIENTED_EDGE('',*,*,#36239,.T.);
#52944=ORIENTED_EDGE('',*,*,#36236,.T.);
#52945=ORIENTED_EDGE('',*,*,#36233,.T.);
#52946=ORIENTED_EDGE('',*,*,#36230,.T.);
#52947=ORIENTED_EDGE('',*,*,#36227,.T.);
#52948=ORIENTED_EDGE('',*,*,#36224,.T.);
#52949=ORIENTED_EDGE('',*,*,#36221,.T.);
#52950=ORIENTED_EDGE('',*,*,#36218,.T.);
#52951=ORIENTED_EDGE('',*,*,#36215,.T.);
#52952=ORIENTED_EDGE('',*,*,#36212,.T.);
#52953=ORIENTED_EDGE('',*,*,#36209,.T.);
#52954=ORIENTED_EDGE('',*,*,#36206,.T.);
#52955=ORIENTED_EDGE('',*,*,#36203,.T.);
#52956=ORIENTED_EDGE('',*,*,#36200,.T.);
#52957=ORIENTED_EDGE('',*,*,#36197,.T.);
#52958=ORIENTED_EDGE('',*,*,#36194,.T.);
#52959=ORIENTED_EDGE('',*,*,#36191,.T.);
#52960=ORIENTED_EDGE('',*,*,#36188,.T.);
#52961=ORIENTED_EDGE('',*,*,#36185,.T.);
#52962=ORIENTED_EDGE('',*,*,#36182,.T.);
#52963=ORIENTED_EDGE('',*,*,#36179,.T.);
#52964=ORIENTED_EDGE('',*,*,#36176,.T.);
#52965=ORIENTED_EDGE('',*,*,#36173,.T.);
#52966=ORIENTED_EDGE('',*,*,#36170,.T.);
#52967=ORIENTED_EDGE('',*,*,#36167,.T.);
#52968=ORIENTED_EDGE('',*,*,#36164,.T.);
#52969=ORIENTED_EDGE('',*,*,#36161,.T.);
#52970=ORIENTED_EDGE('',*,*,#36158,.T.);
#52971=ORIENTED_EDGE('',*,*,#36155,.T.);
#52972=ORIENTED_EDGE('',*,*,#36152,.T.);
#52973=ORIENTED_EDGE('',*,*,#36149,.T.);
#52974=ORIENTED_EDGE('',*,*,#36146,.T.);
#52975=ORIENTED_EDGE('',*,*,#36143,.T.);
#52976=ORIENTED_EDGE('',*,*,#36140,.T.);
#52977=ORIENTED_EDGE('',*,*,#36137,.T.);
#52978=ORIENTED_EDGE('',*,*,#36134,.T.);
#52979=ORIENTED_EDGE('',*,*,#36131,.T.);
#52980=ORIENTED_EDGE('',*,*,#36128,.T.);
#52981=ORIENTED_EDGE('',*,*,#36125,.T.);
#52982=ORIENTED_EDGE('',*,*,#36122,.T.);
#52983=ORIENTED_EDGE('',*,*,#36119,.T.);
#52984=ORIENTED_EDGE('',*,*,#36116,.T.);
#52985=ORIENTED_EDGE('',*,*,#36113,.T.);
#52986=ORIENTED_EDGE('',*,*,#36110,.T.);
#52987=ORIENTED_EDGE('',*,*,#36107,.T.);
#52988=ORIENTED_EDGE('',*,*,#36104,.T.);
#52989=ORIENTED_EDGE('',*,*,#36101,.T.);
#52990=ORIENTED_EDGE('',*,*,#36098,.T.);
#52991=ORIENTED_EDGE('',*,*,#36095,.T.);
#52992=ORIENTED_EDGE('',*,*,#36092,.T.);
#52993=ORIENTED_EDGE('',*,*,#36089,.T.);
#52994=ORIENTED_EDGE('',*,*,#36086,.T.);
#52995=ORIENTED_EDGE('',*,*,#36065,.T.);
#52996=ORIENTED_EDGE('',*,*,#37581,.T.);
#52997=ORIENTED_EDGE('',*,*,#36084,.F.);
#52998=ORIENTED_EDGE('',*,*,#37582,.F.);
#52999=ORIENTED_EDGE('',*,*,#36063,.F.);
#53000=ORIENTED_EDGE('',*,*,#36085,.F.);
#53001=ORIENTED_EDGE('',*,*,#36088,.F.);
#53002=ORIENTED_EDGE('',*,*,#36091,.F.);
#53003=ORIENTED_EDGE('',*,*,#36094,.F.);
#53004=ORIENTED_EDGE('',*,*,#36097,.F.);
#53005=ORIENTED_EDGE('',*,*,#36100,.F.);
#53006=ORIENTED_EDGE('',*,*,#36103,.F.);
#53007=ORIENTED_EDGE('',*,*,#36106,.F.);
#53008=ORIENTED_EDGE('',*,*,#36109,.F.);
#53009=ORIENTED_EDGE('',*,*,#36112,.F.);
#53010=ORIENTED_EDGE('',*,*,#36115,.F.);
#53011=ORIENTED_EDGE('',*,*,#36118,.F.);
#53012=ORIENTED_EDGE('',*,*,#36121,.F.);
#53013=ORIENTED_EDGE('',*,*,#36124,.F.);
#53014=ORIENTED_EDGE('',*,*,#36127,.F.);
#53015=ORIENTED_EDGE('',*,*,#36130,.F.);
#53016=ORIENTED_EDGE('',*,*,#36133,.F.);
#53017=ORIENTED_EDGE('',*,*,#36136,.F.);
#53018=ORIENTED_EDGE('',*,*,#36139,.F.);
#53019=ORIENTED_EDGE('',*,*,#36142,.F.);
#53020=ORIENTED_EDGE('',*,*,#36145,.F.);
#53021=ORIENTED_EDGE('',*,*,#36148,.F.);
#53022=ORIENTED_EDGE('',*,*,#36151,.F.);
#53023=ORIENTED_EDGE('',*,*,#36154,.F.);
#53024=ORIENTED_EDGE('',*,*,#36157,.F.);
#53025=ORIENTED_EDGE('',*,*,#36160,.F.);
#53026=ORIENTED_EDGE('',*,*,#36163,.F.);
#53027=ORIENTED_EDGE('',*,*,#36166,.F.);
#53028=ORIENTED_EDGE('',*,*,#36169,.F.);
#53029=ORIENTED_EDGE('',*,*,#36172,.F.);
#53030=ORIENTED_EDGE('',*,*,#36175,.F.);
#53031=ORIENTED_EDGE('',*,*,#36178,.F.);
#53032=ORIENTED_EDGE('',*,*,#36181,.F.);
#53033=ORIENTED_EDGE('',*,*,#36184,.F.);
#53034=ORIENTED_EDGE('',*,*,#36187,.F.);
#53035=ORIENTED_EDGE('',*,*,#36190,.F.);
#53036=ORIENTED_EDGE('',*,*,#36193,.F.);
#53037=ORIENTED_EDGE('',*,*,#36196,.F.);
#53038=ORIENTED_EDGE('',*,*,#36199,.F.);
#53039=ORIENTED_EDGE('',*,*,#36202,.F.);
#53040=ORIENTED_EDGE('',*,*,#36205,.F.);
#53041=ORIENTED_EDGE('',*,*,#36208,.F.);
#53042=ORIENTED_EDGE('',*,*,#36211,.F.);
#53043=ORIENTED_EDGE('',*,*,#36214,.F.);
#53044=ORIENTED_EDGE('',*,*,#36217,.F.);
#53045=ORIENTED_EDGE('',*,*,#36220,.F.);
#53046=ORIENTED_EDGE('',*,*,#36223,.F.);
#53047=ORIENTED_EDGE('',*,*,#36226,.F.);
#53048=ORIENTED_EDGE('',*,*,#36229,.F.);
#53049=ORIENTED_EDGE('',*,*,#36232,.F.);
#53050=ORIENTED_EDGE('',*,*,#36235,.F.);
#53051=ORIENTED_EDGE('',*,*,#36238,.F.);
#53052=ORIENTED_EDGE('',*,*,#36241,.F.);
#53053=ORIENTED_EDGE('',*,*,#36244,.F.);
#53054=ORIENTED_EDGE('',*,*,#36247,.F.);
#53055=ORIENTED_EDGE('',*,*,#36250,.F.);
#53056=ORIENTED_EDGE('',*,*,#36253,.F.);
#53057=ORIENTED_EDGE('',*,*,#36256,.F.);
#53058=ORIENTED_EDGE('',*,*,#36259,.F.);
#53059=ORIENTED_EDGE('',*,*,#36262,.F.);
#53060=ORIENTED_EDGE('',*,*,#36265,.F.);
#53061=ORIENTED_EDGE('',*,*,#36268,.F.);
#53062=ORIENTED_EDGE('',*,*,#36271,.F.);
#53063=ORIENTED_EDGE('',*,*,#36274,.F.);
#53064=ORIENTED_EDGE('',*,*,#36277,.F.);
#53065=ORIENTED_EDGE('',*,*,#36280,.F.);
#53066=ORIENTED_EDGE('',*,*,#36283,.F.);
#53067=ORIENTED_EDGE('',*,*,#36286,.F.);
#53068=ORIENTED_EDGE('',*,*,#36289,.F.);
#53069=ORIENTED_EDGE('',*,*,#36292,.F.);
#53070=ORIENTED_EDGE('',*,*,#36295,.F.);
#53071=ORIENTED_EDGE('',*,*,#36298,.F.);
#53072=ORIENTED_EDGE('',*,*,#36301,.F.);
#53073=ORIENTED_EDGE('',*,*,#36304,.F.);
#53074=ORIENTED_EDGE('',*,*,#36307,.F.);
#53075=ORIENTED_EDGE('',*,*,#36310,.F.);
#53076=ORIENTED_EDGE('',*,*,#36313,.F.);
#53077=ORIENTED_EDGE('',*,*,#36316,.F.);
#53078=ORIENTED_EDGE('',*,*,#36319,.F.);
#53079=ORIENTED_EDGE('',*,*,#36322,.F.);
#53080=ORIENTED_EDGE('',*,*,#36325,.F.);
#53081=ORIENTED_EDGE('',*,*,#36328,.F.);
#53082=ORIENTED_EDGE('',*,*,#36331,.F.);
#53083=ORIENTED_EDGE('',*,*,#36334,.F.);
#53084=ORIENTED_EDGE('',*,*,#36337,.F.);
#53085=ORIENTED_EDGE('',*,*,#36340,.F.);
#53086=ORIENTED_EDGE('',*,*,#36343,.F.);
#53087=ORIENTED_EDGE('',*,*,#36346,.F.);
#53088=ORIENTED_EDGE('',*,*,#36349,.F.);
#53089=ORIENTED_EDGE('',*,*,#36352,.F.);
#53090=ORIENTED_EDGE('',*,*,#36355,.F.);
#53091=ORIENTED_EDGE('',*,*,#36358,.F.);
#53092=ORIENTED_EDGE('',*,*,#36361,.F.);
#53093=ORIENTED_EDGE('',*,*,#36364,.F.);
#53094=ORIENTED_EDGE('',*,*,#36367,.F.);
#53095=ORIENTED_EDGE('',*,*,#36370,.F.);
#53096=ORIENTED_EDGE('',*,*,#36373,.F.);
#53097=ORIENTED_EDGE('',*,*,#36376,.F.);
#53098=ORIENTED_EDGE('',*,*,#36379,.F.);
#53099=ORIENTED_EDGE('',*,*,#36382,.F.);
#53100=ORIENTED_EDGE('',*,*,#36385,.F.);
#53101=ORIENTED_EDGE('',*,*,#36388,.F.);
#53102=ORIENTED_EDGE('',*,*,#36391,.F.);
#53103=ORIENTED_EDGE('',*,*,#36394,.F.);
#53104=ORIENTED_EDGE('',*,*,#36397,.F.);
#53105=ORIENTED_EDGE('',*,*,#36400,.F.);
#53106=ORIENTED_EDGE('',*,*,#36403,.F.);
#53107=ORIENTED_EDGE('',*,*,#36406,.F.);
#53108=ORIENTED_EDGE('',*,*,#36409,.F.);
#53109=ORIENTED_EDGE('',*,*,#36412,.F.);
#53110=ORIENTED_EDGE('',*,*,#36415,.F.);
#53111=ORIENTED_EDGE('',*,*,#36418,.F.);
#53112=ORIENTED_EDGE('',*,*,#36421,.F.);
#53113=ORIENTED_EDGE('',*,*,#36424,.F.);
#53114=ORIENTED_EDGE('',*,*,#36427,.F.);
#53115=ORIENTED_EDGE('',*,*,#36430,.F.);
#53116=ORIENTED_EDGE('',*,*,#36433,.F.);
#53117=ORIENTED_EDGE('',*,*,#36436,.F.);
#53118=ORIENTED_EDGE('',*,*,#36439,.F.);
#53119=ORIENTED_EDGE('',*,*,#36442,.F.);
#53120=ORIENTED_EDGE('',*,*,#36445,.F.);
#53121=ORIENTED_EDGE('',*,*,#36448,.F.);
#53122=ORIENTED_EDGE('',*,*,#36451,.F.);
#53123=ORIENTED_EDGE('',*,*,#36454,.F.);
#53124=ORIENTED_EDGE('',*,*,#36457,.F.);
#53125=ORIENTED_EDGE('',*,*,#36460,.F.);
#53126=ORIENTED_EDGE('',*,*,#36463,.F.);
#53127=ORIENTED_EDGE('',*,*,#36466,.F.);
#53128=ORIENTED_EDGE('',*,*,#36469,.F.);
#53129=ORIENTED_EDGE('',*,*,#36472,.F.);
#53130=ORIENTED_EDGE('',*,*,#36475,.F.);
#53131=ORIENTED_EDGE('',*,*,#36478,.F.);
#53132=ORIENTED_EDGE('',*,*,#36481,.F.);
#53133=ORIENTED_EDGE('',*,*,#36484,.F.);
#53134=ORIENTED_EDGE('',*,*,#36487,.F.);
#53135=ORIENTED_EDGE('',*,*,#36490,.F.);
#53136=ORIENTED_EDGE('',*,*,#36493,.F.);
#53137=ORIENTED_EDGE('',*,*,#36496,.F.);
#53138=ORIENTED_EDGE('',*,*,#36499,.F.);
#53139=ORIENTED_EDGE('',*,*,#36502,.F.);
#53140=ORIENTED_EDGE('',*,*,#36505,.F.);
#53141=ORIENTED_EDGE('',*,*,#36508,.F.);
#53142=ORIENTED_EDGE('',*,*,#36511,.F.);
#53143=ORIENTED_EDGE('',*,*,#36514,.F.);
#53144=ORIENTED_EDGE('',*,*,#36517,.F.);
#53145=ORIENTED_EDGE('',*,*,#36520,.F.);
#53146=ORIENTED_EDGE('',*,*,#36523,.F.);
#53147=ORIENTED_EDGE('',*,*,#36526,.F.);
#53148=ORIENTED_EDGE('',*,*,#36529,.F.);
#53149=ORIENTED_EDGE('',*,*,#36532,.F.);
#53150=ORIENTED_EDGE('',*,*,#36535,.F.);
#53151=ORIENTED_EDGE('',*,*,#36538,.F.);
#53152=ORIENTED_EDGE('',*,*,#36541,.F.);
#53153=ORIENTED_EDGE('',*,*,#36544,.F.);
#53154=ORIENTED_EDGE('',*,*,#36547,.F.);
#53155=ORIENTED_EDGE('',*,*,#36550,.F.);
#53156=ORIENTED_EDGE('',*,*,#36553,.F.);
#53157=ORIENTED_EDGE('',*,*,#36556,.F.);
#53158=ORIENTED_EDGE('',*,*,#36559,.F.);
#53159=ORIENTED_EDGE('',*,*,#36562,.F.);
#53160=ORIENTED_EDGE('',*,*,#36565,.F.);
#53161=ORIENTED_EDGE('',*,*,#36568,.F.);
#53162=ORIENTED_EDGE('',*,*,#36571,.F.);
#53163=ORIENTED_EDGE('',*,*,#36574,.F.);
#53164=ORIENTED_EDGE('',*,*,#36577,.F.);
#53165=ORIENTED_EDGE('',*,*,#36580,.F.);
#53166=ORIENTED_EDGE('',*,*,#36583,.F.);
#53167=ORIENTED_EDGE('',*,*,#36586,.F.);
#53168=ORIENTED_EDGE('',*,*,#36589,.F.);
#53169=ORIENTED_EDGE('',*,*,#36592,.F.);
#53170=ORIENTED_EDGE('',*,*,#36595,.F.);
#53171=ORIENTED_EDGE('',*,*,#36598,.F.);
#53172=ORIENTED_EDGE('',*,*,#36601,.F.);
#53173=ORIENTED_EDGE('',*,*,#36604,.F.);
#53174=ORIENTED_EDGE('',*,*,#36607,.F.);
#53175=ORIENTED_EDGE('',*,*,#36610,.F.);
#53176=ORIENTED_EDGE('',*,*,#36613,.F.);
#53177=ORIENTED_EDGE('',*,*,#36616,.F.);
#53178=ORIENTED_EDGE('',*,*,#36619,.F.);
#53179=ORIENTED_EDGE('',*,*,#36622,.F.);
#53180=ORIENTED_EDGE('',*,*,#36625,.F.);
#53181=ORIENTED_EDGE('',*,*,#36628,.F.);
#53182=ORIENTED_EDGE('',*,*,#36631,.F.);
#53183=ORIENTED_EDGE('',*,*,#36634,.F.);
#53184=ORIENTED_EDGE('',*,*,#36637,.F.);
#53185=ORIENTED_EDGE('',*,*,#36640,.F.);
#53186=ORIENTED_EDGE('',*,*,#36643,.F.);
#53187=ORIENTED_EDGE('',*,*,#36646,.F.);
#53188=ORIENTED_EDGE('',*,*,#36649,.F.);
#53189=ORIENTED_EDGE('',*,*,#36652,.F.);
#53190=ORIENTED_EDGE('',*,*,#36655,.F.);
#53191=ORIENTED_EDGE('',*,*,#36658,.F.);
#53192=ORIENTED_EDGE('',*,*,#36661,.F.);
#53193=ORIENTED_EDGE('',*,*,#36664,.F.);
#53194=ORIENTED_EDGE('',*,*,#36667,.F.);
#53195=ORIENTED_EDGE('',*,*,#36670,.F.);
#53196=ORIENTED_EDGE('',*,*,#36673,.F.);
#53197=ORIENTED_EDGE('',*,*,#36676,.F.);
#53198=ORIENTED_EDGE('',*,*,#36679,.F.);
#53199=ORIENTED_EDGE('',*,*,#36682,.F.);
#53200=ORIENTED_EDGE('',*,*,#36685,.F.);
#53201=ORIENTED_EDGE('',*,*,#36688,.F.);
#53202=ORIENTED_EDGE('',*,*,#36691,.F.);
#53203=ORIENTED_EDGE('',*,*,#36694,.F.);
#53204=ORIENTED_EDGE('',*,*,#36697,.F.);
#53205=ORIENTED_EDGE('',*,*,#36700,.F.);
#53206=ORIENTED_EDGE('',*,*,#36703,.F.);
#53207=ORIENTED_EDGE('',*,*,#36706,.F.);
#53208=ORIENTED_EDGE('',*,*,#36709,.F.);
#53209=ORIENTED_EDGE('',*,*,#36712,.F.);
#53210=ORIENTED_EDGE('',*,*,#36715,.F.);
#53211=ORIENTED_EDGE('',*,*,#36718,.F.);
#53212=ORIENTED_EDGE('',*,*,#36721,.F.);
#53213=ORIENTED_EDGE('',*,*,#36724,.F.);
#53214=ORIENTED_EDGE('',*,*,#36727,.F.);
#53215=ORIENTED_EDGE('',*,*,#36730,.F.);
#53216=ORIENTED_EDGE('',*,*,#36733,.F.);
#53217=ORIENTED_EDGE('',*,*,#36736,.F.);
#53218=ORIENTED_EDGE('',*,*,#36739,.F.);
#53219=ORIENTED_EDGE('',*,*,#36742,.F.);
#53220=ORIENTED_EDGE('',*,*,#36745,.F.);
#53221=ORIENTED_EDGE('',*,*,#36748,.F.);
#53222=ORIENTED_EDGE('',*,*,#36751,.F.);
#53223=ORIENTED_EDGE('',*,*,#36754,.F.);
#53224=ORIENTED_EDGE('',*,*,#36757,.F.);
#53225=ORIENTED_EDGE('',*,*,#36760,.F.);
#53226=ORIENTED_EDGE('',*,*,#36763,.F.);
#53227=ORIENTED_EDGE('',*,*,#36766,.F.);
#53228=ORIENTED_EDGE('',*,*,#36769,.F.);
#53229=ORIENTED_EDGE('',*,*,#36772,.F.);
#53230=ORIENTED_EDGE('',*,*,#36775,.F.);
#53231=ORIENTED_EDGE('',*,*,#36778,.F.);
#53232=ORIENTED_EDGE('',*,*,#36781,.F.);
#53233=ORIENTED_EDGE('',*,*,#36784,.F.);
#53234=ORIENTED_EDGE('',*,*,#36787,.F.);
#53235=ORIENTED_EDGE('',*,*,#36790,.F.);
#53236=ORIENTED_EDGE('',*,*,#36793,.F.);
#53237=ORIENTED_EDGE('',*,*,#36796,.F.);
#53238=ORIENTED_EDGE('',*,*,#36799,.F.);
#53239=ORIENTED_EDGE('',*,*,#36802,.F.);
#53240=ORIENTED_EDGE('',*,*,#36805,.F.);
#53241=ORIENTED_EDGE('',*,*,#36808,.F.);
#53242=ORIENTED_EDGE('',*,*,#36811,.F.);
#53243=ORIENTED_EDGE('',*,*,#36814,.F.);
#53244=ORIENTED_EDGE('',*,*,#36817,.F.);
#53245=ORIENTED_EDGE('',*,*,#36820,.F.);
#53246=ORIENTED_EDGE('',*,*,#36823,.F.);
#53247=ORIENTED_EDGE('',*,*,#36826,.F.);
#53248=ORIENTED_EDGE('',*,*,#36829,.F.);
#53249=ORIENTED_EDGE('',*,*,#36832,.F.);
#53250=ORIENTED_EDGE('',*,*,#36835,.F.);
#53251=ORIENTED_EDGE('',*,*,#36838,.F.);
#53252=ORIENTED_EDGE('',*,*,#36841,.F.);
#53253=ORIENTED_EDGE('',*,*,#36844,.F.);
#53254=ORIENTED_EDGE('',*,*,#36847,.F.);
#53255=ORIENTED_EDGE('',*,*,#36850,.F.);
#53256=ORIENTED_EDGE('',*,*,#36853,.F.);
#53257=ORIENTED_EDGE('',*,*,#36856,.F.);
#53258=ORIENTED_EDGE('',*,*,#36859,.F.);
#53259=ORIENTED_EDGE('',*,*,#36862,.F.);
#53260=ORIENTED_EDGE('',*,*,#36865,.F.);
#53261=ORIENTED_EDGE('',*,*,#36868,.F.);
#53262=ORIENTED_EDGE('',*,*,#36871,.F.);
#53263=ORIENTED_EDGE('',*,*,#36874,.F.);
#53264=ORIENTED_EDGE('',*,*,#36877,.F.);
#53265=ORIENTED_EDGE('',*,*,#36880,.F.);
#53266=ORIENTED_EDGE('',*,*,#36883,.F.);
#53267=ORIENTED_EDGE('',*,*,#36886,.F.);
#53268=ORIENTED_EDGE('',*,*,#36889,.F.);
#53269=ORIENTED_EDGE('',*,*,#36892,.F.);
#53270=ORIENTED_EDGE('',*,*,#36895,.F.);
#53271=ORIENTED_EDGE('',*,*,#36898,.F.);
#53272=ORIENTED_EDGE('',*,*,#36901,.F.);
#53273=ORIENTED_EDGE('',*,*,#36904,.F.);
#53274=ORIENTED_EDGE('',*,*,#36907,.F.);
#53275=ORIENTED_EDGE('',*,*,#36910,.F.);
#53276=ORIENTED_EDGE('',*,*,#36913,.F.);
#53277=ORIENTED_EDGE('',*,*,#36916,.F.);
#53278=ORIENTED_EDGE('',*,*,#36919,.F.);
#53279=ORIENTED_EDGE('',*,*,#36922,.F.);
#53280=ORIENTED_EDGE('',*,*,#36925,.F.);
#53281=ORIENTED_EDGE('',*,*,#36928,.F.);
#53282=ORIENTED_EDGE('',*,*,#36931,.F.);
#53283=ORIENTED_EDGE('',*,*,#36934,.F.);
#53284=ORIENTED_EDGE('',*,*,#36937,.F.);
#53285=ORIENTED_EDGE('',*,*,#36940,.F.);
#53286=ORIENTED_EDGE('',*,*,#36943,.F.);
#53287=ORIENTED_EDGE('',*,*,#36946,.F.);
#53288=ORIENTED_EDGE('',*,*,#36949,.F.);
#53289=ORIENTED_EDGE('',*,*,#36952,.F.);
#53290=ORIENTED_EDGE('',*,*,#36955,.F.);
#53291=ORIENTED_EDGE('',*,*,#36958,.F.);
#53292=ORIENTED_EDGE('',*,*,#36961,.F.);
#53293=ORIENTED_EDGE('',*,*,#36964,.F.);
#53294=ORIENTED_EDGE('',*,*,#36967,.F.);
#53295=ORIENTED_EDGE('',*,*,#36970,.F.);
#53296=ORIENTED_EDGE('',*,*,#36973,.F.);
#53297=ORIENTED_EDGE('',*,*,#36976,.F.);
#53298=ORIENTED_EDGE('',*,*,#36979,.F.);
#53299=ORIENTED_EDGE('',*,*,#36982,.F.);
#53300=ORIENTED_EDGE('',*,*,#36985,.F.);
#53301=ORIENTED_EDGE('',*,*,#36988,.F.);
#53302=ORIENTED_EDGE('',*,*,#36991,.F.);
#53303=ORIENTED_EDGE('',*,*,#36994,.F.);
#53304=ORIENTED_EDGE('',*,*,#36997,.F.);
#53305=ORIENTED_EDGE('',*,*,#37000,.F.);
#53306=ORIENTED_EDGE('',*,*,#37003,.F.);
#53307=ORIENTED_EDGE('',*,*,#37006,.F.);
#53308=ORIENTED_EDGE('',*,*,#37009,.F.);
#53309=ORIENTED_EDGE('',*,*,#37012,.F.);
#53310=ORIENTED_EDGE('',*,*,#37015,.F.);
#53311=ORIENTED_EDGE('',*,*,#37018,.F.);
#53312=ORIENTED_EDGE('',*,*,#37021,.F.);
#53313=ORIENTED_EDGE('',*,*,#37024,.F.);
#53314=ORIENTED_EDGE('',*,*,#37027,.F.);
#53315=ORIENTED_EDGE('',*,*,#37030,.F.);
#53316=ORIENTED_EDGE('',*,*,#37033,.F.);
#53317=ORIENTED_EDGE('',*,*,#37036,.F.);
#53318=ORIENTED_EDGE('',*,*,#37039,.F.);
#53319=ORIENTED_EDGE('',*,*,#37042,.F.);
#53320=ORIENTED_EDGE('',*,*,#37045,.F.);
#53321=ORIENTED_EDGE('',*,*,#37048,.F.);
#53322=ORIENTED_EDGE('',*,*,#37051,.F.);
#53323=ORIENTED_EDGE('',*,*,#37054,.F.);
#53324=ORIENTED_EDGE('',*,*,#37057,.F.);
#53325=ORIENTED_EDGE('',*,*,#37060,.F.);
#53326=ORIENTED_EDGE('',*,*,#37063,.F.);
#53327=ORIENTED_EDGE('',*,*,#37066,.F.);
#53328=ORIENTED_EDGE('',*,*,#37069,.F.);
#53329=ORIENTED_EDGE('',*,*,#37072,.F.);
#53330=ORIENTED_EDGE('',*,*,#37075,.F.);
#53331=ORIENTED_EDGE('',*,*,#37078,.F.);
#53332=ORIENTED_EDGE('',*,*,#37081,.F.);
#53333=ORIENTED_EDGE('',*,*,#37084,.F.);
#53334=ORIENTED_EDGE('',*,*,#37087,.F.);
#53335=ORIENTED_EDGE('',*,*,#37090,.F.);
#53336=ORIENTED_EDGE('',*,*,#37093,.F.);
#53337=ORIENTED_EDGE('',*,*,#37096,.F.);
#53338=ORIENTED_EDGE('',*,*,#37099,.F.);
#53339=ORIENTED_EDGE('',*,*,#37102,.F.);
#53340=ORIENTED_EDGE('',*,*,#37105,.F.);
#53341=ORIENTED_EDGE('',*,*,#37108,.F.);
#53342=ORIENTED_EDGE('',*,*,#37111,.F.);
#53343=ORIENTED_EDGE('',*,*,#37114,.F.);
#53344=ORIENTED_EDGE('',*,*,#37117,.F.);
#53345=ORIENTED_EDGE('',*,*,#37120,.F.);
#53346=ORIENTED_EDGE('',*,*,#37123,.F.);
#53347=ORIENTED_EDGE('',*,*,#37126,.F.);
#53348=ORIENTED_EDGE('',*,*,#37129,.F.);
#53349=ORIENTED_EDGE('',*,*,#37132,.F.);
#53350=ORIENTED_EDGE('',*,*,#37135,.F.);
#53351=ORIENTED_EDGE('',*,*,#37138,.F.);
#53352=ORIENTED_EDGE('',*,*,#37141,.F.);
#53353=ORIENTED_EDGE('',*,*,#37144,.F.);
#53354=ORIENTED_EDGE('',*,*,#37147,.F.);
#53355=ORIENTED_EDGE('',*,*,#37150,.F.);
#53356=ORIENTED_EDGE('',*,*,#37153,.F.);
#53357=ORIENTED_EDGE('',*,*,#37156,.F.);
#53358=ORIENTED_EDGE('',*,*,#37159,.F.);
#53359=ORIENTED_EDGE('',*,*,#37162,.F.);
#53360=ORIENTED_EDGE('',*,*,#37165,.F.);
#53361=ORIENTED_EDGE('',*,*,#37168,.F.);
#53362=ORIENTED_EDGE('',*,*,#37171,.F.);
#53363=ORIENTED_EDGE('',*,*,#37174,.F.);
#53364=ORIENTED_EDGE('',*,*,#37177,.F.);
#53365=ORIENTED_EDGE('',*,*,#37180,.F.);
#53366=ORIENTED_EDGE('',*,*,#37183,.F.);
#53367=ORIENTED_EDGE('',*,*,#37186,.F.);
#53368=ORIENTED_EDGE('',*,*,#37189,.F.);
#53369=ORIENTED_EDGE('',*,*,#37192,.F.);
#53370=ORIENTED_EDGE('',*,*,#37195,.F.);
#53371=ORIENTED_EDGE('',*,*,#37198,.F.);
#53372=ORIENTED_EDGE('',*,*,#37201,.F.);
#53373=ORIENTED_EDGE('',*,*,#37204,.F.);
#53374=ORIENTED_EDGE('',*,*,#37207,.F.);
#53375=ORIENTED_EDGE('',*,*,#37210,.F.);
#53376=ORIENTED_EDGE('',*,*,#37213,.F.);
#53377=ORIENTED_EDGE('',*,*,#37216,.F.);
#53378=ORIENTED_EDGE('',*,*,#37219,.F.);
#53379=ORIENTED_EDGE('',*,*,#37222,.F.);
#53380=ORIENTED_EDGE('',*,*,#37225,.F.);
#53381=ORIENTED_EDGE('',*,*,#37228,.F.);
#53382=ORIENTED_EDGE('',*,*,#37231,.F.);
#53383=ORIENTED_EDGE('',*,*,#37234,.F.);
#53384=ORIENTED_EDGE('',*,*,#37237,.F.);
#53385=ORIENTED_EDGE('',*,*,#37240,.F.);
#53386=ORIENTED_EDGE('',*,*,#37243,.F.);
#53387=ORIENTED_EDGE('',*,*,#37246,.F.);
#53388=ORIENTED_EDGE('',*,*,#37249,.F.);
#53389=ORIENTED_EDGE('',*,*,#37252,.F.);
#53390=ORIENTED_EDGE('',*,*,#37255,.F.);
#53391=ORIENTED_EDGE('',*,*,#37258,.F.);
#53392=ORIENTED_EDGE('',*,*,#37261,.F.);
#53393=ORIENTED_EDGE('',*,*,#37264,.F.);
#53394=ORIENTED_EDGE('',*,*,#37267,.F.);
#53395=ORIENTED_EDGE('',*,*,#37270,.F.);
#53396=ORIENTED_EDGE('',*,*,#37273,.F.);
#53397=ORIENTED_EDGE('',*,*,#37276,.F.);
#53398=ORIENTED_EDGE('',*,*,#37279,.F.);
#53399=ORIENTED_EDGE('',*,*,#37282,.F.);
#53400=ORIENTED_EDGE('',*,*,#37285,.F.);
#53401=ORIENTED_EDGE('',*,*,#37288,.F.);
#53402=ORIENTED_EDGE('',*,*,#37291,.F.);
#53403=ORIENTED_EDGE('',*,*,#37294,.F.);
#53404=ORIENTED_EDGE('',*,*,#37297,.F.);
#53405=ORIENTED_EDGE('',*,*,#37300,.F.);
#53406=ORIENTED_EDGE('',*,*,#37303,.F.);
#53407=ORIENTED_EDGE('',*,*,#37306,.F.);
#53408=ORIENTED_EDGE('',*,*,#37309,.F.);
#53409=ORIENTED_EDGE('',*,*,#37312,.F.);
#53410=ORIENTED_EDGE('',*,*,#37315,.F.);
#53411=ORIENTED_EDGE('',*,*,#37318,.F.);
#53412=ORIENTED_EDGE('',*,*,#37321,.F.);
#53413=ORIENTED_EDGE('',*,*,#37324,.F.);
#53414=ORIENTED_EDGE('',*,*,#37327,.F.);
#53415=ORIENTED_EDGE('',*,*,#37330,.F.);
#53416=ORIENTED_EDGE('',*,*,#37333,.F.);
#53417=ORIENTED_EDGE('',*,*,#37336,.F.);
#53418=ORIENTED_EDGE('',*,*,#37339,.F.);
#53419=ORIENTED_EDGE('',*,*,#37342,.F.);
#53420=ORIENTED_EDGE('',*,*,#37345,.F.);
#53421=ORIENTED_EDGE('',*,*,#37348,.F.);
#53422=ORIENTED_EDGE('',*,*,#37351,.F.);
#53423=ORIENTED_EDGE('',*,*,#37354,.F.);
#53424=ORIENTED_EDGE('',*,*,#37357,.F.);
#53425=ORIENTED_EDGE('',*,*,#37360,.F.);
#53426=ORIENTED_EDGE('',*,*,#37363,.F.);
#53427=ORIENTED_EDGE('',*,*,#37366,.F.);
#53428=ORIENTED_EDGE('',*,*,#37369,.F.);
#53429=ORIENTED_EDGE('',*,*,#37372,.F.);
#53430=ORIENTED_EDGE('',*,*,#37375,.F.);
#53431=ORIENTED_EDGE('',*,*,#37378,.F.);
#53432=ORIENTED_EDGE('',*,*,#37381,.F.);
#53433=ORIENTED_EDGE('',*,*,#37384,.F.);
#53434=ORIENTED_EDGE('',*,*,#37387,.F.);
#53435=ORIENTED_EDGE('',*,*,#37390,.F.);
#53436=ORIENTED_EDGE('',*,*,#37393,.F.);
#53437=ORIENTED_EDGE('',*,*,#37396,.F.);
#53438=ORIENTED_EDGE('',*,*,#37399,.F.);
#53439=ORIENTED_EDGE('',*,*,#37402,.F.);
#53440=ORIENTED_EDGE('',*,*,#37405,.F.);
#53441=ORIENTED_EDGE('',*,*,#37408,.F.);
#53442=ORIENTED_EDGE('',*,*,#37411,.F.);
#53443=ORIENTED_EDGE('',*,*,#37414,.F.);
#53444=ORIENTED_EDGE('',*,*,#37417,.F.);
#53445=ORIENTED_EDGE('',*,*,#37420,.F.);
#53446=ORIENTED_EDGE('',*,*,#37423,.F.);
#53447=ORIENTED_EDGE('',*,*,#37426,.F.);
#53448=ORIENTED_EDGE('',*,*,#37429,.F.);
#53449=ORIENTED_EDGE('',*,*,#37432,.F.);
#53450=ORIENTED_EDGE('',*,*,#37435,.F.);
#53451=ORIENTED_EDGE('',*,*,#37438,.F.);
#53452=ORIENTED_EDGE('',*,*,#37441,.F.);
#53453=ORIENTED_EDGE('',*,*,#37444,.F.);
#53454=ORIENTED_EDGE('',*,*,#37447,.F.);
#53455=ORIENTED_EDGE('',*,*,#37450,.F.);
#53456=ORIENTED_EDGE('',*,*,#37453,.F.);
#53457=ORIENTED_EDGE('',*,*,#37456,.F.);
#53458=ORIENTED_EDGE('',*,*,#37459,.F.);
#53459=ORIENTED_EDGE('',*,*,#37462,.F.);
#53460=ORIENTED_EDGE('',*,*,#37465,.F.);
#53461=ORIENTED_EDGE('',*,*,#37468,.F.);
#53462=ORIENTED_EDGE('',*,*,#37471,.F.);
#53463=ORIENTED_EDGE('',*,*,#37474,.F.);
#53464=ORIENTED_EDGE('',*,*,#37477,.F.);
#53465=ORIENTED_EDGE('',*,*,#37480,.F.);
#53466=ORIENTED_EDGE('',*,*,#37483,.F.);
#53467=ORIENTED_EDGE('',*,*,#37486,.F.);
#53468=ORIENTED_EDGE('',*,*,#37489,.F.);
#53469=ORIENTED_EDGE('',*,*,#37492,.F.);
#53470=ORIENTED_EDGE('',*,*,#37495,.F.);
#53471=ORIENTED_EDGE('',*,*,#37498,.F.);
#53472=ORIENTED_EDGE('',*,*,#37501,.F.);
#53473=ORIENTED_EDGE('',*,*,#37504,.F.);
#53474=ORIENTED_EDGE('',*,*,#37507,.F.);
#53475=ORIENTED_EDGE('',*,*,#37510,.F.);
#53476=ORIENTED_EDGE('',*,*,#37513,.F.);
#53477=ORIENTED_EDGE('',*,*,#37516,.F.);
#53478=ORIENTED_EDGE('',*,*,#37519,.F.);
#53479=ORIENTED_EDGE('',*,*,#37522,.F.);
#53480=ORIENTED_EDGE('',*,*,#37525,.F.);
#53481=ORIENTED_EDGE('',*,*,#37528,.F.);
#53482=ORIENTED_EDGE('',*,*,#37531,.F.);
#53483=ORIENTED_EDGE('',*,*,#37534,.F.);
#53484=ORIENTED_EDGE('',*,*,#37537,.F.);
#53485=ORIENTED_EDGE('',*,*,#37540,.F.);
#53486=ORIENTED_EDGE('',*,*,#37543,.F.);
#53487=ORIENTED_EDGE('',*,*,#37546,.F.);
#53488=ORIENTED_EDGE('',*,*,#37549,.F.);
#53489=ORIENTED_EDGE('',*,*,#37552,.F.);
#53490=ORIENTED_EDGE('',*,*,#37555,.F.);
#53491=ORIENTED_EDGE('',*,*,#37558,.F.);
#53492=ORIENTED_EDGE('',*,*,#37561,.F.);
#53493=ORIENTED_EDGE('',*,*,#37564,.F.);
#53494=ORIENTED_EDGE('',*,*,#37567,.F.);
#53495=ORIENTED_EDGE('',*,*,#37570,.F.);
#53496=ORIENTED_EDGE('',*,*,#37573,.F.);
#53497=ORIENTED_EDGE('',*,*,#37576,.F.);
#53498=ORIENTED_EDGE('',*,*,#37579,.F.);
#53499=ORIENTED_EDGE('',*,*,#36054,.F.);
#53500=ORIENTED_EDGE('',*,*,#36079,.F.);
#53501=ORIENTED_EDGE('',*,*,#37583,.T.);
#53502=ORIENTED_EDGE('',*,*,#37584,.T.);
#53503=ORIENTED_EDGE('',*,*,#37585,.T.);
#53504=ORIENTED_EDGE('',*,*,#37586,.T.);
#53505=ORIENTED_EDGE('',*,*,#37584,.F.);
#53506=ORIENTED_EDGE('',*,*,#37587,.T.);
#53507=ORIENTED_EDGE('',*,*,#37588,.F.);
#53508=ORIENTED_EDGE('',*,*,#37589,.F.);
#53509=ORIENTED_EDGE('',*,*,#37590,.T.);
#53510=ORIENTED_EDGE('',*,*,#37591,.T.);
#53511=ORIENTED_EDGE('',*,*,#37592,.T.);
#53512=ORIENTED_EDGE('',*,*,#37588,.T.);
#53513=ORIENTED_EDGE('',*,*,#37591,.F.);
#53514=ORIENTED_EDGE('',*,*,#37593,.F.);
#53515=ORIENTED_EDGE('',*,*,#37594,.T.);
#53516=ORIENTED_EDGE('',*,*,#37595,.F.);
#53517=ORIENTED_EDGE('',*,*,#37596,.F.);
#53518=ORIENTED_EDGE('',*,*,#37597,.F.);
#53519=ORIENTED_EDGE('',*,*,#37598,.T.);
#53520=ORIENTED_EDGE('',*,*,#37596,.T.);
#53521=ORIENTED_EDGE('',*,*,#37599,.T.);
#53522=ORIENTED_EDGE('',*,*,#37600,.T.);
#53523=ORIENTED_EDGE('',*,*,#37601,.F.);
#53524=ORIENTED_EDGE('',*,*,#37594,.F.);
#53525=ORIENTED_EDGE('',*,*,#37602,.F.);
#53526=ORIENTED_EDGE('',*,*,#37603,.F.);
#53527=ORIENTED_EDGE('',*,*,#37600,.F.);
#53528=ORIENTED_EDGE('',*,*,#37604,.T.);
#53529=ORIENTED_EDGE('',*,*,#37605,.T.);
#53530=ORIENTED_EDGE('',*,*,#37606,.T.);
#53531=ORIENTED_EDGE('',*,*,#37607,.F.);
#53532=ORIENTED_EDGE('',*,*,#37608,.F.);
#53533=ORIENTED_EDGE('',*,*,#37609,.F.);
#53534=ORIENTED_EDGE('',*,*,#37610,.T.);
#53535=ORIENTED_EDGE('',*,*,#37608,.T.);
#53536=ORIENTED_EDGE('',*,*,#37611,.T.);
#53537=ORIENTED_EDGE('',*,*,#37612,.T.);
#53538=ORIENTED_EDGE('',*,*,#37611,.F.);
#53539=ORIENTED_EDGE('',*,*,#37607,.T.);
#53540=ORIENTED_EDGE('',*,*,#37613,.T.);
#53541=ORIENTED_EDGE('',*,*,#37614,.T.);
#53542=ORIENTED_EDGE('',*,*,#37615,.F.);
#53543=ORIENTED_EDGE('',*,*,#37602,.T.);
#53544=ORIENTED_EDGE('',*,*,#37593,.T.);
#53545=ORIENTED_EDGE('',*,*,#37590,.F.);
#53546=ORIENTED_EDGE('',*,*,#37587,.F.);
#53547=ORIENTED_EDGE('',*,*,#37583,.F.);
#53548=ORIENTED_EDGE('',*,*,#37616,.T.);
#53549=ORIENTED_EDGE('',*,*,#37617,.T.);
#53550=ORIENTED_EDGE('',*,*,#37618,.T.);
#53551=ORIENTED_EDGE('',*,*,#37603,.T.);
#53552=ORIENTED_EDGE('',*,*,#37615,.T.);
#53553=ORIENTED_EDGE('',*,*,#37619,.T.);
#53554=ORIENTED_EDGE('',*,*,#37613,.F.);
#53555=ORIENTED_EDGE('',*,*,#37606,.F.);
#53556=ORIENTED_EDGE('',*,*,#37620,.T.);
#53557=ORIENTED_EDGE('',*,*,#37621,.F.);
#53558=ORIENTED_EDGE('',*,*,#37622,.F.);
#53559=ORIENTED_EDGE('',*,*,#37623,.F.);
#53560=ORIENTED_EDGE('',*,*,#37605,.F.);
#53561=ORIENTED_EDGE('',*,*,#37624,.T.);
#53562=ORIENTED_EDGE('',*,*,#37625,.F.);
#53563=ORIENTED_EDGE('',*,*,#37620,.F.);
#53564=ORIENTED_EDGE('',*,*,#37618,.F.);
#53565=ORIENTED_EDGE('',*,*,#37626,.F.);
#53566=ORIENTED_EDGE('',*,*,#37627,.T.);
#53567=ORIENTED_EDGE('',*,*,#37628,.F.);
#53568=ORIENTED_EDGE('',*,*,#37624,.F.);
#53569=ORIENTED_EDGE('',*,*,#37604,.F.);
#53570=ORIENTED_EDGE('',*,*,#37599,.F.);
#53571=ORIENTED_EDGE('',*,*,#37595,.T.);
#53572=ORIENTED_EDGE('',*,*,#37601,.T.);
#53573=ORIENTED_EDGE('',*,*,#37629,.F.);
#53574=ORIENTED_EDGE('',*,*,#37622,.T.);
#53575=ORIENTED_EDGE('',*,*,#37630,.F.);
#53576=ORIENTED_EDGE('',*,*,#37627,.F.);
#53577=ORIENTED_EDGE('',*,*,#37614,.F.);
#53578=ORIENTED_EDGE('',*,*,#37623,.T.);
#53579=ORIENTED_EDGE('',*,*,#37629,.T.);
#53580=ORIENTED_EDGE('',*,*,#37626,.T.);
#53581=ORIENTED_EDGE('',*,*,#37619,.F.);
#53582=ORIENTED_EDGE('',*,*,#37625,.T.);
#53583=ORIENTED_EDGE('',*,*,#37628,.T.);
#53584=ORIENTED_EDGE('',*,*,#37630,.T.);
#53585=ORIENTED_EDGE('',*,*,#37621,.T.);
#53586=ORIENTED_EDGE('',*,*,#37617,.F.);
#53587=ORIENTED_EDGE('',*,*,#37631,.T.);
#53588=ORIENTED_EDGE('',*,*,#37632,.F.);
#53589=ORIENTED_EDGE('',*,*,#37631,.F.);
#53590=ORIENTED_EDGE('',*,*,#37586,.F.);
#53591=ORIENTED_EDGE('',*,*,#37633,.F.);
#53592=ORIENTED_EDGE('',*,*,#37612,.F.);
#53593=ORIENTED_EDGE('',*,*,#37616,.F.);
#53594=ORIENTED_EDGE('',*,*,#37598,.F.);
#53595=ORIENTED_EDGE('',*,*,#37609,.T.);
#53596=ORIENTED_EDGE('',*,*,#37610,.F.);
#53597=ORIENTED_EDGE('',*,*,#37633,.T.);
#53598=ORIENTED_EDGE('',*,*,#37585,.F.);
#53599=ORIENTED_EDGE('',*,*,#37589,.T.);
#53600=ORIENTED_EDGE('',*,*,#37592,.F.);
#53601=ORIENTED_EDGE('',*,*,#37597,.T.);
#53602=ORIENTED_EDGE('',*,*,#37632,.T.);
#53603=ORIENTED_EDGE('',*,*,#37634,.F.);
#53604=ORIENTED_EDGE('',*,*,#37635,.F.);
#53605=ORIENTED_EDGE('',*,*,#37636,.T.);
#53606=ORIENTED_EDGE('',*,*,#37637,.T.);
#53607=ORIENTED_EDGE('',*,*,#37638,.F.);
#53608=ORIENTED_EDGE('',*,*,#37637,.F.);
#53609=ORIENTED_EDGE('',*,*,#37639,.F.);
#53610=ORIENTED_EDGE('',*,*,#37640,.F.);
#53611=ORIENTED_EDGE('',*,*,#37641,.F.);
#53612=ORIENTED_EDGE('',*,*,#37642,.T.);
#53613=ORIENTED_EDGE('',*,*,#37639,.T.);
#53614=ORIENTED_EDGE('',*,*,#37636,.F.);
#53615=ORIENTED_EDGE('',*,*,#37643,.F.);
#53616=ORIENTED_EDGE('',*,*,#37640,.T.);
#53617=ORIENTED_EDGE('',*,*,#37642,.F.);
#53618=ORIENTED_EDGE('',*,*,#37644,.F.);
#53619=ORIENTED_EDGE('',*,*,#37645,.F.);
#53620=ORIENTED_EDGE('',*,*,#37646,.F.);
#53621=ORIENTED_EDGE('',*,*,#37647,.T.);
#53622=ORIENTED_EDGE('',*,*,#37648,.T.);
#53623=ORIENTED_EDGE('',*,*,#37649,.F.);
#53624=ORIENTED_EDGE('',*,*,#37648,.F.);
#53625=ORIENTED_EDGE('',*,*,#37650,.F.);
#53626=ORIENTED_EDGE('',*,*,#37651,.F.);
#53627=ORIENTED_EDGE('',*,*,#37652,.F.);
#53628=ORIENTED_EDGE('',*,*,#37653,.T.);
#53629=ORIENTED_EDGE('',*,*,#37650,.T.);
#53630=ORIENTED_EDGE('',*,*,#37647,.F.);
#53631=ORIENTED_EDGE('',*,*,#37654,.F.);
#53632=ORIENTED_EDGE('',*,*,#37651,.T.);
#53633=ORIENTED_EDGE('',*,*,#37653,.F.);
#53634=ORIENTED_EDGE('',*,*,#37655,.F.);
#53635=ORIENTED_EDGE('',*,*,#37656,.F.);
#53636=ORIENTED_EDGE('',*,*,#37657,.F.);
#53637=ORIENTED_EDGE('',*,*,#37658,.T.);
#53638=ORIENTED_EDGE('',*,*,#37659,.T.);
#53639=ORIENTED_EDGE('',*,*,#37660,.F.);
#53640=ORIENTED_EDGE('',*,*,#37659,.F.);
#53641=ORIENTED_EDGE('',*,*,#37661,.F.);
#53642=ORIENTED_EDGE('',*,*,#37662,.F.);
#53643=ORIENTED_EDGE('',*,*,#37663,.F.);
#53644=ORIENTED_EDGE('',*,*,#37664,.T.);
#53645=ORIENTED_EDGE('',*,*,#37661,.T.);
#53646=ORIENTED_EDGE('',*,*,#37658,.F.);
#53647=ORIENTED_EDGE('',*,*,#37665,.F.);
#53648=ORIENTED_EDGE('',*,*,#37662,.T.);
#53649=ORIENTED_EDGE('',*,*,#37664,.F.);
#53650=ORIENTED_EDGE('',*,*,#37666,.F.);
#53651=ORIENTED_EDGE('',*,*,#37667,.F.);
#53652=ORIENTED_EDGE('',*,*,#37668,.F.);
#53653=ORIENTED_EDGE('',*,*,#37669,.T.);
#53654=ORIENTED_EDGE('',*,*,#37670,.T.);
#53655=ORIENTED_EDGE('',*,*,#37671,.F.);
#53656=ORIENTED_EDGE('',*,*,#37670,.F.);
#53657=ORIENTED_EDGE('',*,*,#37672,.F.);
#53658=ORIENTED_EDGE('',*,*,#37673,.F.);
#53659=ORIENTED_EDGE('',*,*,#37674,.F.);
#53660=ORIENTED_EDGE('',*,*,#37675,.T.);
#53661=ORIENTED_EDGE('',*,*,#37672,.T.);
#53662=ORIENTED_EDGE('',*,*,#37669,.F.);
#53663=ORIENTED_EDGE('',*,*,#37676,.F.);
#53664=ORIENTED_EDGE('',*,*,#37673,.T.);
#53665=ORIENTED_EDGE('',*,*,#37675,.F.);
#53666=ORIENTED_EDGE('',*,*,#37677,.F.);
#53667=ORIENTED_EDGE('',*,*,#37678,.F.);
#53668=ORIENTED_EDGE('',*,*,#37679,.F.);
#53669=ORIENTED_EDGE('',*,*,#37680,.T.);
#53670=ORIENTED_EDGE('',*,*,#37681,.T.);
#53671=ORIENTED_EDGE('',*,*,#37682,.F.);
#53672=ORIENTED_EDGE('',*,*,#37681,.F.);
#53673=ORIENTED_EDGE('',*,*,#37683,.F.);
#53674=ORIENTED_EDGE('',*,*,#37684,.F.);
#53675=ORIENTED_EDGE('',*,*,#37685,.F.);
#53676=ORIENTED_EDGE('',*,*,#37686,.T.);
#53677=ORIENTED_EDGE('',*,*,#37683,.T.);
#53678=ORIENTED_EDGE('',*,*,#37680,.F.);
#53679=ORIENTED_EDGE('',*,*,#37687,.F.);
#53680=ORIENTED_EDGE('',*,*,#37684,.T.);
#53681=ORIENTED_EDGE('',*,*,#37686,.F.);
#53682=ORIENTED_EDGE('',*,*,#37688,.F.);
#53683=ORIENTED_EDGE('',*,*,#37689,.F.);
#53684=ORIENTED_EDGE('',*,*,#37690,.F.);
#53685=ORIENTED_EDGE('',*,*,#37691,.T.);
#53686=ORIENTED_EDGE('',*,*,#37692,.T.);
#53687=ORIENTED_EDGE('',*,*,#37693,.F.);
#53688=ORIENTED_EDGE('',*,*,#37692,.F.);
#53689=ORIENTED_EDGE('',*,*,#37694,.F.);
#53690=ORIENTED_EDGE('',*,*,#37695,.F.);
#53691=ORIENTED_EDGE('',*,*,#37696,.F.);
#53692=ORIENTED_EDGE('',*,*,#37697,.T.);
#53693=ORIENTED_EDGE('',*,*,#37694,.T.);
#53694=ORIENTED_EDGE('',*,*,#37691,.F.);
#53695=ORIENTED_EDGE('',*,*,#37698,.F.);
#53696=ORIENTED_EDGE('',*,*,#37695,.T.);
#53697=ORIENTED_EDGE('',*,*,#37697,.F.);
#53698=ORIENTED_EDGE('',*,*,#37699,.F.);
#53699=ORIENTED_EDGE('',*,*,#37700,.F.);
#53700=ORIENTED_EDGE('',*,*,#37701,.F.);
#53701=ORIENTED_EDGE('',*,*,#37702,.T.);
#53702=ORIENTED_EDGE('',*,*,#37703,.T.);
#53703=ORIENTED_EDGE('',*,*,#37704,.F.);
#53704=ORIENTED_EDGE('',*,*,#37703,.F.);
#53705=ORIENTED_EDGE('',*,*,#37705,.F.);
#53706=ORIENTED_EDGE('',*,*,#37706,.F.);
#53707=ORIENTED_EDGE('',*,*,#37707,.F.);
#53708=ORIENTED_EDGE('',*,*,#37708,.T.);
#53709=ORIENTED_EDGE('',*,*,#37705,.T.);
#53710=ORIENTED_EDGE('',*,*,#37702,.F.);
#53711=ORIENTED_EDGE('',*,*,#37709,.F.);
#53712=ORIENTED_EDGE('',*,*,#37706,.T.);
#53713=ORIENTED_EDGE('',*,*,#37708,.F.);
#53714=ORIENTED_EDGE('',*,*,#37710,.F.);
#53715=ORIENTED_EDGE('',*,*,#37711,.F.);
#53716=ORIENTED_EDGE('',*,*,#37712,.F.);
#53717=ORIENTED_EDGE('',*,*,#37713,.T.);
#53718=ORIENTED_EDGE('',*,*,#37714,.T.);
#53719=ORIENTED_EDGE('',*,*,#37715,.F.);
#53720=ORIENTED_EDGE('',*,*,#37714,.F.);
#53721=ORIENTED_EDGE('',*,*,#37716,.F.);
#53722=ORIENTED_EDGE('',*,*,#37717,.F.);
#53723=ORIENTED_EDGE('',*,*,#37718,.F.);
#53724=ORIENTED_EDGE('',*,*,#37719,.T.);
#53725=ORIENTED_EDGE('',*,*,#37716,.T.);
#53726=ORIENTED_EDGE('',*,*,#37713,.F.);
#53727=ORIENTED_EDGE('',*,*,#37720,.F.);
#53728=ORIENTED_EDGE('',*,*,#37717,.T.);
#53729=ORIENTED_EDGE('',*,*,#37719,.F.);
#53730=ORIENTED_EDGE('',*,*,#37721,.F.);
#53731=ORIENTED_EDGE('',*,*,#37722,.F.);
#53732=ORIENTED_EDGE('',*,*,#37723,.T.);
#53733=ORIENTED_EDGE('',*,*,#37724,.F.);
#53734=ORIENTED_EDGE('',*,*,#37725,.F.);
#53735=ORIENTED_EDGE('',*,*,#37726,.F.);
#53736=ORIENTED_EDGE('',*,*,#37727,.F.);
#53737=ORIENTED_EDGE('',*,*,#37728,.F.);
#53738=ORIENTED_EDGE('',*,*,#37729,.T.);
#53739=ORIENTED_EDGE('',*,*,#37730,.F.);
#53740=ORIENTED_EDGE('',*,*,#37729,.F.);
#53741=ORIENTED_EDGE('',*,*,#37731,.F.);
#53742=ORIENTED_EDGE('',*,*,#37723,.F.);
#53743=ORIENTED_EDGE('',*,*,#37732,.F.);
#53744=ORIENTED_EDGE('',*,*,#37733,.F.);
#53745=ORIENTED_EDGE('',*,*,#37734,.T.);
#53746=ORIENTED_EDGE('',*,*,#37735,.T.);
#53747=ORIENTED_EDGE('',*,*,#37736,.F.);
#53748=ORIENTED_EDGE('',*,*,#37735,.F.);
#53749=ORIENTED_EDGE('',*,*,#37737,.F.);
#53750=ORIENTED_EDGE('',*,*,#37738,.F.);
#53751=ORIENTED_EDGE('',*,*,#37739,.F.);
#53752=ORIENTED_EDGE('',*,*,#37740,.T.);
#53753=ORIENTED_EDGE('',*,*,#37737,.T.);
#53754=ORIENTED_EDGE('',*,*,#37734,.F.);
#53755=ORIENTED_EDGE('',*,*,#37741,.F.);
#53756=ORIENTED_EDGE('',*,*,#37738,.T.);
#53757=ORIENTED_EDGE('',*,*,#37740,.F.);
#53758=ORIENTED_EDGE('',*,*,#37742,.F.);
#53759=ORIENTED_EDGE('',*,*,#37743,.F.);
#53760=ORIENTED_EDGE('',*,*,#37744,.F.);
#53761=ORIENTED_EDGE('',*,*,#37745,.T.);
#53762=ORIENTED_EDGE('',*,*,#37746,.T.);
#53763=ORIENTED_EDGE('',*,*,#37747,.F.);
#53764=ORIENTED_EDGE('',*,*,#37746,.F.);
#53765=ORIENTED_EDGE('',*,*,#37748,.F.);
#53766=ORIENTED_EDGE('',*,*,#37749,.F.);
#53767=ORIENTED_EDGE('',*,*,#37750,.F.);
#53768=ORIENTED_EDGE('',*,*,#37751,.T.);
#53769=ORIENTED_EDGE('',*,*,#37748,.T.);
#53770=ORIENTED_EDGE('',*,*,#37745,.F.);
#53771=ORIENTED_EDGE('',*,*,#37752,.F.);
#53772=ORIENTED_EDGE('',*,*,#37749,.T.);
#53773=ORIENTED_EDGE('',*,*,#37751,.F.);
#53774=ORIENTED_EDGE('',*,*,#37753,.F.);
#53775=ORIENTED_EDGE('',*,*,#37754,.F.);
#53776=ORIENTED_EDGE('',*,*,#37755,.F.);
#53777=ORIENTED_EDGE('',*,*,#37756,.T.);
#53778=ORIENTED_EDGE('',*,*,#37757,.T.);
#53779=ORIENTED_EDGE('',*,*,#37758,.F.);
#53780=ORIENTED_EDGE('',*,*,#37757,.F.);
#53781=ORIENTED_EDGE('',*,*,#37759,.F.);
#53782=ORIENTED_EDGE('',*,*,#37760,.F.);
#53783=ORIENTED_EDGE('',*,*,#37761,.F.);
#53784=ORIENTED_EDGE('',*,*,#37762,.T.);
#53785=ORIENTED_EDGE('',*,*,#37759,.T.);
#53786=ORIENTED_EDGE('',*,*,#37756,.F.);
#53787=ORIENTED_EDGE('',*,*,#37763,.F.);
#53788=ORIENTED_EDGE('',*,*,#37760,.T.);
#53789=ORIENTED_EDGE('',*,*,#37762,.F.);
#53790=ORIENTED_EDGE('',*,*,#37764,.F.);
#53791=ORIENTED_EDGE('',*,*,#37765,.F.);
#53792=ORIENTED_EDGE('',*,*,#37766,.F.);
#53793=ORIENTED_EDGE('',*,*,#37767,.T.);
#53794=ORIENTED_EDGE('',*,*,#37768,.T.);
#53795=ORIENTED_EDGE('',*,*,#37769,.F.);
#53796=ORIENTED_EDGE('',*,*,#37768,.F.);
#53797=ORIENTED_EDGE('',*,*,#37770,.F.);
#53798=ORIENTED_EDGE('',*,*,#37771,.F.);
#53799=ORIENTED_EDGE('',*,*,#37772,.F.);
#53800=ORIENTED_EDGE('',*,*,#37773,.T.);
#53801=ORIENTED_EDGE('',*,*,#37770,.T.);
#53802=ORIENTED_EDGE('',*,*,#37767,.F.);
#53803=ORIENTED_EDGE('',*,*,#37774,.F.);
#53804=ORIENTED_EDGE('',*,*,#37771,.T.);
#53805=ORIENTED_EDGE('',*,*,#37773,.F.);
#53806=ORIENTED_EDGE('',*,*,#37775,.F.);
#53807=ORIENTED_EDGE('',*,*,#37776,.F.);
#53808=ORIENTED_EDGE('',*,*,#37777,.F.);
#53809=ORIENTED_EDGE('',*,*,#37778,.T.);
#53810=ORIENTED_EDGE('',*,*,#37779,.T.);
#53811=ORIENTED_EDGE('',*,*,#37780,.F.);
#53812=ORIENTED_EDGE('',*,*,#37779,.F.);
#53813=ORIENTED_EDGE('',*,*,#37781,.F.);
#53814=ORIENTED_EDGE('',*,*,#37782,.F.);
#53815=ORIENTED_EDGE('',*,*,#37783,.F.);
#53816=ORIENTED_EDGE('',*,*,#37784,.T.);
#53817=ORIENTED_EDGE('',*,*,#37781,.T.);
#53818=ORIENTED_EDGE('',*,*,#37778,.F.);
#53819=ORIENTED_EDGE('',*,*,#37785,.F.);
#53820=ORIENTED_EDGE('',*,*,#37782,.T.);
#53821=ORIENTED_EDGE('',*,*,#37784,.F.);
#53822=ORIENTED_EDGE('',*,*,#37786,.F.);
#53823=ORIENTED_EDGE('',*,*,#37787,.F.);
#53824=ORIENTED_EDGE('',*,*,#37788,.F.);
#53825=ORIENTED_EDGE('',*,*,#37789,.T.);
#53826=ORIENTED_EDGE('',*,*,#37790,.T.);
#53827=ORIENTED_EDGE('',*,*,#37791,.F.);
#53828=ORIENTED_EDGE('',*,*,#37790,.F.);
#53829=ORIENTED_EDGE('',*,*,#37792,.F.);
#53830=ORIENTED_EDGE('',*,*,#37793,.F.);
#53831=ORIENTED_EDGE('',*,*,#37794,.F.);
#53832=ORIENTED_EDGE('',*,*,#37795,.T.);
#53833=ORIENTED_EDGE('',*,*,#37792,.T.);
#53834=ORIENTED_EDGE('',*,*,#37789,.F.);
#53835=ORIENTED_EDGE('',*,*,#37796,.F.);
#53836=ORIENTED_EDGE('',*,*,#37793,.T.);
#53837=ORIENTED_EDGE('',*,*,#37795,.F.);
#53838=ORIENTED_EDGE('',*,*,#37797,.F.);
#53839=ORIENTED_EDGE('',*,*,#37798,.F.);
#53840=ORIENTED_EDGE('',*,*,#37799,.F.);
#53841=ORIENTED_EDGE('',*,*,#37800,.T.);
#53842=ORIENTED_EDGE('',*,*,#37801,.T.);
#53843=ORIENTED_EDGE('',*,*,#37802,.F.);
#53844=ORIENTED_EDGE('',*,*,#37801,.F.);
#53845=ORIENTED_EDGE('',*,*,#37803,.F.);
#53846=ORIENTED_EDGE('',*,*,#37804,.F.);
#53847=ORIENTED_EDGE('',*,*,#37805,.F.);
#53848=ORIENTED_EDGE('',*,*,#37806,.T.);
#53849=ORIENTED_EDGE('',*,*,#37803,.T.);
#53850=ORIENTED_EDGE('',*,*,#37800,.F.);
#53851=ORIENTED_EDGE('',*,*,#37807,.F.);
#53852=ORIENTED_EDGE('',*,*,#37804,.T.);
#53853=ORIENTED_EDGE('',*,*,#37806,.F.);
#53854=ORIENTED_EDGE('',*,*,#37808,.F.);
#53855=ORIENTED_EDGE('',*,*,#37809,.F.);
#53856=ORIENTED_EDGE('',*,*,#37810,.T.);
#53857=ORIENTED_EDGE('',*,*,#37811,.F.);
#53858=ORIENTED_EDGE('',*,*,#37812,.F.);
#53859=ORIENTED_EDGE('',*,*,#37813,.F.);
#53860=ORIENTED_EDGE('',*,*,#37814,.F.);
#53861=ORIENTED_EDGE('',*,*,#37815,.F.);
#53862=ORIENTED_EDGE('',*,*,#37816,.T.);
#53863=ORIENTED_EDGE('',*,*,#37817,.F.);
#53864=ORIENTED_EDGE('',*,*,#37816,.F.);
#53865=ORIENTED_EDGE('',*,*,#37818,.F.);
#53866=ORIENTED_EDGE('',*,*,#37810,.F.);
#53867=ORIENTED_EDGE('',*,*,#37812,.T.);
#53868=ORIENTED_EDGE('',*,*,#37819,.T.);
#53869=ORIENTED_EDGE('',*,*,#37820,.T.);
#53870=ORIENTED_EDGE('',*,*,#37727,.T.);
#53871=ORIENTED_EDGE('',*,*,#37821,.T.);
#53872=ORIENTED_EDGE('',*,*,#37822,.T.);
#53873=ORIENTED_EDGE('',*,*,#37634,.T.);
#53874=ORIENTED_EDGE('',*,*,#37638,.T.);
#53875=ORIENTED_EDGE('',*,*,#37643,.T.);
#53876=ORIENTED_EDGE('',*,*,#37823,.F.);
#53877=ORIENTED_EDGE('',*,*,#37798,.T.);
#53878=ORIENTED_EDGE('',*,*,#37802,.T.);
#53879=ORIENTED_EDGE('',*,*,#37807,.T.);
#53880=ORIENTED_EDGE('',*,*,#37824,.F.);
#53881=ORIENTED_EDGE('',*,*,#37645,.T.);
#53882=ORIENTED_EDGE('',*,*,#37649,.T.);
#53883=ORIENTED_EDGE('',*,*,#37654,.T.);
#53884=ORIENTED_EDGE('',*,*,#37825,.F.);
#53885=ORIENTED_EDGE('',*,*,#37787,.T.);
#53886=ORIENTED_EDGE('',*,*,#37791,.T.);
#53887=ORIENTED_EDGE('',*,*,#37796,.T.);
#53888=ORIENTED_EDGE('',*,*,#37826,.F.);
#53889=ORIENTED_EDGE('',*,*,#37656,.T.);
#53890=ORIENTED_EDGE('',*,*,#37660,.T.);
#53891=ORIENTED_EDGE('',*,*,#37665,.T.);
#53892=ORIENTED_EDGE('',*,*,#37827,.F.);
#53893=ORIENTED_EDGE('',*,*,#37776,.T.);
#53894=ORIENTED_EDGE('',*,*,#37780,.T.);
#53895=ORIENTED_EDGE('',*,*,#37785,.T.);
#53896=ORIENTED_EDGE('',*,*,#37828,.F.);
#53897=ORIENTED_EDGE('',*,*,#37667,.T.);
#53898=ORIENTED_EDGE('',*,*,#37671,.T.);
#53899=ORIENTED_EDGE('',*,*,#37676,.T.);
#53900=ORIENTED_EDGE('',*,*,#37829,.F.);
#53901=ORIENTED_EDGE('',*,*,#37678,.T.);
#53902=ORIENTED_EDGE('',*,*,#37682,.T.);
#53903=ORIENTED_EDGE('',*,*,#37687,.T.);
#53904=ORIENTED_EDGE('',*,*,#37830,.F.);
#53905=ORIENTED_EDGE('',*,*,#37765,.T.);
#53906=ORIENTED_EDGE('',*,*,#37769,.T.);
#53907=ORIENTED_EDGE('',*,*,#37774,.T.);
#53908=ORIENTED_EDGE('',*,*,#37831,.F.);
#53909=ORIENTED_EDGE('',*,*,#37689,.T.);
#53910=ORIENTED_EDGE('',*,*,#37693,.T.);
#53911=ORIENTED_EDGE('',*,*,#37698,.T.);
#53912=ORIENTED_EDGE('',*,*,#37832,.F.);
#53913=ORIENTED_EDGE('',*,*,#37754,.T.);
#53914=ORIENTED_EDGE('',*,*,#37758,.T.);
#53915=ORIENTED_EDGE('',*,*,#37763,.T.);
#53916=ORIENTED_EDGE('',*,*,#37833,.F.);
#53917=ORIENTED_EDGE('',*,*,#37700,.T.);
#53918=ORIENTED_EDGE('',*,*,#37704,.T.);
#53919=ORIENTED_EDGE('',*,*,#37709,.T.);
#53920=ORIENTED_EDGE('',*,*,#37834,.F.);
#53921=ORIENTED_EDGE('',*,*,#37743,.T.);
#53922=ORIENTED_EDGE('',*,*,#37747,.T.);
#53923=ORIENTED_EDGE('',*,*,#37752,.T.);
#53924=ORIENTED_EDGE('',*,*,#37835,.F.);
#53925=ORIENTED_EDGE('',*,*,#37711,.T.);
#53926=ORIENTED_EDGE('',*,*,#37715,.T.);
#53927=ORIENTED_EDGE('',*,*,#37720,.T.);
#53928=ORIENTED_EDGE('',*,*,#37836,.F.);
#53929=ORIENTED_EDGE('',*,*,#37732,.T.);
#53930=ORIENTED_EDGE('',*,*,#37736,.T.);
#53931=ORIENTED_EDGE('',*,*,#37741,.T.);
#53932=ORIENTED_EDGE('',*,*,#37837,.F.);
#53933=ORIENTED_EDGE('',*,*,#37724,.T.);
#53934=ORIENTED_EDGE('',*,*,#37731,.T.);
#53935=ORIENTED_EDGE('',*,*,#37728,.T.);
#53936=ORIENTED_EDGE('',*,*,#37822,.F.);
#53937=ORIENTED_EDGE('',*,*,#37838,.T.);
#53938=ORIENTED_EDGE('',*,*,#37839,.F.);
#53939=ORIENTED_EDGE('',*,*,#37840,.F.);
#53940=ORIENTED_EDGE('',*,*,#37841,.T.);
#53941=ORIENTED_EDGE('',*,*,#37842,.T.);
#53942=ORIENTED_EDGE('',*,*,#37843,.F.);
#53943=ORIENTED_EDGE('',*,*,#37844,.T.);
#53944=ORIENTED_EDGE('',*,*,#37819,.F.);
#53945=ORIENTED_EDGE('',*,*,#37811,.T.);
#53946=ORIENTED_EDGE('',*,*,#37818,.T.);
#53947=ORIENTED_EDGE('',*,*,#37815,.T.);
#53948=ORIENTED_EDGE('',*,*,#37845,.F.);
#53949=ORIENTED_EDGE('',*,*,#37846,.F.);
#53950=ORIENTED_EDGE('',*,*,#37847,.T.);
#53951=ORIENTED_EDGE('',*,*,#37848,.T.);
#53952=ORIENTED_EDGE('',*,*,#37847,.F.);
#53953=ORIENTED_EDGE('',*,*,#37848,.F.);
#53954=ORIENTED_EDGE('',*,*,#37849,.T.);
#53955=ORIENTED_EDGE('',*,*,#37850,.F.);
#53956=ORIENTED_EDGE('',*,*,#37813,.T.);
#53957=ORIENTED_EDGE('',*,*,#37817,.T.);
#53958=ORIENTED_EDGE('',*,*,#37809,.T.);
#53959=ORIENTED_EDGE('',*,*,#37820,.F.);
#53960=ORIENTED_EDGE('',*,*,#37844,.F.);
#53961=ORIENTED_EDGE('',*,*,#37851,.F.);
#53962=ORIENTED_EDGE('',*,*,#37852,.F.);
#53963=ORIENTED_EDGE('',*,*,#37853,.F.);
#53964=ORIENTED_EDGE('',*,*,#37849,.F.);
#53965=ORIENTED_EDGE('',*,*,#37635,.T.);
#53966=ORIENTED_EDGE('',*,*,#37845,.T.);
#53967=ORIENTED_EDGE('',*,*,#37814,.T.);
#53968=ORIENTED_EDGE('',*,*,#37850,.T.);
#53969=ORIENTED_EDGE('',*,*,#37853,.T.);
#53970=ORIENTED_EDGE('',*,*,#37854,.T.);
#53971=ORIENTED_EDGE('',*,*,#37855,.T.);
#53972=ORIENTED_EDGE('',*,*,#37725,.T.);
#53973=ORIENTED_EDGE('',*,*,#37837,.T.);
#53974=ORIENTED_EDGE('',*,*,#37742,.T.);
#53975=ORIENTED_EDGE('',*,*,#37739,.T.);
#53976=ORIENTED_EDGE('',*,*,#37733,.T.);
#53977=ORIENTED_EDGE('',*,*,#37836,.T.);
#53978=ORIENTED_EDGE('',*,*,#37721,.T.);
#53979=ORIENTED_EDGE('',*,*,#37718,.T.);
#53980=ORIENTED_EDGE('',*,*,#37712,.T.);
#53981=ORIENTED_EDGE('',*,*,#37835,.T.);
#53982=ORIENTED_EDGE('',*,*,#37753,.T.);
#53983=ORIENTED_EDGE('',*,*,#37750,.T.);
#53984=ORIENTED_EDGE('',*,*,#37744,.T.);
#53985=ORIENTED_EDGE('',*,*,#37834,.T.);
#53986=ORIENTED_EDGE('',*,*,#37710,.T.);
#53987=ORIENTED_EDGE('',*,*,#37707,.T.);
#53988=ORIENTED_EDGE('',*,*,#37701,.T.);
#53989=ORIENTED_EDGE('',*,*,#37833,.T.);
#53990=ORIENTED_EDGE('',*,*,#37764,.T.);
#53991=ORIENTED_EDGE('',*,*,#37761,.T.);
#53992=ORIENTED_EDGE('',*,*,#37755,.T.);
#53993=ORIENTED_EDGE('',*,*,#37832,.T.);
#53994=ORIENTED_EDGE('',*,*,#37699,.T.);
#53995=ORIENTED_EDGE('',*,*,#37696,.T.);
#53996=ORIENTED_EDGE('',*,*,#37690,.T.);
#53997=ORIENTED_EDGE('',*,*,#37831,.T.);
#53998=ORIENTED_EDGE('',*,*,#37775,.T.);
#53999=ORIENTED_EDGE('',*,*,#37772,.T.);
#54000=ORIENTED_EDGE('',*,*,#37766,.T.);
#54001=ORIENTED_EDGE('',*,*,#37830,.T.);
#54002=ORIENTED_EDGE('',*,*,#37688,.T.);
#54003=ORIENTED_EDGE('',*,*,#37685,.T.);
#54004=ORIENTED_EDGE('',*,*,#37679,.T.);
#54005=ORIENTED_EDGE('',*,*,#37829,.T.);
#54006=ORIENTED_EDGE('',*,*,#37677,.T.);
#54007=ORIENTED_EDGE('',*,*,#37674,.T.);
#54008=ORIENTED_EDGE('',*,*,#37668,.T.);
#54009=ORIENTED_EDGE('',*,*,#37828,.T.);
#54010=ORIENTED_EDGE('',*,*,#37786,.T.);
#54011=ORIENTED_EDGE('',*,*,#37783,.T.);
#54012=ORIENTED_EDGE('',*,*,#37777,.T.);
#54013=ORIENTED_EDGE('',*,*,#37827,.T.);
#54014=ORIENTED_EDGE('',*,*,#37666,.T.);
#54015=ORIENTED_EDGE('',*,*,#37663,.T.);
#54016=ORIENTED_EDGE('',*,*,#37657,.T.);
#54017=ORIENTED_EDGE('',*,*,#37826,.T.);
#54018=ORIENTED_EDGE('',*,*,#37797,.T.);
#54019=ORIENTED_EDGE('',*,*,#37794,.T.);
#54020=ORIENTED_EDGE('',*,*,#37788,.T.);
#54021=ORIENTED_EDGE('',*,*,#37825,.T.);
#54022=ORIENTED_EDGE('',*,*,#37655,.T.);
#54023=ORIENTED_EDGE('',*,*,#37652,.T.);
#54024=ORIENTED_EDGE('',*,*,#37646,.T.);
#54025=ORIENTED_EDGE('',*,*,#37824,.T.);
#54026=ORIENTED_EDGE('',*,*,#37808,.T.);
#54027=ORIENTED_EDGE('',*,*,#37805,.T.);
#54028=ORIENTED_EDGE('',*,*,#37799,.T.);
#54029=ORIENTED_EDGE('',*,*,#37823,.T.);
#54030=ORIENTED_EDGE('',*,*,#37644,.T.);
#54031=ORIENTED_EDGE('',*,*,#37641,.T.);
#54032=ORIENTED_EDGE('',*,*,#37851,.T.);
#54033=ORIENTED_EDGE('',*,*,#37843,.T.);
#54034=ORIENTED_EDGE('',*,*,#37856,.T.);
#54035=ORIENTED_EDGE('',*,*,#37857,.T.);
#54036=ORIENTED_EDGE('',*,*,#37858,.T.);
#54037=ORIENTED_EDGE('',*,*,#37859,.F.);
#54038=ORIENTED_EDGE('',*,*,#37860,.T.);
#54039=ORIENTED_EDGE('',*,*,#37861,.T.);
#54040=ORIENTED_EDGE('',*,*,#37860,.F.);
#54041=ORIENTED_EDGE('',*,*,#37861,.F.);
#54042=ORIENTED_EDGE('',*,*,#37862,.T.);
#54043=ORIENTED_EDGE('',*,*,#37863,.F.);
#54044=ORIENTED_EDGE('',*,*,#37838,.F.);
#54045=ORIENTED_EDGE('',*,*,#37821,.F.);
#54046=ORIENTED_EDGE('',*,*,#37726,.T.);
#54047=ORIENTED_EDGE('',*,*,#37730,.T.);
#54048=ORIENTED_EDGE('',*,*,#37722,.T.);
#54049=ORIENTED_EDGE('',*,*,#37855,.F.);
#54050=ORIENTED_EDGE('',*,*,#37864,.F.);
#54051=ORIENTED_EDGE('',*,*,#37865,.F.);
#54052=ORIENTED_EDGE('',*,*,#37862,.F.);
#54053=ORIENTED_EDGE('',*,*,#37863,.T.);
#54054=ORIENTED_EDGE('',*,*,#37865,.T.);
#54055=ORIENTED_EDGE('',*,*,#37866,.T.);
#54056=ORIENTED_EDGE('',*,*,#37867,.T.);
#54057=ORIENTED_EDGE('',*,*,#37868,.T.);
#54058=ORIENTED_EDGE('',*,*,#37839,.T.);
#54059=ORIENTED_EDGE('',*,*,#37869,.T.);
#54060=ORIENTED_EDGE('',*,*,#37870,.T.);
#54061=ORIENTED_EDGE('',*,*,#37867,.F.);
#54062=ORIENTED_EDGE('',*,*,#37871,.F.);
#54063=ORIENTED_EDGE('',*,*,#37852,.T.);
#54064=ORIENTED_EDGE('',*,*,#37858,.F.);
#54065=ORIENTED_EDGE('',*,*,#37872,.F.);
#54066=ORIENTED_EDGE('',*,*,#37873,.T.);
#54067=ORIENTED_EDGE('',*,*,#37871,.T.);
#54068=ORIENTED_EDGE('',*,*,#37866,.F.);
#54069=ORIENTED_EDGE('',*,*,#37864,.T.);
#54070=ORIENTED_EDGE('',*,*,#37854,.F.);
#54071=ORIENTED_EDGE('',*,*,#37874,.T.);
#54072=ORIENTED_EDGE('',*,*,#37872,.T.);
#54073=ORIENTED_EDGE('',*,*,#37857,.F.);
#54074=ORIENTED_EDGE('',*,*,#37875,.F.);
#54075=ORIENTED_EDGE('',*,*,#37876,.T.);
#54076=ORIENTED_EDGE('',*,*,#37875,.T.);
#54077=ORIENTED_EDGE('',*,*,#37856,.F.);
#54078=ORIENTED_EDGE('',*,*,#37842,.F.);
#54079=ORIENTED_EDGE('',*,*,#37877,.T.);
#54080=ORIENTED_EDGE('',*,*,#37840,.T.);
#54081=ORIENTED_EDGE('',*,*,#37868,.F.);
#54082=ORIENTED_EDGE('',*,*,#37870,.F.);
#54083=ORIENTED_EDGE('',*,*,#37877,.F.);
#54084=ORIENTED_EDGE('',*,*,#37869,.F.);
#54085=ORIENTED_EDGE('',*,*,#37873,.F.);
#54086=ORIENTED_EDGE('',*,*,#37874,.F.);
#54087=ORIENTED_EDGE('',*,*,#37876,.F.);
#54088=ORIENTED_EDGE('',*,*,#37841,.F.);
#54089=ORIENTED_EDGE('',*,*,#37846,.T.);
#54090=ORIENTED_EDGE('',*,*,#37859,.T.);
#54091=ORIENTED_EDGE('',*,*,#37878,.F.);
#54092=ORIENTED_EDGE('',*,*,#37879,.T.);
#54093=ORIENTED_EDGE('',*,*,#37880,.F.);
#54094=ORIENTED_EDGE('',*,*,#37881,.T.);
#54095=ORIENTED_EDGE('',*,*,#37882,.F.);
#54096=ORIENTED_EDGE('',*,*,#37883,.T.);
#54097=ORIENTED_EDGE('',*,*,#37878,.T.);
#54098=ORIENTED_EDGE('',*,*,#37884,.T.);
#54099=ORIENTED_EDGE('',*,*,#37885,.F.);
#54100=ORIENTED_EDGE('',*,*,#37886,.T.);
#54101=ORIENTED_EDGE('',*,*,#37882,.T.);
#54102=ORIENTED_EDGE('',*,*,#37887,.T.);
#54103=ORIENTED_EDGE('',*,*,#37888,.F.);
#54104=ORIENTED_EDGE('',*,*,#37889,.T.);
#54105=ORIENTED_EDGE('',*,*,#37885,.T.);
#54106=ORIENTED_EDGE('',*,*,#37890,.T.);
#54107=ORIENTED_EDGE('',*,*,#37891,.F.);
#54108=ORIENTED_EDGE('',*,*,#37892,.T.);
#54109=ORIENTED_EDGE('',*,*,#37888,.T.);
#54110=ORIENTED_EDGE('',*,*,#37893,.T.);
#54111=ORIENTED_EDGE('',*,*,#37894,.F.);
#54112=ORIENTED_EDGE('',*,*,#37895,.T.);
#54113=ORIENTED_EDGE('',*,*,#37891,.T.);
#54114=ORIENTED_EDGE('',*,*,#37896,.T.);
#54115=ORIENTED_EDGE('',*,*,#37897,.F.);
#54116=ORIENTED_EDGE('',*,*,#37898,.T.);
#54117=ORIENTED_EDGE('',*,*,#37894,.T.);
#54118=ORIENTED_EDGE('',*,*,#37899,.T.);
#54119=ORIENTED_EDGE('',*,*,#37900,.F.);
#54120=ORIENTED_EDGE('',*,*,#37901,.T.);
#54121=ORIENTED_EDGE('',*,*,#37897,.T.);
#54122=ORIENTED_EDGE('',*,*,#37902,.T.);
#54123=ORIENTED_EDGE('',*,*,#37903,.F.);
#54124=ORIENTED_EDGE('',*,*,#37904,.T.);
#54125=ORIENTED_EDGE('',*,*,#37900,.T.);
#54126=ORIENTED_EDGE('',*,*,#37905,.T.);
#54127=ORIENTED_EDGE('',*,*,#37906,.F.);
#54128=ORIENTED_EDGE('',*,*,#37907,.T.);
#54129=ORIENTED_EDGE('',*,*,#37903,.T.);
#54130=ORIENTED_EDGE('',*,*,#37908,.T.);
#54131=ORIENTED_EDGE('',*,*,#37909,.F.);
#54132=ORIENTED_EDGE('',*,*,#37910,.T.);
#54133=ORIENTED_EDGE('',*,*,#37906,.T.);
#54134=ORIENTED_EDGE('',*,*,#37911,.T.);
#54135=ORIENTED_EDGE('',*,*,#37912,.F.);
#54136=ORIENTED_EDGE('',*,*,#37913,.T.);
#54137=ORIENTED_EDGE('',*,*,#37914,.F.);
#54138=ORIENTED_EDGE('',*,*,#37915,.F.);
#54139=ORIENTED_EDGE('',*,*,#37916,.F.);
#54140=ORIENTED_EDGE('',*,*,#37917,.T.);
#54141=ORIENTED_EDGE('',*,*,#37912,.T.);
#54142=ORIENTED_EDGE('',*,*,#37918,.F.);
#54143=ORIENTED_EDGE('',*,*,#37919,.F.);
#54144=ORIENTED_EDGE('',*,*,#37920,.T.);
#54145=ORIENTED_EDGE('',*,*,#37916,.T.);
#54146=ORIENTED_EDGE('',*,*,#37921,.F.);
#54147=ORIENTED_EDGE('',*,*,#37922,.F.);
#54148=ORIENTED_EDGE('',*,*,#37923,.T.);
#54149=ORIENTED_EDGE('',*,*,#37919,.T.);
#54150=ORIENTED_EDGE('',*,*,#37924,.F.);
#54151=ORIENTED_EDGE('',*,*,#37925,.F.);
#54152=ORIENTED_EDGE('',*,*,#37926,.T.);
#54153=ORIENTED_EDGE('',*,*,#37922,.T.);
#54154=ORIENTED_EDGE('',*,*,#37927,.F.);
#54155=ORIENTED_EDGE('',*,*,#37928,.F.);
#54156=ORIENTED_EDGE('',*,*,#37929,.T.);
#54157=ORIENTED_EDGE('',*,*,#37925,.T.);
#54158=ORIENTED_EDGE('',*,*,#37930,.F.);
#54159=ORIENTED_EDGE('',*,*,#37931,.F.);
#54160=ORIENTED_EDGE('',*,*,#37932,.T.);
#54161=ORIENTED_EDGE('',*,*,#37928,.T.);
#54162=ORIENTED_EDGE('',*,*,#37933,.F.);
#54163=ORIENTED_EDGE('',*,*,#37934,.F.);
#54164=ORIENTED_EDGE('',*,*,#37935,.T.);
#54165=ORIENTED_EDGE('',*,*,#37931,.T.);
#54166=ORIENTED_EDGE('',*,*,#37936,.F.);
#54167=ORIENTED_EDGE('',*,*,#37937,.F.);
#54168=ORIENTED_EDGE('',*,*,#37938,.T.);
#54169=ORIENTED_EDGE('',*,*,#37934,.T.);
#54170=ORIENTED_EDGE('',*,*,#37939,.F.);
#54171=ORIENTED_EDGE('',*,*,#37940,.F.);
#54172=ORIENTED_EDGE('',*,*,#37941,.T.);
#54173=ORIENTED_EDGE('',*,*,#37937,.T.);
#54174=ORIENTED_EDGE('',*,*,#37942,.F.);
#54175=ORIENTED_EDGE('',*,*,#37914,.T.);
#54176=ORIENTED_EDGE('',*,*,#37943,.T.);
#54177=ORIENTED_EDGE('',*,*,#37944,.F.);
#54178=ORIENTED_EDGE('',*,*,#37945,.F.);
#54179=ORIENTED_EDGE('',*,*,#37946,.T.);
#54180=ORIENTED_EDGE('',*,*,#37946,.F.);
#54181=ORIENTED_EDGE('',*,*,#37947,.F.);
#54182=ORIENTED_EDGE('',*,*,#37911,.F.);
#54183=ORIENTED_EDGE('',*,*,#37908,.F.);
#54184=ORIENTED_EDGE('',*,*,#37905,.F.);
#54185=ORIENTED_EDGE('',*,*,#37902,.F.);
#54186=ORIENTED_EDGE('',*,*,#37899,.F.);
#54187=ORIENTED_EDGE('',*,*,#37896,.F.);
#54188=ORIENTED_EDGE('',*,*,#37893,.F.);
#54189=ORIENTED_EDGE('',*,*,#37890,.F.);
#54190=ORIENTED_EDGE('',*,*,#37887,.F.);
#54191=ORIENTED_EDGE('',*,*,#37884,.F.);
#54192=ORIENTED_EDGE('',*,*,#37881,.F.);
#54193=ORIENTED_EDGE('',*,*,#37948,.F.);
#54194=ORIENTED_EDGE('',*,*,#37949,.T.);
#54195=ORIENTED_EDGE('',*,*,#37942,.T.);
#54196=ORIENTED_EDGE('',*,*,#37939,.T.);
#54197=ORIENTED_EDGE('',*,*,#37936,.T.);
#54198=ORIENTED_EDGE('',*,*,#37933,.T.);
#54199=ORIENTED_EDGE('',*,*,#37930,.T.);
#54200=ORIENTED_EDGE('',*,*,#37927,.T.);
#54201=ORIENTED_EDGE('',*,*,#37924,.T.);
#54202=ORIENTED_EDGE('',*,*,#37921,.T.);
#54203=ORIENTED_EDGE('',*,*,#37918,.T.);
#54204=ORIENTED_EDGE('',*,*,#37915,.T.);
#54205=ORIENTED_EDGE('',*,*,#37950,.F.);
#54206=ORIENTED_EDGE('',*,*,#37951,.T.);
#54207=ORIENTED_EDGE('',*,*,#37952,.T.);
#54208=ORIENTED_EDGE('',*,*,#37948,.T.);
#54209=ORIENTED_EDGE('',*,*,#37953,.F.);
#54210=ORIENTED_EDGE('',*,*,#37940,.T.);
#54211=ORIENTED_EDGE('',*,*,#37949,.F.);
#54212=ORIENTED_EDGE('',*,*,#37952,.F.);
#54213=ORIENTED_EDGE('',*,*,#37954,.T.);
#54214=ORIENTED_EDGE('',*,*,#37943,.F.);
#54215=ORIENTED_EDGE('',*,*,#37913,.F.);
#54216=ORIENTED_EDGE('',*,*,#37917,.F.);
#54217=ORIENTED_EDGE('',*,*,#37920,.F.);
#54218=ORIENTED_EDGE('',*,*,#37923,.F.);
#54219=ORIENTED_EDGE('',*,*,#37926,.F.);
#54220=ORIENTED_EDGE('',*,*,#37929,.F.);
#54221=ORIENTED_EDGE('',*,*,#37932,.F.);
#54222=ORIENTED_EDGE('',*,*,#37935,.F.);
#54223=ORIENTED_EDGE('',*,*,#37938,.F.);
#54224=ORIENTED_EDGE('',*,*,#37941,.F.);
#54225=ORIENTED_EDGE('',*,*,#37954,.F.);
#54226=ORIENTED_EDGE('',*,*,#37951,.F.);
#54227=ORIENTED_EDGE('',*,*,#37879,.F.);
#54228=ORIENTED_EDGE('',*,*,#37883,.F.);
#54229=ORIENTED_EDGE('',*,*,#37886,.F.);
#54230=ORIENTED_EDGE('',*,*,#37889,.F.);
#54231=ORIENTED_EDGE('',*,*,#37892,.F.);
#54232=ORIENTED_EDGE('',*,*,#37895,.F.);
#54233=ORIENTED_EDGE('',*,*,#37898,.F.);
#54234=ORIENTED_EDGE('',*,*,#37901,.F.);
#54235=ORIENTED_EDGE('',*,*,#37904,.F.);
#54236=ORIENTED_EDGE('',*,*,#37907,.F.);
#54237=ORIENTED_EDGE('',*,*,#37910,.F.);
#54238=ORIENTED_EDGE('',*,*,#37955,.F.);
#54239=ORIENTED_EDGE('',*,*,#37956,.T.);
#54240=ORIENTED_EDGE('',*,*,#37957,.T.);
#54241=ORIENTED_EDGE('',*,*,#37953,.T.);
#54242=ORIENTED_EDGE('',*,*,#37880,.T.);
#54243=ORIENTED_EDGE('',*,*,#37950,.T.);
#54244=ORIENTED_EDGE('',*,*,#37957,.F.);
#54245=ORIENTED_EDGE('',*,*,#37958,.T.);
#54246=ORIENTED_EDGE('',*,*,#37956,.F.);
#54247=ORIENTED_EDGE('',*,*,#37909,.T.);
#54248=ORIENTED_EDGE('',*,*,#37947,.T.);
#54249=ORIENTED_EDGE('',*,*,#37959,.F.);
#54250=ORIENTED_EDGE('',*,*,#37955,.T.);
#54251=ORIENTED_EDGE('',*,*,#37960,.F.);
#54252=ORIENTED_EDGE('',*,*,#37961,.T.);
#54253=ORIENTED_EDGE('',*,*,#37962,.F.);
#54254=ORIENTED_EDGE('',*,*,#37963,.F.);
#54255=ORIENTED_EDGE('',*,*,#37964,.F.);
#54256=ORIENTED_EDGE('',*,*,#37965,.F.);
#54257=ORIENTED_EDGE('',*,*,#37966,.F.);
#54258=ORIENTED_EDGE('',*,*,#37967,.F.);
#54259=ORIENTED_EDGE('',*,*,#37968,.F.);
#54260=ORIENTED_EDGE('',*,*,#37969,.F.);
#54261=ORIENTED_EDGE('',*,*,#37970,.F.);
#54262=ORIENTED_EDGE('',*,*,#37971,.T.);
#54263=ORIENTED_EDGE('',*,*,#37972,.F.);
#54264=ORIENTED_EDGE('',*,*,#37971,.F.);
#54265=ORIENTED_EDGE('',*,*,#37973,.F.);
#54266=ORIENTED_EDGE('',*,*,#37974,.F.);
#54267=ORIENTED_EDGE('',*,*,#37961,.F.);
#54268=ORIENTED_EDGE('',*,*,#37967,.T.);
#54269=ORIENTED_EDGE('',*,*,#37975,.F.);
#54270=ORIENTED_EDGE('',*,*,#37969,.T.);
#54271=ORIENTED_EDGE('',*,*,#37976,.T.);
#54272=ORIENTED_EDGE('',*,*,#37965,.T.);
#54273=ORIENTED_EDGE('',*,*,#37977,.T.);
#54274=ORIENTED_EDGE('',*,*,#37963,.T.);
#54275=ORIENTED_EDGE('',*,*,#37978,.F.);
#54276=ORIENTED_EDGE('',*,*,#37968,.T.);
#54277=ORIENTED_EDGE('',*,*,#37976,.F.);
#54278=ORIENTED_EDGE('',*,*,#37964,.T.);
#54279=ORIENTED_EDGE('',*,*,#37977,.F.);
#54280=ORIENTED_EDGE('',*,*,#37958,.F.);
#54281=ORIENTED_EDGE('',*,*,#37979,.T.);
#54282=ORIENTED_EDGE('',*,*,#37973,.T.);
#54283=ORIENTED_EDGE('',*,*,#37970,.T.);
#54284=ORIENTED_EDGE('',*,*,#37975,.T.);
#54285=ORIENTED_EDGE('',*,*,#37966,.T.);
#54286=ORIENTED_EDGE('',*,*,#37972,.T.);
#54287=ORIENTED_EDGE('',*,*,#37960,.T.);
#54288=ORIENTED_EDGE('',*,*,#37978,.T.);
#54289=ORIENTED_EDGE('',*,*,#37962,.T.);
#54290=ORIENTED_EDGE('',*,*,#37974,.T.);
#54291=ORIENTED_EDGE('',*,*,#37979,.F.);
#54292=ORIENTED_EDGE('',*,*,#37980,.F.);
#54293=ORIENTED_EDGE('',*,*,#37981,.T.);
#54294=ORIENTED_EDGE('',*,*,#37944,.T.);
#54295=ORIENTED_EDGE('',*,*,#37959,.T.);
#54296=ORIENTED_EDGE('',*,*,#37945,.T.);
#54297=ORIENTED_EDGE('',*,*,#37981,.F.);
#54298=ORIENTED_EDGE('',*,*,#37980,.T.);
#54299=ORIENTED_EDGE('',*,*,#37982,.F.);
#54300=ORIENTED_EDGE('',*,*,#37983,.T.);
#54301=ORIENTED_EDGE('',*,*,#37984,.T.);
#54302=ORIENTED_EDGE('',*,*,#37985,.T.);
#54303=ORIENTED_EDGE('',*,*,#37986,.F.);
#54304=ORIENTED_EDGE('',*,*,#37987,.T.);
#54305=ORIENTED_EDGE('',*,*,#37982,.T.);
#54306=ORIENTED_EDGE('',*,*,#37988,.T.);
#54307=ORIENTED_EDGE('',*,*,#37989,.F.);
#54308=ORIENTED_EDGE('',*,*,#37990,.T.);
#54309=ORIENTED_EDGE('',*,*,#37986,.T.);
#54310=ORIENTED_EDGE('',*,*,#37991,.T.);
#54311=ORIENTED_EDGE('',*,*,#37992,.F.);
#54312=ORIENTED_EDGE('',*,*,#37993,.T.);
#54313=ORIENTED_EDGE('',*,*,#37989,.T.);
#54314=ORIENTED_EDGE('',*,*,#37994,.T.);
#54315=ORIENTED_EDGE('',*,*,#37995,.F.);
#54316=ORIENTED_EDGE('',*,*,#37996,.T.);
#54317=ORIENTED_EDGE('',*,*,#37992,.T.);
#54318=ORIENTED_EDGE('',*,*,#37997,.T.);
#54319=ORIENTED_EDGE('',*,*,#37998,.F.);
#54320=ORIENTED_EDGE('',*,*,#37999,.T.);
#54321=ORIENTED_EDGE('',*,*,#38000,.F.);
#54322=ORIENTED_EDGE('',*,*,#38001,.F.);
#54323=ORIENTED_EDGE('',*,*,#38002,.F.);
#54324=ORIENTED_EDGE('',*,*,#38003,.T.);
#54325=ORIENTED_EDGE('',*,*,#37998,.T.);
#54326=ORIENTED_EDGE('',*,*,#38004,.F.);
#54327=ORIENTED_EDGE('',*,*,#38005,.F.);
#54328=ORIENTED_EDGE('',*,*,#38006,.T.);
#54329=ORIENTED_EDGE('',*,*,#38002,.T.);
#54330=ORIENTED_EDGE('',*,*,#38007,.F.);
#54331=ORIENTED_EDGE('',*,*,#38008,.F.);
#54332=ORIENTED_EDGE('',*,*,#38009,.T.);
#54333=ORIENTED_EDGE('',*,*,#38005,.T.);
#54334=ORIENTED_EDGE('',*,*,#38010,.F.);
#54335=ORIENTED_EDGE('',*,*,#38000,.T.);
#54336=ORIENTED_EDGE('',*,*,#38011,.T.);
#54337=ORIENTED_EDGE('',*,*,#38012,.F.);
#54338=ORIENTED_EDGE('',*,*,#38013,.F.);
#54339=ORIENTED_EDGE('',*,*,#38014,.T.);
#54340=ORIENTED_EDGE('',*,*,#38014,.F.);
#54341=ORIENTED_EDGE('',*,*,#38015,.F.);
#54342=ORIENTED_EDGE('',*,*,#37997,.F.);
#54343=ORIENTED_EDGE('',*,*,#37994,.F.);
#54344=ORIENTED_EDGE('',*,*,#37991,.F.);
#54345=ORIENTED_EDGE('',*,*,#37988,.F.);
#54346=ORIENTED_EDGE('',*,*,#37985,.F.);
#54347=ORIENTED_EDGE('',*,*,#38016,.F.);
#54348=ORIENTED_EDGE('',*,*,#38017,.T.);
#54349=ORIENTED_EDGE('',*,*,#38010,.T.);
#54350=ORIENTED_EDGE('',*,*,#38007,.T.);
#54351=ORIENTED_EDGE('',*,*,#38004,.T.);
#54352=ORIENTED_EDGE('',*,*,#38001,.T.);
#54353=ORIENTED_EDGE('',*,*,#38018,.T.);
#54354=ORIENTED_EDGE('',*,*,#38019,.T.);
#54355=ORIENTED_EDGE('',*,*,#38020,.T.);
#54356=ORIENTED_EDGE('',*,*,#38021,.T.);
#54357=ORIENTED_EDGE('',*,*,#38016,.T.);
#54358=ORIENTED_EDGE('',*,*,#38008,.T.);
#54359=ORIENTED_EDGE('',*,*,#38017,.F.);
#54360=ORIENTED_EDGE('',*,*,#38021,.F.);
#54361=ORIENTED_EDGE('',*,*,#38022,.T.);
#54362=ORIENTED_EDGE('',*,*,#38011,.F.);
#54363=ORIENTED_EDGE('',*,*,#37999,.F.);
#54364=ORIENTED_EDGE('',*,*,#38003,.F.);
#54365=ORIENTED_EDGE('',*,*,#38006,.F.);
#54366=ORIENTED_EDGE('',*,*,#38009,.F.);
#54367=ORIENTED_EDGE('',*,*,#38022,.F.);
#54368=ORIENTED_EDGE('',*,*,#38020,.F.);
#54369=ORIENTED_EDGE('',*,*,#37983,.F.);
#54370=ORIENTED_EDGE('',*,*,#37987,.F.);
#54371=ORIENTED_EDGE('',*,*,#37990,.F.);
#54372=ORIENTED_EDGE('',*,*,#37993,.F.);
#54373=ORIENTED_EDGE('',*,*,#37996,.F.);
#54374=ORIENTED_EDGE('',*,*,#38023,.F.);
#54375=ORIENTED_EDGE('',*,*,#38024,.F.);
#54376=ORIENTED_EDGE('',*,*,#38025,.T.);
#54377=ORIENTED_EDGE('',*,*,#38026,.F.);
#54378=ORIENTED_EDGE('',*,*,#38027,.T.);
#54379=ORIENTED_EDGE('',*,*,#38028,.F.);
#54380=ORIENTED_EDGE('',*,*,#38029,.F.);
#54381=ORIENTED_EDGE('',*,*,#38030,.T.);
#54382=ORIENTED_EDGE('',*,*,#38031,.F.);
#54383=ORIENTED_EDGE('',*,*,#38032,.F.);
#54384=ORIENTED_EDGE('',*,*,#38033,.T.);
#54385=ORIENTED_EDGE('',*,*,#38034,.F.);
#54386=ORIENTED_EDGE('',*,*,#38035,.F.);
#54387=ORIENTED_EDGE('',*,*,#38036,.T.);
#54388=ORIENTED_EDGE('',*,*,#38037,.F.);
#54389=ORIENTED_EDGE('',*,*,#38038,.F.);
#54390=ORIENTED_EDGE('',*,*,#38039,.T.);
#54391=ORIENTED_EDGE('',*,*,#38040,.F.);
#54392=ORIENTED_EDGE('',*,*,#38041,.F.);
#54393=ORIENTED_EDGE('',*,*,#38042,.T.);
#54394=ORIENTED_EDGE('',*,*,#38043,.F.);
#54395=ORIENTED_EDGE('',*,*,#38025,.F.);
#54396=ORIENTED_EDGE('',*,*,#38044,.F.);
#54397=ORIENTED_EDGE('',*,*,#38030,.F.);
#54398=ORIENTED_EDGE('',*,*,#38045,.F.);
#54399=ORIENTED_EDGE('',*,*,#38046,.F.);
#54400=ORIENTED_EDGE('',*,*,#38047,.F.);
#54401=ORIENTED_EDGE('',*,*,#38033,.F.);
#54402=ORIENTED_EDGE('',*,*,#38048,.F.);
#54403=ORIENTED_EDGE('',*,*,#38049,.F.);
#54404=ORIENTED_EDGE('',*,*,#38050,.F.);
#54405=ORIENTED_EDGE('',*,*,#38051,.F.);
#54406=ORIENTED_EDGE('',*,*,#38052,.F.);
#54407=ORIENTED_EDGE('',*,*,#38027,.F.);
#54408=ORIENTED_EDGE('',*,*,#38053,.F.);
#54409=ORIENTED_EDGE('',*,*,#38036,.F.);
#54410=ORIENTED_EDGE('',*,*,#38054,.F.);
#54411=ORIENTED_EDGE('',*,*,#38055,.F.);
#54412=ORIENTED_EDGE('',*,*,#38056,.F.);
#54413=ORIENTED_EDGE('',*,*,#38057,.F.);
#54414=ORIENTED_EDGE('',*,*,#38058,.F.);
#54415=ORIENTED_EDGE('',*,*,#38042,.F.);
#54416=ORIENTED_EDGE('',*,*,#38059,.F.);
#54417=ORIENTED_EDGE('',*,*,#38060,.F.);
#54418=ORIENTED_EDGE('',*,*,#38061,.F.);
#54419=ORIENTED_EDGE('',*,*,#38039,.F.);
#54420=ORIENTED_EDGE('',*,*,#38037,.T.);
#54421=ORIENTED_EDGE('',*,*,#38053,.T.);
#54422=ORIENTED_EDGE('',*,*,#38062,.F.);
#54423=ORIENTED_EDGE('',*,*,#38054,.T.);
#54424=ORIENTED_EDGE('',*,*,#38035,.T.);
#54425=ORIENTED_EDGE('',*,*,#38063,.T.);
#54426=ORIENTED_EDGE('',*,*,#38064,.T.);
#54427=ORIENTED_EDGE('',*,*,#38065,.F.);
#54428=ORIENTED_EDGE('',*,*,#38034,.T.);
#54429=ORIENTED_EDGE('',*,*,#38047,.T.);
#54430=ORIENTED_EDGE('',*,*,#38066,.F.);
#54431=ORIENTED_EDGE('',*,*,#38048,.T.);
#54432=ORIENTED_EDGE('',*,*,#38032,.T.);
#54433=ORIENTED_EDGE('',*,*,#38067,.T.);
#54434=ORIENTED_EDGE('',*,*,#38068,.T.);
#54435=ORIENTED_EDGE('',*,*,#38063,.F.);
#54436=ORIENTED_EDGE('',*,*,#38031,.T.);
#54437=ORIENTED_EDGE('',*,*,#38044,.T.);
#54438=ORIENTED_EDGE('',*,*,#38069,.F.);
#54439=ORIENTED_EDGE('',*,*,#38045,.T.);
#54440=ORIENTED_EDGE('',*,*,#38029,.T.);
#54441=ORIENTED_EDGE('',*,*,#38070,.T.);
#54442=ORIENTED_EDGE('',*,*,#38071,.T.);
#54443=ORIENTED_EDGE('',*,*,#38067,.F.);
#54444=ORIENTED_EDGE('',*,*,#38046,.T.);
#54445=ORIENTED_EDGE('',*,*,#38069,.T.);
#54446=ORIENTED_EDGE('',*,*,#38049,.T.);
#54447=ORIENTED_EDGE('',*,*,#38066,.T.);
#54448=ORIENTED_EDGE('',*,*,#38051,.T.);
#54449=ORIENTED_EDGE('',*,*,#38072,.T.);
#54450=ORIENTED_EDGE('',*,*,#38055,.T.);
#54451=ORIENTED_EDGE('',*,*,#38062,.T.);
#54452=ORIENTED_EDGE('',*,*,#38057,.T.);
#54453=ORIENTED_EDGE('',*,*,#38073,.T.);
#54454=ORIENTED_EDGE('',*,*,#38060,.T.);
#54455=ORIENTED_EDGE('',*,*,#38074,.T.);
#54456=ORIENTED_EDGE('',*,*,#38075,.F.);
#54457=ORIENTED_EDGE('',*,*,#38076,.T.);
#54458=ORIENTED_EDGE('',*,*,#38071,.F.);
#54459=ORIENTED_EDGE('',*,*,#38077,.T.);
#54460=ORIENTED_EDGE('',*,*,#38068,.F.);
#54461=ORIENTED_EDGE('',*,*,#38078,.T.);
#54462=ORIENTED_EDGE('',*,*,#38064,.F.);
#54463=ORIENTED_EDGE('',*,*,#38079,.T.);
#54464=ORIENTED_EDGE('',*,*,#38080,.F.);
#54465=ORIENTED_EDGE('',*,*,#38081,.T.);
#54466=ORIENTED_EDGE('',*,*,#38082,.F.);
#54467=ORIENTED_EDGE('',*,*,#38083,.T.);
#54468=ORIENTED_EDGE('',*,*,#38079,.F.);
#54469=ORIENTED_EDGE('',*,*,#38078,.F.);
#54470=ORIENTED_EDGE('',*,*,#38077,.F.);
#54471=ORIENTED_EDGE('',*,*,#38076,.F.);
#54472=ORIENTED_EDGE('',*,*,#38084,.T.);
#54473=ORIENTED_EDGE('',*,*,#38084,.F.);
#54474=ORIENTED_EDGE('',*,*,#38083,.F.);
#54475=ORIENTED_EDGE('',*,*,#38081,.F.);
#54476=ORIENTED_EDGE('',*,*,#38026,.T.);
#54477=ORIENTED_EDGE('',*,*,#38085,.T.);
#54478=ORIENTED_EDGE('',*,*,#38075,.T.);
#54479=ORIENTED_EDGE('',*,*,#38070,.F.);
#54480=ORIENTED_EDGE('',*,*,#38028,.T.);
#54481=ORIENTED_EDGE('',*,*,#38052,.T.);
#54482=ORIENTED_EDGE('',*,*,#38072,.F.);
#54483=ORIENTED_EDGE('',*,*,#38050,.T.);
#54484=ORIENTED_EDGE('',*,*,#38041,.T.);
#54485=ORIENTED_EDGE('',*,*,#38086,.T.);
#54486=ORIENTED_EDGE('',*,*,#38082,.T.);
#54487=ORIENTED_EDGE('',*,*,#38085,.F.);
#54488=ORIENTED_EDGE('',*,*,#38043,.T.);
#54489=ORIENTED_EDGE('',*,*,#38058,.T.);
#54490=ORIENTED_EDGE('',*,*,#38073,.F.);
#54491=ORIENTED_EDGE('',*,*,#38056,.T.);
#54492=ORIENTED_EDGE('',*,*,#38038,.T.);
#54493=ORIENTED_EDGE('',*,*,#38065,.T.);
#54494=ORIENTED_EDGE('',*,*,#38080,.T.);
#54495=ORIENTED_EDGE('',*,*,#38086,.F.);
#54496=ORIENTED_EDGE('',*,*,#38040,.T.);
#54497=ORIENTED_EDGE('',*,*,#38061,.T.);
#54498=ORIENTED_EDGE('',*,*,#38074,.F.);
#54499=ORIENTED_EDGE('',*,*,#38059,.T.);
#54500=ORIENTED_EDGE('',*,*,#38087,.F.);
#54501=ORIENTED_EDGE('',*,*,#38024,.T.);
#54502=ORIENTED_EDGE('',*,*,#38018,.F.);
#54503=ORIENTED_EDGE('',*,*,#37984,.F.);
#54504=ORIENTED_EDGE('',*,*,#38019,.F.);
#54505=ORIENTED_EDGE('',*,*,#38088,.T.);
#54506=ORIENTED_EDGE('',*,*,#38087,.T.);
#54507=ORIENTED_EDGE('',*,*,#38088,.F.);
#54508=ORIENTED_EDGE('',*,*,#37995,.T.);
#54509=ORIENTED_EDGE('',*,*,#38015,.T.);
#54510=ORIENTED_EDGE('',*,*,#38089,.F.);
#54511=ORIENTED_EDGE('',*,*,#38023,.T.);
#54512=ORIENTED_EDGE('',*,*,#38090,.F.);
#54513=ORIENTED_EDGE('',*,*,#38091,.T.);
#54514=ORIENTED_EDGE('',*,*,#38012,.T.);
#54515=ORIENTED_EDGE('',*,*,#38089,.T.);
#54516=ORIENTED_EDGE('',*,*,#38013,.T.);
#54517=ORIENTED_EDGE('',*,*,#38091,.F.);
#54518=ORIENTED_EDGE('',*,*,#38090,.T.);
#54519=ORIENTED_EDGE('',*,*,#38092,.F.);
#54520=ORIENTED_EDGE('',*,*,#38093,.T.);
#54521=ORIENTED_EDGE('',*,*,#38094,.T.);
#54522=ORIENTED_EDGE('',*,*,#38095,.T.);
#54523=ORIENTED_EDGE('',*,*,#38096,.F.);
#54524=ORIENTED_EDGE('',*,*,#38097,.T.);
#54525=ORIENTED_EDGE('',*,*,#38092,.T.);
#54526=ORIENTED_EDGE('',*,*,#38098,.T.);
#54527=ORIENTED_EDGE('',*,*,#38099,.F.);
#54528=ORIENTED_EDGE('',*,*,#38100,.T.);
#54529=ORIENTED_EDGE('',*,*,#38096,.T.);
#54530=ORIENTED_EDGE('',*,*,#38101,.T.);
#54531=ORIENTED_EDGE('',*,*,#38102,.F.);
#54532=ORIENTED_EDGE('',*,*,#38103,.F.);
#54533=ORIENTED_EDGE('',*,*,#38104,.T.);
#54534=ORIENTED_EDGE('',*,*,#38099,.T.);
#54535=ORIENTED_EDGE('',*,*,#38105,.T.);
#54536=ORIENTED_EDGE('',*,*,#38106,.F.);
#54537=ORIENTED_EDGE('',*,*,#38107,.T.);
#54538=ORIENTED_EDGE('',*,*,#38108,.F.);
#54539=ORIENTED_EDGE('',*,*,#38109,.F.);
#54540=ORIENTED_EDGE('',*,*,#38110,.F.);
#54541=ORIENTED_EDGE('',*,*,#38111,.T.);
#54542=ORIENTED_EDGE('',*,*,#38106,.T.);
#54543=ORIENTED_EDGE('',*,*,#38112,.F.);
#54544=ORIENTED_EDGE('',*,*,#38113,.F.);
#54545=ORIENTED_EDGE('',*,*,#38114,.T.);
#54546=ORIENTED_EDGE('',*,*,#38110,.T.);
#54547=ORIENTED_EDGE('',*,*,#38115,.F.);
#54548=ORIENTED_EDGE('',*,*,#38108,.T.);
#54549=ORIENTED_EDGE('',*,*,#38116,.T.);
#54550=ORIENTED_EDGE('',*,*,#38117,.F.);
#54551=ORIENTED_EDGE('',*,*,#38118,.T.);
#54552=ORIENTED_EDGE('',*,*,#38118,.F.);
#54553=ORIENTED_EDGE('',*,*,#38119,.F.);
#54554=ORIENTED_EDGE('',*,*,#38105,.F.);
#54555=ORIENTED_EDGE('',*,*,#38101,.F.);
#54556=ORIENTED_EDGE('',*,*,#38098,.F.);
#54557=ORIENTED_EDGE('',*,*,#38095,.F.);
#54558=ORIENTED_EDGE('',*,*,#38120,.F.);
#54559=ORIENTED_EDGE('',*,*,#38121,.T.);
#54560=ORIENTED_EDGE('',*,*,#38115,.T.);
#54561=ORIENTED_EDGE('',*,*,#38112,.T.);
#54562=ORIENTED_EDGE('',*,*,#38109,.T.);
#54563=ORIENTED_EDGE('',*,*,#38122,.T.);
#54564=ORIENTED_EDGE('',*,*,#38123,.T.);
#54565=ORIENTED_EDGE('',*,*,#38124,.T.);
#54566=ORIENTED_EDGE('',*,*,#38125,.T.);
#54567=ORIENTED_EDGE('',*,*,#38120,.T.);
#54568=ORIENTED_EDGE('',*,*,#38113,.T.);
#54569=ORIENTED_EDGE('',*,*,#38121,.F.);
#54570=ORIENTED_EDGE('',*,*,#38125,.F.);
#54571=ORIENTED_EDGE('',*,*,#38126,.T.);
#54572=ORIENTED_EDGE('',*,*,#38116,.F.);
#54573=ORIENTED_EDGE('',*,*,#38107,.F.);
#54574=ORIENTED_EDGE('',*,*,#38111,.F.);
#54575=ORIENTED_EDGE('',*,*,#38114,.F.);
#54576=ORIENTED_EDGE('',*,*,#38126,.F.);
#54577=ORIENTED_EDGE('',*,*,#38124,.F.);
#54578=ORIENTED_EDGE('',*,*,#38093,.F.);
#54579=ORIENTED_EDGE('',*,*,#38097,.F.);
#54580=ORIENTED_EDGE('',*,*,#38100,.F.);
#54581=ORIENTED_EDGE('',*,*,#38104,.F.);
#54582=ORIENTED_EDGE('',*,*,#38127,.F.);
#54583=ORIENTED_EDGE('',*,*,#38128,.T.);
#54584=ORIENTED_EDGE('',*,*,#38129,.F.);
#54585=ORIENTED_EDGE('',*,*,#38130,.T.);
#54586=ORIENTED_EDGE('',*,*,#38131,.F.);
#54587=ORIENTED_EDGE('',*,*,#38132,.F.);
#54588=ORIENTED_EDGE('',*,*,#38133,.T.);
#54589=ORIENTED_EDGE('',*,*,#38134,.F.);
#54590=ORIENTED_EDGE('',*,*,#38135,.F.);
#54591=ORIENTED_EDGE('',*,*,#38136,.T.);
#54592=ORIENTED_EDGE('',*,*,#38137,.F.);
#54593=ORIENTED_EDGE('',*,*,#38138,.F.);
#54594=ORIENTED_EDGE('',*,*,#38139,.T.);
#54595=ORIENTED_EDGE('',*,*,#38140,.F.);
#54596=ORIENTED_EDGE('',*,*,#38141,.F.);
#54597=ORIENTED_EDGE('',*,*,#38142,.T.);
#54598=ORIENTED_EDGE('',*,*,#38143,.F.);
#54599=ORIENTED_EDGE('',*,*,#38144,.F.);
#54600=ORIENTED_EDGE('',*,*,#38145,.T.);
#54601=ORIENTED_EDGE('',*,*,#38146,.F.);
#54602=ORIENTED_EDGE('',*,*,#38128,.F.);
#54603=ORIENTED_EDGE('',*,*,#38147,.F.);
#54604=ORIENTED_EDGE('',*,*,#38133,.F.);
#54605=ORIENTED_EDGE('',*,*,#38148,.F.);
#54606=ORIENTED_EDGE('',*,*,#38149,.F.);
#54607=ORIENTED_EDGE('',*,*,#38150,.F.);
#54608=ORIENTED_EDGE('',*,*,#38136,.F.);
#54609=ORIENTED_EDGE('',*,*,#38151,.F.);
#54610=ORIENTED_EDGE('',*,*,#38152,.F.);
#54611=ORIENTED_EDGE('',*,*,#38153,.F.);
#54612=ORIENTED_EDGE('',*,*,#38154,.F.);
#54613=ORIENTED_EDGE('',*,*,#38155,.F.);
#54614=ORIENTED_EDGE('',*,*,#38130,.F.);
#54615=ORIENTED_EDGE('',*,*,#38156,.F.);
#54616=ORIENTED_EDGE('',*,*,#38139,.F.);
#54617=ORIENTED_EDGE('',*,*,#38157,.F.);
#54618=ORIENTED_EDGE('',*,*,#38158,.F.);
#54619=ORIENTED_EDGE('',*,*,#38159,.F.);
#54620=ORIENTED_EDGE('',*,*,#38160,.F.);
#54621=ORIENTED_EDGE('',*,*,#38161,.F.);
#54622=ORIENTED_EDGE('',*,*,#38145,.F.);
#54623=ORIENTED_EDGE('',*,*,#38162,.F.);
#54624=ORIENTED_EDGE('',*,*,#38163,.F.);
#54625=ORIENTED_EDGE('',*,*,#38164,.F.);
#54626=ORIENTED_EDGE('',*,*,#38142,.F.);
#54627=ORIENTED_EDGE('',*,*,#38140,.T.);
#54628=ORIENTED_EDGE('',*,*,#38156,.T.);
#54629=ORIENTED_EDGE('',*,*,#38165,.F.);
#54630=ORIENTED_EDGE('',*,*,#38157,.T.);
#54631=ORIENTED_EDGE('',*,*,#38138,.T.);
#54632=ORIENTED_EDGE('',*,*,#38166,.T.);
#54633=ORIENTED_EDGE('',*,*,#38167,.T.);
#54634=ORIENTED_EDGE('',*,*,#38168,.F.);
#54635=ORIENTED_EDGE('',*,*,#38137,.T.);
#54636=ORIENTED_EDGE('',*,*,#38150,.T.);
#54637=ORIENTED_EDGE('',*,*,#38169,.F.);
#54638=ORIENTED_EDGE('',*,*,#38151,.T.);
#54639=ORIENTED_EDGE('',*,*,#38135,.T.);
#54640=ORIENTED_EDGE('',*,*,#38170,.T.);
#54641=ORIENTED_EDGE('',*,*,#38171,.T.);
#54642=ORIENTED_EDGE('',*,*,#38166,.F.);
#54643=ORIENTED_EDGE('',*,*,#38134,.T.);
#54644=ORIENTED_EDGE('',*,*,#38147,.T.);
#54645=ORIENTED_EDGE('',*,*,#38172,.F.);
#54646=ORIENTED_EDGE('',*,*,#38148,.T.);
#54647=ORIENTED_EDGE('',*,*,#38132,.T.);
#54648=ORIENTED_EDGE('',*,*,#38173,.T.);
#54649=ORIENTED_EDGE('',*,*,#38174,.T.);
#54650=ORIENTED_EDGE('',*,*,#38170,.F.);
#54651=ORIENTED_EDGE('',*,*,#38149,.T.);
#54652=ORIENTED_EDGE('',*,*,#38172,.T.);
#54653=ORIENTED_EDGE('',*,*,#38152,.T.);
#54654=ORIENTED_EDGE('',*,*,#38169,.T.);
#54655=ORIENTED_EDGE('',*,*,#38154,.T.);
#54656=ORIENTED_EDGE('',*,*,#38175,.T.);
#54657=ORIENTED_EDGE('',*,*,#38158,.T.);
#54658=ORIENTED_EDGE('',*,*,#38165,.T.);
#54659=ORIENTED_EDGE('',*,*,#38160,.T.);
#54660=ORIENTED_EDGE('',*,*,#38176,.T.);
#54661=ORIENTED_EDGE('',*,*,#38163,.T.);
#54662=ORIENTED_EDGE('',*,*,#38177,.T.);
#54663=ORIENTED_EDGE('',*,*,#38178,.F.);
#54664=ORIENTED_EDGE('',*,*,#38179,.T.);
#54665=ORIENTED_EDGE('',*,*,#38174,.F.);
#54666=ORIENTED_EDGE('',*,*,#38180,.T.);
#54667=ORIENTED_EDGE('',*,*,#38171,.F.);
#54668=ORIENTED_EDGE('',*,*,#38181,.T.);
#54669=ORIENTED_EDGE('',*,*,#38167,.F.);
#54670=ORIENTED_EDGE('',*,*,#38182,.T.);
#54671=ORIENTED_EDGE('',*,*,#38183,.F.);
#54672=ORIENTED_EDGE('',*,*,#38184,.T.);
#54673=ORIENTED_EDGE('',*,*,#38185,.F.);
#54674=ORIENTED_EDGE('',*,*,#38186,.T.);
#54675=ORIENTED_EDGE('',*,*,#38182,.F.);
#54676=ORIENTED_EDGE('',*,*,#38181,.F.);
#54677=ORIENTED_EDGE('',*,*,#38180,.F.);
#54678=ORIENTED_EDGE('',*,*,#38179,.F.);
#54679=ORIENTED_EDGE('',*,*,#38187,.T.);
#54680=ORIENTED_EDGE('',*,*,#38187,.F.);
#54681=ORIENTED_EDGE('',*,*,#38186,.F.);
#54682=ORIENTED_EDGE('',*,*,#38184,.F.);
#54683=ORIENTED_EDGE('',*,*,#38129,.T.);
#54684=ORIENTED_EDGE('',*,*,#38188,.T.);
#54685=ORIENTED_EDGE('',*,*,#38178,.T.);
#54686=ORIENTED_EDGE('',*,*,#38173,.F.);
#54687=ORIENTED_EDGE('',*,*,#38131,.T.);
#54688=ORIENTED_EDGE('',*,*,#38155,.T.);
#54689=ORIENTED_EDGE('',*,*,#38175,.F.);
#54690=ORIENTED_EDGE('',*,*,#38153,.T.);
#54691=ORIENTED_EDGE('',*,*,#38144,.T.);
#54692=ORIENTED_EDGE('',*,*,#38189,.T.);
#54693=ORIENTED_EDGE('',*,*,#38185,.T.);
#54694=ORIENTED_EDGE('',*,*,#38188,.F.);
#54695=ORIENTED_EDGE('',*,*,#38146,.T.);
#54696=ORIENTED_EDGE('',*,*,#38161,.T.);
#54697=ORIENTED_EDGE('',*,*,#38176,.F.);
#54698=ORIENTED_EDGE('',*,*,#38159,.T.);
#54699=ORIENTED_EDGE('',*,*,#38141,.T.);
#54700=ORIENTED_EDGE('',*,*,#38168,.T.);
#54701=ORIENTED_EDGE('',*,*,#38183,.T.);
#54702=ORIENTED_EDGE('',*,*,#38189,.F.);
#54703=ORIENTED_EDGE('',*,*,#38143,.T.);
#54704=ORIENTED_EDGE('',*,*,#38164,.T.);
#54705=ORIENTED_EDGE('',*,*,#38177,.F.);
#54706=ORIENTED_EDGE('',*,*,#38162,.T.);
#54707=ORIENTED_EDGE('',*,*,#38190,.F.);
#54708=ORIENTED_EDGE('',*,*,#38127,.T.);
#54709=ORIENTED_EDGE('',*,*,#38122,.F.);
#54710=ORIENTED_EDGE('',*,*,#38094,.F.);
#54711=ORIENTED_EDGE('',*,*,#38123,.F.);
#54712=ORIENTED_EDGE('',*,*,#38191,.T.);
#54713=ORIENTED_EDGE('',*,*,#38190,.T.);
#54714=ORIENTED_EDGE('',*,*,#38191,.F.);
#54715=ORIENTED_EDGE('',*,*,#38102,.T.);
#54716=ORIENTED_EDGE('',*,*,#38119,.T.);
#54717=ORIENTED_EDGE('',*,*,#38192,.F.);
#54718=ORIENTED_EDGE('',*,*,#38193,.F.);
#54719=ORIENTED_EDGE('',*,*,#38194,.T.);
#54720=ORIENTED_EDGE('',*,*,#38192,.T.);
#54721=ORIENTED_EDGE('',*,*,#38117,.T.);
#54722=ORIENTED_EDGE('',*,*,#38103,.T.);
#54723=ORIENTED_EDGE('',*,*,#38194,.F.);
#54724=ORIENTED_EDGE('',*,*,#38193,.T.);
#54725=ORIENTED_EDGE('',*,*,#38195,.F.);
#54726=ORIENTED_EDGE('',*,*,#38196,.T.);
#54727=ORIENTED_EDGE('',*,*,#38197,.T.);
#54728=ORIENTED_EDGE('',*,*,#38198,.T.);
#54729=ORIENTED_EDGE('',*,*,#38199,.F.);
#54730=ORIENTED_EDGE('',*,*,#38200,.T.);
#54731=ORIENTED_EDGE('',*,*,#38195,.T.);
#54732=ORIENTED_EDGE('',*,*,#38201,.T.);
#54733=ORIENTED_EDGE('',*,*,#38202,.F.);
#54734=ORIENTED_EDGE('',*,*,#38203,.T.);
#54735=ORIENTED_EDGE('',*,*,#38199,.T.);
#54736=ORIENTED_EDGE('',*,*,#38204,.T.);
#54737=ORIENTED_EDGE('',*,*,#38205,.F.);
#54738=ORIENTED_EDGE('',*,*,#38206,.T.);
#54739=ORIENTED_EDGE('',*,*,#38202,.T.);
#54740=ORIENTED_EDGE('',*,*,#38207,.T.);
#54741=ORIENTED_EDGE('',*,*,#38208,.F.);
#54742=ORIENTED_EDGE('',*,*,#38209,.T.);
#54743=ORIENTED_EDGE('',*,*,#38205,.T.);
#54744=ORIENTED_EDGE('',*,*,#38210,.T.);
#54745=ORIENTED_EDGE('',*,*,#38211,.F.);
#54746=ORIENTED_EDGE('',*,*,#38212,.T.);
#54747=ORIENTED_EDGE('',*,*,#38208,.T.);
#54748=ORIENTED_EDGE('',*,*,#38213,.T.);
#54749=ORIENTED_EDGE('',*,*,#38214,.F.);
#54750=ORIENTED_EDGE('',*,*,#38215,.T.);
#54751=ORIENTED_EDGE('',*,*,#38211,.T.);
#54752=ORIENTED_EDGE('',*,*,#38216,.T.);
#54753=ORIENTED_EDGE('',*,*,#38217,.F.);
#54754=ORIENTED_EDGE('',*,*,#38218,.T.);
#54755=ORIENTED_EDGE('',*,*,#38214,.T.);
#54756=ORIENTED_EDGE('',*,*,#38219,.T.);
#54757=ORIENTED_EDGE('',*,*,#38220,.F.);
#54758=ORIENTED_EDGE('',*,*,#38221,.T.);
#54759=ORIENTED_EDGE('',*,*,#38217,.T.);
#54760=ORIENTED_EDGE('',*,*,#38222,.T.);
#54761=ORIENTED_EDGE('',*,*,#38223,.F.);
#54762=ORIENTED_EDGE('',*,*,#38224,.T.);
#54763=ORIENTED_EDGE('',*,*,#38220,.T.);
#54764=ORIENTED_EDGE('',*,*,#38225,.T.);
#54765=ORIENTED_EDGE('',*,*,#38226,.F.);
#54766=ORIENTED_EDGE('',*,*,#38227,.T.);
#54767=ORIENTED_EDGE('',*,*,#38223,.T.);
#54768=ORIENTED_EDGE('',*,*,#38228,.T.);
#54769=ORIENTED_EDGE('',*,*,#38229,.F.);
#54770=ORIENTED_EDGE('',*,*,#38230,.T.);
#54771=ORIENTED_EDGE('',*,*,#38231,.F.);
#54772=ORIENTED_EDGE('',*,*,#38232,.F.);
#54773=ORIENTED_EDGE('',*,*,#38233,.F.);
#54774=ORIENTED_EDGE('',*,*,#38234,.T.);
#54775=ORIENTED_EDGE('',*,*,#38229,.T.);
#54776=ORIENTED_EDGE('',*,*,#38235,.F.);
#54777=ORIENTED_EDGE('',*,*,#38236,.F.);
#54778=ORIENTED_EDGE('',*,*,#38237,.T.);
#54779=ORIENTED_EDGE('',*,*,#38233,.T.);
#54780=ORIENTED_EDGE('',*,*,#38238,.F.);
#54781=ORIENTED_EDGE('',*,*,#38239,.F.);
#54782=ORIENTED_EDGE('',*,*,#38240,.T.);
#54783=ORIENTED_EDGE('',*,*,#38236,.T.);
#54784=ORIENTED_EDGE('',*,*,#38241,.F.);
#54785=ORIENTED_EDGE('',*,*,#38242,.F.);
#54786=ORIENTED_EDGE('',*,*,#38243,.T.);
#54787=ORIENTED_EDGE('',*,*,#38239,.T.);
#54788=ORIENTED_EDGE('',*,*,#38244,.F.);
#54789=ORIENTED_EDGE('',*,*,#38245,.F.);
#54790=ORIENTED_EDGE('',*,*,#38246,.T.);
#54791=ORIENTED_EDGE('',*,*,#38242,.T.);
#54792=ORIENTED_EDGE('',*,*,#38247,.F.);
#54793=ORIENTED_EDGE('',*,*,#38248,.F.);
#54794=ORIENTED_EDGE('',*,*,#38249,.T.);
#54795=ORIENTED_EDGE('',*,*,#38245,.T.);
#54796=ORIENTED_EDGE('',*,*,#38250,.F.);
#54797=ORIENTED_EDGE('',*,*,#38251,.F.);
#54798=ORIENTED_EDGE('',*,*,#38252,.T.);
#54799=ORIENTED_EDGE('',*,*,#38248,.T.);
#54800=ORIENTED_EDGE('',*,*,#38253,.F.);
#54801=ORIENTED_EDGE('',*,*,#38254,.F.);
#54802=ORIENTED_EDGE('',*,*,#38255,.T.);
#54803=ORIENTED_EDGE('',*,*,#38251,.T.);
#54804=ORIENTED_EDGE('',*,*,#38256,.F.);
#54805=ORIENTED_EDGE('',*,*,#38257,.F.);
#54806=ORIENTED_EDGE('',*,*,#38258,.T.);
#54807=ORIENTED_EDGE('',*,*,#38254,.T.);
#54808=ORIENTED_EDGE('',*,*,#38259,.F.);
#54809=ORIENTED_EDGE('',*,*,#38231,.T.);
#54810=ORIENTED_EDGE('',*,*,#38260,.T.);
#54811=ORIENTED_EDGE('',*,*,#38261,.F.);
#54812=ORIENTED_EDGE('',*,*,#38262,.F.);
#54813=ORIENTED_EDGE('',*,*,#38263,.T.);
#54814=ORIENTED_EDGE('',*,*,#38263,.F.);
#54815=ORIENTED_EDGE('',*,*,#38264,.F.);
#54816=ORIENTED_EDGE('',*,*,#38228,.F.);
#54817=ORIENTED_EDGE('',*,*,#38225,.F.);
#54818=ORIENTED_EDGE('',*,*,#38222,.F.);
#54819=ORIENTED_EDGE('',*,*,#38219,.F.);
#54820=ORIENTED_EDGE('',*,*,#38216,.F.);
#54821=ORIENTED_EDGE('',*,*,#38213,.F.);
#54822=ORIENTED_EDGE('',*,*,#38210,.F.);
#54823=ORIENTED_EDGE('',*,*,#38207,.F.);
#54824=ORIENTED_EDGE('',*,*,#38204,.F.);
#54825=ORIENTED_EDGE('',*,*,#38201,.F.);
#54826=ORIENTED_EDGE('',*,*,#38198,.F.);
#54827=ORIENTED_EDGE('',*,*,#38265,.F.);
#54828=ORIENTED_EDGE('',*,*,#38266,.T.);
#54829=ORIENTED_EDGE('',*,*,#38259,.T.);
#54830=ORIENTED_EDGE('',*,*,#38256,.T.);
#54831=ORIENTED_EDGE('',*,*,#38253,.T.);
#54832=ORIENTED_EDGE('',*,*,#38250,.T.);
#54833=ORIENTED_EDGE('',*,*,#38247,.T.);
#54834=ORIENTED_EDGE('',*,*,#38244,.T.);
#54835=ORIENTED_EDGE('',*,*,#38241,.T.);
#54836=ORIENTED_EDGE('',*,*,#38238,.T.);
#54837=ORIENTED_EDGE('',*,*,#38235,.T.);
#54838=ORIENTED_EDGE('',*,*,#38232,.T.);
#54839=ORIENTED_EDGE('',*,*,#38267,.T.);
#54840=ORIENTED_EDGE('',*,*,#38268,.T.);
#54841=ORIENTED_EDGE('',*,*,#38269,.T.);
#54842=ORIENTED_EDGE('',*,*,#38270,.T.);
#54843=ORIENTED_EDGE('',*,*,#38265,.T.);
#54844=ORIENTED_EDGE('',*,*,#38257,.T.);
#54845=ORIENTED_EDGE('',*,*,#38266,.F.);
#54846=ORIENTED_EDGE('',*,*,#38270,.F.);
#54847=ORIENTED_EDGE('',*,*,#38271,.T.);
#54848=ORIENTED_EDGE('',*,*,#38260,.F.);
#54849=ORIENTED_EDGE('',*,*,#38230,.F.);
#54850=ORIENTED_EDGE('',*,*,#38234,.F.);
#54851=ORIENTED_EDGE('',*,*,#38237,.F.);
#54852=ORIENTED_EDGE('',*,*,#38240,.F.);
#54853=ORIENTED_EDGE('',*,*,#38243,.F.);
#54854=ORIENTED_EDGE('',*,*,#38246,.F.);
#54855=ORIENTED_EDGE('',*,*,#38249,.F.);
#54856=ORIENTED_EDGE('',*,*,#38252,.F.);
#54857=ORIENTED_EDGE('',*,*,#38255,.F.);
#54858=ORIENTED_EDGE('',*,*,#38258,.F.);
#54859=ORIENTED_EDGE('',*,*,#38271,.F.);
#54860=ORIENTED_EDGE('',*,*,#38269,.F.);
#54861=ORIENTED_EDGE('',*,*,#38196,.F.);
#54862=ORIENTED_EDGE('',*,*,#38200,.F.);
#54863=ORIENTED_EDGE('',*,*,#38203,.F.);
#54864=ORIENTED_EDGE('',*,*,#38206,.F.);
#54865=ORIENTED_EDGE('',*,*,#38209,.F.);
#54866=ORIENTED_EDGE('',*,*,#38212,.F.);
#54867=ORIENTED_EDGE('',*,*,#38215,.F.);
#54868=ORIENTED_EDGE('',*,*,#38218,.F.);
#54869=ORIENTED_EDGE('',*,*,#38221,.F.);
#54870=ORIENTED_EDGE('',*,*,#38224,.F.);
#54871=ORIENTED_EDGE('',*,*,#38227,.F.);
#54872=ORIENTED_EDGE('',*,*,#38272,.F.);
#54873=ORIENTED_EDGE('',*,*,#38273,.F.);
#54874=ORIENTED_EDGE('',*,*,#38274,.T.);
#54875=ORIENTED_EDGE('',*,*,#38275,.F.);
#54876=ORIENTED_EDGE('',*,*,#38276,.T.);
#54877=ORIENTED_EDGE('',*,*,#38277,.F.);
#54878=ORIENTED_EDGE('',*,*,#38278,.F.);
#54879=ORIENTED_EDGE('',*,*,#38279,.T.);
#54880=ORIENTED_EDGE('',*,*,#38280,.F.);
#54881=ORIENTED_EDGE('',*,*,#38281,.F.);
#54882=ORIENTED_EDGE('',*,*,#38282,.T.);
#54883=ORIENTED_EDGE('',*,*,#38283,.F.);
#54884=ORIENTED_EDGE('',*,*,#38284,.F.);
#54885=ORIENTED_EDGE('',*,*,#38285,.T.);
#54886=ORIENTED_EDGE('',*,*,#38286,.F.);
#54887=ORIENTED_EDGE('',*,*,#38287,.F.);
#54888=ORIENTED_EDGE('',*,*,#38288,.T.);
#54889=ORIENTED_EDGE('',*,*,#38289,.F.);
#54890=ORIENTED_EDGE('',*,*,#38290,.F.);
#54891=ORIENTED_EDGE('',*,*,#38291,.T.);
#54892=ORIENTED_EDGE('',*,*,#38292,.F.);
#54893=ORIENTED_EDGE('',*,*,#38274,.F.);
#54894=ORIENTED_EDGE('',*,*,#38293,.F.);
#54895=ORIENTED_EDGE('',*,*,#38282,.F.);
#54896=ORIENTED_EDGE('',*,*,#38294,.F.);
#54897=ORIENTED_EDGE('',*,*,#38295,.F.);
#54898=ORIENTED_EDGE('',*,*,#38296,.F.);
#54899=ORIENTED_EDGE('',*,*,#38285,.F.);
#54900=ORIENTED_EDGE('',*,*,#38297,.F.);
#54901=ORIENTED_EDGE('',*,*,#38298,.F.);
#54902=ORIENTED_EDGE('',*,*,#38299,.F.);
#54903=ORIENTED_EDGE('',*,*,#38300,.F.);
#54904=ORIENTED_EDGE('',*,*,#38301,.F.);
#54905=ORIENTED_EDGE('',*,*,#38279,.F.);
#54906=ORIENTED_EDGE('',*,*,#38302,.F.);
#54907=ORIENTED_EDGE('',*,*,#38288,.F.);
#54908=ORIENTED_EDGE('',*,*,#38303,.F.);
#54909=ORIENTED_EDGE('',*,*,#38304,.F.);
#54910=ORIENTED_EDGE('',*,*,#38305,.F.);
#54911=ORIENTED_EDGE('',*,*,#38306,.F.);
#54912=ORIENTED_EDGE('',*,*,#38307,.F.);
#54913=ORIENTED_EDGE('',*,*,#38276,.F.);
#54914=ORIENTED_EDGE('',*,*,#38308,.F.);
#54915=ORIENTED_EDGE('',*,*,#38309,.F.);
#54916=ORIENTED_EDGE('',*,*,#38310,.F.);
#54917=ORIENTED_EDGE('',*,*,#38291,.F.);
#54918=ORIENTED_EDGE('',*,*,#38289,.T.);
#54919=ORIENTED_EDGE('',*,*,#38302,.T.);
#54920=ORIENTED_EDGE('',*,*,#38311,.F.);
#54921=ORIENTED_EDGE('',*,*,#38303,.T.);
#54922=ORIENTED_EDGE('',*,*,#38287,.T.);
#54923=ORIENTED_EDGE('',*,*,#38312,.T.);
#54924=ORIENTED_EDGE('',*,*,#38313,.T.);
#54925=ORIENTED_EDGE('',*,*,#38314,.F.);
#54926=ORIENTED_EDGE('',*,*,#38286,.T.);
#54927=ORIENTED_EDGE('',*,*,#38296,.T.);
#54928=ORIENTED_EDGE('',*,*,#38315,.F.);
#54929=ORIENTED_EDGE('',*,*,#38297,.T.);
#54930=ORIENTED_EDGE('',*,*,#38284,.T.);
#54931=ORIENTED_EDGE('',*,*,#38316,.T.);
#54932=ORIENTED_EDGE('',*,*,#38317,.T.);
#54933=ORIENTED_EDGE('',*,*,#38312,.F.);
#54934=ORIENTED_EDGE('',*,*,#38283,.T.);
#54935=ORIENTED_EDGE('',*,*,#38293,.T.);
#54936=ORIENTED_EDGE('',*,*,#38318,.F.);
#54937=ORIENTED_EDGE('',*,*,#38294,.T.);
#54938=ORIENTED_EDGE('',*,*,#38281,.T.);
#54939=ORIENTED_EDGE('',*,*,#38319,.T.);
#54940=ORIENTED_EDGE('',*,*,#38320,.T.);
#54941=ORIENTED_EDGE('',*,*,#38316,.F.);
#54942=ORIENTED_EDGE('',*,*,#38295,.T.);
#54943=ORIENTED_EDGE('',*,*,#38318,.T.);
#54944=ORIENTED_EDGE('',*,*,#38298,.T.);
#54945=ORIENTED_EDGE('',*,*,#38315,.T.);
#54946=ORIENTED_EDGE('',*,*,#38300,.T.);
#54947=ORIENTED_EDGE('',*,*,#38321,.T.);
#54948=ORIENTED_EDGE('',*,*,#38304,.T.);
#54949=ORIENTED_EDGE('',*,*,#38311,.T.);
#54950=ORIENTED_EDGE('',*,*,#38306,.T.);
#54951=ORIENTED_EDGE('',*,*,#38322,.T.);
#54952=ORIENTED_EDGE('',*,*,#38309,.T.);
#54953=ORIENTED_EDGE('',*,*,#38323,.T.);
#54954=ORIENTED_EDGE('',*,*,#38324,.F.);
#54955=ORIENTED_EDGE('',*,*,#38325,.T.);
#54956=ORIENTED_EDGE('',*,*,#38320,.F.);
#54957=ORIENTED_EDGE('',*,*,#38326,.T.);
#54958=ORIENTED_EDGE('',*,*,#38317,.F.);
#54959=ORIENTED_EDGE('',*,*,#38327,.T.);
#54960=ORIENTED_EDGE('',*,*,#38313,.F.);
#54961=ORIENTED_EDGE('',*,*,#38328,.T.);
#54962=ORIENTED_EDGE('',*,*,#38329,.F.);
#54963=ORIENTED_EDGE('',*,*,#38330,.T.);
#54964=ORIENTED_EDGE('',*,*,#38331,.F.);
#54965=ORIENTED_EDGE('',*,*,#38332,.T.);
#54966=ORIENTED_EDGE('',*,*,#38327,.F.);
#54967=ORIENTED_EDGE('',*,*,#38326,.F.);
#54968=ORIENTED_EDGE('',*,*,#38325,.F.);
#54969=ORIENTED_EDGE('',*,*,#38332,.F.);
#54970=ORIENTED_EDGE('',*,*,#38333,.T.);
#54971=ORIENTED_EDGE('',*,*,#38333,.F.);
#54972=ORIENTED_EDGE('',*,*,#38330,.F.);
#54973=ORIENTED_EDGE('',*,*,#38328,.F.);
#54974=ORIENTED_EDGE('',*,*,#38278,.T.);
#54975=ORIENTED_EDGE('',*,*,#38334,.T.);
#54976=ORIENTED_EDGE('',*,*,#38324,.T.);
#54977=ORIENTED_EDGE('',*,*,#38319,.F.);
#54978=ORIENTED_EDGE('',*,*,#38280,.T.);
#54979=ORIENTED_EDGE('',*,*,#38301,.T.);
#54980=ORIENTED_EDGE('',*,*,#38321,.F.);
#54981=ORIENTED_EDGE('',*,*,#38299,.T.);
#54982=ORIENTED_EDGE('',*,*,#38275,.T.);
#54983=ORIENTED_EDGE('',*,*,#38335,.T.);
#54984=ORIENTED_EDGE('',*,*,#38331,.T.);
#54985=ORIENTED_EDGE('',*,*,#38334,.F.);
#54986=ORIENTED_EDGE('',*,*,#38277,.T.);
#54987=ORIENTED_EDGE('',*,*,#38307,.T.);
#54988=ORIENTED_EDGE('',*,*,#38322,.F.);
#54989=ORIENTED_EDGE('',*,*,#38305,.T.);
#54990=ORIENTED_EDGE('',*,*,#38290,.T.);
#54991=ORIENTED_EDGE('',*,*,#38314,.T.);
#54992=ORIENTED_EDGE('',*,*,#38329,.T.);
#54993=ORIENTED_EDGE('',*,*,#38335,.F.);
#54994=ORIENTED_EDGE('',*,*,#38292,.T.);
#54995=ORIENTED_EDGE('',*,*,#38310,.T.);
#54996=ORIENTED_EDGE('',*,*,#38323,.F.);
#54997=ORIENTED_EDGE('',*,*,#38308,.T.);
#54998=ORIENTED_EDGE('',*,*,#38336,.F.);
#54999=ORIENTED_EDGE('',*,*,#38273,.T.);
#55000=ORIENTED_EDGE('',*,*,#38267,.F.);
#55001=ORIENTED_EDGE('',*,*,#38197,.F.);
#55002=ORIENTED_EDGE('',*,*,#38268,.F.);
#55003=ORIENTED_EDGE('',*,*,#38337,.T.);
#55004=ORIENTED_EDGE('',*,*,#38336,.T.);
#55005=ORIENTED_EDGE('',*,*,#38337,.F.);
#55006=ORIENTED_EDGE('',*,*,#38226,.T.);
#55007=ORIENTED_EDGE('',*,*,#38264,.T.);
#55008=ORIENTED_EDGE('',*,*,#38338,.F.);
#55009=ORIENTED_EDGE('',*,*,#38272,.T.);
#55010=ORIENTED_EDGE('',*,*,#38339,.F.);
#55011=ORIENTED_EDGE('',*,*,#38340,.T.);
#55012=ORIENTED_EDGE('',*,*,#38261,.T.);
#55013=ORIENTED_EDGE('',*,*,#38338,.T.);
#55014=ORIENTED_EDGE('',*,*,#38262,.T.);
#55015=ORIENTED_EDGE('',*,*,#38340,.F.);
#55016=ORIENTED_EDGE('',*,*,#38339,.T.);
#55017=ORIENTED_EDGE('',*,*,#38341,.F.);
#55018=ORIENTED_EDGE('',*,*,#38342,.T.);
#55019=ORIENTED_EDGE('',*,*,#38343,.T.);
#55020=ORIENTED_EDGE('',*,*,#38344,.T.);
#55021=ORIENTED_EDGE('',*,*,#38345,.F.);
#55022=ORIENTED_EDGE('',*,*,#38346,.T.);
#55023=ORIENTED_EDGE('',*,*,#38341,.T.);
#55024=ORIENTED_EDGE('',*,*,#38347,.T.);
#55025=ORIENTED_EDGE('',*,*,#38348,.F.);
#55026=ORIENTED_EDGE('',*,*,#38349,.T.);
#55027=ORIENTED_EDGE('',*,*,#38345,.T.);
#55028=ORIENTED_EDGE('',*,*,#38350,.T.);
#55029=ORIENTED_EDGE('',*,*,#38351,.F.);
#55030=ORIENTED_EDGE('',*,*,#38352,.T.);
#55031=ORIENTED_EDGE('',*,*,#38348,.T.);
#55032=ORIENTED_EDGE('',*,*,#38353,.T.);
#55033=ORIENTED_EDGE('',*,*,#38354,.F.);
#55034=ORIENTED_EDGE('',*,*,#38355,.T.);
#55035=ORIENTED_EDGE('',*,*,#38351,.T.);
#55036=ORIENTED_EDGE('',*,*,#38356,.T.);
#55037=ORIENTED_EDGE('',*,*,#38357,.F.);
#55038=ORIENTED_EDGE('',*,*,#38358,.T.);
#55039=ORIENTED_EDGE('',*,*,#38354,.T.);
#55040=ORIENTED_EDGE('',*,*,#38359,.T.);
#55041=ORIENTED_EDGE('',*,*,#38360,.F.);
#55042=ORIENTED_EDGE('',*,*,#38361,.T.);
#55043=ORIENTED_EDGE('',*,*,#38362,.F.);
#55044=ORIENTED_EDGE('',*,*,#38363,.F.);
#55045=ORIENTED_EDGE('',*,*,#38364,.T.);
#55046=ORIENTED_EDGE('',*,*,#38360,.T.);
#55047=ORIENTED_EDGE('',*,*,#38365,.F.);
#55048=ORIENTED_EDGE('',*,*,#38366,.F.);
#55049=ORIENTED_EDGE('',*,*,#38367,.F.);
#55050=ORIENTED_EDGE('',*,*,#38368,.T.);
#55051=ORIENTED_EDGE('',*,*,#38363,.T.);
#55052=ORIENTED_EDGE('',*,*,#38369,.F.);
#55053=ORIENTED_EDGE('',*,*,#38370,.F.);
#55054=ORIENTED_EDGE('',*,*,#38371,.T.);
#55055=ORIENTED_EDGE('',*,*,#38367,.T.);
#55056=ORIENTED_EDGE('',*,*,#38372,.F.);
#55057=ORIENTED_EDGE('',*,*,#38373,.F.);
#55058=ORIENTED_EDGE('',*,*,#38374,.T.);
#55059=ORIENTED_EDGE('',*,*,#38370,.T.);
#55060=ORIENTED_EDGE('',*,*,#38375,.F.);
#55061=ORIENTED_EDGE('',*,*,#38376,.F.);
#55062=ORIENTED_EDGE('',*,*,#38377,.T.);
#55063=ORIENTED_EDGE('',*,*,#38373,.T.);
#55064=ORIENTED_EDGE('',*,*,#38378,.F.);
#55065=ORIENTED_EDGE('',*,*,#38365,.T.);
#55066=ORIENTED_EDGE('',*,*,#38362,.T.);
#55067=ORIENTED_EDGE('',*,*,#38379,.T.);
#55068=ORIENTED_EDGE('',*,*,#38380,.F.);
#55069=ORIENTED_EDGE('',*,*,#38381,.F.);
#55070=ORIENTED_EDGE('',*,*,#38382,.T.);
#55071=ORIENTED_EDGE('',*,*,#38382,.F.);
#55072=ORIENTED_EDGE('',*,*,#38383,.F.);
#55073=ORIENTED_EDGE('',*,*,#38359,.F.);
#55074=ORIENTED_EDGE('',*,*,#38356,.F.);
#55075=ORIENTED_EDGE('',*,*,#38353,.F.);
#55076=ORIENTED_EDGE('',*,*,#38350,.F.);
#55077=ORIENTED_EDGE('',*,*,#38347,.F.);
#55078=ORIENTED_EDGE('',*,*,#38344,.F.);
#55079=ORIENTED_EDGE('',*,*,#38384,.F.);
#55080=ORIENTED_EDGE('',*,*,#38385,.T.);
#55081=ORIENTED_EDGE('',*,*,#38378,.T.);
#55082=ORIENTED_EDGE('',*,*,#38375,.T.);
#55083=ORIENTED_EDGE('',*,*,#38372,.T.);
#55084=ORIENTED_EDGE('',*,*,#38369,.T.);
#55085=ORIENTED_EDGE('',*,*,#38366,.T.);
#55086=ORIENTED_EDGE('',*,*,#38386,.T.);
#55087=ORIENTED_EDGE('',*,*,#38387,.T.);
#55088=ORIENTED_EDGE('',*,*,#38388,.T.);
#55089=ORIENTED_EDGE('',*,*,#38389,.T.);
#55090=ORIENTED_EDGE('',*,*,#38384,.T.);
#55091=ORIENTED_EDGE('',*,*,#38376,.T.);
#55092=ORIENTED_EDGE('',*,*,#38385,.F.);
#55093=ORIENTED_EDGE('',*,*,#38389,.F.);
#55094=ORIENTED_EDGE('',*,*,#38390,.T.);
#55095=ORIENTED_EDGE('',*,*,#38379,.F.);
#55096=ORIENTED_EDGE('',*,*,#38361,.F.);
#55097=ORIENTED_EDGE('',*,*,#38364,.F.);
#55098=ORIENTED_EDGE('',*,*,#38368,.F.);
#55099=ORIENTED_EDGE('',*,*,#38371,.F.);
#55100=ORIENTED_EDGE('',*,*,#38374,.F.);
#55101=ORIENTED_EDGE('',*,*,#38377,.F.);
#55102=ORIENTED_EDGE('',*,*,#38390,.F.);
#55103=ORIENTED_EDGE('',*,*,#38388,.F.);
#55104=ORIENTED_EDGE('',*,*,#38342,.F.);
#55105=ORIENTED_EDGE('',*,*,#38346,.F.);
#55106=ORIENTED_EDGE('',*,*,#38349,.F.);
#55107=ORIENTED_EDGE('',*,*,#38352,.F.);
#55108=ORIENTED_EDGE('',*,*,#38355,.F.);
#55109=ORIENTED_EDGE('',*,*,#38358,.F.);
#55110=ORIENTED_EDGE('',*,*,#38391,.F.);
#55111=ORIENTED_EDGE('',*,*,#38392,.F.);
#55112=ORIENTED_EDGE('',*,*,#38393,.T.);
#55113=ORIENTED_EDGE('',*,*,#38394,.F.);
#55114=ORIENTED_EDGE('',*,*,#38395,.T.);
#55115=ORIENTED_EDGE('',*,*,#38396,.F.);
#55116=ORIENTED_EDGE('',*,*,#38397,.F.);
#55117=ORIENTED_EDGE('',*,*,#38398,.T.);
#55118=ORIENTED_EDGE('',*,*,#38399,.F.);
#55119=ORIENTED_EDGE('',*,*,#38400,.F.);
#55120=ORIENTED_EDGE('',*,*,#38401,.T.);
#55121=ORIENTED_EDGE('',*,*,#38402,.F.);
#55122=ORIENTED_EDGE('',*,*,#38403,.F.);
#55123=ORIENTED_EDGE('',*,*,#38404,.T.);
#55124=ORIENTED_EDGE('',*,*,#38405,.F.);
#55125=ORIENTED_EDGE('',*,*,#38406,.F.);
#55126=ORIENTED_EDGE('',*,*,#38407,.T.);
#55127=ORIENTED_EDGE('',*,*,#38408,.F.);
#55128=ORIENTED_EDGE('',*,*,#38409,.F.);
#55129=ORIENTED_EDGE('',*,*,#38410,.T.);
#55130=ORIENTED_EDGE('',*,*,#38411,.F.);
#55131=ORIENTED_EDGE('',*,*,#38393,.F.);
#55132=ORIENTED_EDGE('',*,*,#38412,.F.);
#55133=ORIENTED_EDGE('',*,*,#38398,.F.);
#55134=ORIENTED_EDGE('',*,*,#38413,.F.);
#55135=ORIENTED_EDGE('',*,*,#38414,.F.);
#55136=ORIENTED_EDGE('',*,*,#38415,.F.);
#55137=ORIENTED_EDGE('',*,*,#38401,.F.);
#55138=ORIENTED_EDGE('',*,*,#38416,.F.);
#55139=ORIENTED_EDGE('',*,*,#38417,.F.);
#55140=ORIENTED_EDGE('',*,*,#38418,.F.);
#55141=ORIENTED_EDGE('',*,*,#38419,.F.);
#55142=ORIENTED_EDGE('',*,*,#38420,.F.);
#55143=ORIENTED_EDGE('',*,*,#38395,.F.);
#55144=ORIENTED_EDGE('',*,*,#38421,.F.);
#55145=ORIENTED_EDGE('',*,*,#38404,.F.);
#55146=ORIENTED_EDGE('',*,*,#38422,.F.);
#55147=ORIENTED_EDGE('',*,*,#38423,.F.);
#55148=ORIENTED_EDGE('',*,*,#38424,.F.);
#55149=ORIENTED_EDGE('',*,*,#38425,.F.);
#55150=ORIENTED_EDGE('',*,*,#38426,.F.);
#55151=ORIENTED_EDGE('',*,*,#38410,.F.);
#55152=ORIENTED_EDGE('',*,*,#38427,.F.);
#55153=ORIENTED_EDGE('',*,*,#38428,.F.);
#55154=ORIENTED_EDGE('',*,*,#38429,.F.);
#55155=ORIENTED_EDGE('',*,*,#38407,.F.);
#55156=ORIENTED_EDGE('',*,*,#38405,.T.);
#55157=ORIENTED_EDGE('',*,*,#38421,.T.);
#55158=ORIENTED_EDGE('',*,*,#38430,.F.);
#55159=ORIENTED_EDGE('',*,*,#38422,.T.);
#55160=ORIENTED_EDGE('',*,*,#38403,.T.);
#55161=ORIENTED_EDGE('',*,*,#38431,.T.);
#55162=ORIENTED_EDGE('',*,*,#38432,.T.);
#55163=ORIENTED_EDGE('',*,*,#38433,.F.);
#55164=ORIENTED_EDGE('',*,*,#38402,.T.);
#55165=ORIENTED_EDGE('',*,*,#38415,.T.);
#55166=ORIENTED_EDGE('',*,*,#38434,.F.);
#55167=ORIENTED_EDGE('',*,*,#38416,.T.);
#55168=ORIENTED_EDGE('',*,*,#38400,.T.);
#55169=ORIENTED_EDGE('',*,*,#38435,.T.);
#55170=ORIENTED_EDGE('',*,*,#38436,.T.);
#55171=ORIENTED_EDGE('',*,*,#38431,.F.);
#55172=ORIENTED_EDGE('',*,*,#38399,.T.);
#55173=ORIENTED_EDGE('',*,*,#38412,.T.);
#55174=ORIENTED_EDGE('',*,*,#38437,.F.);
#55175=ORIENTED_EDGE('',*,*,#38413,.T.);
#55176=ORIENTED_EDGE('',*,*,#38397,.T.);
#55177=ORIENTED_EDGE('',*,*,#38438,.T.);
#55178=ORIENTED_EDGE('',*,*,#38439,.T.);
#55179=ORIENTED_EDGE('',*,*,#38435,.F.);
#55180=ORIENTED_EDGE('',*,*,#38414,.T.);
#55181=ORIENTED_EDGE('',*,*,#38437,.T.);
#55182=ORIENTED_EDGE('',*,*,#38417,.T.);
#55183=ORIENTED_EDGE('',*,*,#38434,.T.);
#55184=ORIENTED_EDGE('',*,*,#38419,.T.);
#55185=ORIENTED_EDGE('',*,*,#38440,.T.);
#55186=ORIENTED_EDGE('',*,*,#38423,.T.);
#55187=ORIENTED_EDGE('',*,*,#38430,.T.);
#55188=ORIENTED_EDGE('',*,*,#38425,.T.);
#55189=ORIENTED_EDGE('',*,*,#38441,.T.);
#55190=ORIENTED_EDGE('',*,*,#38428,.T.);
#55191=ORIENTED_EDGE('',*,*,#38442,.T.);
#55192=ORIENTED_EDGE('',*,*,#38443,.F.);
#55193=ORIENTED_EDGE('',*,*,#38444,.T.);
#55194=ORIENTED_EDGE('',*,*,#38439,.F.);
#55195=ORIENTED_EDGE('',*,*,#38445,.T.);
#55196=ORIENTED_EDGE('',*,*,#38436,.F.);
#55197=ORIENTED_EDGE('',*,*,#38446,.T.);
#55198=ORIENTED_EDGE('',*,*,#38432,.F.);
#55199=ORIENTED_EDGE('',*,*,#38447,.T.);
#55200=ORIENTED_EDGE('',*,*,#38448,.F.);
#55201=ORIENTED_EDGE('',*,*,#38449,.T.);
#55202=ORIENTED_EDGE('',*,*,#38450,.F.);
#55203=ORIENTED_EDGE('',*,*,#38451,.T.);
#55204=ORIENTED_EDGE('',*,*,#38447,.F.);
#55205=ORIENTED_EDGE('',*,*,#38446,.F.);
#55206=ORIENTED_EDGE('',*,*,#38445,.F.);
#55207=ORIENTED_EDGE('',*,*,#38444,.F.);
#55208=ORIENTED_EDGE('',*,*,#38452,.T.);
#55209=ORIENTED_EDGE('',*,*,#38452,.F.);
#55210=ORIENTED_EDGE('',*,*,#38451,.F.);
#55211=ORIENTED_EDGE('',*,*,#38449,.F.);
#55212=ORIENTED_EDGE('',*,*,#38394,.T.);
#55213=ORIENTED_EDGE('',*,*,#38453,.T.);
#55214=ORIENTED_EDGE('',*,*,#38443,.T.);
#55215=ORIENTED_EDGE('',*,*,#38438,.F.);
#55216=ORIENTED_EDGE('',*,*,#38396,.T.);
#55217=ORIENTED_EDGE('',*,*,#38420,.T.);
#55218=ORIENTED_EDGE('',*,*,#38440,.F.);
#55219=ORIENTED_EDGE('',*,*,#38418,.T.);
#55220=ORIENTED_EDGE('',*,*,#38409,.T.);
#55221=ORIENTED_EDGE('',*,*,#38454,.T.);
#55222=ORIENTED_EDGE('',*,*,#38450,.T.);
#55223=ORIENTED_EDGE('',*,*,#38453,.F.);
#55224=ORIENTED_EDGE('',*,*,#38411,.T.);
#55225=ORIENTED_EDGE('',*,*,#38426,.T.);
#55226=ORIENTED_EDGE('',*,*,#38441,.F.);
#55227=ORIENTED_EDGE('',*,*,#38424,.T.);
#55228=ORIENTED_EDGE('',*,*,#38406,.T.);
#55229=ORIENTED_EDGE('',*,*,#38433,.T.);
#55230=ORIENTED_EDGE('',*,*,#38448,.T.);
#55231=ORIENTED_EDGE('',*,*,#38454,.F.);
#55232=ORIENTED_EDGE('',*,*,#38408,.T.);
#55233=ORIENTED_EDGE('',*,*,#38429,.T.);
#55234=ORIENTED_EDGE('',*,*,#38442,.F.);
#55235=ORIENTED_EDGE('',*,*,#38427,.T.);
#55236=ORIENTED_EDGE('',*,*,#38455,.F.);
#55237=ORIENTED_EDGE('',*,*,#38392,.T.);
#55238=ORIENTED_EDGE('',*,*,#38386,.F.);
#55239=ORIENTED_EDGE('',*,*,#38343,.F.);
#55240=ORIENTED_EDGE('',*,*,#38387,.F.);
#55241=ORIENTED_EDGE('',*,*,#38456,.T.);
#55242=ORIENTED_EDGE('',*,*,#38455,.T.);
#55243=ORIENTED_EDGE('',*,*,#38456,.F.);
#55244=ORIENTED_EDGE('',*,*,#38357,.T.);
#55245=ORIENTED_EDGE('',*,*,#38383,.T.);
#55246=ORIENTED_EDGE('',*,*,#38457,.F.);
#55247=ORIENTED_EDGE('',*,*,#38391,.T.);
#55248=ORIENTED_EDGE('',*,*,#38458,.F.);
#55249=ORIENTED_EDGE('',*,*,#38459,.T.);
#55250=ORIENTED_EDGE('',*,*,#38380,.T.);
#55251=ORIENTED_EDGE('',*,*,#38457,.T.);
#55252=ORIENTED_EDGE('',*,*,#38381,.T.);
#55253=ORIENTED_EDGE('',*,*,#38459,.F.);
#55254=ORIENTED_EDGE('',*,*,#38458,.T.);
#55255=ORIENTED_EDGE('',*,*,#38460,.F.);
#55256=ORIENTED_EDGE('',*,*,#38461,.T.);
#55257=ORIENTED_EDGE('',*,*,#38462,.T.);
#55258=ORIENTED_EDGE('',*,*,#38463,.T.);
#55259=ORIENTED_EDGE('',*,*,#38464,.F.);
#55260=ORIENTED_EDGE('',*,*,#38465,.T.);
#55261=ORIENTED_EDGE('',*,*,#38460,.T.);
#55262=ORIENTED_EDGE('',*,*,#38466,.T.);
#55263=ORIENTED_EDGE('',*,*,#38467,.F.);
#55264=ORIENTED_EDGE('',*,*,#38468,.T.);
#55265=ORIENTED_EDGE('',*,*,#38464,.T.);
#55266=ORIENTED_EDGE('',*,*,#38469,.T.);
#55267=ORIENTED_EDGE('',*,*,#38470,.F.);
#55268=ORIENTED_EDGE('',*,*,#38471,.T.);
#55269=ORIENTED_EDGE('',*,*,#38467,.T.);
#55270=ORIENTED_EDGE('',*,*,#38472,.T.);
#55271=ORIENTED_EDGE('',*,*,#38473,.F.);
#55272=ORIENTED_EDGE('',*,*,#38474,.T.);
#55273=ORIENTED_EDGE('',*,*,#38470,.T.);
#55274=ORIENTED_EDGE('',*,*,#38475,.T.);
#55275=ORIENTED_EDGE('',*,*,#38476,.F.);
#55276=ORIENTED_EDGE('',*,*,#38477,.T.);
#55277=ORIENTED_EDGE('',*,*,#38473,.T.);
#55278=ORIENTED_EDGE('',*,*,#38478,.T.);
#55279=ORIENTED_EDGE('',*,*,#38479,.F.);
#55280=ORIENTED_EDGE('',*,*,#38480,.T.);
#55281=ORIENTED_EDGE('',*,*,#38476,.T.);
#55282=ORIENTED_EDGE('',*,*,#38481,.T.);
#55283=ORIENTED_EDGE('',*,*,#38482,.F.);
#55284=ORIENTED_EDGE('',*,*,#38483,.F.);
#55285=ORIENTED_EDGE('',*,*,#38484,.T.);
#55286=ORIENTED_EDGE('',*,*,#38479,.T.);
#55287=ORIENTED_EDGE('',*,*,#38485,.T.);
#55288=ORIENTED_EDGE('',*,*,#38486,.F.);
#55289=ORIENTED_EDGE('',*,*,#38487,.T.);
#55290=ORIENTED_EDGE('',*,*,#38488,.F.);
#55291=ORIENTED_EDGE('',*,*,#38489,.F.);
#55292=ORIENTED_EDGE('',*,*,#38490,.F.);
#55293=ORIENTED_EDGE('',*,*,#38491,.T.);
#55294=ORIENTED_EDGE('',*,*,#38486,.T.);
#55295=ORIENTED_EDGE('',*,*,#38492,.F.);
#55296=ORIENTED_EDGE('',*,*,#38493,.F.);
#55297=ORIENTED_EDGE('',*,*,#38494,.T.);
#55298=ORIENTED_EDGE('',*,*,#38490,.T.);
#55299=ORIENTED_EDGE('',*,*,#38495,.F.);
#55300=ORIENTED_EDGE('',*,*,#38496,.F.);
#55301=ORIENTED_EDGE('',*,*,#38497,.T.);
#55302=ORIENTED_EDGE('',*,*,#38493,.T.);
#55303=ORIENTED_EDGE('',*,*,#38498,.F.);
#55304=ORIENTED_EDGE('',*,*,#38499,.F.);
#55305=ORIENTED_EDGE('',*,*,#38500,.T.);
#55306=ORIENTED_EDGE('',*,*,#38496,.T.);
#55307=ORIENTED_EDGE('',*,*,#38501,.F.);
#55308=ORIENTED_EDGE('',*,*,#38502,.F.);
#55309=ORIENTED_EDGE('',*,*,#38503,.T.);
#55310=ORIENTED_EDGE('',*,*,#38499,.T.);
#55311=ORIENTED_EDGE('',*,*,#38504,.F.);
#55312=ORIENTED_EDGE('',*,*,#38505,.F.);
#55313=ORIENTED_EDGE('',*,*,#38506,.T.);
#55314=ORIENTED_EDGE('',*,*,#38502,.T.);
#55315=ORIENTED_EDGE('',*,*,#38507,.F.);
#55316=ORIENTED_EDGE('',*,*,#38488,.T.);
#55317=ORIENTED_EDGE('',*,*,#38508,.T.);
#55318=ORIENTED_EDGE('',*,*,#38509,.F.);
#55319=ORIENTED_EDGE('',*,*,#38510,.T.);
#55320=ORIENTED_EDGE('',*,*,#38510,.F.);
#55321=ORIENTED_EDGE('',*,*,#38511,.F.);
#55322=ORIENTED_EDGE('',*,*,#38485,.F.);
#55323=ORIENTED_EDGE('',*,*,#38481,.F.);
#55324=ORIENTED_EDGE('',*,*,#38478,.F.);
#55325=ORIENTED_EDGE('',*,*,#38475,.F.);
#55326=ORIENTED_EDGE('',*,*,#38472,.F.);
#55327=ORIENTED_EDGE('',*,*,#38469,.F.);
#55328=ORIENTED_EDGE('',*,*,#38466,.F.);
#55329=ORIENTED_EDGE('',*,*,#38463,.F.);
#55330=ORIENTED_EDGE('',*,*,#38512,.F.);
#55331=ORIENTED_EDGE('',*,*,#38513,.T.);
#55332=ORIENTED_EDGE('',*,*,#38507,.T.);
#55333=ORIENTED_EDGE('',*,*,#38504,.T.);
#55334=ORIENTED_EDGE('',*,*,#38501,.T.);
#55335=ORIENTED_EDGE('',*,*,#38498,.T.);
#55336=ORIENTED_EDGE('',*,*,#38495,.T.);
#55337=ORIENTED_EDGE('',*,*,#38492,.T.);
#55338=ORIENTED_EDGE('',*,*,#38489,.T.);
#55339=ORIENTED_EDGE('',*,*,#38514,.T.);
#55340=ORIENTED_EDGE('',*,*,#38515,.T.);
#55341=ORIENTED_EDGE('',*,*,#38516,.T.);
#55342=ORIENTED_EDGE('',*,*,#38517,.T.);
#55343=ORIENTED_EDGE('',*,*,#38512,.T.);
#55344=ORIENTED_EDGE('',*,*,#38505,.T.);
#55345=ORIENTED_EDGE('',*,*,#38513,.F.);
#55346=ORIENTED_EDGE('',*,*,#38517,.F.);
#55347=ORIENTED_EDGE('',*,*,#38518,.T.);
#55348=ORIENTED_EDGE('',*,*,#38508,.F.);
#55349=ORIENTED_EDGE('',*,*,#38487,.F.);
#55350=ORIENTED_EDGE('',*,*,#38491,.F.);
#55351=ORIENTED_EDGE('',*,*,#38494,.F.);
#55352=ORIENTED_EDGE('',*,*,#38497,.F.);
#55353=ORIENTED_EDGE('',*,*,#38500,.F.);
#55354=ORIENTED_EDGE('',*,*,#38503,.F.);
#55355=ORIENTED_EDGE('',*,*,#38506,.F.);
#55356=ORIENTED_EDGE('',*,*,#38518,.F.);
#55357=ORIENTED_EDGE('',*,*,#38516,.F.);
#55358=ORIENTED_EDGE('',*,*,#38461,.F.);
#55359=ORIENTED_EDGE('',*,*,#38465,.F.);
#55360=ORIENTED_EDGE('',*,*,#38468,.F.);
#55361=ORIENTED_EDGE('',*,*,#38471,.F.);
#55362=ORIENTED_EDGE('',*,*,#38474,.F.);
#55363=ORIENTED_EDGE('',*,*,#38477,.F.);
#55364=ORIENTED_EDGE('',*,*,#38480,.F.);
#55365=ORIENTED_EDGE('',*,*,#38484,.F.);
#55366=ORIENTED_EDGE('',*,*,#38519,.F.);
#55367=ORIENTED_EDGE('',*,*,#38520,.T.);
#55368=ORIENTED_EDGE('',*,*,#38521,.T.);
#55369=ORIENTED_EDGE('',*,*,#38522,.F.);
#55370=ORIENTED_EDGE('',*,*,#38523,.F.);
#55371=ORIENTED_EDGE('',*,*,#38524,.T.);
#55372=ORIENTED_EDGE('',*,*,#38525,.T.);
#55373=ORIENTED_EDGE('',*,*,#38520,.F.);
#55374=ORIENTED_EDGE('',*,*,#38526,.F.);
#55375=ORIENTED_EDGE('',*,*,#38527,.T.);
#55376=ORIENTED_EDGE('',*,*,#38528,.T.);
#55377=ORIENTED_EDGE('',*,*,#38524,.F.);
#55378=ORIENTED_EDGE('',*,*,#38529,.F.);
#55379=ORIENTED_EDGE('',*,*,#38530,.T.);
#55380=ORIENTED_EDGE('',*,*,#38531,.T.);
#55381=ORIENTED_EDGE('',*,*,#38527,.F.);
#55382=ORIENTED_EDGE('',*,*,#38532,.F.);
#55383=ORIENTED_EDGE('',*,*,#38533,.T.);
#55384=ORIENTED_EDGE('',*,*,#38534,.T.);
#55385=ORIENTED_EDGE('',*,*,#38530,.F.);
#55386=ORIENTED_EDGE('',*,*,#38535,.F.);
#55387=ORIENTED_EDGE('',*,*,#38522,.T.);
#55388=ORIENTED_EDGE('',*,*,#38536,.T.);
#55389=ORIENTED_EDGE('',*,*,#38533,.F.);
#55390=ORIENTED_EDGE('',*,*,#38536,.F.);
#55391=ORIENTED_EDGE('',*,*,#38521,.F.);
#55392=ORIENTED_EDGE('',*,*,#38525,.F.);
#55393=ORIENTED_EDGE('',*,*,#38528,.F.);
#55394=ORIENTED_EDGE('',*,*,#38531,.F.);
#55395=ORIENTED_EDGE('',*,*,#38534,.F.);
#55396=ORIENTED_EDGE('',*,*,#38537,.F.);
#55397=ORIENTED_EDGE('',*,*,#38514,.F.);
#55398=ORIENTED_EDGE('',*,*,#38462,.F.);
#55399=ORIENTED_EDGE('',*,*,#38515,.F.);
#55400=ORIENTED_EDGE('',*,*,#38538,.T.);
#55401=ORIENTED_EDGE('',*,*,#38537,.T.);
#55402=ORIENTED_EDGE('',*,*,#38538,.F.);
#55403=ORIENTED_EDGE('',*,*,#38482,.T.);
#55404=ORIENTED_EDGE('',*,*,#38511,.T.);
#55405=ORIENTED_EDGE('',*,*,#38539,.F.);
#55406=ORIENTED_EDGE('',*,*,#38540,.F.);
#55407=ORIENTED_EDGE('',*,*,#38541,.T.);
#55408=ORIENTED_EDGE('',*,*,#38539,.T.);
#55409=ORIENTED_EDGE('',*,*,#38509,.T.);
#55410=ORIENTED_EDGE('',*,*,#38483,.T.);
#55411=ORIENTED_EDGE('',*,*,#38541,.F.);
#55412=ORIENTED_EDGE('',*,*,#38540,.T.);
#55413=ORIENTED_EDGE('',*,*,#38519,.T.);
#55414=ORIENTED_EDGE('',*,*,#38535,.T.);
#55415=ORIENTED_EDGE('',*,*,#38532,.T.);
#55416=ORIENTED_EDGE('',*,*,#38529,.T.);
#55417=ORIENTED_EDGE('',*,*,#38526,.T.);
#55418=ORIENTED_EDGE('',*,*,#38523,.T.);
#55419=ORIENTED_EDGE('',*,*,#38542,.F.);
#55420=ORIENTED_EDGE('',*,*,#38543,.T.);
#55421=ORIENTED_EDGE('',*,*,#38544,.F.);
#55422=ORIENTED_EDGE('',*,*,#38545,.T.);
#55423=ORIENTED_EDGE('',*,*,#38546,.F.);
#55424=ORIENTED_EDGE('',*,*,#38547,.T.);
#55425=ORIENTED_EDGE('',*,*,#38542,.T.);
#55426=ORIENTED_EDGE('',*,*,#38548,.T.);
#55427=ORIENTED_EDGE('',*,*,#38549,.F.);
#55428=ORIENTED_EDGE('',*,*,#38550,.T.);
#55429=ORIENTED_EDGE('',*,*,#38546,.T.);
#55430=ORIENTED_EDGE('',*,*,#38551,.T.);
#55431=ORIENTED_EDGE('',*,*,#38552,.F.);
#55432=ORIENTED_EDGE('',*,*,#38553,.T.);
#55433=ORIENTED_EDGE('',*,*,#38549,.T.);
#55434=ORIENTED_EDGE('',*,*,#38554,.T.);
#55435=ORIENTED_EDGE('',*,*,#38555,.F.);
#55436=ORIENTED_EDGE('',*,*,#38556,.T.);
#55437=ORIENTED_EDGE('',*,*,#38552,.T.);
#55438=ORIENTED_EDGE('',*,*,#38557,.T.);
#55439=ORIENTED_EDGE('',*,*,#38558,.F.);
#55440=ORIENTED_EDGE('',*,*,#38559,.T.);
#55441=ORIENTED_EDGE('',*,*,#38555,.T.);
#55442=ORIENTED_EDGE('',*,*,#38560,.T.);
#55443=ORIENTED_EDGE('',*,*,#38561,.F.);
#55444=ORIENTED_EDGE('',*,*,#38562,.T.);
#55445=ORIENTED_EDGE('',*,*,#38558,.T.);
#55446=ORIENTED_EDGE('',*,*,#38563,.T.);
#55447=ORIENTED_EDGE('',*,*,#38564,.F.);
#55448=ORIENTED_EDGE('',*,*,#38565,.T.);
#55449=ORIENTED_EDGE('',*,*,#38561,.T.);
#55450=ORIENTED_EDGE('',*,*,#38566,.T.);
#55451=ORIENTED_EDGE('',*,*,#38567,.F.);
#55452=ORIENTED_EDGE('',*,*,#38568,.T.);
#55453=ORIENTED_EDGE('',*,*,#38564,.T.);
#55454=ORIENTED_EDGE('',*,*,#38569,.T.);
#55455=ORIENTED_EDGE('',*,*,#38570,.F.);
#55456=ORIENTED_EDGE('',*,*,#38571,.T.);
#55457=ORIENTED_EDGE('',*,*,#38567,.T.);
#55458=ORIENTED_EDGE('',*,*,#38572,.T.);
#55459=ORIENTED_EDGE('',*,*,#38573,.F.);
#55460=ORIENTED_EDGE('',*,*,#38574,.T.);
#55461=ORIENTED_EDGE('',*,*,#38570,.T.);
#55462=ORIENTED_EDGE('',*,*,#38575,.T.);
#55463=ORIENTED_EDGE('',*,*,#38576,.F.);
#55464=ORIENTED_EDGE('',*,*,#38577,.T.);
#55465=ORIENTED_EDGE('',*,*,#38573,.T.);
#55466=ORIENTED_EDGE('',*,*,#38578,.T.);
#55467=ORIENTED_EDGE('',*,*,#38579,.F.);
#55468=ORIENTED_EDGE('',*,*,#38580,.T.);
#55469=ORIENTED_EDGE('',*,*,#38576,.T.);
#55470=ORIENTED_EDGE('',*,*,#38581,.T.);
#55471=ORIENTED_EDGE('',*,*,#38582,.F.);
#55472=ORIENTED_EDGE('',*,*,#38583,.T.);
#55473=ORIENTED_EDGE('',*,*,#38584,.F.);
#55474=ORIENTED_EDGE('',*,*,#38585,.F.);
#55475=ORIENTED_EDGE('',*,*,#38586,.F.);
#55476=ORIENTED_EDGE('',*,*,#38587,.T.);
#55477=ORIENTED_EDGE('',*,*,#38582,.T.);
#55478=ORIENTED_EDGE('',*,*,#38588,.F.);
#55479=ORIENTED_EDGE('',*,*,#38589,.F.);
#55480=ORIENTED_EDGE('',*,*,#38590,.T.);
#55481=ORIENTED_EDGE('',*,*,#38586,.T.);
#55482=ORIENTED_EDGE('',*,*,#38591,.F.);
#55483=ORIENTED_EDGE('',*,*,#38592,.F.);
#55484=ORIENTED_EDGE('',*,*,#38593,.T.);
#55485=ORIENTED_EDGE('',*,*,#38589,.T.);
#55486=ORIENTED_EDGE('',*,*,#38594,.F.);
#55487=ORIENTED_EDGE('',*,*,#38595,.F.);
#55488=ORIENTED_EDGE('',*,*,#38596,.T.);
#55489=ORIENTED_EDGE('',*,*,#38592,.T.);
#55490=ORIENTED_EDGE('',*,*,#38597,.F.);
#55491=ORIENTED_EDGE('',*,*,#38598,.F.);
#55492=ORIENTED_EDGE('',*,*,#38599,.T.);
#55493=ORIENTED_EDGE('',*,*,#38595,.T.);
#55494=ORIENTED_EDGE('',*,*,#38600,.F.);
#55495=ORIENTED_EDGE('',*,*,#38601,.F.);
#55496=ORIENTED_EDGE('',*,*,#38602,.T.);
#55497=ORIENTED_EDGE('',*,*,#38598,.T.);
#55498=ORIENTED_EDGE('',*,*,#38603,.F.);
#55499=ORIENTED_EDGE('',*,*,#38604,.F.);
#55500=ORIENTED_EDGE('',*,*,#38605,.T.);
#55501=ORIENTED_EDGE('',*,*,#38601,.T.);
#55502=ORIENTED_EDGE('',*,*,#38606,.F.);
#55503=ORIENTED_EDGE('',*,*,#38607,.F.);
#55504=ORIENTED_EDGE('',*,*,#38608,.T.);
#55505=ORIENTED_EDGE('',*,*,#38604,.T.);
#55506=ORIENTED_EDGE('',*,*,#38609,.F.);
#55507=ORIENTED_EDGE('',*,*,#38610,.F.);
#55508=ORIENTED_EDGE('',*,*,#38611,.T.);
#55509=ORIENTED_EDGE('',*,*,#38607,.T.);
#55510=ORIENTED_EDGE('',*,*,#38612,.F.);
#55511=ORIENTED_EDGE('',*,*,#38613,.F.);
#55512=ORIENTED_EDGE('',*,*,#38614,.T.);
#55513=ORIENTED_EDGE('',*,*,#38610,.T.);
#55514=ORIENTED_EDGE('',*,*,#38615,.F.);
#55515=ORIENTED_EDGE('',*,*,#38616,.F.);
#55516=ORIENTED_EDGE('',*,*,#38617,.T.);
#55517=ORIENTED_EDGE('',*,*,#38613,.T.);
#55518=ORIENTED_EDGE('',*,*,#38618,.F.);
#55519=ORIENTED_EDGE('',*,*,#38584,.T.);
#55520=ORIENTED_EDGE('',*,*,#38619,.T.);
#55521=ORIENTED_EDGE('',*,*,#38620,.F.);
#55522=ORIENTED_EDGE('',*,*,#38621,.F.);
#55523=ORIENTED_EDGE('',*,*,#38622,.T.);
#55524=ORIENTED_EDGE('',*,*,#38622,.F.);
#55525=ORIENTED_EDGE('',*,*,#38623,.F.);
#55526=ORIENTED_EDGE('',*,*,#38581,.F.);
#55527=ORIENTED_EDGE('',*,*,#38578,.F.);
#55528=ORIENTED_EDGE('',*,*,#38575,.F.);
#55529=ORIENTED_EDGE('',*,*,#38572,.F.);
#55530=ORIENTED_EDGE('',*,*,#38569,.F.);
#55531=ORIENTED_EDGE('',*,*,#38566,.F.);
#55532=ORIENTED_EDGE('',*,*,#38563,.F.);
#55533=ORIENTED_EDGE('',*,*,#38560,.F.);
#55534=ORIENTED_EDGE('',*,*,#38557,.F.);
#55535=ORIENTED_EDGE('',*,*,#38554,.F.);
#55536=ORIENTED_EDGE('',*,*,#38551,.F.);
#55537=ORIENTED_EDGE('',*,*,#38548,.F.);
#55538=ORIENTED_EDGE('',*,*,#38545,.F.);
#55539=ORIENTED_EDGE('',*,*,#38624,.F.);
#55540=ORIENTED_EDGE('',*,*,#38625,.T.);
#55541=ORIENTED_EDGE('',*,*,#38618,.T.);
#55542=ORIENTED_EDGE('',*,*,#38615,.T.);
#55543=ORIENTED_EDGE('',*,*,#38612,.T.);
#55544=ORIENTED_EDGE('',*,*,#38609,.T.);
#55545=ORIENTED_EDGE('',*,*,#38606,.T.);
#55546=ORIENTED_EDGE('',*,*,#38603,.T.);
#55547=ORIENTED_EDGE('',*,*,#38600,.T.);
#55548=ORIENTED_EDGE('',*,*,#38597,.T.);
#55549=ORIENTED_EDGE('',*,*,#38594,.T.);
#55550=ORIENTED_EDGE('',*,*,#38591,.T.);
#55551=ORIENTED_EDGE('',*,*,#38588,.T.);
#55552=ORIENTED_EDGE('',*,*,#38585,.T.);
#55553=ORIENTED_EDGE('',*,*,#38626,.F.);
#55554=ORIENTED_EDGE('',*,*,#38627,.T.);
#55555=ORIENTED_EDGE('',*,*,#38628,.T.);
#55556=ORIENTED_EDGE('',*,*,#38624,.T.);
#55557=ORIENTED_EDGE('',*,*,#38629,.F.);
#55558=ORIENTED_EDGE('',*,*,#38616,.T.);
#55559=ORIENTED_EDGE('',*,*,#38625,.F.);
#55560=ORIENTED_EDGE('',*,*,#38628,.F.);
#55561=ORIENTED_EDGE('',*,*,#38630,.T.);
#55562=ORIENTED_EDGE('',*,*,#38619,.F.);
#55563=ORIENTED_EDGE('',*,*,#38583,.F.);
#55564=ORIENTED_EDGE('',*,*,#38587,.F.);
#55565=ORIENTED_EDGE('',*,*,#38590,.F.);
#55566=ORIENTED_EDGE('',*,*,#38593,.F.);
#55567=ORIENTED_EDGE('',*,*,#38596,.F.);
#55568=ORIENTED_EDGE('',*,*,#38599,.F.);
#55569=ORIENTED_EDGE('',*,*,#38602,.F.);
#55570=ORIENTED_EDGE('',*,*,#38605,.F.);
#55571=ORIENTED_EDGE('',*,*,#38608,.F.);
#55572=ORIENTED_EDGE('',*,*,#38611,.F.);
#55573=ORIENTED_EDGE('',*,*,#38614,.F.);
#55574=ORIENTED_EDGE('',*,*,#38617,.F.);
#55575=ORIENTED_EDGE('',*,*,#38630,.F.);
#55576=ORIENTED_EDGE('',*,*,#38627,.F.);
#55577=ORIENTED_EDGE('',*,*,#38543,.F.);
#55578=ORIENTED_EDGE('',*,*,#38547,.F.);
#55579=ORIENTED_EDGE('',*,*,#38550,.F.);
#55580=ORIENTED_EDGE('',*,*,#38553,.F.);
#55581=ORIENTED_EDGE('',*,*,#38556,.F.);
#55582=ORIENTED_EDGE('',*,*,#38559,.F.);
#55583=ORIENTED_EDGE('',*,*,#38562,.F.);
#55584=ORIENTED_EDGE('',*,*,#38565,.F.);
#55585=ORIENTED_EDGE('',*,*,#38568,.F.);
#55586=ORIENTED_EDGE('',*,*,#38571,.F.);
#55587=ORIENTED_EDGE('',*,*,#38574,.F.);
#55588=ORIENTED_EDGE('',*,*,#38577,.F.);
#55589=ORIENTED_EDGE('',*,*,#38580,.F.);
#55590=ORIENTED_EDGE('',*,*,#38631,.F.);
#55591=ORIENTED_EDGE('',*,*,#38626,.T.);
#55592=ORIENTED_EDGE('',*,*,#38632,.T.);
#55593=ORIENTED_EDGE('',*,*,#38633,.T.);
#55594=ORIENTED_EDGE('',*,*,#38632,.F.);
#55595=ORIENTED_EDGE('',*,*,#38629,.T.);
#55596=ORIENTED_EDGE('',*,*,#38544,.T.);
#55597=ORIENTED_EDGE('',*,*,#38579,.T.);
#55598=ORIENTED_EDGE('',*,*,#38623,.T.);
#55599=ORIENTED_EDGE('',*,*,#38634,.F.);
#55600=ORIENTED_EDGE('',*,*,#38631,.T.);
#55601=ORIENTED_EDGE('',*,*,#38635,.F.);
#55602=ORIENTED_EDGE('',*,*,#38633,.F.);
#55603=ORIENTED_EDGE('',*,*,#38621,.T.);
#55604=ORIENTED_EDGE('',*,*,#38636,.T.);
#55605=ORIENTED_EDGE('',*,*,#38637,.T.);
#55606=ORIENTED_EDGE('',*,*,#38636,.F.);
#55607=ORIENTED_EDGE('',*,*,#38620,.T.);
#55608=ORIENTED_EDGE('',*,*,#38634,.T.);
#55609=ORIENTED_EDGE('',*,*,#38637,.F.);
#55610=ORIENTED_EDGE('',*,*,#38638,.F.);
#55611=ORIENTED_EDGE('',*,*,#38639,.T.);
#55612=ORIENTED_EDGE('',*,*,#38640,.T.);
#55613=ORIENTED_EDGE('',*,*,#38641,.F.);
#55614=ORIENTED_EDGE('',*,*,#38642,.F.);
#55615=ORIENTED_EDGE('',*,*,#38640,.F.);
#55616=ORIENTED_EDGE('',*,*,#38643,.F.);
#55617=ORIENTED_EDGE('',*,*,#38644,.F.);
#55618=ORIENTED_EDGE('',*,*,#38645,.F.);
#55619=ORIENTED_EDGE('',*,*,#38643,.T.);
#55620=ORIENTED_EDGE('',*,*,#38639,.F.);
#55621=ORIENTED_EDGE('',*,*,#38641,.T.);
#55622=ORIENTED_EDGE('',*,*,#38642,.T.);
#55623=ORIENTED_EDGE('',*,*,#38645,.T.);
#55624=ORIENTED_EDGE('',*,*,#38646,.F.);
#55625=ORIENTED_EDGE('',*,*,#38647,.T.);
#55626=ORIENTED_EDGE('',*,*,#38648,.T.);
#55627=ORIENTED_EDGE('',*,*,#38649,.T.);
#55628=ORIENTED_EDGE('',*,*,#38650,.F.);
#55629=ORIENTED_EDGE('',*,*,#38651,.T.);
#55630=ORIENTED_EDGE('',*,*,#38652,.T.);
#55631=ORIENTED_EDGE('',*,*,#38653,.T.);
#55632=ORIENTED_EDGE('',*,*,#38654,.F.);
#55633=ORIENTED_EDGE('',*,*,#38655,.T.);
#55634=ORIENTED_EDGE('',*,*,#38656,.T.);
#55635=ORIENTED_EDGE('',*,*,#38657,.T.);
#55636=ORIENTED_EDGE('',*,*,#38658,.F.);
#55637=ORIENTED_EDGE('',*,*,#38659,.T.);
#55638=ORIENTED_EDGE('',*,*,#38660,.T.);
#55639=ORIENTED_EDGE('',*,*,#38661,.T.);
#55640=ORIENTED_EDGE('',*,*,#38662,.F.);
#55641=ORIENTED_EDGE('',*,*,#38663,.T.);
#55642=ORIENTED_EDGE('',*,*,#38664,.T.);
#55643=ORIENTED_EDGE('',*,*,#38665,.T.);
#55644=ORIENTED_EDGE('',*,*,#38666,.F.);
#55645=ORIENTED_EDGE('',*,*,#38667,.T.);
#55646=ORIENTED_EDGE('',*,*,#38668,.T.);
#55647=ORIENTED_EDGE('',*,*,#38669,.T.);
#55648=ORIENTED_EDGE('',*,*,#38670,.F.);
#55649=ORIENTED_EDGE('',*,*,#38671,.T.);
#55650=ORIENTED_EDGE('',*,*,#38672,.T.);
#55651=ORIENTED_EDGE('',*,*,#38673,.T.);
#55652=ORIENTED_EDGE('',*,*,#38674,.F.);
#55653=ORIENTED_EDGE('',*,*,#38675,.T.);
#55654=ORIENTED_EDGE('',*,*,#38676,.T.);
#55655=ORIENTED_EDGE('',*,*,#38677,.T.);
#55656=ORIENTED_EDGE('',*,*,#38678,.F.);
#55657=ORIENTED_EDGE('',*,*,#38679,.T.);
#55658=ORIENTED_EDGE('',*,*,#38680,.T.);
#55659=ORIENTED_EDGE('',*,*,#38681,.T.);
#55660=ORIENTED_EDGE('',*,*,#38682,.F.);
#55661=ORIENTED_EDGE('',*,*,#38683,.T.);
#55662=ORIENTED_EDGE('',*,*,#38684,.T.);
#55663=ORIENTED_EDGE('',*,*,#38685,.T.);
#55664=ORIENTED_EDGE('',*,*,#38686,.F.);
#55665=ORIENTED_EDGE('',*,*,#38687,.T.);
#55666=ORIENTED_EDGE('',*,*,#38688,.T.);
#55667=ORIENTED_EDGE('',*,*,#38689,.T.);
#55668=ORIENTED_EDGE('',*,*,#38690,.F.);
#55669=ORIENTED_EDGE('',*,*,#38691,.T.);
#55670=ORIENTED_EDGE('',*,*,#38692,.T.);
#55671=ORIENTED_EDGE('',*,*,#38693,.T.);
#55672=ORIENTED_EDGE('',*,*,#38694,.F.);
#55673=ORIENTED_EDGE('',*,*,#38695,.T.);
#55674=ORIENTED_EDGE('',*,*,#38696,.T.);
#55675=ORIENTED_EDGE('',*,*,#38697,.T.);
#55676=ORIENTED_EDGE('',*,*,#38698,.F.);
#55677=ORIENTED_EDGE('',*,*,#38699,.T.);
#55678=ORIENTED_EDGE('',*,*,#38700,.T.);
#55679=ORIENTED_EDGE('',*,*,#38701,.T.);
#55680=ORIENTED_EDGE('',*,*,#38702,.F.);
#55681=ORIENTED_EDGE('',*,*,#38703,.T.);
#55682=ORIENTED_EDGE('',*,*,#38704,.T.);
#55683=ORIENTED_EDGE('',*,*,#38705,.T.);
#55684=ORIENTED_EDGE('',*,*,#38706,.F.);
#55685=ORIENTED_EDGE('',*,*,#38707,.T.);
#55686=ORIENTED_EDGE('',*,*,#38708,.T.);
#55687=ORIENTED_EDGE('',*,*,#38709,.T.);
#55688=ORIENTED_EDGE('',*,*,#38710,.F.);
#55689=ORIENTED_EDGE('',*,*,#38711,.T.);
#55690=ORIENTED_EDGE('',*,*,#38712,.T.);
#55691=ORIENTED_EDGE('',*,*,#38713,.T.);
#55692=ORIENTED_EDGE('',*,*,#38714,.F.);
#55693=ORIENTED_EDGE('',*,*,#38715,.T.);
#55694=ORIENTED_EDGE('',*,*,#38716,.T.);
#55695=ORIENTED_EDGE('',*,*,#38717,.T.);
#55696=ORIENTED_EDGE('',*,*,#38718,.F.);
#55697=ORIENTED_EDGE('',*,*,#38719,.T.);
#55698=ORIENTED_EDGE('',*,*,#38720,.T.);
#55699=ORIENTED_EDGE('',*,*,#38721,.T.);
#55700=ORIENTED_EDGE('',*,*,#38722,.F.);
#55701=ORIENTED_EDGE('',*,*,#38723,.F.);
#55702=ORIENTED_EDGE('',*,*,#38721,.F.);
#55703=ORIENTED_EDGE('',*,*,#38724,.T.);
#55704=ORIENTED_EDGE('',*,*,#38725,.T.);
#55705=ORIENTED_EDGE('',*,*,#38726,.F.);
#55706=ORIENTED_EDGE('',*,*,#38727,.T.);
#55707=ORIENTED_EDGE('',*,*,#38728,.T.);
#55708=ORIENTED_EDGE('',*,*,#38729,.T.);
#55709=ORIENTED_EDGE('',*,*,#38730,.F.);
#55710=ORIENTED_EDGE('',*,*,#38731,.T.);
#55711=ORIENTED_EDGE('',*,*,#38732,.T.);
#55712=ORIENTED_EDGE('',*,*,#38733,.T.);
#55713=ORIENTED_EDGE('',*,*,#38734,.F.);
#55714=ORIENTED_EDGE('',*,*,#38735,.T.);
#55715=ORIENTED_EDGE('',*,*,#38736,.T.);
#55716=ORIENTED_EDGE('',*,*,#38737,.T.);
#55717=ORIENTED_EDGE('',*,*,#38738,.F.);
#55718=ORIENTED_EDGE('',*,*,#38739,.T.);
#55719=ORIENTED_EDGE('',*,*,#38740,.T.);
#55720=ORIENTED_EDGE('',*,*,#38741,.T.);
#55721=ORIENTED_EDGE('',*,*,#38742,.F.);
#55722=ORIENTED_EDGE('',*,*,#38743,.T.);
#55723=ORIENTED_EDGE('',*,*,#38744,.T.);
#55724=ORIENTED_EDGE('',*,*,#38745,.T.);
#55725=ORIENTED_EDGE('',*,*,#38746,.F.);
#55726=ORIENTED_EDGE('',*,*,#38747,.T.);
#55727=ORIENTED_EDGE('',*,*,#38748,.T.);
#55728=ORIENTED_EDGE('',*,*,#38749,.T.);
#55729=ORIENTED_EDGE('',*,*,#38750,.F.);
#55730=ORIENTED_EDGE('',*,*,#38751,.T.);
#55731=ORIENTED_EDGE('',*,*,#38752,.T.);
#55732=ORIENTED_EDGE('',*,*,#38753,.T.);
#55733=ORIENTED_EDGE('',*,*,#38754,.F.);
#55734=ORIENTED_EDGE('',*,*,#38755,.T.);
#55735=ORIENTED_EDGE('',*,*,#38756,.T.);
#55736=ORIENTED_EDGE('',*,*,#38757,.T.);
#55737=ORIENTED_EDGE('',*,*,#38758,.F.);
#55738=ORIENTED_EDGE('',*,*,#38759,.T.);
#55739=ORIENTED_EDGE('',*,*,#38760,.T.);
#55740=ORIENTED_EDGE('',*,*,#38761,.T.);
#55741=ORIENTED_EDGE('',*,*,#38762,.F.);
#55742=ORIENTED_EDGE('',*,*,#38763,.T.);
#55743=ORIENTED_EDGE('',*,*,#38764,.T.);
#55744=ORIENTED_EDGE('',*,*,#38765,.T.);
#55745=ORIENTED_EDGE('',*,*,#38766,.F.);
#55746=ORIENTED_EDGE('',*,*,#38767,.T.);
#55747=ORIENTED_EDGE('',*,*,#38768,.T.);
#55748=ORIENTED_EDGE('',*,*,#38769,.T.);
#55749=ORIENTED_EDGE('',*,*,#38770,.F.);
#55750=ORIENTED_EDGE('',*,*,#38771,.T.);
#55751=ORIENTED_EDGE('',*,*,#38772,.T.);
#55752=ORIENTED_EDGE('',*,*,#38773,.T.);
#55753=ORIENTED_EDGE('',*,*,#38774,.F.);
#55754=ORIENTED_EDGE('',*,*,#38775,.T.);
#55755=ORIENTED_EDGE('',*,*,#38776,.T.);
#55756=ORIENTED_EDGE('',*,*,#38777,.T.);
#55757=ORIENTED_EDGE('',*,*,#38778,.F.);
#55758=ORIENTED_EDGE('',*,*,#38779,.T.);
#55759=ORIENTED_EDGE('',*,*,#38780,.T.);
#55760=ORIENTED_EDGE('',*,*,#38781,.T.);
#55761=ORIENTED_EDGE('',*,*,#38782,.F.);
#55762=ORIENTED_EDGE('',*,*,#38783,.T.);
#55763=ORIENTED_EDGE('',*,*,#38784,.T.);
#55764=ORIENTED_EDGE('',*,*,#38785,.T.);
#55765=ORIENTED_EDGE('',*,*,#38786,.F.);
#55766=ORIENTED_EDGE('',*,*,#38787,.T.);
#55767=ORIENTED_EDGE('',*,*,#38788,.T.);
#55768=ORIENTED_EDGE('',*,*,#38789,.T.);
#55769=ORIENTED_EDGE('',*,*,#38790,.F.);
#55770=ORIENTED_EDGE('',*,*,#38791,.F.);
#55771=ORIENTED_EDGE('',*,*,#38792,.T.);
#55772=ORIENTED_EDGE('',*,*,#38793,.T.);
#55773=ORIENTED_EDGE('',*,*,#38787,.F.);
#55774=ORIENTED_EDGE('',*,*,#38788,.F.);
#55775=ORIENTED_EDGE('',*,*,#38793,.F.);
#55776=ORIENTED_EDGE('',*,*,#38794,.F.);
#55777=ORIENTED_EDGE('',*,*,#38795,.F.);
#55778=ORIENTED_EDGE('',*,*,#38789,.F.);
#55779=ORIENTED_EDGE('',*,*,#38794,.T.);
#55780=ORIENTED_EDGE('',*,*,#38792,.F.);
#55781=ORIENTED_EDGE('',*,*,#38796,.F.);
#55782=ORIENTED_EDGE('',*,*,#38797,.T.);
#55783=ORIENTED_EDGE('',*,*,#38798,.T.);
#55784=ORIENTED_EDGE('',*,*,#38783,.F.);
#55785=ORIENTED_EDGE('',*,*,#38784,.F.);
#55786=ORIENTED_EDGE('',*,*,#38798,.F.);
#55787=ORIENTED_EDGE('',*,*,#38799,.F.);
#55788=ORIENTED_EDGE('',*,*,#38800,.F.);
#55789=ORIENTED_EDGE('',*,*,#38785,.F.);
#55790=ORIENTED_EDGE('',*,*,#38799,.T.);
#55791=ORIENTED_EDGE('',*,*,#38797,.F.);
#55792=ORIENTED_EDGE('',*,*,#38801,.F.);
#55793=ORIENTED_EDGE('',*,*,#38802,.T.);
#55794=ORIENTED_EDGE('',*,*,#38803,.T.);
#55795=ORIENTED_EDGE('',*,*,#38779,.F.);
#55796=ORIENTED_EDGE('',*,*,#38780,.F.);
#55797=ORIENTED_EDGE('',*,*,#38803,.F.);
#55798=ORIENTED_EDGE('',*,*,#38804,.F.);
#55799=ORIENTED_EDGE('',*,*,#38805,.F.);
#55800=ORIENTED_EDGE('',*,*,#38781,.F.);
#55801=ORIENTED_EDGE('',*,*,#38804,.T.);
#55802=ORIENTED_EDGE('',*,*,#38802,.F.);
#55803=ORIENTED_EDGE('',*,*,#38806,.F.);
#55804=ORIENTED_EDGE('',*,*,#38807,.T.);
#55805=ORIENTED_EDGE('',*,*,#38808,.T.);
#55806=ORIENTED_EDGE('',*,*,#38775,.F.);
#55807=ORIENTED_EDGE('',*,*,#38776,.F.);
#55808=ORIENTED_EDGE('',*,*,#38808,.F.);
#55809=ORIENTED_EDGE('',*,*,#38809,.F.);
#55810=ORIENTED_EDGE('',*,*,#38810,.F.);
#55811=ORIENTED_EDGE('',*,*,#38777,.F.);
#55812=ORIENTED_EDGE('',*,*,#38809,.T.);
#55813=ORIENTED_EDGE('',*,*,#38807,.F.);
#55814=ORIENTED_EDGE('',*,*,#38811,.F.);
#55815=ORIENTED_EDGE('',*,*,#38812,.T.);
#55816=ORIENTED_EDGE('',*,*,#38813,.T.);
#55817=ORIENTED_EDGE('',*,*,#38771,.F.);
#55818=ORIENTED_EDGE('',*,*,#38772,.F.);
#55819=ORIENTED_EDGE('',*,*,#38813,.F.);
#55820=ORIENTED_EDGE('',*,*,#38814,.F.);
#55821=ORIENTED_EDGE('',*,*,#38815,.F.);
#55822=ORIENTED_EDGE('',*,*,#38773,.F.);
#55823=ORIENTED_EDGE('',*,*,#38814,.T.);
#55824=ORIENTED_EDGE('',*,*,#38812,.F.);
#55825=ORIENTED_EDGE('',*,*,#38816,.F.);
#55826=ORIENTED_EDGE('',*,*,#38817,.T.);
#55827=ORIENTED_EDGE('',*,*,#38818,.T.);
#55828=ORIENTED_EDGE('',*,*,#38767,.F.);
#55829=ORIENTED_EDGE('',*,*,#38768,.F.);
#55830=ORIENTED_EDGE('',*,*,#38818,.F.);
#55831=ORIENTED_EDGE('',*,*,#38819,.F.);
#55832=ORIENTED_EDGE('',*,*,#38820,.F.);
#55833=ORIENTED_EDGE('',*,*,#38769,.F.);
#55834=ORIENTED_EDGE('',*,*,#38819,.T.);
#55835=ORIENTED_EDGE('',*,*,#38817,.F.);
#55836=ORIENTED_EDGE('',*,*,#38821,.F.);
#55837=ORIENTED_EDGE('',*,*,#38822,.T.);
#55838=ORIENTED_EDGE('',*,*,#38823,.T.);
#55839=ORIENTED_EDGE('',*,*,#38763,.F.);
#55840=ORIENTED_EDGE('',*,*,#38764,.F.);
#55841=ORIENTED_EDGE('',*,*,#38823,.F.);
#55842=ORIENTED_EDGE('',*,*,#38824,.F.);
#55843=ORIENTED_EDGE('',*,*,#38825,.F.);
#55844=ORIENTED_EDGE('',*,*,#38765,.F.);
#55845=ORIENTED_EDGE('',*,*,#38824,.T.);
#55846=ORIENTED_EDGE('',*,*,#38822,.F.);
#55847=ORIENTED_EDGE('',*,*,#38826,.F.);
#55848=ORIENTED_EDGE('',*,*,#38827,.T.);
#55849=ORIENTED_EDGE('',*,*,#38828,.T.);
#55850=ORIENTED_EDGE('',*,*,#38759,.F.);
#55851=ORIENTED_EDGE('',*,*,#38760,.F.);
#55852=ORIENTED_EDGE('',*,*,#38828,.F.);
#55853=ORIENTED_EDGE('',*,*,#38829,.F.);
#55854=ORIENTED_EDGE('',*,*,#38830,.F.);
#55855=ORIENTED_EDGE('',*,*,#38761,.F.);
#55856=ORIENTED_EDGE('',*,*,#38829,.T.);
#55857=ORIENTED_EDGE('',*,*,#38827,.F.);
#55858=ORIENTED_EDGE('',*,*,#38831,.F.);
#55859=ORIENTED_EDGE('',*,*,#38832,.T.);
#55860=ORIENTED_EDGE('',*,*,#38833,.T.);
#55861=ORIENTED_EDGE('',*,*,#38755,.F.);
#55862=ORIENTED_EDGE('',*,*,#38756,.F.);
#55863=ORIENTED_EDGE('',*,*,#38833,.F.);
#55864=ORIENTED_EDGE('',*,*,#38834,.F.);
#55865=ORIENTED_EDGE('',*,*,#38835,.F.);
#55866=ORIENTED_EDGE('',*,*,#38757,.F.);
#55867=ORIENTED_EDGE('',*,*,#38834,.T.);
#55868=ORIENTED_EDGE('',*,*,#38832,.F.);
#55869=ORIENTED_EDGE('',*,*,#38836,.F.);
#55870=ORIENTED_EDGE('',*,*,#38837,.T.);
#55871=ORIENTED_EDGE('',*,*,#38838,.T.);
#55872=ORIENTED_EDGE('',*,*,#38751,.F.);
#55873=ORIENTED_EDGE('',*,*,#38752,.F.);
#55874=ORIENTED_EDGE('',*,*,#38838,.F.);
#55875=ORIENTED_EDGE('',*,*,#38839,.F.);
#55876=ORIENTED_EDGE('',*,*,#38840,.F.);
#55877=ORIENTED_EDGE('',*,*,#38753,.F.);
#55878=ORIENTED_EDGE('',*,*,#38839,.T.);
#55879=ORIENTED_EDGE('',*,*,#38837,.F.);
#55880=ORIENTED_EDGE('',*,*,#38841,.F.);
#55881=ORIENTED_EDGE('',*,*,#38842,.T.);
#55882=ORIENTED_EDGE('',*,*,#38843,.T.);
#55883=ORIENTED_EDGE('',*,*,#38747,.F.);
#55884=ORIENTED_EDGE('',*,*,#38748,.F.);
#55885=ORIENTED_EDGE('',*,*,#38843,.F.);
#55886=ORIENTED_EDGE('',*,*,#38844,.F.);
#55887=ORIENTED_EDGE('',*,*,#38845,.F.);
#55888=ORIENTED_EDGE('',*,*,#38749,.F.);
#55889=ORIENTED_EDGE('',*,*,#38844,.T.);
#55890=ORIENTED_EDGE('',*,*,#38842,.F.);
#55891=ORIENTED_EDGE('',*,*,#38846,.F.);
#55892=ORIENTED_EDGE('',*,*,#38847,.T.);
#55893=ORIENTED_EDGE('',*,*,#38848,.T.);
#55894=ORIENTED_EDGE('',*,*,#38743,.F.);
#55895=ORIENTED_EDGE('',*,*,#38744,.F.);
#55896=ORIENTED_EDGE('',*,*,#38848,.F.);
#55897=ORIENTED_EDGE('',*,*,#38849,.F.);
#55898=ORIENTED_EDGE('',*,*,#38850,.F.);
#55899=ORIENTED_EDGE('',*,*,#38745,.F.);
#55900=ORIENTED_EDGE('',*,*,#38849,.T.);
#55901=ORIENTED_EDGE('',*,*,#38847,.F.);
#55902=ORIENTED_EDGE('',*,*,#38851,.F.);
#55903=ORIENTED_EDGE('',*,*,#38852,.T.);
#55904=ORIENTED_EDGE('',*,*,#38853,.T.);
#55905=ORIENTED_EDGE('',*,*,#38739,.F.);
#55906=ORIENTED_EDGE('',*,*,#38740,.F.);
#55907=ORIENTED_EDGE('',*,*,#38853,.F.);
#55908=ORIENTED_EDGE('',*,*,#38854,.F.);
#55909=ORIENTED_EDGE('',*,*,#38855,.F.);
#55910=ORIENTED_EDGE('',*,*,#38741,.F.);
#55911=ORIENTED_EDGE('',*,*,#38854,.T.);
#55912=ORIENTED_EDGE('',*,*,#38852,.F.);
#55913=ORIENTED_EDGE('',*,*,#38856,.F.);
#55914=ORIENTED_EDGE('',*,*,#38857,.T.);
#55915=ORIENTED_EDGE('',*,*,#38858,.T.);
#55916=ORIENTED_EDGE('',*,*,#38735,.F.);
#55917=ORIENTED_EDGE('',*,*,#38736,.F.);
#55918=ORIENTED_EDGE('',*,*,#38858,.F.);
#55919=ORIENTED_EDGE('',*,*,#38859,.F.);
#55920=ORIENTED_EDGE('',*,*,#38860,.F.);
#55921=ORIENTED_EDGE('',*,*,#38737,.F.);
#55922=ORIENTED_EDGE('',*,*,#38859,.T.);
#55923=ORIENTED_EDGE('',*,*,#38857,.F.);
#55924=ORIENTED_EDGE('',*,*,#38861,.F.);
#55925=ORIENTED_EDGE('',*,*,#38862,.T.);
#55926=ORIENTED_EDGE('',*,*,#38863,.T.);
#55927=ORIENTED_EDGE('',*,*,#38731,.F.);
#55928=ORIENTED_EDGE('',*,*,#38732,.F.);
#55929=ORIENTED_EDGE('',*,*,#38863,.F.);
#55930=ORIENTED_EDGE('',*,*,#38864,.F.);
#55931=ORIENTED_EDGE('',*,*,#38865,.F.);
#55932=ORIENTED_EDGE('',*,*,#38733,.F.);
#55933=ORIENTED_EDGE('',*,*,#38864,.T.);
#55934=ORIENTED_EDGE('',*,*,#38862,.F.);
#55935=ORIENTED_EDGE('',*,*,#38866,.F.);
#55936=ORIENTED_EDGE('',*,*,#38867,.T.);
#55937=ORIENTED_EDGE('',*,*,#38868,.T.);
#55938=ORIENTED_EDGE('',*,*,#38727,.F.);
#55939=ORIENTED_EDGE('',*,*,#38728,.F.);
#55940=ORIENTED_EDGE('',*,*,#38868,.F.);
#55941=ORIENTED_EDGE('',*,*,#38869,.F.);
#55942=ORIENTED_EDGE('',*,*,#38870,.F.);
#55943=ORIENTED_EDGE('',*,*,#38729,.F.);
#55944=ORIENTED_EDGE('',*,*,#38869,.T.);
#55945=ORIENTED_EDGE('',*,*,#38867,.F.);
#55946=ORIENTED_EDGE('',*,*,#38871,.F.);
#55947=ORIENTED_EDGE('',*,*,#38872,.T.);
#55948=ORIENTED_EDGE('',*,*,#38873,.T.);
#55949=ORIENTED_EDGE('',*,*,#38719,.F.);
#55950=ORIENTED_EDGE('',*,*,#38720,.F.);
#55951=ORIENTED_EDGE('',*,*,#38873,.F.);
#55952=ORIENTED_EDGE('',*,*,#38874,.F.);
#55953=ORIENTED_EDGE('',*,*,#38724,.F.);
#55954=ORIENTED_EDGE('',*,*,#38875,.F.);
#55955=ORIENTED_EDGE('',*,*,#38725,.F.);
#55956=ORIENTED_EDGE('',*,*,#38874,.T.);
#55957=ORIENTED_EDGE('',*,*,#38872,.F.);
#55958=ORIENTED_EDGE('',*,*,#38876,.F.);
#55959=ORIENTED_EDGE('',*,*,#38877,.T.);
#55960=ORIENTED_EDGE('',*,*,#38878,.T.);
#55961=ORIENTED_EDGE('',*,*,#38715,.F.);
#55962=ORIENTED_EDGE('',*,*,#38716,.F.);
#55963=ORIENTED_EDGE('',*,*,#38878,.F.);
#55964=ORIENTED_EDGE('',*,*,#38879,.F.);
#55965=ORIENTED_EDGE('',*,*,#38880,.F.);
#55966=ORIENTED_EDGE('',*,*,#38717,.F.);
#55967=ORIENTED_EDGE('',*,*,#38879,.T.);
#55968=ORIENTED_EDGE('',*,*,#38877,.F.);
#55969=ORIENTED_EDGE('',*,*,#38881,.F.);
#55970=ORIENTED_EDGE('',*,*,#38882,.T.);
#55971=ORIENTED_EDGE('',*,*,#38883,.T.);
#55972=ORIENTED_EDGE('',*,*,#38711,.F.);
#55973=ORIENTED_EDGE('',*,*,#38712,.F.);
#55974=ORIENTED_EDGE('',*,*,#38883,.F.);
#55975=ORIENTED_EDGE('',*,*,#38884,.F.);
#55976=ORIENTED_EDGE('',*,*,#38885,.F.);
#55977=ORIENTED_EDGE('',*,*,#38713,.F.);
#55978=ORIENTED_EDGE('',*,*,#38884,.T.);
#55979=ORIENTED_EDGE('',*,*,#38882,.F.);
#55980=ORIENTED_EDGE('',*,*,#38886,.F.);
#55981=ORIENTED_EDGE('',*,*,#38887,.T.);
#55982=ORIENTED_EDGE('',*,*,#38888,.T.);
#55983=ORIENTED_EDGE('',*,*,#38707,.F.);
#55984=ORIENTED_EDGE('',*,*,#38708,.F.);
#55985=ORIENTED_EDGE('',*,*,#38888,.F.);
#55986=ORIENTED_EDGE('',*,*,#38889,.F.);
#55987=ORIENTED_EDGE('',*,*,#38890,.F.);
#55988=ORIENTED_EDGE('',*,*,#38709,.F.);
#55989=ORIENTED_EDGE('',*,*,#38889,.T.);
#55990=ORIENTED_EDGE('',*,*,#38887,.F.);
#55991=ORIENTED_EDGE('',*,*,#38891,.F.);
#55992=ORIENTED_EDGE('',*,*,#38892,.T.);
#55993=ORIENTED_EDGE('',*,*,#38893,.T.);
#55994=ORIENTED_EDGE('',*,*,#38703,.F.);
#55995=ORIENTED_EDGE('',*,*,#38704,.F.);
#55996=ORIENTED_EDGE('',*,*,#38893,.F.);
#55997=ORIENTED_EDGE('',*,*,#38894,.F.);
#55998=ORIENTED_EDGE('',*,*,#38895,.F.);
#55999=ORIENTED_EDGE('',*,*,#38705,.F.);
#56000=ORIENTED_EDGE('',*,*,#38894,.T.);
#56001=ORIENTED_EDGE('',*,*,#38892,.F.);
#56002=ORIENTED_EDGE('',*,*,#38896,.F.);
#56003=ORIENTED_EDGE('',*,*,#38897,.T.);
#56004=ORIENTED_EDGE('',*,*,#38898,.T.);
#56005=ORIENTED_EDGE('',*,*,#38699,.F.);
#56006=ORIENTED_EDGE('',*,*,#38700,.F.);
#56007=ORIENTED_EDGE('',*,*,#38898,.F.);
#56008=ORIENTED_EDGE('',*,*,#38899,.F.);
#56009=ORIENTED_EDGE('',*,*,#38900,.F.);
#56010=ORIENTED_EDGE('',*,*,#38701,.F.);
#56011=ORIENTED_EDGE('',*,*,#38899,.T.);
#56012=ORIENTED_EDGE('',*,*,#38897,.F.);
#56013=ORIENTED_EDGE('',*,*,#38901,.F.);
#56014=ORIENTED_EDGE('',*,*,#38902,.T.);
#56015=ORIENTED_EDGE('',*,*,#38903,.T.);
#56016=ORIENTED_EDGE('',*,*,#38695,.F.);
#56017=ORIENTED_EDGE('',*,*,#38696,.F.);
#56018=ORIENTED_EDGE('',*,*,#38903,.F.);
#56019=ORIENTED_EDGE('',*,*,#38904,.F.);
#56020=ORIENTED_EDGE('',*,*,#38905,.F.);
#56021=ORIENTED_EDGE('',*,*,#38697,.F.);
#56022=ORIENTED_EDGE('',*,*,#38904,.T.);
#56023=ORIENTED_EDGE('',*,*,#38902,.F.);
#56024=ORIENTED_EDGE('',*,*,#38906,.F.);
#56025=ORIENTED_EDGE('',*,*,#38907,.T.);
#56026=ORIENTED_EDGE('',*,*,#38908,.T.);
#56027=ORIENTED_EDGE('',*,*,#38691,.F.);
#56028=ORIENTED_EDGE('',*,*,#38692,.F.);
#56029=ORIENTED_EDGE('',*,*,#38908,.F.);
#56030=ORIENTED_EDGE('',*,*,#38909,.F.);
#56031=ORIENTED_EDGE('',*,*,#38910,.F.);
#56032=ORIENTED_EDGE('',*,*,#38693,.F.);
#56033=ORIENTED_EDGE('',*,*,#38909,.T.);
#56034=ORIENTED_EDGE('',*,*,#38907,.F.);
#56035=ORIENTED_EDGE('',*,*,#38911,.F.);
#56036=ORIENTED_EDGE('',*,*,#38912,.T.);
#56037=ORIENTED_EDGE('',*,*,#38913,.T.);
#56038=ORIENTED_EDGE('',*,*,#38687,.F.);
#56039=ORIENTED_EDGE('',*,*,#38688,.F.);
#56040=ORIENTED_EDGE('',*,*,#38913,.F.);
#56041=ORIENTED_EDGE('',*,*,#38914,.F.);
#56042=ORIENTED_EDGE('',*,*,#38915,.F.);
#56043=ORIENTED_EDGE('',*,*,#38689,.F.);
#56044=ORIENTED_EDGE('',*,*,#38914,.T.);
#56045=ORIENTED_EDGE('',*,*,#38912,.F.);
#56046=ORIENTED_EDGE('',*,*,#38916,.F.);
#56047=ORIENTED_EDGE('',*,*,#38917,.T.);
#56048=ORIENTED_EDGE('',*,*,#38918,.T.);
#56049=ORIENTED_EDGE('',*,*,#38683,.F.);
#56050=ORIENTED_EDGE('',*,*,#38684,.F.);
#56051=ORIENTED_EDGE('',*,*,#38918,.F.);
#56052=ORIENTED_EDGE('',*,*,#38919,.F.);
#56053=ORIENTED_EDGE('',*,*,#38920,.F.);
#56054=ORIENTED_EDGE('',*,*,#38685,.F.);
#56055=ORIENTED_EDGE('',*,*,#38919,.T.);
#56056=ORIENTED_EDGE('',*,*,#38917,.F.);
#56057=ORIENTED_EDGE('',*,*,#38921,.F.);
#56058=ORIENTED_EDGE('',*,*,#38922,.T.);
#56059=ORIENTED_EDGE('',*,*,#38923,.T.);
#56060=ORIENTED_EDGE('',*,*,#38679,.F.);
#56061=ORIENTED_EDGE('',*,*,#38680,.F.);
#56062=ORIENTED_EDGE('',*,*,#38923,.F.);
#56063=ORIENTED_EDGE('',*,*,#38924,.F.);
#56064=ORIENTED_EDGE('',*,*,#38925,.F.);
#56065=ORIENTED_EDGE('',*,*,#38681,.F.);
#56066=ORIENTED_EDGE('',*,*,#38924,.T.);
#56067=ORIENTED_EDGE('',*,*,#38922,.F.);
#56068=ORIENTED_EDGE('',*,*,#38926,.F.);
#56069=ORIENTED_EDGE('',*,*,#38927,.T.);
#56070=ORIENTED_EDGE('',*,*,#38928,.T.);
#56071=ORIENTED_EDGE('',*,*,#38675,.F.);
#56072=ORIENTED_EDGE('',*,*,#38676,.F.);
#56073=ORIENTED_EDGE('',*,*,#38928,.F.);
#56074=ORIENTED_EDGE('',*,*,#38929,.F.);
#56075=ORIENTED_EDGE('',*,*,#38930,.F.);
#56076=ORIENTED_EDGE('',*,*,#38677,.F.);
#56077=ORIENTED_EDGE('',*,*,#38929,.T.);
#56078=ORIENTED_EDGE('',*,*,#38927,.F.);
#56079=ORIENTED_EDGE('',*,*,#38931,.F.);
#56080=ORIENTED_EDGE('',*,*,#38932,.T.);
#56081=ORIENTED_EDGE('',*,*,#38933,.T.);
#56082=ORIENTED_EDGE('',*,*,#38671,.F.);
#56083=ORIENTED_EDGE('',*,*,#38672,.F.);
#56084=ORIENTED_EDGE('',*,*,#38933,.F.);
#56085=ORIENTED_EDGE('',*,*,#38934,.F.);
#56086=ORIENTED_EDGE('',*,*,#38935,.F.);
#56087=ORIENTED_EDGE('',*,*,#38673,.F.);
#56088=ORIENTED_EDGE('',*,*,#38934,.T.);
#56089=ORIENTED_EDGE('',*,*,#38932,.F.);
#56090=ORIENTED_EDGE('',*,*,#38936,.F.);
#56091=ORIENTED_EDGE('',*,*,#38937,.T.);
#56092=ORIENTED_EDGE('',*,*,#38938,.T.);
#56093=ORIENTED_EDGE('',*,*,#38667,.F.);
#56094=ORIENTED_EDGE('',*,*,#38668,.F.);
#56095=ORIENTED_EDGE('',*,*,#38938,.F.);
#56096=ORIENTED_EDGE('',*,*,#38939,.F.);
#56097=ORIENTED_EDGE('',*,*,#38940,.F.);
#56098=ORIENTED_EDGE('',*,*,#38669,.F.);
#56099=ORIENTED_EDGE('',*,*,#38939,.T.);
#56100=ORIENTED_EDGE('',*,*,#38937,.F.);
#56101=ORIENTED_EDGE('',*,*,#38941,.F.);
#56102=ORIENTED_EDGE('',*,*,#38942,.T.);
#56103=ORIENTED_EDGE('',*,*,#38943,.T.);
#56104=ORIENTED_EDGE('',*,*,#38663,.F.);
#56105=ORIENTED_EDGE('',*,*,#38664,.F.);
#56106=ORIENTED_EDGE('',*,*,#38943,.F.);
#56107=ORIENTED_EDGE('',*,*,#38944,.F.);
#56108=ORIENTED_EDGE('',*,*,#38945,.F.);
#56109=ORIENTED_EDGE('',*,*,#38665,.F.);
#56110=ORIENTED_EDGE('',*,*,#38944,.T.);
#56111=ORIENTED_EDGE('',*,*,#38942,.F.);
#56112=ORIENTED_EDGE('',*,*,#38946,.F.);
#56113=ORIENTED_EDGE('',*,*,#38947,.T.);
#56114=ORIENTED_EDGE('',*,*,#38948,.T.);
#56115=ORIENTED_EDGE('',*,*,#38659,.F.);
#56116=ORIENTED_EDGE('',*,*,#38660,.F.);
#56117=ORIENTED_EDGE('',*,*,#38948,.F.);
#56118=ORIENTED_EDGE('',*,*,#38949,.F.);
#56119=ORIENTED_EDGE('',*,*,#38950,.F.);
#56120=ORIENTED_EDGE('',*,*,#38661,.F.);
#56121=ORIENTED_EDGE('',*,*,#38949,.T.);
#56122=ORIENTED_EDGE('',*,*,#38947,.F.);
#56123=ORIENTED_EDGE('',*,*,#38951,.F.);
#56124=ORIENTED_EDGE('',*,*,#38952,.T.);
#56125=ORIENTED_EDGE('',*,*,#38953,.T.);
#56126=ORIENTED_EDGE('',*,*,#38655,.F.);
#56127=ORIENTED_EDGE('',*,*,#38656,.F.);
#56128=ORIENTED_EDGE('',*,*,#38953,.F.);
#56129=ORIENTED_EDGE('',*,*,#38954,.F.);
#56130=ORIENTED_EDGE('',*,*,#38955,.F.);
#56131=ORIENTED_EDGE('',*,*,#38657,.F.);
#56132=ORIENTED_EDGE('',*,*,#38954,.T.);
#56133=ORIENTED_EDGE('',*,*,#38952,.F.);
#56134=ORIENTED_EDGE('',*,*,#38956,.F.);
#56135=ORIENTED_EDGE('',*,*,#38957,.T.);
#56136=ORIENTED_EDGE('',*,*,#38958,.T.);
#56137=ORIENTED_EDGE('',*,*,#38651,.F.);
#56138=ORIENTED_EDGE('',*,*,#38652,.F.);
#56139=ORIENTED_EDGE('',*,*,#38958,.F.);
#56140=ORIENTED_EDGE('',*,*,#38959,.F.);
#56141=ORIENTED_EDGE('',*,*,#38960,.F.);
#56142=ORIENTED_EDGE('',*,*,#38653,.F.);
#56143=ORIENTED_EDGE('',*,*,#38959,.T.);
#56144=ORIENTED_EDGE('',*,*,#38957,.F.);
#56145=ORIENTED_EDGE('',*,*,#38961,.F.);
#56146=ORIENTED_EDGE('',*,*,#38962,.T.);
#56147=ORIENTED_EDGE('',*,*,#38963,.T.);
#56148=ORIENTED_EDGE('',*,*,#38647,.F.);
#56149=ORIENTED_EDGE('',*,*,#38648,.F.);
#56150=ORIENTED_EDGE('',*,*,#38963,.F.);
#56151=ORIENTED_EDGE('',*,*,#38964,.F.);
#56152=ORIENTED_EDGE('',*,*,#38965,.F.);
#56153=ORIENTED_EDGE('',*,*,#38649,.F.);
#56154=ORIENTED_EDGE('',*,*,#38964,.T.);
#56155=ORIENTED_EDGE('',*,*,#38962,.F.);
#56156=ORIENTED_EDGE('',*,*,#38723,.T.);
#56157=ORIENTED_EDGE('',*,*,#38966,.T.);
#56158=ORIENTED_EDGE('',*,*,#38635,.T.);
#56159=ORIENTED_EDGE('',*,*,#38966,.F.);
#56160=ORIENTED_EDGE('',*,*,#38722,.T.);
#56161=ORIENTED_EDGE('',*,*,#38967,.T.);
#56162=ORIENTED_EDGE('',*,*,#38968,.T.);
#56163=ORIENTED_EDGE('',*,*,#38871,.T.);
#56164=ORIENTED_EDGE('',*,*,#38718,.T.);
#56165=ORIENTED_EDGE('',*,*,#38880,.T.);
#56166=ORIENTED_EDGE('',*,*,#38876,.T.);
#56167=ORIENTED_EDGE('',*,*,#38714,.T.);
#56168=ORIENTED_EDGE('',*,*,#38885,.T.);
#56169=ORIENTED_EDGE('',*,*,#38881,.T.);
#56170=ORIENTED_EDGE('',*,*,#38710,.T.);
#56171=ORIENTED_EDGE('',*,*,#38890,.T.);
#56172=ORIENTED_EDGE('',*,*,#38886,.T.);
#56173=ORIENTED_EDGE('',*,*,#38706,.T.);
#56174=ORIENTED_EDGE('',*,*,#38895,.T.);
#56175=ORIENTED_EDGE('',*,*,#38891,.T.);
#56176=ORIENTED_EDGE('',*,*,#38702,.T.);
#56177=ORIENTED_EDGE('',*,*,#38900,.T.);
#56178=ORIENTED_EDGE('',*,*,#38896,.T.);
#56179=ORIENTED_EDGE('',*,*,#38698,.T.);
#56180=ORIENTED_EDGE('',*,*,#38905,.T.);
#56181=ORIENTED_EDGE('',*,*,#38901,.T.);
#56182=ORIENTED_EDGE('',*,*,#38694,.T.);
#56183=ORIENTED_EDGE('',*,*,#38910,.T.);
#56184=ORIENTED_EDGE('',*,*,#38906,.T.);
#56185=ORIENTED_EDGE('',*,*,#38690,.T.);
#56186=ORIENTED_EDGE('',*,*,#38915,.T.);
#56187=ORIENTED_EDGE('',*,*,#38911,.T.);
#56188=ORIENTED_EDGE('',*,*,#38686,.T.);
#56189=ORIENTED_EDGE('',*,*,#38920,.T.);
#56190=ORIENTED_EDGE('',*,*,#38916,.T.);
#56191=ORIENTED_EDGE('',*,*,#38682,.T.);
#56192=ORIENTED_EDGE('',*,*,#38925,.T.);
#56193=ORIENTED_EDGE('',*,*,#38921,.T.);
#56194=ORIENTED_EDGE('',*,*,#38678,.T.);
#56195=ORIENTED_EDGE('',*,*,#38930,.T.);
#56196=ORIENTED_EDGE('',*,*,#38926,.T.);
#56197=ORIENTED_EDGE('',*,*,#38674,.T.);
#56198=ORIENTED_EDGE('',*,*,#38935,.T.);
#56199=ORIENTED_EDGE('',*,*,#38931,.T.);
#56200=ORIENTED_EDGE('',*,*,#38670,.T.);
#56201=ORIENTED_EDGE('',*,*,#38940,.T.);
#56202=ORIENTED_EDGE('',*,*,#38936,.T.);
#56203=ORIENTED_EDGE('',*,*,#38666,.T.);
#56204=ORIENTED_EDGE('',*,*,#38945,.T.);
#56205=ORIENTED_EDGE('',*,*,#38941,.T.);
#56206=ORIENTED_EDGE('',*,*,#38662,.T.);
#56207=ORIENTED_EDGE('',*,*,#38950,.T.);
#56208=ORIENTED_EDGE('',*,*,#38946,.T.);
#56209=ORIENTED_EDGE('',*,*,#38658,.T.);
#56210=ORIENTED_EDGE('',*,*,#38955,.T.);
#56211=ORIENTED_EDGE('',*,*,#38951,.T.);
#56212=ORIENTED_EDGE('',*,*,#38654,.T.);
#56213=ORIENTED_EDGE('',*,*,#38960,.T.);
#56214=ORIENTED_EDGE('',*,*,#38956,.T.);
#56215=ORIENTED_EDGE('',*,*,#38650,.T.);
#56216=ORIENTED_EDGE('',*,*,#38965,.T.);
#56217=ORIENTED_EDGE('',*,*,#38961,.T.);
#56218=ORIENTED_EDGE('',*,*,#38646,.T.);
#56219=ORIENTED_EDGE('',*,*,#38644,.T.);
#56220=ORIENTED_EDGE('',*,*,#38638,.T.);
#56221=ORIENTED_EDGE('',*,*,#38790,.T.);
#56222=ORIENTED_EDGE('',*,*,#38795,.T.);
#56223=ORIENTED_EDGE('',*,*,#38791,.T.);
#56224=ORIENTED_EDGE('',*,*,#38786,.T.);
#56225=ORIENTED_EDGE('',*,*,#38800,.T.);
#56226=ORIENTED_EDGE('',*,*,#38796,.T.);
#56227=ORIENTED_EDGE('',*,*,#38782,.T.);
#56228=ORIENTED_EDGE('',*,*,#38805,.T.);
#56229=ORIENTED_EDGE('',*,*,#38801,.T.);
#56230=ORIENTED_EDGE('',*,*,#38778,.T.);
#56231=ORIENTED_EDGE('',*,*,#38810,.T.);
#56232=ORIENTED_EDGE('',*,*,#38806,.T.);
#56233=ORIENTED_EDGE('',*,*,#38774,.T.);
#56234=ORIENTED_EDGE('',*,*,#38815,.T.);
#56235=ORIENTED_EDGE('',*,*,#38811,.T.);
#56236=ORIENTED_EDGE('',*,*,#38770,.T.);
#56237=ORIENTED_EDGE('',*,*,#38820,.T.);
#56238=ORIENTED_EDGE('',*,*,#38816,.T.);
#56239=ORIENTED_EDGE('',*,*,#38766,.T.);
#56240=ORIENTED_EDGE('',*,*,#38825,.T.);
#56241=ORIENTED_EDGE('',*,*,#38821,.T.);
#56242=ORIENTED_EDGE('',*,*,#38762,.T.);
#56243=ORIENTED_EDGE('',*,*,#38830,.T.);
#56244=ORIENTED_EDGE('',*,*,#38826,.T.);
#56245=ORIENTED_EDGE('',*,*,#38758,.T.);
#56246=ORIENTED_EDGE('',*,*,#38835,.T.);
#56247=ORIENTED_EDGE('',*,*,#38831,.T.);
#56248=ORIENTED_EDGE('',*,*,#38754,.T.);
#56249=ORIENTED_EDGE('',*,*,#38840,.T.);
#56250=ORIENTED_EDGE('',*,*,#38836,.T.);
#56251=ORIENTED_EDGE('',*,*,#38750,.T.);
#56252=ORIENTED_EDGE('',*,*,#38845,.T.);
#56253=ORIENTED_EDGE('',*,*,#38841,.T.);
#56254=ORIENTED_EDGE('',*,*,#38746,.T.);
#56255=ORIENTED_EDGE('',*,*,#38850,.T.);
#56256=ORIENTED_EDGE('',*,*,#38846,.T.);
#56257=ORIENTED_EDGE('',*,*,#38742,.T.);
#56258=ORIENTED_EDGE('',*,*,#38855,.T.);
#56259=ORIENTED_EDGE('',*,*,#38851,.T.);
#56260=ORIENTED_EDGE('',*,*,#38738,.T.);
#56261=ORIENTED_EDGE('',*,*,#38860,.T.);
#56262=ORIENTED_EDGE('',*,*,#38856,.T.);
#56263=ORIENTED_EDGE('',*,*,#38734,.T.);
#56264=ORIENTED_EDGE('',*,*,#38865,.T.);
#56265=ORIENTED_EDGE('',*,*,#38861,.T.);
#56266=ORIENTED_EDGE('',*,*,#38730,.T.);
#56267=ORIENTED_EDGE('',*,*,#38870,.T.);
#56268=ORIENTED_EDGE('',*,*,#38866,.T.);
#56269=ORIENTED_EDGE('',*,*,#38726,.T.);
#56270=ORIENTED_EDGE('',*,*,#38875,.T.);
#56271=ORIENTED_EDGE('',*,*,#38968,.F.);
#56272=ORIENTED_EDGE('',*,*,#38967,.F.);
#56273=ORIENTED_EDGE('',*,*,#38969,.T.);
#56274=ORIENTED_EDGE('',*,*,#38969,.F.);
#56275=ORIENTED_EDGE('',*,*,#38970,.T.);
#56276=ORIENTED_EDGE('',*,*,#38971,.F.);
#56277=ORIENTED_EDGE('',*,*,#38972,.T.);
#56278=ORIENTED_EDGE('',*,*,#38973,.F.);
#56279=ORIENTED_EDGE('',*,*,#38974,.F.);
#56280=ORIENTED_EDGE('',*,*,#38975,.T.);
#56281=ORIENTED_EDGE('',*,*,#38976,.F.);
#56282=ORIENTED_EDGE('',*,*,#38977,.F.);
#56283=ORIENTED_EDGE('',*,*,#38978,.T.);
#56284=ORIENTED_EDGE('',*,*,#38979,.F.);
#56285=ORIENTED_EDGE('',*,*,#38980,.F.);
#56286=ORIENTED_EDGE('',*,*,#38981,.T.);
#56287=ORIENTED_EDGE('',*,*,#38982,.F.);
#56288=ORIENTED_EDGE('',*,*,#38983,.F.);
#56289=ORIENTED_EDGE('',*,*,#38984,.T.);
#56290=ORIENTED_EDGE('',*,*,#38985,.F.);
#56291=ORIENTED_EDGE('',*,*,#38986,.F.);
#56292=ORIENTED_EDGE('',*,*,#38987,.T.);
#56293=ORIENTED_EDGE('',*,*,#38988,.F.);
#56294=ORIENTED_EDGE('',*,*,#38970,.F.);
#56295=ORIENTED_EDGE('',*,*,#38989,.F.);
#56296=ORIENTED_EDGE('',*,*,#38975,.F.);
#56297=ORIENTED_EDGE('',*,*,#38990,.F.);
#56298=ORIENTED_EDGE('',*,*,#38991,.F.);
#56299=ORIENTED_EDGE('',*,*,#38992,.F.);
#56300=ORIENTED_EDGE('',*,*,#38978,.F.);
#56301=ORIENTED_EDGE('',*,*,#38993,.F.);
#56302=ORIENTED_EDGE('',*,*,#38994,.F.);
#56303=ORIENTED_EDGE('',*,*,#38995,.F.);
#56304=ORIENTED_EDGE('',*,*,#38996,.F.);
#56305=ORIENTED_EDGE('',*,*,#38997,.F.);
#56306=ORIENTED_EDGE('',*,*,#38972,.F.);
#56307=ORIENTED_EDGE('',*,*,#38998,.F.);
#56308=ORIENTED_EDGE('',*,*,#38981,.F.);
#56309=ORIENTED_EDGE('',*,*,#38999,.F.);
#56310=ORIENTED_EDGE('',*,*,#39000,.F.);
#56311=ORIENTED_EDGE('',*,*,#39001,.F.);
#56312=ORIENTED_EDGE('',*,*,#39002,.F.);
#56313=ORIENTED_EDGE('',*,*,#39003,.F.);
#56314=ORIENTED_EDGE('',*,*,#38987,.F.);
#56315=ORIENTED_EDGE('',*,*,#39004,.F.);
#56316=ORIENTED_EDGE('',*,*,#39005,.F.);
#56317=ORIENTED_EDGE('',*,*,#39006,.F.);
#56318=ORIENTED_EDGE('',*,*,#38984,.F.);
#56319=ORIENTED_EDGE('',*,*,#38982,.T.);
#56320=ORIENTED_EDGE('',*,*,#38998,.T.);
#56321=ORIENTED_EDGE('',*,*,#39007,.F.);
#56322=ORIENTED_EDGE('',*,*,#38999,.T.);
#56323=ORIENTED_EDGE('',*,*,#38980,.T.);
#56324=ORIENTED_EDGE('',*,*,#39008,.T.);
#56325=ORIENTED_EDGE('',*,*,#39009,.T.);
#56326=ORIENTED_EDGE('',*,*,#39010,.F.);
#56327=ORIENTED_EDGE('',*,*,#38979,.T.);
#56328=ORIENTED_EDGE('',*,*,#38992,.T.);
#56329=ORIENTED_EDGE('',*,*,#39011,.F.);
#56330=ORIENTED_EDGE('',*,*,#38993,.T.);
#56331=ORIENTED_EDGE('',*,*,#38977,.T.);
#56332=ORIENTED_EDGE('',*,*,#39012,.T.);
#56333=ORIENTED_EDGE('',*,*,#39013,.T.);
#56334=ORIENTED_EDGE('',*,*,#39008,.F.);
#56335=ORIENTED_EDGE('',*,*,#38976,.T.);
#56336=ORIENTED_EDGE('',*,*,#38989,.T.);
#56337=ORIENTED_EDGE('',*,*,#39014,.F.);
#56338=ORIENTED_EDGE('',*,*,#38990,.T.);
#56339=ORIENTED_EDGE('',*,*,#38974,.T.);
#56340=ORIENTED_EDGE('',*,*,#39015,.T.);
#56341=ORIENTED_EDGE('',*,*,#39016,.T.);
#56342=ORIENTED_EDGE('',*,*,#39012,.F.);
#56343=ORIENTED_EDGE('',*,*,#38991,.T.);
#56344=ORIENTED_EDGE('',*,*,#39014,.T.);
#56345=ORIENTED_EDGE('',*,*,#38994,.T.);
#56346=ORIENTED_EDGE('',*,*,#39011,.T.);
#56347=ORIENTED_EDGE('',*,*,#38996,.T.);
#56348=ORIENTED_EDGE('',*,*,#39017,.T.);
#56349=ORIENTED_EDGE('',*,*,#39000,.T.);
#56350=ORIENTED_EDGE('',*,*,#39007,.T.);
#56351=ORIENTED_EDGE('',*,*,#39002,.T.);
#56352=ORIENTED_EDGE('',*,*,#39018,.T.);
#56353=ORIENTED_EDGE('',*,*,#39005,.T.);
#56354=ORIENTED_EDGE('',*,*,#39019,.T.);
#56355=ORIENTED_EDGE('',*,*,#39020,.F.);
#56356=ORIENTED_EDGE('',*,*,#39021,.T.);
#56357=ORIENTED_EDGE('',*,*,#39016,.F.);
#56358=ORIENTED_EDGE('',*,*,#39022,.T.);
#56359=ORIENTED_EDGE('',*,*,#39013,.F.);
#56360=ORIENTED_EDGE('',*,*,#39023,.T.);
#56361=ORIENTED_EDGE('',*,*,#39009,.F.);
#56362=ORIENTED_EDGE('',*,*,#39024,.T.);
#56363=ORIENTED_EDGE('',*,*,#39025,.F.);
#56364=ORIENTED_EDGE('',*,*,#39026,.T.);
#56365=ORIENTED_EDGE('',*,*,#39027,.F.);
#56366=ORIENTED_EDGE('',*,*,#39028,.T.);
#56367=ORIENTED_EDGE('',*,*,#39024,.F.);
#56368=ORIENTED_EDGE('',*,*,#39023,.F.);
#56369=ORIENTED_EDGE('',*,*,#39022,.F.);
#56370=ORIENTED_EDGE('',*,*,#39021,.F.);
#56371=ORIENTED_EDGE('',*,*,#39029,.T.);
#56372=ORIENTED_EDGE('',*,*,#39029,.F.);
#56373=ORIENTED_EDGE('',*,*,#39028,.F.);
#56374=ORIENTED_EDGE('',*,*,#39026,.F.);
#56375=ORIENTED_EDGE('',*,*,#38971,.T.);
#56376=ORIENTED_EDGE('',*,*,#39030,.T.);
#56377=ORIENTED_EDGE('',*,*,#39020,.T.);
#56378=ORIENTED_EDGE('',*,*,#39015,.F.);
#56379=ORIENTED_EDGE('',*,*,#38973,.T.);
#56380=ORIENTED_EDGE('',*,*,#38997,.T.);
#56381=ORIENTED_EDGE('',*,*,#39017,.F.);
#56382=ORIENTED_EDGE('',*,*,#38995,.T.);
#56383=ORIENTED_EDGE('',*,*,#38986,.T.);
#56384=ORIENTED_EDGE('',*,*,#39031,.T.);
#56385=ORIENTED_EDGE('',*,*,#39027,.T.);
#56386=ORIENTED_EDGE('',*,*,#39030,.F.);
#56387=ORIENTED_EDGE('',*,*,#38988,.T.);
#56388=ORIENTED_EDGE('',*,*,#39003,.T.);
#56389=ORIENTED_EDGE('',*,*,#39018,.F.);
#56390=ORIENTED_EDGE('',*,*,#39001,.T.);
#56391=ORIENTED_EDGE('',*,*,#38983,.T.);
#56392=ORIENTED_EDGE('',*,*,#39010,.T.);
#56393=ORIENTED_EDGE('',*,*,#39025,.T.);
#56394=ORIENTED_EDGE('',*,*,#39031,.F.);
#56395=ORIENTED_EDGE('',*,*,#38985,.T.);
#56396=ORIENTED_EDGE('',*,*,#39006,.T.);
#56397=ORIENTED_EDGE('',*,*,#39019,.F.);
#56398=ORIENTED_EDGE('',*,*,#39004,.T.);
#56399=ORIENTED_EDGE('',*,*,#39032,.F.);
#56400=ORIENTED_EDGE('',*,*,#39033,.F.);
#56401=ORIENTED_EDGE('',*,*,#39034,.T.);
#56402=ORIENTED_EDGE('',*,*,#39032,.T.);
#56403=ORIENTED_EDGE('',*,*,#39034,.F.);
#56404=ORIENTED_EDGE('',*,*,#39035,.F.);
#56405=ORIENTED_EDGE('',*,*,#39036,.T.);
#56406=ORIENTED_EDGE('',*,*,#39033,.T.);
#56407=ORIENTED_EDGE('',*,*,#39036,.F.);
#56408=ORIENTED_EDGE('',*,*,#39037,.F.);
#56409=ORIENTED_EDGE('',*,*,#39038,.T.);
#56410=ORIENTED_EDGE('',*,*,#39035,.T.);
#56411=ORIENTED_EDGE('',*,*,#39038,.F.);
#56412=ORIENTED_EDGE('',*,*,#39037,.T.);
#56413=B_SPLINE_SURFACE_WITH_KNOTS('',2,1,((#76146,#76147),(#76148,#76149),
(#76150,#76151)),.UNSPECIFIED.,.F.,.F.,.F.,(3,3),(2,2),(0.,1.),(0.,0.0149999999999997),
 .UNSPECIFIED.);
#56414=B_SPLINE_SURFACE_WITH_KNOTS('',2,1,((#76164,#76165),(#76166,#76167),
(#76168,#76169)),.UNSPECIFIED.,.F.,.F.,.F.,(3,3),(2,2),(0.,1.),(0.,0.0149999999999997),
 .UNSPECIFIED.);
#56415=B_SPLINE_SURFACE_WITH_KNOTS('',2,1,((#76179,#76180),(#76181,#76182),
(#76183,#76184)),.UNSPECIFIED.,.F.,.F.,.F.,(3,3),(2,2),(0.,1.),(0.,0.0149999999999997),
 .UNSPECIFIED.);
#56416=B_SPLINE_SURFACE_WITH_KNOTS('',2,1,((#76194,#76195),(#76196,#76197),
(#76198,#76199)),.UNSPECIFIED.,.F.,.F.,.F.,(3,3),(2,2),(0.,1.),(0.,0.0149999999999997),
 .UNSPECIFIED.);
#56417=B_SPLINE_SURFACE_WITH_KNOTS('',2,1,((#76209,#76210),(#76211,#76212),
(#76213,#76214)),.UNSPECIFIED.,.F.,.F.,.F.,(3,3),(2,2),(0.,1.),(0.,0.0149999999999997),
 .UNSPECIFIED.);
#56418=B_SPLINE_SURFACE_WITH_KNOTS('',2,1,((#76224,#76225),(#76226,#76227),
(#76228,#76229)),.UNSPECIFIED.,.F.,.F.,.F.,(3,3),(2,2),(0.,1.),(0.,0.0149999999999997),
 .UNSPECIFIED.);
#56419=B_SPLINE_SURFACE_WITH_KNOTS('',2,1,((#76239,#76240),(#76241,#76242),
(#76243,#76244)),.UNSPECIFIED.,.F.,.F.,.F.,(3,3),(2,2),(0.,1.),(0.,0.0149999999999997),
 .UNSPECIFIED.);
#56420=B_SPLINE_SURFACE_WITH_KNOTS('',2,1,((#76254,#76255),(#76256,#76257),
(#76258,#76259)),.UNSPECIFIED.,.F.,.F.,.F.,(3,3),(2,2),(0.,1.),(0.,0.0149999999999997),
 .UNSPECIFIED.);
#56421=B_SPLINE_SURFACE_WITH_KNOTS('',2,1,((#76266,#76267),(#76268,#76269),
(#76270,#76271)),.UNSPECIFIED.,.F.,.F.,.F.,(3,3),(2,2),(0.,1.),(0.,0.0149999999999997),
 .UNSPECIFIED.);
#56422=B_SPLINE_SURFACE_WITH_KNOTS('',2,1,((#76284,#76285),(#76286,#76287),
(#76288,#76289)),.UNSPECIFIED.,.F.,.F.,.F.,(3,3),(2,2),(0.,1.),(0.,0.0149999999999997),
 .UNSPECIFIED.);
#56423=B_SPLINE_SURFACE_WITH_KNOTS('',2,1,((#76299,#76300),(#76301,#76302),
(#76303,#76304)),.UNSPECIFIED.,.F.,.F.,.F.,(3,3),(2,2),(0.,1.),(0.,0.0149999999999997),
 .UNSPECIFIED.);
#56424=B_SPLINE_SURFACE_WITH_KNOTS('',2,1,((#76314,#76315),(#76316,#76317),
(#76318,#76319)),.UNSPECIFIED.,.F.,.F.,.F.,(3,3),(2,2),(0.,1.),(0.,0.0149999999999997),
 .UNSPECIFIED.);
#56425=B_SPLINE_SURFACE_WITH_KNOTS('',2,1,((#76329,#76330),(#76331,#76332),
(#76333,#76334)),.UNSPECIFIED.,.F.,.F.,.F.,(3,3),(2,2),(0.,1.),(0.,0.0149999999999997),
 .UNSPECIFIED.);
#56426=B_SPLINE_SURFACE_WITH_KNOTS('',2,1,((#76344,#76345),(#76346,#76347),
(#76348,#76349)),.UNSPECIFIED.,.F.,.F.,.F.,(3,3),(2,2),(0.,1.),(0.,0.0149999999999997),
 .UNSPECIFIED.);
#56427=B_SPLINE_SURFACE_WITH_KNOTS('',2,1,((#76359,#76360),(#76361,#76362),
(#76363,#76364)),.UNSPECIFIED.,.F.,.F.,.F.,(3,3),(2,2),(0.,1.),(0.,0.0149999999999997),
 .UNSPECIFIED.);
#56428=B_SPLINE_SURFACE_WITH_KNOTS('',2,1,((#76374,#76375),(#76376,#76377),
(#76378,#76379)),.UNSPECIFIED.,.F.,.F.,.F.,(3,3),(2,2),(0.,1.),(0.,0.0149999999999997),
 .UNSPECIFIED.);
#56429=B_SPLINE_SURFACE_WITH_KNOTS('',2,1,((#76389,#76390),(#76391,#76392),
(#76393,#76394)),.UNSPECIFIED.,.F.,.F.,.F.,(3,3),(2,2),(0.,1.),(0.,0.0149999999999997),
 .UNSPECIFIED.);
#56430=B_SPLINE_SURFACE_WITH_KNOTS('',2,1,((#76404,#76405),(#76406,#76407),
(#76408,#76409)),.UNSPECIFIED.,.F.,.F.,.F.,(3,3),(2,2),(0.,1.),(0.,0.0149999999999997),
 .UNSPECIFIED.);
#56431=B_SPLINE_SURFACE_WITH_KNOTS('',2,1,((#76419,#76420),(#76421,#76422),
(#76423,#76424)),.UNSPECIFIED.,.F.,.F.,.F.,(3,3),(2,2),(0.,1.),(0.,0.0149999999999997),
 .UNSPECIFIED.);
#56432=B_SPLINE_SURFACE_WITH_KNOTS('',2,1,((#76434,#76435),(#76436,#76437),
(#76438,#76439)),.UNSPECIFIED.,.F.,.F.,.F.,(3,3),(2,2),(0.,1.),(0.,0.0149999999999997),
 .UNSPECIFIED.);
#56433=B_SPLINE_SURFACE_WITH_KNOTS('',2,1,((#76447,#76448),(#76449,#76450),
(#76451,#76452)),.UNSPECIFIED.,.F.,.F.,.F.,(3,3),(2,2),(0.,1.),(0.,0.0149999999999997),
 .UNSPECIFIED.);
#56434=B_SPLINE_SURFACE_WITH_KNOTS('',2,1,((#76465,#76466),(#76467,#76468),
(#76469,#76470)),.UNSPECIFIED.,.F.,.F.,.F.,(3,3),(2,2),(0.,1.),(0.,0.0149999999999997),
 .UNSPECIFIED.);
#56435=B_SPLINE_SURFACE_WITH_KNOTS('',2,1,((#76480,#76481),(#76482,#76483),
(#76484,#76485)),.UNSPECIFIED.,.F.,.F.,.F.,(3,3),(2,2),(0.,1.),(0.,0.0149999999999997),
 .UNSPECIFIED.);
#56436=B_SPLINE_SURFACE_WITH_KNOTS('',2,1,((#76495,#76496),(#76497,#76498),
(#76499,#76500)),.UNSPECIFIED.,.F.,.F.,.F.,(3,3),(2,2),(0.,1.),(0.,0.0149999999999997),
 .UNSPECIFIED.);
#56437=B_SPLINE_SURFACE_WITH_KNOTS('',2,1,((#76510,#76511),(#76512,#76513),
(#76514,#76515)),.UNSPECIFIED.,.F.,.F.,.F.,(3,3),(2,2),(0.,1.),(0.,0.0149999999999997),
 .UNSPECIFIED.);
#56438=B_SPLINE_SURFACE_WITH_KNOTS('',2,1,((#76525,#76526),(#76527,#76528),
(#76529,#76530)),.UNSPECIFIED.,.F.,.F.,.F.,(3,3),(2,2),(0.,1.),(0.,0.0149999999999997),
 .UNSPECIFIED.);
#56439=B_SPLINE_SURFACE_WITH_KNOTS('',2,1,((#76540,#76541),(#76542,#76543),
(#76544,#76545)),.UNSPECIFIED.,.F.,.F.,.F.,(3,3),(2,2),(0.,1.),(0.,0.0149999999999997),
 .UNSPECIFIED.);
#56440=B_SPLINE_SURFACE_WITH_KNOTS('',2,1,((#76555,#76556),(#76557,#76558),
(#76559,#76560)),.UNSPECIFIED.,.F.,.F.,.F.,(3,3),(2,2),(0.,1.),(0.,0.0149999999999997),
 .UNSPECIFIED.);
#56441=B_SPLINE_SURFACE_WITH_KNOTS('',2,1,((#76567,#76568),(#76569,#76570),
(#76571,#76572)),.UNSPECIFIED.,.F.,.F.,.F.,(3,3),(2,2),(0.,1.),(0.,0.0149999999999997),
 .UNSPECIFIED.);
#56442=B_SPLINE_SURFACE_WITH_KNOTS('',2,1,((#76585,#76586),(#76587,#76588),
(#76589,#76590)),.UNSPECIFIED.,.F.,.F.,.F.,(3,3),(2,2),(0.,1.),(0.,0.0149999999999997),
 .UNSPECIFIED.);
#56443=B_SPLINE_SURFACE_WITH_KNOTS('',2,1,((#76600,#76601),(#76602,#76603),
(#76604,#76605)),.UNSPECIFIED.,.F.,.F.,.F.,(3,3),(2,2),(0.,1.),(0.,0.0149999999999997),
 .UNSPECIFIED.);
#56444=B_SPLINE_SURFACE_WITH_KNOTS('',2,1,((#76615,#76616),(#76617,#76618),
(#76619,#76620)),.UNSPECIFIED.,.F.,.F.,.F.,(3,3),(2,2),(0.,1.),(0.,0.0149999999999997),
 .UNSPECIFIED.);
#56445=B_SPLINE_SURFACE_WITH_KNOTS('',2,1,((#76630,#76631),(#76632,#76633),
(#76634,#76635)),.UNSPECIFIED.,.F.,.F.,.F.,(3,3),(2,2),(0.,1.),(0.,0.0149999999999997),
 .UNSPECIFIED.);
#56446=B_SPLINE_SURFACE_WITH_KNOTS('',2,1,((#76645,#76646),(#76647,#76648),
(#76649,#76650)),.UNSPECIFIED.,.F.,.F.,.F.,(3,3),(2,2),(0.,1.),(0.,0.0149999999999997),
 .UNSPECIFIED.);
#56447=B_SPLINE_SURFACE_WITH_KNOTS('',2,1,((#76660,#76661),(#76662,#76663),
(#76664,#76665)),.UNSPECIFIED.,.F.,.F.,.F.,(3,3),(2,2),(0.,1.),(0.,0.0149999999999997),
 .UNSPECIFIED.);
#56448=B_SPLINE_SURFACE_WITH_KNOTS('',2,1,((#76675,#76676),(#76677,#76678),
(#76679,#76680)),.UNSPECIFIED.,.F.,.F.,.F.,(3,3),(2,2),(0.,1.),(0.,0.0149999999999997),
 .UNSPECIFIED.);
#56449=B_SPLINE_SURFACE_WITH_KNOTS('',2,1,((#76690,#76691),(#76692,#76693),
(#76694,#76695)),.UNSPECIFIED.,.F.,.F.,.F.,(3,3),(2,2),(0.,1.),(0.,0.0149999999999997),
 .UNSPECIFIED.);
#56450=B_SPLINE_SURFACE_WITH_KNOTS('',2,1,((#76705,#76706),(#76707,#76708),
(#76709,#76710)),.UNSPECIFIED.,.F.,.F.,.F.,(3,3),(2,2),(0.,1.),(0.,0.0149999999999997),
 .UNSPECIFIED.);
#56451=B_SPLINE_SURFACE_WITH_KNOTS('',2,1,((#76720,#76721),(#76722,#76723),
(#76724,#76725)),.UNSPECIFIED.,.F.,.F.,.F.,(3,3),(2,2),(0.,1.),(0.,0.0149999999999997),
 .UNSPECIFIED.);
#56452=B_SPLINE_SURFACE_WITH_KNOTS('',2,1,((#76735,#76736),(#76737,#76738),
(#76739,#76740)),.UNSPECIFIED.,.F.,.F.,.F.,(3,3),(2,2),(0.,1.),(0.,0.0149999999999997),
 .UNSPECIFIED.);
#56453=B_SPLINE_SURFACE_WITH_KNOTS('',2,1,((#76750,#76751),(#76752,#76753),
(#76754,#76755)),.UNSPECIFIED.,.F.,.F.,.F.,(3,3),(2,2),(0.,1.),(0.,0.0149999999999997),
 .UNSPECIFIED.);
#56454=B_SPLINE_SURFACE_WITH_KNOTS('',2,1,((#76765,#76766),(#76767,#76768),
(#76769,#76770)),.UNSPECIFIED.,.F.,.F.,.F.,(3,3),(2,2),(0.,1.),(0.,0.0149999999999997),
 .UNSPECIFIED.);
#56455=B_SPLINE_SURFACE_WITH_KNOTS('',2,1,((#76780,#76781),(#76782,#76783),
(#76784,#76785)),.UNSPECIFIED.,.F.,.F.,.F.,(3,3),(2,2),(0.,1.),(0.,0.0149999999999997),
 .UNSPECIFIED.);
#56456=B_SPLINE_SURFACE_WITH_KNOTS('',2,1,((#76795,#76796),(#76797,#76798),
(#76799,#76800)),.UNSPECIFIED.,.F.,.F.,.F.,(3,3),(2,2),(0.,1.),(0.,0.0149999999999997),
 .UNSPECIFIED.);
#56457=B_SPLINE_SURFACE_WITH_KNOTS('',2,1,((#76810,#76811),(#76812,#76813),
(#76814,#76815)),.UNSPECIFIED.,.F.,.F.,.F.,(3,3),(2,2),(0.,1.),(0.,0.0149999999999997),
 .UNSPECIFIED.);
#56458=B_SPLINE_SURFACE_WITH_KNOTS('',2,1,((#76825,#76826),(#76827,#76828),
(#76829,#76830)),.UNSPECIFIED.,.F.,.F.,.F.,(3,3),(2,2),(0.,1.),(0.,0.0149999999999997),
 .UNSPECIFIED.);
#56459=B_SPLINE_SURFACE_WITH_KNOTS('',2,1,((#76840,#76841),(#76842,#76843),
(#76844,#76845)),.UNSPECIFIED.,.F.,.F.,.F.,(3,3),(2,2),(0.,1.),(0.,0.0149999999999997),
 .UNSPECIFIED.);
#56460=B_SPLINE_SURFACE_WITH_KNOTS('',2,1,((#76855,#76856),(#76857,#76858),
(#76859,#76860)),.UNSPECIFIED.,.F.,.F.,.F.,(3,3),(2,2),(0.,1.),(0.,0.0149999999999997),
 .UNSPECIFIED.);
#56461=B_SPLINE_SURFACE_WITH_KNOTS('',2,1,((#76876,#76877),(#76878,#76879),
(#76880,#76881)),.UNSPECIFIED.,.F.,.F.,.F.,(3,3),(2,2),(0.,1.),(0.,0.0149999999999997),
 .UNSPECIFIED.);
#56462=B_SPLINE_SURFACE_WITH_KNOTS('',2,1,((#76891,#76892),(#76893,#76894),
(#76895,#76896)),.UNSPECIFIED.,.F.,.F.,.F.,(3,3),(2,2),(0.,1.),(0.,0.0149999999999997),
 .UNSPECIFIED.);
#56463=B_SPLINE_SURFACE_WITH_KNOTS('',2,1,((#76909,#76910),(#76911,#76912),
(#76913,#76914)),.UNSPECIFIED.,.F.,.F.,.F.,(3,3),(2,2),(0.,1.),(0.,0.0149999999999997),
 .UNSPECIFIED.);
#56464=B_SPLINE_SURFACE_WITH_KNOTS('',2,1,((#76924,#76925),(#76926,#76927),
(#76928,#76929)),.UNSPECIFIED.,.F.,.F.,.F.,(3,3),(2,2),(0.,1.),(0.,0.0149999999999997),
 .UNSPECIFIED.);
#56465=B_SPLINE_SURFACE_WITH_KNOTS('',2,1,((#76939,#76940),(#76941,#76942),
(#76943,#76944)),.UNSPECIFIED.,.F.,.F.,.F.,(3,3),(2,2),(0.,1.),(0.,0.0149999999999997),
 .UNSPECIFIED.);
#56466=B_SPLINE_SURFACE_WITH_KNOTS('',2,1,((#76954,#76955),(#76956,#76957),
(#76958,#76959)),.UNSPECIFIED.,.F.,.F.,.F.,(3,3),(2,2),(0.,1.),(0.,0.0149999999999997),
 .UNSPECIFIED.);
#56467=B_SPLINE_SURFACE_WITH_KNOTS('',2,1,((#76969,#76970),(#76971,#76972),
(#76973,#76974)),.UNSPECIFIED.,.F.,.F.,.F.,(3,3),(2,2),(0.,1.),(0.,0.0149999999999997),
 .UNSPECIFIED.);
#56468=B_SPLINE_SURFACE_WITH_KNOTS('',2,1,((#76984,#76985),(#76986,#76987),
(#76988,#76989)),.UNSPECIFIED.,.F.,.F.,.F.,(3,3),(2,2),(0.,1.),(0.,0.0149999999999997),
 .UNSPECIFIED.);
#56469=B_SPLINE_SURFACE_WITH_KNOTS('',2,1,((#76999,#77000),(#77001,#77002),
(#77003,#77004)),.UNSPECIFIED.,.F.,.F.,.F.,(3,3),(2,2),(0.,1.),(0.,0.0149999999999997),
 .UNSPECIFIED.);
#56470=B_SPLINE_SURFACE_WITH_KNOTS('',2,1,((#77011,#77012),(#77013,#77014),
(#77015,#77016)),.UNSPECIFIED.,.F.,.F.,.F.,(3,3),(2,2),(0.,1.),(0.,0.0149999999999997),
 .UNSPECIFIED.);
#56471=B_SPLINE_SURFACE_WITH_KNOTS('',2,1,((#77029,#77030),(#77031,#77032),
(#77033,#77034)),.UNSPECIFIED.,.F.,.F.,.F.,(3,3),(2,2),(0.,1.),(0.,0.0149999999999997),
 .UNSPECIFIED.);
#56472=B_SPLINE_SURFACE_WITH_KNOTS('',2,1,((#77044,#77045),(#77046,#77047),
(#77048,#77049)),.UNSPECIFIED.,.F.,.F.,.F.,(3,3),(2,2),(0.,1.),(0.,0.0149999999999997),
 .UNSPECIFIED.);
#56473=B_SPLINE_SURFACE_WITH_KNOTS('',2,1,((#77059,#77060),(#77061,#77062),
(#77063,#77064)),.UNSPECIFIED.,.F.,.F.,.F.,(3,3),(2,2),(0.,1.),(0.,0.0149999999999997),
 .UNSPECIFIED.);
#56474=B_SPLINE_SURFACE_WITH_KNOTS('',2,1,((#77074,#77075),(#77076,#77077),
(#77078,#77079)),.UNSPECIFIED.,.F.,.F.,.F.,(3,3),(2,2),(0.,1.),(0.,0.0149999999999997),
 .UNSPECIFIED.);
#56475=B_SPLINE_SURFACE_WITH_KNOTS('',2,1,((#77089,#77090),(#77091,#77092),
(#77093,#77094)),.UNSPECIFIED.,.F.,.F.,.F.,(3,3),(2,2),(0.,1.),(0.,0.0149999999999997),
 .UNSPECIFIED.);
#56476=B_SPLINE_SURFACE_WITH_KNOTS('',2,1,((#77104,#77105),(#77106,#77107),
(#77108,#77109)),.UNSPECIFIED.,.F.,.F.,.F.,(3,3),(2,2),(0.,1.),(0.,0.0149999999999997),
 .UNSPECIFIED.);
#56477=B_SPLINE_SURFACE_WITH_KNOTS('',2,1,((#77119,#77120),(#77121,#77122),
(#77123,#77124)),.UNSPECIFIED.,.F.,.F.,.F.,(3,3),(2,2),(0.,1.),(0.,0.0149999999999997),
 .UNSPECIFIED.);
#56478=B_SPLINE_SURFACE_WITH_KNOTS('',2,1,((#77134,#77135),(#77136,#77137),
(#77138,#77139)),.UNSPECIFIED.,.F.,.F.,.F.,(3,3),(2,2),(0.,1.),(0.,0.0149999999999997),
 .UNSPECIFIED.);
#56479=B_SPLINE_SURFACE_WITH_KNOTS('',2,1,((#77149,#77150),(#77151,#77152),
(#77153,#77154)),.UNSPECIFIED.,.F.,.F.,.F.,(3,3),(2,2),(0.,1.),(0.,0.0149999999999997),
 .UNSPECIFIED.);
#56480=B_SPLINE_SURFACE_WITH_KNOTS('',2,1,((#77164,#77165),(#77166,#77167),
(#77168,#77169)),.UNSPECIFIED.,.F.,.F.,.F.,(3,3),(2,2),(0.,1.),(0.,0.0149999999999997),
 .UNSPECIFIED.);
#56481=B_SPLINE_SURFACE_WITH_KNOTS('',2,1,((#77179,#77180),(#77181,#77182),
(#77183,#77184)),.UNSPECIFIED.,.F.,.F.,.F.,(3,3),(2,2),(0.,1.),(0.,0.0149999999999997),
 .UNSPECIFIED.);
#56482=B_SPLINE_SURFACE_WITH_KNOTS('',2,1,((#77192,#77193),(#77194,#77195),
(#77196,#77197)),.UNSPECIFIED.,.F.,.F.,.F.,(3,3),(2,2),(0.,1.),(0.,0.0149999999999997),
 .UNSPECIFIED.);
#56483=B_SPLINE_SURFACE_WITH_KNOTS('',2,1,((#77210,#77211),(#77212,#77213),
(#77214,#77215)),.UNSPECIFIED.,.F.,.F.,.F.,(3,3),(2,2),(0.,1.),(0.,0.0149999999999997),
 .UNSPECIFIED.);
#56484=B_SPLINE_SURFACE_WITH_KNOTS('',2,1,((#77225,#77226),(#77227,#77228),
(#77229,#77230)),.UNSPECIFIED.,.F.,.F.,.F.,(3,3),(2,2),(0.,1.),(0.,0.0149999999999997),
 .UNSPECIFIED.);
#56485=B_SPLINE_SURFACE_WITH_KNOTS('',2,1,((#77240,#77241),(#77242,#77243),
(#77244,#77245)),.UNSPECIFIED.,.F.,.F.,.F.,(3,3),(2,2),(0.,1.),(0.,0.0149999999999997),
 .UNSPECIFIED.);
#56486=B_SPLINE_SURFACE_WITH_KNOTS('',2,1,((#77255,#77256),(#77257,#77258),
(#77259,#77260)),.UNSPECIFIED.,.F.,.F.,.F.,(3,3),(2,2),(0.,1.),(0.,0.0149999999999997),
 .UNSPECIFIED.);
#56487=B_SPLINE_SURFACE_WITH_KNOTS('',2,1,((#77270,#77271),(#77272,#77273),
(#77274,#77275)),.UNSPECIFIED.,.F.,.F.,.F.,(3,3),(2,2),(0.,1.),(0.,0.0149999999999997),
 .UNSPECIFIED.);
#56488=B_SPLINE_SURFACE_WITH_KNOTS('',2,1,((#77285,#77286),(#77287,#77288),
(#77289,#77290)),.UNSPECIFIED.,.F.,.F.,.F.,(3,3),(2,2),(0.,1.),(0.,0.0149999999999997),
 .UNSPECIFIED.);
#56489=B_SPLINE_SURFACE_WITH_KNOTS('',2,1,((#77300,#77301),(#77302,#77303),
(#77304,#77305)),.UNSPECIFIED.,.F.,.F.,.F.,(3,3),(2,2),(0.,1.),(0.,0.0149999999999997),
 .UNSPECIFIED.);
#56490=B_SPLINE_SURFACE_WITH_KNOTS('',2,1,((#77312,#77313),(#77314,#77315),
(#77316,#77317)),.UNSPECIFIED.,.F.,.F.,.F.,(3,3),(2,2),(0.,1.),(0.,0.0149999999999997),
 .UNSPECIFIED.);
#56491=B_SPLINE_SURFACE_WITH_KNOTS('',2,1,((#77330,#77331),(#77332,#77333),
(#77334,#77335)),.UNSPECIFIED.,.F.,.F.,.F.,(3,3),(2,2),(0.,1.),(0.,0.0149999999999997),
 .UNSPECIFIED.);
#56492=B_SPLINE_SURFACE_WITH_KNOTS('',2,1,((#77345,#77346),(#77347,#77348),
(#77349,#77350)),.UNSPECIFIED.,.F.,.F.,.F.,(3,3),(2,2),(0.,1.),(0.,0.0149999999999997),
 .UNSPECIFIED.);
#56493=B_SPLINE_SURFACE_WITH_KNOTS('',2,1,((#77360,#77361),(#77362,#77363),
(#77364,#77365)),.UNSPECIFIED.,.F.,.F.,.F.,(3,3),(2,2),(0.,1.),(0.,0.0149999999999997),
 .UNSPECIFIED.);
#56494=B_SPLINE_SURFACE_WITH_KNOTS('',2,1,((#77375,#77376),(#77377,#77378),
(#77379,#77380)),.UNSPECIFIED.,.F.,.F.,.F.,(3,3),(2,2),(0.,1.),(0.,0.0149999999999997),
 .UNSPECIFIED.);
#56495=B_SPLINE_SURFACE_WITH_KNOTS('',2,1,((#77390,#77391),(#77392,#77393),
(#77394,#77395)),.UNSPECIFIED.,.F.,.F.,.F.,(3,3),(2,2),(0.,1.),(0.,0.0149999999999997),
 .UNSPECIFIED.);
#56496=B_SPLINE_SURFACE_WITH_KNOTS('',2,1,((#77405,#77406),(#77407,#77408),
(#77409,#77410)),.UNSPECIFIED.,.F.,.F.,.F.,(3,3),(2,2),(0.,1.),(0.,0.0149999999999997),
 .UNSPECIFIED.);
#56497=B_SPLINE_SURFACE_WITH_KNOTS('',2,1,((#77420,#77421),(#77422,#77423),
(#77424,#77425)),.UNSPECIFIED.,.F.,.F.,.F.,(3,3),(2,2),(0.,1.),(0.,0.0149999999999997),
 .UNSPECIFIED.);
#56498=B_SPLINE_SURFACE_WITH_KNOTS('',2,1,((#77435,#77436),(#77437,#77438),
(#77439,#77440)),.UNSPECIFIED.,.F.,.F.,.F.,(3,3),(2,2),(0.,1.),(0.,0.0149999999999997),
 .UNSPECIFIED.);
#56499=B_SPLINE_SURFACE_WITH_KNOTS('',2,1,((#77447,#77448),(#77449,#77450),
(#77451,#77452)),.UNSPECIFIED.,.F.,.F.,.F.,(3,3),(2,2),(0.,1.),(0.,0.0149999999999997),
 .UNSPECIFIED.);
#56500=B_SPLINE_SURFACE_WITH_KNOTS('',2,1,((#77465,#77466),(#77467,#77468),
(#77469,#77470)),.UNSPECIFIED.,.F.,.F.,.F.,(3,3),(2,2),(0.,1.),(0.,0.0149999999999997),
 .UNSPECIFIED.);
#56501=B_SPLINE_SURFACE_WITH_KNOTS('',2,1,((#77480,#77481),(#77482,#77483),
(#77484,#77485)),.UNSPECIFIED.,.F.,.F.,.F.,(3,3),(2,2),(0.,1.),(0.,0.0149999999999997),
 .UNSPECIFIED.);
#56502=B_SPLINE_SURFACE_WITH_KNOTS('',2,1,((#77495,#77496),(#77497,#77498),
(#77499,#77500)),.UNSPECIFIED.,.F.,.F.,.F.,(3,3),(2,2),(0.,1.),(0.,0.0149999999999997),
 .UNSPECIFIED.);
#56503=B_SPLINE_SURFACE_WITH_KNOTS('',2,1,((#77510,#77511),(#77512,#77513),
(#77514,#77515)),.UNSPECIFIED.,.F.,.F.,.F.,(3,3),(2,2),(0.,1.),(0.,0.0149999999999997),
 .UNSPECIFIED.);
#56504=B_SPLINE_SURFACE_WITH_KNOTS('',2,1,((#77525,#77526),(#77527,#77528),
(#77529,#77530)),.UNSPECIFIED.,.F.,.F.,.F.,(3,3),(2,2),(0.,1.),(0.,0.0149999999999997),
 .UNSPECIFIED.);
#56505=B_SPLINE_SURFACE_WITH_KNOTS('',2,1,((#77540,#77541),(#77542,#77543),
(#77544,#77545)),.UNSPECIFIED.,.F.,.F.,.F.,(3,3),(2,2),(0.,1.),(0.,0.0149999999999997),
 .UNSPECIFIED.);
#56506=B_SPLINE_SURFACE_WITH_KNOTS('',2,1,((#77555,#77556),(#77557,#77558),
(#77559,#77560)),.UNSPECIFIED.,.F.,.F.,.F.,(3,3),(2,2),(0.,1.),(0.,0.0149999999999997),
 .UNSPECIFIED.);
#56507=B_SPLINE_SURFACE_WITH_KNOTS('',2,1,((#77570,#77571),(#77572,#77573),
(#77574,#77575)),.UNSPECIFIED.,.F.,.F.,.F.,(3,3),(2,2),(0.,1.),(0.,0.0149999999999997),
 .UNSPECIFIED.);
#56508=B_SPLINE_SURFACE_WITH_KNOTS('',2,1,((#77585,#77586),(#77587,#77588),
(#77589,#77590)),.UNSPECIFIED.,.F.,.F.,.F.,(3,3),(2,2),(0.,1.),(0.,0.0149999999999997),
 .UNSPECIFIED.);
#56509=B_SPLINE_SURFACE_WITH_KNOTS('',2,1,((#77600,#77601),(#77602,#77603),
(#77604,#77605)),.UNSPECIFIED.,.F.,.F.,.F.,(3,3),(2,2),(0.,1.),(0.,0.0149999999999997),
 .UNSPECIFIED.);
#56510=B_SPLINE_SURFACE_WITH_KNOTS('',2,1,((#77615,#77616),(#77617,#77618),
(#77619,#77620)),.UNSPECIFIED.,.F.,.F.,.F.,(3,3),(2,2),(0.,1.),(0.,0.0149999999999997),
 .UNSPECIFIED.);
#56511=B_SPLINE_SURFACE_WITH_KNOTS('',2,1,((#77630,#77631),(#77632,#77633),
(#77634,#77635)),.UNSPECIFIED.,.F.,.F.,.F.,(3,3),(2,2),(0.,1.),(0.,0.0149999999999997),
 .UNSPECIFIED.);
#56512=B_SPLINE_SURFACE_WITH_KNOTS('',2,1,((#77645,#77646),(#77647,#77648),
(#77649,#77650)),.UNSPECIFIED.,.F.,.F.,.F.,(3,3),(2,2),(0.,1.),(0.,0.0149999999999997),
 .UNSPECIFIED.);
#56513=B_SPLINE_SURFACE_WITH_KNOTS('',2,1,((#77660,#77661),(#77662,#77663),
(#77664,#77665)),.UNSPECIFIED.,.F.,.F.,.F.,(3,3),(2,2),(0.,1.),(0.,0.0149999999999997),
 .UNSPECIFIED.);
#56514=B_SPLINE_SURFACE_WITH_KNOTS('',2,1,((#77675,#77676),(#77677,#77678),
(#77679,#77680)),.UNSPECIFIED.,.F.,.F.,.F.,(3,3),(2,2),(0.,1.),(0.,0.0149999999999997),
 .UNSPECIFIED.);
#56515=B_SPLINE_SURFACE_WITH_KNOTS('',2,1,((#77691,#77692),(#77693,#77694),
(#77695,#77696)),.UNSPECIFIED.,.F.,.F.,.F.,(3,3),(2,2),(0.,1.),(0.,0.0149999999999997),
 .UNSPECIFIED.);
#56516=B_SPLINE_SURFACE_WITH_KNOTS('',2,1,((#77709,#77710),(#77711,#77712),
(#77713,#77714)),.UNSPECIFIED.,.F.,.F.,.F.,(3,3),(2,2),(0.,1.),(0.,0.0149999999999997),
 .UNSPECIFIED.);
#56517=B_SPLINE_SURFACE_WITH_KNOTS('',2,1,((#77724,#77725),(#77726,#77727),
(#77728,#77729)),.UNSPECIFIED.,.F.,.F.,.F.,(3,3),(2,2),(0.,1.),(0.,0.0149999999999997),
 .UNSPECIFIED.);
#56518=B_SPLINE_SURFACE_WITH_KNOTS('',2,1,((#77739,#77740),(#77741,#77742),
(#77743,#77744)),.UNSPECIFIED.,.F.,.F.,.F.,(3,3),(2,2),(0.,1.),(0.,0.0149999999999997),
 .UNSPECIFIED.);
#56519=B_SPLINE_SURFACE_WITH_KNOTS('',2,1,((#77754,#77755),(#77756,#77757),
(#77758,#77759)),.UNSPECIFIED.,.F.,.F.,.F.,(3,3),(2,2),(0.,1.),(0.,0.0149999999999997),
 .UNSPECIFIED.);
#56520=B_SPLINE_SURFACE_WITH_KNOTS('',2,1,((#77769,#77770),(#77771,#77772),
(#77773,#77774)),.UNSPECIFIED.,.F.,.F.,.F.,(3,3),(2,2),(0.,1.),(0.,0.0149999999999997),
 .UNSPECIFIED.);
#56521=B_SPLINE_SURFACE_WITH_KNOTS('',2,1,((#77784,#77785),(#77786,#77787),
(#77788,#77789)),.UNSPECIFIED.,.F.,.F.,.F.,(3,3),(2,2),(0.,1.),(0.,0.0149999999999997),
 .UNSPECIFIED.);
#56522=B_SPLINE_SURFACE_WITH_KNOTS('',2,1,((#77799,#77800),(#77801,#77802),
(#77803,#77804)),.UNSPECIFIED.,.F.,.F.,.F.,(3,3),(2,2),(0.,1.),(0.,0.0149999999999997),
 .UNSPECIFIED.);
#56523=B_SPLINE_SURFACE_WITH_KNOTS('',2,1,((#77811,#77812),(#77813,#77814),
(#77815,#77816)),.UNSPECIFIED.,.F.,.F.,.F.,(3,3),(2,2),(0.,1.),(0.,0.0149999999999997),
 .UNSPECIFIED.);
#56524=B_SPLINE_SURFACE_WITH_KNOTS('',2,1,((#77829,#77830),(#77831,#77832),
(#77833,#77834)),.UNSPECIFIED.,.F.,.F.,.F.,(3,3),(2,2),(0.,1.),(0.,0.0149999999999997),
 .UNSPECIFIED.);
#56525=B_SPLINE_SURFACE_WITH_KNOTS('',2,1,((#77844,#77845),(#77846,#77847),
(#77848,#77849)),.UNSPECIFIED.,.F.,.F.,.F.,(3,3),(2,2),(0.,1.),(0.,0.0149999999999997),
 .UNSPECIFIED.);
#56526=B_SPLINE_SURFACE_WITH_KNOTS('',2,1,((#77859,#77860),(#77861,#77862),
(#77863,#77864)),.UNSPECIFIED.,.F.,.F.,.F.,(3,3),(2,2),(0.,1.),(0.,0.0149999999999997),
 .UNSPECIFIED.);
#56527=B_SPLINE_SURFACE_WITH_KNOTS('',2,1,((#77874,#77875),(#77876,#77877),
(#77878,#77879)),.UNSPECIFIED.,.F.,.F.,.F.,(3,3),(2,2),(0.,1.),(0.,0.0149999999999997),
 .UNSPECIFIED.);
#56528=B_SPLINE_SURFACE_WITH_KNOTS('',2,1,((#77889,#77890),(#77891,#77892),
(#77893,#77894)),.UNSPECIFIED.,.F.,.F.,.F.,(3,3),(2,2),(0.,1.),(0.,0.0149999999999997),
 .UNSPECIFIED.);
#56529=B_SPLINE_SURFACE_WITH_KNOTS('',2,1,((#77904,#77905),(#77906,#77907),
(#77908,#77909)),.UNSPECIFIED.,.F.,.F.,.F.,(3,3),(2,2),(0.,1.),(0.,0.0149999999999997),
 .UNSPECIFIED.);
#56530=B_SPLINE_SURFACE_WITH_KNOTS('',2,1,((#77919,#77920),(#77921,#77922),
(#77923,#77924)),.UNSPECIFIED.,.F.,.F.,.F.,(3,3),(2,2),(0.,1.),(0.,0.0149999999999997),
 .UNSPECIFIED.);
#56531=B_SPLINE_SURFACE_WITH_KNOTS('',2,1,((#77934,#77935),(#77936,#77937),
(#77938,#77939)),.UNSPECIFIED.,.F.,.F.,.F.,(3,3),(2,2),(0.,1.),(0.,0.0149999999999997),
 .UNSPECIFIED.);
#56532=B_SPLINE_SURFACE_WITH_KNOTS('',2,1,((#77949,#77950),(#77951,#77952),
(#77953,#77954)),.UNSPECIFIED.,.F.,.F.,.F.,(3,3),(2,2),(0.,1.),(0.,0.0149999999999997),
 .UNSPECIFIED.);
#56533=B_SPLINE_SURFACE_WITH_KNOTS('',2,1,((#77964,#77965),(#77966,#77967),
(#77968,#77969)),.UNSPECIFIED.,.F.,.F.,.F.,(3,3),(2,2),(0.,1.),(0.,0.0149999999999997),
 .UNSPECIFIED.);
#56534=B_SPLINE_SURFACE_WITH_KNOTS('',2,1,((#77979,#77980),(#77981,#77982),
(#77983,#77984)),.UNSPECIFIED.,.F.,.F.,.F.,(3,3),(2,2),(0.,1.),(0.,0.0149999999999997),
 .UNSPECIFIED.);
#56535=B_SPLINE_SURFACE_WITH_KNOTS('',2,1,((#77992,#77993),(#77994,#77995),
(#77996,#77997)),.UNSPECIFIED.,.F.,.F.,.F.,(3,3),(2,2),(0.,1.),(0.,0.0149999999999997),
 .UNSPECIFIED.);
#56536=B_SPLINE_SURFACE_WITH_KNOTS('',2,1,((#78010,#78011),(#78012,#78013),
(#78014,#78015)),.UNSPECIFIED.,.F.,.F.,.F.,(3,3),(2,2),(0.,1.),(0.,0.0149999999999997),
 .UNSPECIFIED.);
#56537=B_SPLINE_SURFACE_WITH_KNOTS('',2,1,((#78025,#78026),(#78027,#78028),
(#78029,#78030)),.UNSPECIFIED.,.F.,.F.,.F.,(3,3),(2,2),(0.,1.),(0.,0.0149999999999997),
 .UNSPECIFIED.);
#56538=B_SPLINE_SURFACE_WITH_KNOTS('',2,1,((#78046,#78047),(#78048,#78049),
(#78050,#78051)),.UNSPECIFIED.,.F.,.F.,.F.,(3,3),(2,2),(0.,1.),(0.,0.0149999999999997),
 .UNSPECIFIED.);
#56539=B_SPLINE_SURFACE_WITH_KNOTS('',2,1,((#78061,#78062),(#78063,#78064),
(#78065,#78066)),.UNSPECIFIED.,.F.,.F.,.F.,(3,3),(2,2),(0.,1.),(0.,0.0149999999999997),
 .UNSPECIFIED.);
#56540=B_SPLINE_SURFACE_WITH_KNOTS('',2,1,((#78076,#78077),(#78078,#78079),
(#78080,#78081)),.UNSPECIFIED.,.F.,.F.,.F.,(3,3),(2,2),(0.,1.),(0.,0.0149999999999997),
 .UNSPECIFIED.);
#56541=B_SPLINE_SURFACE_WITH_KNOTS('',2,1,((#78114,#78115),(#78116,#78117),
(#78118,#78119)),.UNSPECIFIED.,.F.,.F.,.F.,(3,3),(2,2),(0.,1.),(0.,0.0149999999999997),
 .UNSPECIFIED.);
#56542=B_SPLINE_SURFACE_WITH_KNOTS('',2,1,((#78132,#78133),(#78134,#78135),
(#78136,#78137)),.UNSPECIFIED.,.F.,.F.,.F.,(3,3),(2,2),(0.,1.),(0.,0.0149999999999997),
 .UNSPECIFIED.);
#56543=B_SPLINE_SURFACE_WITH_KNOTS('',2,1,((#78147,#78148),(#78149,#78150),
(#78151,#78152)),.UNSPECIFIED.,.F.,.F.,.F.,(3,3),(2,2),(0.,1.),(0.,0.0149999999999997),
 .UNSPECIFIED.);
#56544=B_SPLINE_SURFACE_WITH_KNOTS('',2,1,((#78162,#78163),(#78164,#78165),
(#78166,#78167)),.UNSPECIFIED.,.F.,.F.,.F.,(3,3),(2,2),(0.,1.),(0.,0.0149999999999997),
 .UNSPECIFIED.);
#56545=B_SPLINE_SURFACE_WITH_KNOTS('',2,1,((#78177,#78178),(#78179,#78180),
(#78181,#78182)),.UNSPECIFIED.,.F.,.F.,.F.,(3,3),(2,2),(0.,1.),(0.,0.0149999999999997),
 .UNSPECIFIED.);
#56546=B_SPLINE_SURFACE_WITH_KNOTS('',2,1,((#78192,#78193),(#78194,#78195),
(#78196,#78197)),.UNSPECIFIED.,.F.,.F.,.F.,(3,3),(2,2),(0.,1.),(0.,0.0149999999999997),
 .UNSPECIFIED.);
#56547=B_SPLINE_SURFACE_WITH_KNOTS('',2,1,((#78207,#78208),(#78209,#78210),
(#78211,#78212)),.UNSPECIFIED.,.F.,.F.,.F.,(3,3),(2,2),(0.,1.),(0.,0.0149999999999997),
 .UNSPECIFIED.);
#56548=B_SPLINE_SURFACE_WITH_KNOTS('',2,1,((#78222,#78223),(#78224,#78225),
(#78226,#78227)),.UNSPECIFIED.,.F.,.F.,.F.,(3,3),(2,2),(0.,1.),(0.,0.0149999999999997),
 .UNSPECIFIED.);
#56549=B_SPLINE_SURFACE_WITH_KNOTS('',2,1,((#78234,#78235),(#78236,#78237),
(#78238,#78239)),.UNSPECIFIED.,.F.,.F.,.F.,(3,3),(2,2),(0.,1.),(0.,0.0149999999999997),
 .UNSPECIFIED.);
#56550=B_SPLINE_SURFACE_WITH_KNOTS('',2,1,((#78252,#78253),(#78254,#78255),
(#78256,#78257)),.UNSPECIFIED.,.F.,.F.,.F.,(3,3),(2,2),(0.,1.),(0.,0.0149999999999997),
 .UNSPECIFIED.);
#56551=B_SPLINE_SURFACE_WITH_KNOTS('',2,1,((#78267,#78268),(#78269,#78270),
(#78271,#78272)),.UNSPECIFIED.,.F.,.F.,.F.,(3,3),(2,2),(0.,1.),(0.,0.0149999999999997),
 .UNSPECIFIED.);
#56552=B_SPLINE_SURFACE_WITH_KNOTS('',2,1,((#78282,#78283),(#78284,#78285),
(#78286,#78287)),.UNSPECIFIED.,.F.,.F.,.F.,(3,3),(2,2),(0.,1.),(0.,0.0149999999999997),
 .UNSPECIFIED.);
#56553=B_SPLINE_SURFACE_WITH_KNOTS('',2,1,((#78297,#78298),(#78299,#78300),
(#78301,#78302)),.UNSPECIFIED.,.F.,.F.,.F.,(3,3),(2,2),(0.,1.),(0.,0.0149999999999997),
 .UNSPECIFIED.);
#56554=B_SPLINE_SURFACE_WITH_KNOTS('',2,1,((#78312,#78313),(#78314,#78315),
(#78316,#78317)),.UNSPECIFIED.,.F.,.F.,.F.,(3,3),(2,2),(0.,1.),(0.,0.0149999999999997),
 .UNSPECIFIED.);
#56555=B_SPLINE_SURFACE_WITH_KNOTS('',2,1,((#78327,#78328),(#78329,#78330),
(#78331,#78332)),.UNSPECIFIED.,.F.,.F.,.F.,(3,3),(2,2),(0.,1.),(0.,0.0149999999999997),
 .UNSPECIFIED.);
#56556=B_SPLINE_SURFACE_WITH_KNOTS('',2,1,((#78342,#78343),(#78344,#78345),
(#78346,#78347)),.UNSPECIFIED.,.F.,.F.,.F.,(3,3),(2,2),(0.,1.),(0.,0.0149999999999997),
 .UNSPECIFIED.);
#56557=B_SPLINE_SURFACE_WITH_KNOTS('',2,1,((#78357,#78358),(#78359,#78360),
(#78361,#78362)),.UNSPECIFIED.,.F.,.F.,.F.,(3,3),(2,2),(0.,1.),(0.,0.0149999999999997),
 .UNSPECIFIED.);
#56558=B_SPLINE_SURFACE_WITH_KNOTS('',2,1,((#78372,#78373),(#78374,#78375),
(#78376,#78377)),.UNSPECIFIED.,.F.,.F.,.F.,(3,3),(2,2),(0.,1.),(0.,0.0149999999999997),
 .UNSPECIFIED.);
#56559=B_SPLINE_SURFACE_WITH_KNOTS('',2,1,((#78387,#78388),(#78389,#78390),
(#78391,#78392)),.UNSPECIFIED.,.F.,.F.,.F.,(3,3),(2,2),(0.,1.),(0.,0.0149999999999997),
 .UNSPECIFIED.);
#56560=B_SPLINE_SURFACE_WITH_KNOTS('',2,1,((#78402,#78403),(#78404,#78405),
(#78406,#78407)),.UNSPECIFIED.,.F.,.F.,.F.,(3,3),(2,2),(0.,1.),(0.,0.0149999999999997),
 .UNSPECIFIED.);
#56561=B_SPLINE_SURFACE_WITH_KNOTS('',2,1,((#78415,#78416),(#78417,#78418),
(#78419,#78420)),.UNSPECIFIED.,.F.,.F.,.F.,(3,3),(2,2),(0.,1.),(0.,0.0149999999999997),
 .UNSPECIFIED.);
#56562=B_SPLINE_SURFACE_WITH_KNOTS('',2,1,((#78433,#78434),(#78435,#78436),
(#78437,#78438)),.UNSPECIFIED.,.F.,.F.,.F.,(3,3),(2,2),(0.,1.),(0.,0.0149999999999997),
 .UNSPECIFIED.);
#56563=B_SPLINE_SURFACE_WITH_KNOTS('',2,1,((#78448,#78449),(#78450,#78451),
(#78452,#78453)),.UNSPECIFIED.,.F.,.F.,.F.,(3,3),(2,2),(0.,1.),(0.,0.0149999999999997),
 .UNSPECIFIED.);
#56564=B_SPLINE_SURFACE_WITH_KNOTS('',2,1,((#78463,#78464),(#78465,#78466),
(#78467,#78468)),.UNSPECIFIED.,.F.,.F.,.F.,(3,3),(2,2),(0.,1.),(0.,0.0149999999999997),
 .UNSPECIFIED.);
#56565=B_SPLINE_SURFACE_WITH_KNOTS('',2,1,((#78478,#78479),(#78480,#78481),
(#78482,#78483)),.UNSPECIFIED.,.F.,.F.,.F.,(3,3),(2,2),(0.,1.),(0.,0.0149999999999997),
 .UNSPECIFIED.);
#56566=B_SPLINE_SURFACE_WITH_KNOTS('',2,1,((#78493,#78494),(#78495,#78496),
(#78497,#78498)),.UNSPECIFIED.,.F.,.F.,.F.,(3,3),(2,2),(0.,1.),(0.,0.0149999999999997),
 .UNSPECIFIED.);
#56567=B_SPLINE_SURFACE_WITH_KNOTS('',2,1,((#78508,#78509),(#78510,#78511),
(#78512,#78513)),.UNSPECIFIED.,.F.,.F.,.F.,(3,3),(2,2),(0.,1.),(0.,0.0149999999999997),
 .UNSPECIFIED.);
#56568=B_SPLINE_SURFACE_WITH_KNOTS('',2,1,((#78523,#78524),(#78525,#78526),
(#78527,#78528)),.UNSPECIFIED.,.F.,.F.,.F.,(3,3),(2,2),(0.,1.),(0.,0.0149999999999997),
 .UNSPECIFIED.);
#56569=B_SPLINE_SURFACE_WITH_KNOTS('',2,1,((#78538,#78539),(#78540,#78541),
(#78542,#78543)),.UNSPECIFIED.,.F.,.F.,.F.,(3,3),(2,2),(0.,1.),(0.,0.0149999999999997),
 .UNSPECIFIED.);
#56570=B_SPLINE_SURFACE_WITH_KNOTS('',2,1,((#78550,#78551),(#78552,#78553),
(#78554,#78555)),.UNSPECIFIED.,.F.,.F.,.F.,(3,3),(2,2),(0.,1.),(0.,0.0149999999999997),
 .UNSPECIFIED.);
#56571=B_SPLINE_SURFACE_WITH_KNOTS('',2,1,((#78568,#78569),(#78570,#78571),
(#78572,#78573)),.UNSPECIFIED.,.F.,.F.,.F.,(3,3),(2,2),(0.,1.),(0.,0.0149999999999997),
 .UNSPECIFIED.);
#56572=B_SPLINE_SURFACE_WITH_KNOTS('',2,1,((#78583,#78584),(#78585,#78586),
(#78587,#78588)),.UNSPECIFIED.,.F.,.F.,.F.,(3,3),(2,2),(0.,1.),(0.,0.0149999999999997),
 .UNSPECIFIED.);
#56573=B_SPLINE_SURFACE_WITH_KNOTS('',2,1,((#78598,#78599),(#78600,#78601),
(#78602,#78603)),.UNSPECIFIED.,.F.,.F.,.F.,(3,3),(2,2),(0.,1.),(0.,0.0149999999999997),
 .UNSPECIFIED.);
#56574=B_SPLINE_SURFACE_WITH_KNOTS('',2,1,((#78613,#78614),(#78615,#78616),
(#78617,#78618)),.UNSPECIFIED.,.F.,.F.,.F.,(3,3),(2,2),(0.,1.),(0.,0.0149999999999997),
 .UNSPECIFIED.);
#56575=B_SPLINE_SURFACE_WITH_KNOTS('',2,1,((#78628,#78629),(#78630,#78631),
(#78632,#78633)),.UNSPECIFIED.,.F.,.F.,.F.,(3,3),(2,2),(0.,1.),(0.,0.0149999999999997),
 .UNSPECIFIED.);
#56576=B_SPLINE_SURFACE_WITH_KNOTS('',2,1,((#78643,#78644),(#78645,#78646),
(#78647,#78648)),.UNSPECIFIED.,.F.,.F.,.F.,(3,3),(2,2),(0.,1.),(0.,0.0149999999999997),
 .UNSPECIFIED.);
#56577=B_SPLINE_SURFACE_WITH_KNOTS('',2,1,((#78658,#78659),(#78660,#78661),
(#78662,#78663)),.UNSPECIFIED.,.F.,.F.,.F.,(3,3),(2,2),(0.,1.),(0.,0.0149999999999997),
 .UNSPECIFIED.);
#56578=B_SPLINE_SURFACE_WITH_KNOTS('',2,1,((#78673,#78674),(#78675,#78676),
(#78677,#78678)),.UNSPECIFIED.,.F.,.F.,.F.,(3,3),(2,2),(0.,1.),(0.,0.0149999999999997),
 .UNSPECIFIED.);
#56579=B_SPLINE_SURFACE_WITH_KNOTS('',2,1,((#78688,#78689),(#78690,#78691),
(#78692,#78693)),.UNSPECIFIED.,.F.,.F.,.F.,(3,3),(2,2),(0.,1.),(0.,0.0149999999999997),
 .UNSPECIFIED.);
#56580=B_SPLINE_SURFACE_WITH_KNOTS('',2,1,((#78703,#78704),(#78705,#78706),
(#78707,#78708)),.UNSPECIFIED.,.F.,.F.,.F.,(3,3),(2,2),(0.,1.),(0.,0.0149999999999997),
 .UNSPECIFIED.);
#56581=B_SPLINE_SURFACE_WITH_KNOTS('',2,1,((#78718,#78719),(#78720,#78721),
(#78722,#78723)),.UNSPECIFIED.,.F.,.F.,.F.,(3,3),(2,2),(0.,1.),(0.,0.0149999999999997),
 .UNSPECIFIED.);
#56582=B_SPLINE_SURFACE_WITH_KNOTS('',2,1,((#78733,#78734),(#78735,#78736),
(#78737,#78738)),.UNSPECIFIED.,.F.,.F.,.F.,(3,3),(2,2),(0.,1.),(0.,0.0149999999999997),
 .UNSPECIFIED.);
#56583=B_SPLINE_SURFACE_WITH_KNOTS('',2,1,((#78748,#78749),(#78750,#78751),
(#78752,#78753)),.UNSPECIFIED.,.F.,.F.,.F.,(3,3),(2,2),(0.,1.),(0.,0.0149999999999997),
 .UNSPECIFIED.);
#56584=B_SPLINE_SURFACE_WITH_KNOTS('',2,1,((#78763,#78764),(#78765,#78766),
(#78767,#78768)),.UNSPECIFIED.,.F.,.F.,.F.,(3,3),(2,2),(0.,1.),(0.,0.0149999999999997),
 .UNSPECIFIED.);
#56585=B_SPLINE_SURFACE_WITH_KNOTS('',2,1,((#78778,#78779),(#78780,#78781),
(#78782,#78783)),.UNSPECIFIED.,.F.,.F.,.F.,(3,3),(2,2),(0.,1.),(0.,0.0149999999999997),
 .UNSPECIFIED.);
#56586=B_SPLINE_SURFACE_WITH_KNOTS('',2,1,((#78793,#78794),(#78795,#78796),
(#78797,#78798)),.UNSPECIFIED.,.F.,.F.,.F.,(3,3),(2,2),(0.,1.),(0.,0.0149999999999997),
 .UNSPECIFIED.);
#56587=B_SPLINE_SURFACE_WITH_KNOTS('',2,1,((#78814,#78815),(#78816,#78817),
(#78818,#78819)),.UNSPECIFIED.,.F.,.F.,.F.,(3,3),(2,2),(0.,1.),(0.,0.0149999999999997),
 .UNSPECIFIED.);
#56588=B_SPLINE_SURFACE_WITH_KNOTS('',2,1,((#78829,#78830),(#78831,#78832),
(#78833,#78834)),.UNSPECIFIED.,.F.,.F.,.F.,(3,3),(2,2),(0.,1.),(0.,0.0149999999999997),
 .UNSPECIFIED.);
#56589=B_SPLINE_SURFACE_WITH_KNOTS('',2,1,((#78847,#78848),(#78849,#78850),
(#78851,#78852)),.UNSPECIFIED.,.F.,.F.,.F.,(3,3),(2,2),(0.,1.),(0.,0.0149999999999997),
 .UNSPECIFIED.);
#56590=B_SPLINE_SURFACE_WITH_KNOTS('',2,1,((#78862,#78863),(#78864,#78865),
(#78866,#78867)),.UNSPECIFIED.,.F.,.F.,.F.,(3,3),(2,2),(0.,1.),(0.,0.0149999999999997),
 .UNSPECIFIED.);
#56591=B_SPLINE_SURFACE_WITH_KNOTS('',2,1,((#78877,#78878),(#78879,#78880),
(#78881,#78882)),.UNSPECIFIED.,.F.,.F.,.F.,(3,3),(2,2),(0.,1.),(0.,0.0149999999999997),
 .UNSPECIFIED.);
#56592=B_SPLINE_SURFACE_WITH_KNOTS('',2,1,((#78892,#78893),(#78894,#78895),
(#78896,#78897)),.UNSPECIFIED.,.F.,.F.,.F.,(3,3),(2,2),(0.,1.),(0.,0.0149999999999997),
 .UNSPECIFIED.);
#56593=B_SPLINE_SURFACE_WITH_KNOTS('',2,1,((#78907,#78908),(#78909,#78910),
(#78911,#78912)),.UNSPECIFIED.,.F.,.F.,.F.,(3,3),(2,2),(0.,1.),(0.,0.0149999999999997),
 .UNSPECIFIED.);
#56594=B_SPLINE_SURFACE_WITH_KNOTS('',2,1,((#78922,#78923),(#78924,#78925),
(#78926,#78927)),.UNSPECIFIED.,.F.,.F.,.F.,(3,3),(2,2),(0.,1.),(0.,0.0149999999999997),
 .UNSPECIFIED.);
#56595=B_SPLINE_SURFACE_WITH_KNOTS('',2,1,((#78937,#78938),(#78939,#78940),
(#78941,#78942)),.UNSPECIFIED.,.F.,.F.,.F.,(3,3),(2,2),(0.,1.),(0.,0.0149999999999997),
 .UNSPECIFIED.);
#56596=B_SPLINE_SURFACE_WITH_KNOTS('',2,1,((#78949,#78950),(#78951,#78952),
(#78953,#78954)),.UNSPECIFIED.,.F.,.F.,.F.,(3,3),(2,2),(0.,1.),(0.,0.0149999999999997),
 .UNSPECIFIED.);
#56597=B_SPLINE_SURFACE_WITH_KNOTS('',2,1,((#78967,#78968),(#78969,#78970),
(#78971,#78972)),.UNSPECIFIED.,.F.,.F.,.F.,(3,3),(2,2),(0.,1.),(0.,0.0149999999999997),
 .UNSPECIFIED.);
#56598=B_SPLINE_SURFACE_WITH_KNOTS('',2,1,((#78982,#78983),(#78984,#78985),
(#78986,#78987)),.UNSPECIFIED.,.F.,.F.,.F.,(3,3),(2,2),(0.,1.),(0.,0.0149999999999997),
 .UNSPECIFIED.);
#56599=B_SPLINE_SURFACE_WITH_KNOTS('',2,1,((#78997,#78998),(#78999,#79000),
(#79001,#79002)),.UNSPECIFIED.,.F.,.F.,.F.,(3,3),(2,2),(0.,1.),(0.,0.0149999999999997),
 .UNSPECIFIED.);
#56600=B_SPLINE_SURFACE_WITH_KNOTS('',2,1,((#79012,#79013),(#79014,#79015),
(#79016,#79017)),.UNSPECIFIED.,.F.,.F.,.F.,(3,3),(2,2),(0.,1.),(0.,0.0149999999999997),
 .UNSPECIFIED.);
#56601=B_SPLINE_SURFACE_WITH_KNOTS('',2,1,((#79027,#79028),(#79029,#79030),
(#79031,#79032)),.UNSPECIFIED.,.F.,.F.,.F.,(3,3),(2,2),(0.,1.),(0.,0.0149999999999997),
 .UNSPECIFIED.);
#56602=B_SPLINE_SURFACE_WITH_KNOTS('',2,1,((#79042,#79043),(#79044,#79045),
(#79046,#79047)),.UNSPECIFIED.,.F.,.F.,.F.,(3,3),(2,2),(0.,1.),(0.,0.0149999999999997),
 .UNSPECIFIED.);
#56603=B_SPLINE_SURFACE_WITH_KNOTS('',2,1,((#79057,#79058),(#79059,#79060),
(#79061,#79062)),.UNSPECIFIED.,.F.,.F.,.F.,(3,3),(2,2),(0.,1.),(0.,0.0149999999999997),
 .UNSPECIFIED.);
#56604=B_SPLINE_SURFACE_WITH_KNOTS('',2,1,((#79072,#79073),(#79074,#79075),
(#79076,#79077)),.UNSPECIFIED.,.F.,.F.,.F.,(3,3),(2,2),(0.,1.),(0.,0.0149999999999997),
 .UNSPECIFIED.);
#56605=B_SPLINE_SURFACE_WITH_KNOTS('',2,1,((#79087,#79088),(#79089,#79090),
(#79091,#79092)),.UNSPECIFIED.,.F.,.F.,.F.,(3,3),(2,2),(0.,1.),(0.,0.0149999999999997),
 .UNSPECIFIED.);
#56606=B_SPLINE_SURFACE_WITH_KNOTS('',2,1,((#79102,#79103),(#79104,#79105),
(#79106,#79107)),.UNSPECIFIED.,.F.,.F.,.F.,(3,3),(2,2),(0.,1.),(0.,0.0149999999999997),
 .UNSPECIFIED.);
#56607=B_SPLINE_SURFACE_WITH_KNOTS('',2,1,((#79117,#79118),(#79119,#79120),
(#79121,#79122)),.UNSPECIFIED.,.F.,.F.,.F.,(3,3),(2,2),(0.,1.),(0.,0.0149999999999997),
 .UNSPECIFIED.);
#56608=B_SPLINE_SURFACE_WITH_KNOTS('',2,1,((#79130,#79131),(#79132,#79133),
(#79134,#79135)),.UNSPECIFIED.,.F.,.F.,.F.,(3,3),(2,2),(0.,1.),(0.,0.0149999999999997),
 .UNSPECIFIED.);
#56609=B_SPLINE_SURFACE_WITH_KNOTS('',2,1,((#79148,#79149),(#79150,#79151),
(#79152,#79153)),.UNSPECIFIED.,.F.,.F.,.F.,(3,3),(2,2),(0.,1.),(0.,0.0149999999999997),
 .UNSPECIFIED.);
#56610=B_SPLINE_SURFACE_WITH_KNOTS('',2,1,((#79163,#79164),(#79165,#79166),
(#79167,#79168)),.UNSPECIFIED.,.F.,.F.,.F.,(3,3),(2,2),(0.,1.),(0.,0.0149999999999997),
 .UNSPECIFIED.);
#56611=B_SPLINE_SURFACE_WITH_KNOTS('',2,1,((#79178,#79179),(#79180,#79181),
(#79182,#79183)),.UNSPECIFIED.,.F.,.F.,.F.,(3,3),(2,2),(0.,1.),(0.,0.0149999999999997),
 .UNSPECIFIED.);
#56612=B_SPLINE_SURFACE_WITH_KNOTS('',2,1,((#79193,#79194),(#79195,#79196),
(#79197,#79198)),.UNSPECIFIED.,.F.,.F.,.F.,(3,3),(2,2),(0.,1.),(0.,0.0149999999999997),
 .UNSPECIFIED.);
#56613=B_SPLINE_SURFACE_WITH_KNOTS('',2,1,((#79208,#79209),(#79210,#79211),
(#79212,#79213)),.UNSPECIFIED.,.F.,.F.,.F.,(3,3),(2,2),(0.,1.),(0.,0.0149999999999997),
 .UNSPECIFIED.);
#56614=B_SPLINE_SURFACE_WITH_KNOTS('',2,1,((#79259,#79260),(#79261,#79262),
(#79263,#79264)),.UNSPECIFIED.,.F.,.F.,.F.,(3,3),(2,2),(0.,1.),(0.,0.0149999999999997),
 .UNSPECIFIED.);
#56615=B_SPLINE_SURFACE_WITH_KNOTS('',2,1,((#79274,#79275),(#79276,#79277),
(#79278,#79279)),.UNSPECIFIED.,.F.,.F.,.F.,(3,3),(2,2),(0.,1.),(0.,0.0149999999999997),
 .UNSPECIFIED.);
#56616=B_SPLINE_SURFACE_WITH_KNOTS('',2,1,((#79289,#79290),(#79291,#79292),
(#79293,#79294)),.UNSPECIFIED.,.F.,.F.,.F.,(3,3),(2,2),(0.,1.),(0.,0.0149999999999997),
 .UNSPECIFIED.);
#56617=B_SPLINE_SURFACE_WITH_KNOTS('',2,1,((#79304,#79305),(#79306,#79307),
(#79308,#79309)),.UNSPECIFIED.,.F.,.F.,.F.,(3,3),(2,2),(0.,1.),(0.,0.0149999999999997),
 .UNSPECIFIED.);
#56618=B_SPLINE_SURFACE_WITH_KNOTS('',2,1,((#79319,#79320),(#79321,#79322),
(#79323,#79324)),.UNSPECIFIED.,.F.,.F.,.F.,(3,3),(2,2),(0.,1.),(0.,0.0149999999999997),
 .UNSPECIFIED.);
#56619=B_SPLINE_SURFACE_WITH_KNOTS('',2,1,((#79334,#79335),(#79336,#79337),
(#79338,#79339)),.UNSPECIFIED.,.F.,.F.,.F.,(3,3),(2,2),(0.,1.),(0.,0.0149999999999997),
 .UNSPECIFIED.);
#56620=B_SPLINE_SURFACE_WITH_KNOTS('',2,1,((#79349,#79350),(#79351,#79352),
(#79353,#79354)),.UNSPECIFIED.,.F.,.F.,.F.,(3,3),(2,2),(0.,1.),(0.,0.0149999999999997),
 .UNSPECIFIED.);
#56621=B_SPLINE_SURFACE_WITH_KNOTS('',2,1,((#79364,#79365),(#79366,#79367),
(#79368,#79369)),.UNSPECIFIED.,.F.,.F.,.F.,(3,3),(2,2),(0.,1.),(0.,0.0149999999999997),
 .UNSPECIFIED.);
#56622=B_SPLINE_SURFACE_WITH_KNOTS('',2,1,((#79385,#79386),(#79387,#79388),
(#79389,#79390)),.UNSPECIFIED.,.F.,.F.,.F.,(3,3),(2,2),(0.,1.),(0.,0.0149999999999997),
 .UNSPECIFIED.);
#56623=B_SPLINE_SURFACE_WITH_KNOTS('',2,1,((#79399,#79400),(#79401,#79402),
(#79403,#79404)),.UNSPECIFIED.,.F.,.F.,.F.,(3,3),(2,2),(0.,1.),(0.,0.0149999999999997),
 .UNSPECIFIED.);
#56624=B_SPLINE_SURFACE_WITH_KNOTS('',2,1,((#79417,#79418),(#79419,#79420),
(#79421,#79422)),.UNSPECIFIED.,.F.,.F.,.F.,(3,3),(2,2),(0.,1.),(0.,0.0149999999999997),
 .UNSPECIFIED.);
#56625=B_SPLINE_SURFACE_WITH_KNOTS('',2,1,((#79432,#79433),(#79434,#79435),
(#79436,#79437)),.UNSPECIFIED.,.F.,.F.,.F.,(3,3),(2,2),(0.,1.),(0.,0.0149999999999997),
 .UNSPECIFIED.);
#56626=B_SPLINE_SURFACE_WITH_KNOTS('',2,1,((#79447,#79448),(#79449,#79450),
(#79451,#79452)),.UNSPECIFIED.,.F.,.F.,.F.,(3,3),(2,2),(0.,1.),(0.,0.0149999999999997),
 .UNSPECIFIED.);
#56627=B_SPLINE_SURFACE_WITH_KNOTS('',2,1,((#79462,#79463),(#79464,#79465),
(#79466,#79467)),.UNSPECIFIED.,.F.,.F.,.F.,(3,3),(2,2),(0.,1.),(0.,0.0149999999999997),
 .UNSPECIFIED.);
#56628=B_SPLINE_SURFACE_WITH_KNOTS('',2,1,((#79477,#79478),(#79479,#79480),
(#79481,#79482)),.UNSPECIFIED.,.F.,.F.,.F.,(3,3),(2,2),(0.,1.),(0.,0.0149999999999997),
 .UNSPECIFIED.);
#56629=B_SPLINE_SURFACE_WITH_KNOTS('',2,1,((#79492,#79493),(#79494,#79495),
(#79496,#79497)),.UNSPECIFIED.,.F.,.F.,.F.,(3,3),(2,2),(0.,1.),(0.,0.0149999999999997),
 .UNSPECIFIED.);
#56630=B_SPLINE_SURFACE_WITH_KNOTS('',2,1,((#79507,#79508),(#79509,#79510),
(#79511,#79512)),.UNSPECIFIED.,.F.,.F.,.F.,(3,3),(2,2),(0.,1.),(0.,0.0149999999999997),
 .UNSPECIFIED.);
#56631=B_SPLINE_SURFACE_WITH_KNOTS('',2,1,((#79519,#79520),(#79521,#79522),
(#79523,#79524)),.UNSPECIFIED.,.F.,.F.,.F.,(3,3),(2,2),(0.,1.),(0.,0.0149999999999997),
 .UNSPECIFIED.);
#56632=B_SPLINE_SURFACE_WITH_KNOTS('',2,1,((#79537,#79538),(#79539,#79540),
(#79541,#79542)),.UNSPECIFIED.,.F.,.F.,.F.,(3,3),(2,2),(0.,1.),(0.,0.0149999999999997),
 .UNSPECIFIED.);
#56633=B_SPLINE_SURFACE_WITH_KNOTS('',2,1,((#79552,#79553),(#79554,#79555),
(#79556,#79557)),.UNSPECIFIED.,.F.,.F.,.F.,(3,3),(2,2),(0.,1.),(0.,0.0149999999999997),
 .UNSPECIFIED.);
#56634=B_SPLINE_SURFACE_WITH_KNOTS('',2,1,((#79567,#79568),(#79569,#79570),
(#79571,#79572)),.UNSPECIFIED.,.F.,.F.,.F.,(3,3),(2,2),(0.,1.),(0.,0.0149999999999997),
 .UNSPECIFIED.);
#56635=B_SPLINE_SURFACE_WITH_KNOTS('',2,1,((#79582,#79583),(#79584,#79585),
(#79586,#79587)),.UNSPECIFIED.,.F.,.F.,.F.,(3,3),(2,2),(0.,1.),(0.,0.0149999999999997),
 .UNSPECIFIED.);
#56636=B_SPLINE_SURFACE_WITH_KNOTS('',2,1,((#79597,#79598),(#79599,#79600),
(#79601,#79602)),.UNSPECIFIED.,.F.,.F.,.F.,(3,3),(2,2),(0.,1.),(0.,0.0149999999999997),
 .UNSPECIFIED.);
#56637=B_SPLINE_SURFACE_WITH_KNOTS('',2,1,((#79612,#79613),(#79614,#79615),
(#79616,#79617)),.UNSPECIFIED.,.F.,.F.,.F.,(3,3),(2,2),(0.,1.),(0.,0.0149999999999997),
 .UNSPECIFIED.);
#56638=B_SPLINE_SURFACE_WITH_KNOTS('',2,1,((#79627,#79628),(#79629,#79630),
(#79631,#79632)),.UNSPECIFIED.,.F.,.F.,.F.,(3,3),(2,2),(0.,1.),(0.,0.0149999999999997),
 .UNSPECIFIED.);
#56639=B_SPLINE_SURFACE_WITH_KNOTS('',2,1,((#79642,#79643),(#79644,#79645),
(#79646,#79647)),.UNSPECIFIED.,.F.,.F.,.F.,(3,3),(2,2),(0.,1.),(0.,0.0149999999999997),
 .UNSPECIFIED.);
#56640=B_SPLINE_SURFACE_WITH_KNOTS('',2,1,((#79657,#79658),(#79659,#79660),
(#79661,#79662)),.UNSPECIFIED.,.F.,.F.,.F.,(3,3),(2,2),(0.,1.),(0.,0.0149999999999997),
 .UNSPECIFIED.);
#56641=B_SPLINE_SURFACE_WITH_KNOTS('',2,1,((#79672,#79673),(#79674,#79675),
(#79676,#79677)),.UNSPECIFIED.,.F.,.F.,.F.,(3,3),(2,2),(0.,1.),(0.,0.0149999999999997),
 .UNSPECIFIED.);
#56642=B_SPLINE_SURFACE_WITH_KNOTS('',2,1,((#79687,#79688),(#79689,#79690),
(#79691,#79692)),.UNSPECIFIED.,.F.,.F.,.F.,(3,3),(2,2),(0.,1.),(0.,0.0149999999999997),
 .UNSPECIFIED.);
#56643=B_SPLINE_SURFACE_WITH_KNOTS('',2,1,((#79787,#79788),(#79789,#79790),
(#79791,#79792)),.UNSPECIFIED.,.F.,.F.,.F.,(3,3),(2,2),(0.,1.),(0.,0.0149999999999997),
 .UNSPECIFIED.);
#56644=B_SPLINE_SURFACE_WITH_KNOTS('',2,1,((#79805,#79806),(#79807,#79808),
(#79809,#79810)),.UNSPECIFIED.,.F.,.F.,.F.,(3,3),(2,2),(0.,1.),(0.,0.0149999999999997),
 .UNSPECIFIED.);
#56645=B_SPLINE_SURFACE_WITH_KNOTS('',2,1,((#79820,#79821),(#79822,#79823),
(#79824,#79825)),.UNSPECIFIED.,.F.,.F.,.F.,(3,3),(2,2),(0.,1.),(0.,0.0149999999999997),
 .UNSPECIFIED.);
#56646=B_SPLINE_SURFACE_WITH_KNOTS('',2,1,((#79835,#79836),(#79837,#79838),
(#79839,#79840)),.UNSPECIFIED.,.F.,.F.,.F.,(3,3),(2,2),(0.,1.),(0.,0.0149999999999997),
 .UNSPECIFIED.);
#56647=B_SPLINE_SURFACE_WITH_KNOTS('',2,1,((#79850,#79851),(#79852,#79853),
(#79854,#79855)),.UNSPECIFIED.,.F.,.F.,.F.,(3,3),(2,2),(0.,1.),(0.,0.0149999999999997),
 .UNSPECIFIED.);
#56648=B_SPLINE_SURFACE_WITH_KNOTS('',2,1,((#79865,#79866),(#79867,#79868),
(#79869,#79870)),.UNSPECIFIED.,.F.,.F.,.F.,(3,3),(2,2),(0.,1.),(0.,0.0149999999999997),
 .UNSPECIFIED.);
#56649=B_SPLINE_SURFACE_WITH_KNOTS('',2,1,((#79880,#79881),(#79882,#79883),
(#79884,#79885)),.UNSPECIFIED.,.F.,.F.,.F.,(3,3),(2,2),(0.,1.),(0.,0.0149999999999997),
 .UNSPECIFIED.);
#56650=B_SPLINE_SURFACE_WITH_KNOTS('',2,1,((#79895,#79896),(#79897,#79898),
(#79899,#79900)),.UNSPECIFIED.,.F.,.F.,.F.,(3,3),(2,2),(0.,1.),(0.,0.0149999999999997),
 .UNSPECIFIED.);
#56651=B_SPLINE_SURFACE_WITH_KNOTS('',2,1,((#79907,#79908),(#79909,#79910),
(#79911,#79912)),.UNSPECIFIED.,.F.,.F.,.F.,(3,3),(2,2),(0.,1.),(0.,0.0149999999999997),
 .UNSPECIFIED.);
#56652=B_SPLINE_SURFACE_WITH_KNOTS('',2,1,((#79925,#79926),(#79927,#79928),
(#79929,#79930)),.UNSPECIFIED.,.F.,.F.,.F.,(3,3),(2,2),(0.,1.),(0.,0.0149999999999997),
 .UNSPECIFIED.);
#56653=B_SPLINE_SURFACE_WITH_KNOTS('',2,1,((#79940,#79941),(#79942,#79943),
(#79944,#79945)),.UNSPECIFIED.,.F.,.F.,.F.,(3,3),(2,2),(0.,1.),(0.,0.0149999999999997),
 .UNSPECIFIED.);
#56654=B_SPLINE_SURFACE_WITH_KNOTS('',2,1,((#79955,#79956),(#79957,#79958),
(#79959,#79960)),.UNSPECIFIED.,.F.,.F.,.F.,(3,3),(2,2),(0.,1.),(0.,0.0149999999999997),
 .UNSPECIFIED.);
#56655=B_SPLINE_SURFACE_WITH_KNOTS('',2,1,((#79970,#79971),(#79972,#79973),
(#79974,#79975)),.UNSPECIFIED.,.F.,.F.,.F.,(3,3),(2,2),(0.,1.),(0.,0.0149999999999997),
 .UNSPECIFIED.);
#56656=B_SPLINE_SURFACE_WITH_KNOTS('',2,1,((#79985,#79986),(#79987,#79988),
(#79989,#79990)),.UNSPECIFIED.,.F.,.F.,.F.,(3,3),(2,2),(0.,1.),(0.,0.0149999999999997),
 .UNSPECIFIED.);
#56657=B_SPLINE_SURFACE_WITH_KNOTS('',2,1,((#80000,#80001),(#80002,#80003),
(#80004,#80005)),.UNSPECIFIED.,.F.,.F.,.F.,(3,3),(2,2),(0.,1.),(0.,0.0149999999999997),
 .UNSPECIFIED.);
#56658=B_SPLINE_SURFACE_WITH_KNOTS('',2,1,((#80015,#80016),(#80017,#80018),
(#80019,#80020)),.UNSPECIFIED.,.F.,.F.,.F.,(3,3),(2,2),(0.,1.),(0.,0.0149999999999997),
 .UNSPECIFIED.);
#56659=B_SPLINE_SURFACE_WITH_KNOTS('',2,1,((#80030,#80031),(#80032,#80033),
(#80034,#80035)),.UNSPECIFIED.,.F.,.F.,.F.,(3,3),(2,2),(0.,1.),(0.,0.0149999999999997),
 .UNSPECIFIED.);
#56660=B_SPLINE_SURFACE_WITH_KNOTS('',2,1,((#80045,#80046),(#80047,#80048),
(#80049,#80050)),.UNSPECIFIED.,.F.,.F.,.F.,(3,3),(2,2),(0.,1.),(0.,0.0149999999999997),
 .UNSPECIFIED.);
#56661=B_SPLINE_SURFACE_WITH_KNOTS('',2,1,((#80060,#80061),(#80062,#80063),
(#80064,#80065)),.UNSPECIFIED.,.F.,.F.,.F.,(3,3),(2,2),(0.,1.),(0.,0.0149999999999997),
 .UNSPECIFIED.);
#56662=B_SPLINE_SURFACE_WITH_KNOTS('',2,1,((#80075,#80076),(#80077,#80078),
(#80079,#80080)),.UNSPECIFIED.,.F.,.F.,.F.,(3,3),(2,2),(0.,1.),(0.,0.0149999999999997),
 .UNSPECIFIED.);
#56663=B_SPLINE_SURFACE_WITH_KNOTS('',2,1,((#80088,#80089),(#80090,#80091),
(#80092,#80093)),.UNSPECIFIED.,.F.,.F.,.F.,(3,3),(2,2),(0.,1.),(0.,0.0149999999999997),
 .UNSPECIFIED.);
#56664=B_SPLINE_SURFACE_WITH_KNOTS('',2,1,((#80106,#80107),(#80108,#80109),
(#80110,#80111)),.UNSPECIFIED.,.F.,.F.,.F.,(3,3),(2,2),(0.,1.),(0.,0.0149999999999997),
 .UNSPECIFIED.);
#56665=B_SPLINE_SURFACE_WITH_KNOTS('',2,1,((#80121,#80122),(#80123,#80124),
(#80125,#80126)),.UNSPECIFIED.,.F.,.F.,.F.,(3,3),(2,2),(0.,1.),(0.,0.0149999999999997),
 .UNSPECIFIED.);
#56666=B_SPLINE_SURFACE_WITH_KNOTS('',2,1,((#80136,#80137),(#80138,#80139),
(#80140,#80141)),.UNSPECIFIED.,.F.,.F.,.F.,(3,3),(2,2),(0.,1.),(0.,0.0149999999999997),
 .UNSPECIFIED.);
#56667=B_SPLINE_SURFACE_WITH_KNOTS('',2,1,((#80151,#80152),(#80153,#80154),
(#80155,#80156)),.UNSPECIFIED.,.F.,.F.,.F.,(3,3),(2,2),(0.,1.),(0.,0.0149999999999997),
 .UNSPECIFIED.);
#56668=B_SPLINE_SURFACE_WITH_KNOTS('',2,1,((#80166,#80167),(#80168,#80169),
(#80170,#80171)),.UNSPECIFIED.,.F.,.F.,.F.,(3,3),(2,2),(0.,1.),(0.,0.0149999999999997),
 .UNSPECIFIED.);
#56669=B_SPLINE_SURFACE_WITH_KNOTS('',2,1,((#80181,#80182),(#80183,#80184),
(#80185,#80186)),.UNSPECIFIED.,.F.,.F.,.F.,(3,3),(2,2),(0.,1.),(0.,0.0149999999999997),
 .UNSPECIFIED.);
#56670=B_SPLINE_SURFACE_WITH_KNOTS('',2,1,((#80196,#80197),(#80198,#80199),
(#80200,#80201)),.UNSPECIFIED.,.F.,.F.,.F.,(3,3),(2,2),(0.,1.),(0.,0.0149999999999997),
 .UNSPECIFIED.);
#56671=B_SPLINE_SURFACE_WITH_KNOTS('',2,1,((#80211,#80212),(#80213,#80214),
(#80215,#80216)),.UNSPECIFIED.,.F.,.F.,.F.,(3,3),(2,2),(0.,1.),(0.,0.0149999999999997),
 .UNSPECIFIED.);
#56672=B_SPLINE_SURFACE_WITH_KNOTS('',2,1,((#80226,#80227),(#80228,#80229),
(#80230,#80231)),.UNSPECIFIED.,.F.,.F.,.F.,(3,3),(2,2),(0.,1.),(0.,0.0149999999999997),
 .UNSPECIFIED.);
#56673=B_SPLINE_SURFACE_WITH_KNOTS('',2,1,((#80241,#80242),(#80243,#80244),
(#80245,#80246)),.UNSPECIFIED.,.F.,.F.,.F.,(3,3),(2,2),(0.,1.),(0.,0.0149999999999997),
 .UNSPECIFIED.);
#56674=B_SPLINE_SURFACE_WITH_KNOTS('',2,1,((#80256,#80257),(#80258,#80259),
(#80260,#80261)),.UNSPECIFIED.,.F.,.F.,.F.,(3,3),(2,2),(0.,1.),(0.,0.0149999999999997),
 .UNSPECIFIED.);
#56675=B_SPLINE_SURFACE_WITH_KNOTS('',2,1,((#80277,#80278),(#80279,#80280),
(#80281,#80282)),.UNSPECIFIED.,.F.,.F.,.F.,(3,3),(2,2),(0.,1.),(0.,0.0149999999999997),
 .UNSPECIFIED.);
#56676=B_SPLINE_SURFACE_WITH_KNOTS('',2,1,((#80292,#80293),(#80294,#80295),
(#80296,#80297)),.UNSPECIFIED.,.F.,.F.,.F.,(3,3),(2,2),(0.,1.),(0.,0.0149999999999997),
 .UNSPECIFIED.);
#56677=B_SPLINE_SURFACE_WITH_KNOTS('',2,1,((#80307,#80308),(#80309,#80310),
(#80311,#80312)),.UNSPECIFIED.,.F.,.F.,.F.,(3,3),(2,2),(0.,1.),(0.,0.0149999999999997),
 .UNSPECIFIED.);
#56678=B_SPLINE_SURFACE_WITH_KNOTS('',2,1,((#80322,#80323),(#80324,#80325),
(#80326,#80327)),.UNSPECIFIED.,.F.,.F.,.F.,(3,3),(2,2),(0.,1.),(0.,0.0149999999999997),
 .UNSPECIFIED.);
#56679=B_SPLINE_SURFACE_WITH_KNOTS('',2,1,((#80337,#80338),(#80339,#80340),
(#80341,#80342)),.UNSPECIFIED.,.F.,.F.,.F.,(3,3),(2,2),(0.,1.),(0.,0.0149999999999997),
 .UNSPECIFIED.);
#56680=B_SPLINE_SURFACE_WITH_KNOTS('',2,1,((#80352,#80353),(#80354,#80355),
(#80356,#80357)),.UNSPECIFIED.,.F.,.F.,.F.,(3,3),(2,2),(0.,1.),(0.,0.0149999999999997),
 .UNSPECIFIED.);
#56681=B_SPLINE_SURFACE_WITH_KNOTS('',2,1,((#80367,#80368),(#80369,#80370),
(#80371,#80372)),.UNSPECIFIED.,.F.,.F.,.F.,(3,3),(2,2),(0.,1.),(0.,0.0149999999999997),
 .UNSPECIFIED.);
#56682=B_SPLINE_SURFACE_WITH_KNOTS('',2,1,((#80388,#80389),(#80390,#80391),
(#80392,#80393)),.UNSPECIFIED.,.F.,.F.,.F.,(3,3),(2,2),(0.,1.),(0.,0.0149999999999997),
 .UNSPECIFIED.);
#56683=B_SPLINE_SURFACE_WITH_KNOTS('',2,1,((#80403,#80404),(#80405,#80406),
(#80407,#80408)),.UNSPECIFIED.,.F.,.F.,.F.,(3,3),(2,2),(0.,1.),(0.,0.0149999999999997),
 .UNSPECIFIED.);
#56684=B_SPLINE_SURFACE_WITH_KNOTS('',2,1,((#80418,#80419),(#80420,#80421),
(#80422,#80423)),.UNSPECIFIED.,.F.,.F.,.F.,(3,3),(2,2),(0.,1.),(0.,0.0149999999999997),
 .UNSPECIFIED.);
#56685=B_SPLINE_SURFACE_WITH_KNOTS('',2,1,((#80433,#80434),(#80435,#80436),
(#80437,#80438)),.UNSPECIFIED.,.F.,.F.,.F.,(3,3),(2,2),(0.,1.),(0.,0.0149999999999997),
 .UNSPECIFIED.);
#56686=B_SPLINE_SURFACE_WITH_KNOTS('',2,1,((#80448,#80449),(#80450,#80451),
(#80452,#80453)),.UNSPECIFIED.,.F.,.F.,.F.,(3,3),(2,2),(0.,1.),(0.,0.0149999999999997),
 .UNSPECIFIED.);
#56687=B_SPLINE_SURFACE_WITH_KNOTS('',2,1,((#80463,#80464),(#80465,#80466),
(#80467,#80468)),.UNSPECIFIED.,.F.,.F.,.F.,(3,3),(2,2),(0.,1.),(0.,0.0149999999999997),
 .UNSPECIFIED.);
#56688=B_SPLINE_SURFACE_WITH_KNOTS('',2,1,((#80478,#80479),(#80480,#80481),
(#80482,#80483)),.UNSPECIFIED.,.F.,.F.,.F.,(3,3),(2,2),(0.,1.),(0.,0.0149999999999997),
 .UNSPECIFIED.);
#56689=B_SPLINE_SURFACE_WITH_KNOTS('',2,1,((#80499,#80500),(#80501,#80502),
(#80503,#80504)),.UNSPECIFIED.,.F.,.F.,.F.,(3,3),(2,2),(0.,1.),(0.,0.0149999999999997),
 .UNSPECIFIED.);
#56690=B_SPLINE_SURFACE_WITH_KNOTS('',2,1,((#80513,#80514),(#80515,#80516),
(#80517,#80518)),.UNSPECIFIED.,.F.,.F.,.F.,(3,3),(2,2),(0.,1.),(0.,0.0149999999999997),
 .UNSPECIFIED.);
#56691=B_SPLINE_SURFACE_WITH_KNOTS('',2,1,((#80531,#80532),(#80533,#80534),
(#80535,#80536)),.UNSPECIFIED.,.F.,.F.,.F.,(3,3),(2,2),(0.,1.),(0.,0.0149999999999997),
 .UNSPECIFIED.);
#56692=B_SPLINE_SURFACE_WITH_KNOTS('',2,1,((#80546,#80547),(#80548,#80549),
(#80550,#80551)),.UNSPECIFIED.,.F.,.F.,.F.,(3,3),(2,2),(0.,1.),(0.,0.0149999999999997),
 .UNSPECIFIED.);
#56693=B_SPLINE_SURFACE_WITH_KNOTS('',2,1,((#80561,#80562),(#80563,#80564),
(#80565,#80566)),.UNSPECIFIED.,.F.,.F.,.F.,(3,3),(2,2),(0.,1.),(0.,0.0149999999999997),
 .UNSPECIFIED.);
#56694=B_SPLINE_SURFACE_WITH_KNOTS('',2,1,((#80576,#80577),(#80578,#80579),
(#80580,#80581)),.UNSPECIFIED.,.F.,.F.,.F.,(3,3),(2,2),(0.,1.),(0.,0.0149999999999997),
 .UNSPECIFIED.);
#56695=B_SPLINE_SURFACE_WITH_KNOTS('',2,1,((#80591,#80592),(#80593,#80594),
(#80595,#80596)),.UNSPECIFIED.,.F.,.F.,.F.,(3,3),(2,2),(0.,1.),(0.,0.0149999999999997),
 .UNSPECIFIED.);
#56696=B_SPLINE_SURFACE_WITH_KNOTS('',2,1,((#80606,#80607),(#80608,#80609),
(#80610,#80611)),.UNSPECIFIED.,.F.,.F.,.F.,(3,3),(2,2),(0.,1.),(0.,0.0149999999999997),
 .UNSPECIFIED.);
#56697=B_SPLINE_SURFACE_WITH_KNOTS('',2,1,((#80621,#80622),(#80623,#80624),
(#80625,#80626)),.UNSPECIFIED.,.F.,.F.,.F.,(3,3),(2,2),(0.,1.),(0.,0.0149999999999997),
 .UNSPECIFIED.);
#56698=B_SPLINE_SURFACE_WITH_KNOTS('',2,1,((#80633,#80634),(#80635,#80636),
(#80637,#80638)),.UNSPECIFIED.,.F.,.F.,.F.,(3,3),(2,2),(0.,1.),(0.,0.0149999999999997),
 .UNSPECIFIED.);
#56699=B_SPLINE_SURFACE_WITH_KNOTS('',2,1,((#80651,#80652),(#80653,#80654),
(#80655,#80656)),.UNSPECIFIED.,.F.,.F.,.F.,(3,3),(2,2),(0.,1.),(0.,0.0149999999999997),
 .UNSPECIFIED.);
#56700=B_SPLINE_SURFACE_WITH_KNOTS('',2,1,((#80666,#80667),(#80668,#80669),
(#80670,#80671)),.UNSPECIFIED.,.F.,.F.,.F.,(3,3),(2,2),(0.,1.),(0.,0.0149999999999997),
 .UNSPECIFIED.);
#56701=B_SPLINE_SURFACE_WITH_KNOTS('',2,1,((#80681,#80682),(#80683,#80684),
(#80685,#80686)),.UNSPECIFIED.,.F.,.F.,.F.,(3,3),(2,2),(0.,1.),(0.,0.0149999999999997),
 .UNSPECIFIED.);
#56702=B_SPLINE_SURFACE_WITH_KNOTS('',2,1,((#80696,#80697),(#80698,#80699),
(#80700,#80701)),.UNSPECIFIED.,.F.,.F.,.F.,(3,3),(2,2),(0.,1.),(0.,0.0149999999999997),
 .UNSPECIFIED.);
#56703=B_SPLINE_SURFACE_WITH_KNOTS('',2,1,((#80711,#80712),(#80713,#80714),
(#80715,#80716)),.UNSPECIFIED.,.F.,.F.,.F.,(3,3),(2,2),(0.,1.),(0.,0.0149999999999997),
 .UNSPECIFIED.);
#56704=B_SPLINE_SURFACE_WITH_KNOTS('',2,1,((#80726,#80727),(#80728,#80729),
(#80730,#80731)),.UNSPECIFIED.,.F.,.F.,.F.,(3,3),(2,2),(0.,1.),(0.,0.0149999999999997),
 .UNSPECIFIED.);
#56705=B_SPLINE_SURFACE_WITH_KNOTS('',2,1,((#80741,#80742),(#80743,#80744),
(#80745,#80746)),.UNSPECIFIED.,.F.,.F.,.F.,(3,3),(2,2),(0.,1.),(0.,0.0149999999999997),
 .UNSPECIFIED.);
#56706=B_SPLINE_SURFACE_WITH_KNOTS('',2,1,((#80756,#80757),(#80758,#80759),
(#80760,#80761)),.UNSPECIFIED.,.F.,.F.,.F.,(3,3),(2,2),(0.,1.),(0.,0.0149999999999997),
 .UNSPECIFIED.);
#56707=B_SPLINE_SURFACE_WITH_KNOTS('',2,1,((#80771,#80772),(#80773,#80774),
(#80775,#80776)),.UNSPECIFIED.,.F.,.F.,.F.,(3,3),(2,2),(0.,1.),(0.,0.0149999999999997),
 .UNSPECIFIED.);
#56708=B_SPLINE_SURFACE_WITH_KNOTS('',2,1,((#80786,#80787),(#80788,#80789),
(#80790,#80791)),.UNSPECIFIED.,.F.,.F.,.F.,(3,3),(2,2),(0.,1.),(0.,0.0149999999999997),
 .UNSPECIFIED.);
#56709=B_SPLINE_SURFACE_WITH_KNOTS('',2,1,((#80801,#80802),(#80803,#80804),
(#80805,#80806)),.UNSPECIFIED.,.F.,.F.,.F.,(3,3),(2,2),(0.,1.),(0.,0.0149999999999997),
 .UNSPECIFIED.);
#56710=B_SPLINE_SURFACE_WITH_KNOTS('',2,1,((#80814,#80815),(#80816,#80817),
(#80818,#80819)),.UNSPECIFIED.,.F.,.F.,.F.,(3,3),(2,2),(0.,1.),(0.,0.0149999999999997),
 .UNSPECIFIED.);
#56711=B_SPLINE_SURFACE_WITH_KNOTS('',2,1,((#80832,#80833),(#80834,#80835),
(#80836,#80837)),.UNSPECIFIED.,.F.,.F.,.F.,(3,3),(2,2),(0.,1.),(0.,0.0149999999999997),
 .UNSPECIFIED.);
#56712=B_SPLINE_SURFACE_WITH_KNOTS('',2,1,((#80847,#80848),(#80849,#80850),
(#80851,#80852)),.UNSPECIFIED.,.F.,.F.,.F.,(3,3),(2,2),(0.,1.),(0.,0.0149999999999997),
 .UNSPECIFIED.);
#56713=B_SPLINE_SURFACE_WITH_KNOTS('',2,1,((#80862,#80863),(#80864,#80865),
(#80866,#80867)),.UNSPECIFIED.,.F.,.F.,.F.,(3,3),(2,2),(0.,1.),(0.,0.0149999999999997),
 .UNSPECIFIED.);
#56714=B_SPLINE_SURFACE_WITH_KNOTS('',2,1,((#80877,#80878),(#80879,#80880),
(#80881,#80882)),.UNSPECIFIED.,.F.,.F.,.F.,(3,3),(2,2),(0.,1.),(0.,0.0149999999999997),
 .UNSPECIFIED.);
#56715=B_SPLINE_SURFACE_WITH_KNOTS('',2,1,((#80892,#80893),(#80894,#80895),
(#80896,#80897)),.UNSPECIFIED.,.F.,.F.,.F.,(3,3),(2,2),(0.,1.),(0.,0.0149999999999997),
 .UNSPECIFIED.);
#56716=B_SPLINE_SURFACE_WITH_KNOTS('',2,1,((#80907,#80908),(#80909,#80910),
(#80911,#80912)),.UNSPECIFIED.,.F.,.F.,.F.,(3,3),(2,2),(0.,1.),(0.,0.0149999999999997),
 .UNSPECIFIED.);
#56717=B_SPLINE_SURFACE_WITH_KNOTS('',2,1,((#80922,#80923),(#80924,#80925),
(#80926,#80927)),.UNSPECIFIED.,.F.,.F.,.F.,(3,3),(2,2),(0.,1.),(0.,0.0149999999999997),
 .UNSPECIFIED.);
#56718=B_SPLINE_SURFACE_WITH_KNOTS('',2,1,((#80937,#80938),(#80939,#80940),
(#80941,#80942)),.UNSPECIFIED.,.F.,.F.,.F.,(3,3),(2,2),(0.,1.),(0.,0.0149999999999997),
 .UNSPECIFIED.);
#56719=B_SPLINE_SURFACE_WITH_KNOTS('',2,1,((#80958,#80959),(#80960,#80961),
(#80962,#80963)),.UNSPECIFIED.,.F.,.F.,.F.,(3,3),(2,2),(0.,1.),(0.,0.0149999999999997),
 .UNSPECIFIED.);
#56720=B_SPLINE_SURFACE_WITH_KNOTS('',2,1,((#80973,#80974),(#80975,#80976),
(#80977,#80978)),.UNSPECIFIED.,.F.,.F.,.F.,(3,3),(2,2),(0.,1.),(0.,0.0149999999999997),
 .UNSPECIFIED.);
#56721=B_SPLINE_SURFACE_WITH_KNOTS('',2,1,((#80988,#80989),(#80990,#80991),
(#80992,#80993)),.UNSPECIFIED.,.F.,.F.,.F.,(3,3),(2,2),(0.,1.),(0.,0.0149999999999997),
 .UNSPECIFIED.);
#56722=B_SPLINE_SURFACE_WITH_KNOTS('',2,1,((#81003,#81004),(#81005,#81006),
(#81007,#81008)),.UNSPECIFIED.,.F.,.F.,.F.,(3,3),(2,2),(0.,1.),(0.,0.0149999999999997),
 .UNSPECIFIED.);
#56723=B_SPLINE_SURFACE_WITH_KNOTS('',2,1,((#81018,#81019),(#81020,#81021),
(#81022,#81023)),.UNSPECIFIED.,.F.,.F.,.F.,(3,3),(2,2),(0.,1.),(0.,0.0149999999999997),
 .UNSPECIFIED.);
#56724=B_SPLINE_SURFACE_WITH_KNOTS('',2,1,((#81033,#81034),(#81035,#81036),
(#81037,#81038)),.UNSPECIFIED.,.F.,.F.,.F.,(3,3),(2,2),(0.,1.),(0.,0.0149999999999997),
 .UNSPECIFIED.);
#56725=B_SPLINE_SURFACE_WITH_KNOTS('',2,1,((#81048,#81049),(#81050,#81051),
(#81052,#81053)),.UNSPECIFIED.,.F.,.F.,.F.,(3,3),(2,2),(0.,1.),(0.,0.0149999999999997),
 .UNSPECIFIED.);
#56726=B_SPLINE_SURFACE_WITH_KNOTS('',2,1,((#81063,#81064),(#81065,#81066),
(#81067,#81068)),.UNSPECIFIED.,.F.,.F.,.F.,(3,3),(2,2),(0.,1.),(0.,0.0149999999999997),
 .UNSPECIFIED.);
#56727=B_SPLINE_SURFACE_WITH_KNOTS('',2,1,((#81078,#81079),(#81080,#81081),
(#81082,#81083)),.UNSPECIFIED.,.F.,.F.,.F.,(3,3),(2,2),(0.,1.),(0.,0.0149999999999997),
 .UNSPECIFIED.);
#56728=B_SPLINE_SURFACE_WITH_KNOTS('',2,1,((#81110,#81111),(#81112,#81113),
(#81114,#81115)),.UNSPECIFIED.,.F.,.F.,.F.,(3,3),(2,2),(0.,1.),(0.,0.0149999999999997),
 .UNSPECIFIED.);
#56729=B_SPLINE_SURFACE_WITH_KNOTS('',2,1,((#81128,#81129),(#81130,#81131),
(#81132,#81133)),.UNSPECIFIED.,.F.,.F.,.F.,(3,3),(2,2),(0.,1.),(0.,0.0149999999999997),
 .UNSPECIFIED.);
#56730=B_SPLINE_SURFACE_WITH_KNOTS('',2,1,((#81143,#81144),(#81145,#81146),
(#81147,#81148)),.UNSPECIFIED.,.F.,.F.,.F.,(3,3),(2,2),(0.,1.),(0.,0.0149999999999997),
 .UNSPECIFIED.);
#56731=B_SPLINE_SURFACE_WITH_KNOTS('',2,1,((#81158,#81159),(#81160,#81161),
(#81162,#81163)),.UNSPECIFIED.,.F.,.F.,.F.,(3,3),(2,2),(0.,1.),(0.,0.0149999999999997),
 .UNSPECIFIED.);
#56732=B_SPLINE_SURFACE_WITH_KNOTS('',2,1,((#81173,#81174),(#81175,#81176),
(#81177,#81178)),.UNSPECIFIED.,.F.,.F.,.F.,(3,3),(2,2),(0.,1.),(0.,0.0149999999999997),
 .UNSPECIFIED.);
#56733=B_SPLINE_SURFACE_WITH_KNOTS('',2,1,((#81188,#81189),(#81190,#81191),
(#81192,#81193)),.UNSPECIFIED.,.F.,.F.,.F.,(3,3),(2,2),(0.,1.),(0.,0.0149999999999997),
 .UNSPECIFIED.);
#56734=B_SPLINE_SURFACE_WITH_KNOTS('',2,1,((#81203,#81204),(#81205,#81206),
(#81207,#81208)),.UNSPECIFIED.,.F.,.F.,.F.,(3,3),(2,2),(0.,1.),(0.,0.0149999999999997),
 .UNSPECIFIED.);
#56735=B_SPLINE_SURFACE_WITH_KNOTS('',2,1,((#81218,#81219),(#81220,#81221),
(#81222,#81223)),.UNSPECIFIED.,.F.,.F.,.F.,(3,3),(2,2),(0.,1.),(0.,0.0149999999999997),
 .UNSPECIFIED.);
#56736=B_SPLINE_SURFACE_WITH_KNOTS('',2,1,((#81230,#81231),(#81232,#81233),
(#81234,#81235)),.UNSPECIFIED.,.F.,.F.,.F.,(3,3),(2,2),(0.,1.),(0.,0.0149999999999997),
 .UNSPECIFIED.);
#56737=B_SPLINE_SURFACE_WITH_KNOTS('',2,1,((#81248,#81249),(#81250,#81251),
(#81252,#81253)),.UNSPECIFIED.,.F.,.F.,.F.,(3,3),(2,2),(0.,1.),(0.,0.0149999999999997),
 .UNSPECIFIED.);
#56738=B_SPLINE_SURFACE_WITH_KNOTS('',2,1,((#81263,#81264),(#81265,#81266),
(#81267,#81268)),.UNSPECIFIED.,.F.,.F.,.F.,(3,3),(2,2),(0.,1.),(0.,0.0149999999999997),
 .UNSPECIFIED.);
#56739=B_SPLINE_SURFACE_WITH_KNOTS('',2,1,((#81278,#81279),(#81280,#81281),
(#81282,#81283)),.UNSPECIFIED.,.F.,.F.,.F.,(3,3),(2,2),(0.,1.),(0.,0.0149999999999997),
 .UNSPECIFIED.);
#56740=B_SPLINE_SURFACE_WITH_KNOTS('',2,1,((#81293,#81294),(#81295,#81296),
(#81297,#81298)),.UNSPECIFIED.,.F.,.F.,.F.,(3,3),(2,2),(0.,1.),(0.,0.0149999999999997),
 .UNSPECIFIED.);
#56741=B_SPLINE_SURFACE_WITH_KNOTS('',2,1,((#81308,#81309),(#81310,#81311),
(#81312,#81313)),.UNSPECIFIED.,.F.,.F.,.F.,(3,3),(2,2),(0.,1.),(0.,0.0149999999999997),
 .UNSPECIFIED.);
#56742=B_SPLINE_SURFACE_WITH_KNOTS('',2,1,((#81323,#81324),(#81325,#81326),
(#81327,#81328)),.UNSPECIFIED.,.F.,.F.,.F.,(3,3),(2,2),(0.,1.),(0.,0.0149999999999997),
 .UNSPECIFIED.);
#56743=B_SPLINE_SURFACE_WITH_KNOTS('',2,1,((#81338,#81339),(#81340,#81341),
(#81342,#81343)),.UNSPECIFIED.,.F.,.F.,.F.,(3,3),(2,2),(0.,1.),(0.,0.0149999999999997),
 .UNSPECIFIED.);
#56744=B_SPLINE_SURFACE_WITH_KNOTS('',2,1,((#81353,#81354),(#81355,#81356),
(#81357,#81358)),.UNSPECIFIED.,.F.,.F.,.F.,(3,3),(2,2),(0.,1.),(0.,0.0149999999999997),
 .UNSPECIFIED.);
#56745=B_SPLINE_SURFACE_WITH_KNOTS('',2,1,((#81368,#81369),(#81370,#81371),
(#81372,#81373)),.UNSPECIFIED.,.F.,.F.,.F.,(3,3),(2,2),(0.,1.),(0.,0.0149999999999997),
 .UNSPECIFIED.);
#56746=B_SPLINE_SURFACE_WITH_KNOTS('',2,1,((#81383,#81384),(#81385,#81386),
(#81387,#81388)),.UNSPECIFIED.,.F.,.F.,.F.,(3,3),(2,2),(0.,1.),(0.,0.0149999999999997),
 .UNSPECIFIED.);
#56747=B_SPLINE_SURFACE_WITH_KNOTS('',2,1,((#81398,#81399),(#81400,#81401),
(#81402,#81403)),.UNSPECIFIED.,.F.,.F.,.F.,(3,3),(2,2),(0.,1.),(0.,0.0149999999999997),
 .UNSPECIFIED.);
#56748=B_SPLINE_SURFACE_WITH_KNOTS('',2,1,((#81420,#81421),(#81422,#81423),
(#81424,#81425)),.UNSPECIFIED.,.F.,.F.,.F.,(3,3),(2,2),(0.,1.),(0.,0.0149999999999997),
 .UNSPECIFIED.);
#56749=B_SPLINE_SURFACE_WITH_KNOTS('',2,1,((#81435,#81436),(#81437,#81438),
(#81439,#81440)),.UNSPECIFIED.,.F.,.F.,.F.,(3,3),(2,2),(0.,1.),(0.,0.0149999999999997),
 .UNSPECIFIED.);
#56750=B_SPLINE_SURFACE_WITH_KNOTS('',2,1,((#81456,#81457),(#81458,#81459),
(#81460,#81461)),.UNSPECIFIED.,.F.,.F.,.F.,(3,3),(2,2),(0.,1.),(0.,0.0149999999999997),
 .UNSPECIFIED.);
#56751=B_SPLINE_SURFACE_WITH_KNOTS('',2,1,((#81471,#81472),(#81473,#81474),
(#81475,#81476)),.UNSPECIFIED.,.F.,.F.,.F.,(3,3),(2,2),(0.,1.),(0.,0.0149999999999997),
 .UNSPECIFIED.);
#56752=B_SPLINE_SURFACE_WITH_KNOTS('',2,1,((#81503,#81504),(#81505,#81506),
(#81507,#81508)),.UNSPECIFIED.,.F.,.F.,.F.,(3,3),(2,2),(0.,1.),(0.,0.0149999999999997),
 .UNSPECIFIED.);
#56753=B_SPLINE_SURFACE_WITH_KNOTS('',2,1,((#81521,#81522),(#81523,#81524),
(#81525,#81526)),.UNSPECIFIED.,.F.,.F.,.F.,(3,3),(2,2),(0.,1.),(0.,0.0149999999999997),
 .UNSPECIFIED.);
#56754=B_SPLINE_SURFACE_WITH_KNOTS('',2,1,((#81536,#81537),(#81538,#81539),
(#81540,#81541)),.UNSPECIFIED.,.F.,.F.,.F.,(3,3),(2,2),(0.,1.),(0.,0.0149999999999997),
 .UNSPECIFIED.);
#56755=B_SPLINE_SURFACE_WITH_KNOTS('',2,1,((#81551,#81552),(#81553,#81554),
(#81555,#81556)),.UNSPECIFIED.,.F.,.F.,.F.,(3,3),(2,2),(0.,1.),(0.,0.0149999999999997),
 .UNSPECIFIED.);
#56756=B_SPLINE_SURFACE_WITH_KNOTS('',2,1,((#81566,#81567),(#81568,#81569),
(#81570,#81571)),.UNSPECIFIED.,.F.,.F.,.F.,(3,3),(2,2),(0.,1.),(0.,0.0149999999999997),
 .UNSPECIFIED.);
#56757=B_SPLINE_SURFACE_WITH_KNOTS('',2,1,((#81581,#81582),(#81583,#81584),
(#81585,#81586)),.UNSPECIFIED.,.F.,.F.,.F.,(3,3),(2,2),(0.,1.),(0.,0.0149999999999997),
 .UNSPECIFIED.);
#56758=B_SPLINE_SURFACE_WITH_KNOTS('',2,1,((#81596,#81597),(#81598,#81599),
(#81600,#81601)),.UNSPECIFIED.,.F.,.F.,.F.,(3,3),(2,2),(0.,1.),(0.,0.0149999999999997),
 .UNSPECIFIED.);
#56759=B_SPLINE_SURFACE_WITH_KNOTS('',2,1,((#81611,#81612),(#81613,#81614),
(#81615,#81616)),.UNSPECIFIED.,.F.,.F.,.F.,(3,3),(2,2),(0.,1.),(0.,0.0149999999999997),
 .UNSPECIFIED.);
#56760=B_SPLINE_SURFACE_WITH_KNOTS('',2,1,((#81623,#81624),(#81625,#81626),
(#81627,#81628)),.UNSPECIFIED.,.F.,.F.,.F.,(3,3),(2,2),(0.,1.),(0.,0.0149999999999997),
 .UNSPECIFIED.);
#56761=B_SPLINE_SURFACE_WITH_KNOTS('',2,1,((#81641,#81642),(#81643,#81644),
(#81645,#81646)),.UNSPECIFIED.,.F.,.F.,.F.,(3,3),(2,2),(0.,1.),(0.,0.0149999999999997),
 .UNSPECIFIED.);
#56762=B_SPLINE_SURFACE_WITH_KNOTS('',2,1,((#81656,#81657),(#81658,#81659),
(#81660,#81661)),.UNSPECIFIED.,.F.,.F.,.F.,(3,3),(2,2),(0.,1.),(0.,0.0149999999999997),
 .UNSPECIFIED.);
#56763=B_SPLINE_SURFACE_WITH_KNOTS('',2,1,((#81671,#81672),(#81673,#81674),
(#81675,#81676)),.UNSPECIFIED.,.F.,.F.,.F.,(3,3),(2,2),(0.,1.),(0.,0.0149999999999997),
 .UNSPECIFIED.);
#56764=B_SPLINE_SURFACE_WITH_KNOTS('',2,1,((#81686,#81687),(#81688,#81689),
(#81690,#81691)),.UNSPECIFIED.,.F.,.F.,.F.,(3,3),(2,2),(0.,1.),(0.,0.0149999999999997),
 .UNSPECIFIED.);
#56765=B_SPLINE_SURFACE_WITH_KNOTS('',2,1,((#81701,#81702),(#81703,#81704),
(#81705,#81706)),.UNSPECIFIED.,.F.,.F.,.F.,(3,3),(2,2),(0.,1.),(0.,0.0149999999999997),
 .UNSPECIFIED.);
#56766=B_SPLINE_SURFACE_WITH_KNOTS('',2,1,((#81716,#81717),(#81718,#81719),
(#81720,#81721)),.UNSPECIFIED.,.F.,.F.,.F.,(3,3),(2,2),(0.,1.),(0.,0.0149999999999997),
 .UNSPECIFIED.);
#56767=B_SPLINE_SURFACE_WITH_KNOTS('',2,1,((#81731,#81732),(#81733,#81734),
(#81735,#81736)),.UNSPECIFIED.,.F.,.F.,.F.,(3,3),(2,2),(0.,1.),(0.,0.0149999999999997),
 .UNSPECIFIED.);
#56768=B_SPLINE_SURFACE_WITH_KNOTS('',2,1,((#81746,#81747),(#81748,#81749),
(#81750,#81751)),.UNSPECIFIED.,.F.,.F.,.F.,(3,3),(2,2),(0.,1.),(0.,0.0149999999999997),
 .UNSPECIFIED.);
#56769=B_SPLINE_SURFACE_WITH_KNOTS('',2,1,((#81761,#81762),(#81763,#81764),
(#81765,#81766)),.UNSPECIFIED.,.F.,.F.,.F.,(3,3),(2,2),(0.,1.),(0.,0.0149999999999997),
 .UNSPECIFIED.);
#56770=B_SPLINE_SURFACE_WITH_KNOTS('',2,1,((#81776,#81777),(#81778,#81779),
(#81780,#81781)),.UNSPECIFIED.,.F.,.F.,.F.,(3,3),(2,2),(0.,1.),(0.,0.0149999999999997),
 .UNSPECIFIED.);
#56771=B_SPLINE_SURFACE_WITH_KNOTS('',2,1,((#81791,#81792),(#81793,#81794),
(#81795,#81796)),.UNSPECIFIED.,.F.,.F.,.F.,(3,3),(2,2),(0.,1.),(0.,0.0149999999999997),
 .UNSPECIFIED.);
#56772=B_SPLINE_SURFACE_WITH_KNOTS('',2,1,((#81805,#81806),(#81807,#81808),
(#81809,#81810)),.UNSPECIFIED.,.F.,.F.,.F.,(3,3),(2,2),(0.,1.),(0.,0.0149999999999997),
 .UNSPECIFIED.);
#56773=B_SPLINE_SURFACE_WITH_KNOTS('',2,1,((#81823,#81824),(#81825,#81826),
(#81827,#81828)),.UNSPECIFIED.,.F.,.F.,.F.,(3,3),(2,2),(0.,1.),(0.,0.0149999999999997),
 .UNSPECIFIED.);
#56774=B_SPLINE_SURFACE_WITH_KNOTS('',2,1,((#81838,#81839),(#81840,#81841),
(#81842,#81843)),.UNSPECIFIED.,.F.,.F.,.F.,(3,3),(2,2),(0.,1.),(0.,0.0149999999999997),
 .UNSPECIFIED.);
#56775=B_SPLINE_SURFACE_WITH_KNOTS('',2,1,((#81853,#81854),(#81855,#81856),
(#81857,#81858)),.UNSPECIFIED.,.F.,.F.,.F.,(3,3),(2,2),(0.,1.),(0.,0.0149999999999997),
 .UNSPECIFIED.);
#56776=B_SPLINE_SURFACE_WITH_KNOTS('',2,1,((#81868,#81869),(#81870,#81871),
(#81872,#81873)),.UNSPECIFIED.,.F.,.F.,.F.,(3,3),(2,2),(0.,1.),(0.,0.0149999999999997),
 .UNSPECIFIED.);
#56777=B_SPLINE_SURFACE_WITH_KNOTS('',2,1,((#81883,#81884),(#81885,#81886),
(#81887,#81888)),.UNSPECIFIED.,.F.,.F.,.F.,(3,3),(2,2),(0.,1.),(0.,0.0149999999999997),
 .UNSPECIFIED.);
#56778=B_SPLINE_SURFACE_WITH_KNOTS('',2,1,((#81898,#81899),(#81900,#81901),
(#81902,#81903)),.UNSPECIFIED.,.F.,.F.,.F.,(3,3),(2,2),(0.,1.),(0.,0.0149999999999997),
 .UNSPECIFIED.);
#56779=B_SPLINE_SURFACE_WITH_KNOTS('',2,1,((#81913,#81914),(#81915,#81916),
(#81917,#81918)),.UNSPECIFIED.,.F.,.F.,.F.,(3,3),(2,2),(0.,1.),(0.,0.0149999999999997),
 .UNSPECIFIED.);
#56780=B_SPLINE_SURFACE_WITH_KNOTS('',2,1,((#81925,#81926),(#81927,#81928),
(#81929,#81930)),.UNSPECIFIED.,.F.,.F.,.F.,(3,3),(2,2),(0.,1.),(0.,0.0149999999999997),
 .UNSPECIFIED.);
#56781=B_SPLINE_SURFACE_WITH_KNOTS('',2,1,((#81943,#81944),(#81945,#81946),
(#81947,#81948)),.UNSPECIFIED.,.F.,.F.,.F.,(3,3),(2,2),(0.,1.),(0.,0.0149999999999997),
 .UNSPECIFIED.);
#56782=B_SPLINE_SURFACE_WITH_KNOTS('',2,1,((#81958,#81959),(#81960,#81961),
(#81962,#81963)),.UNSPECIFIED.,.F.,.F.,.F.,(3,3),(2,2),(0.,1.),(0.,0.0149999999999997),
 .UNSPECIFIED.);
#56783=B_SPLINE_SURFACE_WITH_KNOTS('',2,1,((#81973,#81974),(#81975,#81976),
(#81977,#81978)),.UNSPECIFIED.,.F.,.F.,.F.,(3,3),(2,2),(0.,1.),(0.,0.0149999999999997),
 .UNSPECIFIED.);
#56784=B_SPLINE_SURFACE_WITH_KNOTS('',2,1,((#81988,#81989),(#81990,#81991),
(#81992,#81993)),.UNSPECIFIED.,.F.,.F.,.F.,(3,3),(2,2),(0.,1.),(0.,0.0149999999999997),
 .UNSPECIFIED.);
#56785=B_SPLINE_SURFACE_WITH_KNOTS('',2,1,((#82003,#82004),(#82005,#82006),
(#82007,#82008)),.UNSPECIFIED.,.F.,.F.,.F.,(3,3),(2,2),(0.,1.),(0.,0.0149999999999997),
 .UNSPECIFIED.);
#56786=B_SPLINE_SURFACE_WITH_KNOTS('',2,1,((#82018,#82019),(#82020,#82021),
(#82022,#82023)),.UNSPECIFIED.,.F.,.F.,.F.,(3,3),(2,2),(0.,1.),(0.,0.0149999999999997),
 .UNSPECIFIED.);
#56787=B_SPLINE_SURFACE_WITH_KNOTS('',2,1,((#82033,#82034),(#82035,#82036),
(#82037,#82038)),.UNSPECIFIED.,.F.,.F.,.F.,(3,3),(2,2),(0.,1.),(0.,0.0149999999999997),
 .UNSPECIFIED.);
#56788=B_SPLINE_SURFACE_WITH_KNOTS('',2,1,((#82048,#82049),(#82050,#82051),
(#82052,#82053)),.UNSPECIFIED.,.F.,.F.,.F.,(3,3),(2,2),(0.,1.),(0.,0.0149999999999997),
 .UNSPECIFIED.);
#56789=B_SPLINE_SURFACE_WITH_KNOTS('',2,1,((#82063,#82064),(#82065,#82066),
(#82067,#82068)),.UNSPECIFIED.,.F.,.F.,.F.,(3,3),(2,2),(0.,1.),(0.,0.0149999999999997),
 .UNSPECIFIED.);
#56790=B_SPLINE_SURFACE_WITH_KNOTS('',2,1,((#82078,#82079),(#82080,#82081),
(#82082,#82083)),.UNSPECIFIED.,.F.,.F.,.F.,(3,3),(2,2),(0.,1.),(0.,0.0149999999999997),
 .UNSPECIFIED.);
#56791=B_SPLINE_SURFACE_WITH_KNOTS('',2,1,((#82093,#82094),(#82095,#82096),
(#82097,#82098)),.UNSPECIFIED.,.F.,.F.,.F.,(3,3),(2,2),(0.,1.),(0.,0.0149999999999997),
 .UNSPECIFIED.);
#56792=B_SPLINE_SURFACE_WITH_KNOTS('',2,1,((#82115,#82116),(#82117,#82118),
(#82119,#82120)),.UNSPECIFIED.,.F.,.F.,.F.,(3,3),(2,2),(0.,1.),(0.,0.0149999999999997),
 .UNSPECIFIED.);
#56793=B_SPLINE_SURFACE_WITH_KNOTS('',2,1,((#82130,#82131),(#82132,#82133),
(#82134,#82135)),.UNSPECIFIED.,.F.,.F.,.F.,(3,3),(2,2),(0.,1.),(0.,0.0149999999999997),
 .UNSPECIFIED.);
#56794=B_SPLINE_SURFACE_WITH_KNOTS('',2,1,((#82151,#82152),(#82153,#82154),
(#82155,#82156)),.UNSPECIFIED.,.F.,.F.,.F.,(3,3),(2,2),(0.,1.),(0.,0.0149999999999997),
 .UNSPECIFIED.);
#56795=B_SPLINE_SURFACE_WITH_KNOTS('',2,1,((#82166,#82167),(#82168,#82169),
(#82170,#82171)),.UNSPECIFIED.,.F.,.F.,.F.,(3,3),(2,2),(0.,1.),(0.,0.0149999999999997),
 .UNSPECIFIED.);
#56796=B_SPLINE_SURFACE_WITH_KNOTS('',2,1,((#82198,#82199),(#82200,#82201),
(#82202,#82203)),.UNSPECIFIED.,.F.,.F.,.F.,(3,3),(2,2),(0.,1.),(0.,0.0149999999999997),
 .UNSPECIFIED.);
#56797=B_SPLINE_SURFACE_WITH_KNOTS('',2,1,((#82216,#82217),(#82218,#82219),
(#82220,#82221)),.UNSPECIFIED.,.F.,.F.,.F.,(3,3),(2,2),(0.,1.),(0.,0.0149999999999997),
 .UNSPECIFIED.);
#56798=B_SPLINE_SURFACE_WITH_KNOTS('',2,1,((#82231,#82232),(#82233,#82234),
(#82235,#82236)),.UNSPECIFIED.,.F.,.F.,.F.,(3,3),(2,2),(0.,1.),(0.,0.0149999999999997),
 .UNSPECIFIED.);
#56799=B_SPLINE_SURFACE_WITH_KNOTS('',2,1,((#82246,#82247),(#82248,#82249),
(#82250,#82251)),.UNSPECIFIED.,.F.,.F.,.F.,(3,3),(2,2),(0.,1.),(0.,0.0149999999999997),
 .UNSPECIFIED.);
#56800=B_SPLINE_SURFACE_WITH_KNOTS('',2,1,((#82261,#82262),(#82263,#82264),
(#82265,#82266)),.UNSPECIFIED.,.F.,.F.,.F.,(3,3),(2,2),(0.,1.),(0.,0.0149999999999997),
 .UNSPECIFIED.);
#56801=B_SPLINE_SURFACE_WITH_KNOTS('',2,1,((#82276,#82277),(#82278,#82279),
(#82280,#82281)),.UNSPECIFIED.,.F.,.F.,.F.,(3,3),(2,2),(0.,1.),(0.,0.0149999999999997),
 .UNSPECIFIED.);
#56802=B_SPLINE_SURFACE_WITH_KNOTS('',2,1,((#82291,#82292),(#82293,#82294),
(#82295,#82296)),.UNSPECIFIED.,.F.,.F.,.F.,(3,3),(2,2),(0.,1.),(0.,0.0149999999999997),
 .UNSPECIFIED.);
#56803=B_SPLINE_SURFACE_WITH_KNOTS('',2,1,((#82306,#82307),(#82308,#82309),
(#82310,#82311)),.UNSPECIFIED.,.F.,.F.,.F.,(3,3),(2,2),(0.,1.),(0.,0.0149999999999997),
 .UNSPECIFIED.);
#56804=B_SPLINE_SURFACE_WITH_KNOTS('',2,1,((#82318,#82319),(#82320,#82321),
(#82322,#82323)),.UNSPECIFIED.,.F.,.F.,.F.,(3,3),(2,2),(0.,1.),(0.,0.0149999999999997),
 .UNSPECIFIED.);
#56805=B_SPLINE_SURFACE_WITH_KNOTS('',2,1,((#82336,#82337),(#82338,#82339),
(#82340,#82341)),.UNSPECIFIED.,.F.,.F.,.F.,(3,3),(2,2),(0.,1.),(0.,0.0149999999999997),
 .UNSPECIFIED.);
#56806=B_SPLINE_SURFACE_WITH_KNOTS('',2,1,((#82351,#82352),(#82353,#82354),
(#82355,#82356)),.UNSPECIFIED.,.F.,.F.,.F.,(3,3),(2,2),(0.,1.),(0.,0.0149999999999997),
 .UNSPECIFIED.);
#56807=B_SPLINE_SURFACE_WITH_KNOTS('',2,1,((#82366,#82367),(#82368,#82369),
(#82370,#82371)),.UNSPECIFIED.,.F.,.F.,.F.,(3,3),(2,2),(0.,1.),(0.,0.0149999999999997),
 .UNSPECIFIED.);
#56808=B_SPLINE_SURFACE_WITH_KNOTS('',2,1,((#82381,#82382),(#82383,#82384),
(#82385,#82386)),.UNSPECIFIED.,.F.,.F.,.F.,(3,3),(2,2),(0.,1.),(0.,0.0149999999999997),
 .UNSPECIFIED.);
#56809=B_SPLINE_SURFACE_WITH_KNOTS('',2,1,((#82396,#82397),(#82398,#82399),
(#82400,#82401)),.UNSPECIFIED.,.F.,.F.,.F.,(3,3),(2,2),(0.,1.),(0.,0.0149999999999997),
 .UNSPECIFIED.);
#56810=B_SPLINE_SURFACE_WITH_KNOTS('',2,1,((#82411,#82412),(#82413,#82414),
(#82415,#82416)),.UNSPECIFIED.,.F.,.F.,.F.,(3,3),(2,2),(0.,1.),(0.,0.0149999999999997),
 .UNSPECIFIED.);
#56811=B_SPLINE_SURFACE_WITH_KNOTS('',2,1,((#82426,#82427),(#82428,#82429),
(#82430,#82431)),.UNSPECIFIED.,.F.,.F.,.F.,(3,3),(2,2),(0.,1.),(0.,0.0149999999999997),
 .UNSPECIFIED.);
#56812=B_SPLINE_SURFACE_WITH_KNOTS('',2,1,((#82441,#82442),(#82443,#82444),
(#82445,#82446)),.UNSPECIFIED.,.F.,.F.,.F.,(3,3),(2,2),(0.,1.),(0.,0.0149999999999997),
 .UNSPECIFIED.);
#56813=B_SPLINE_SURFACE_WITH_KNOTS('',2,1,((#82456,#82457),(#82458,#82459),
(#82460,#82461)),.UNSPECIFIED.,.F.,.F.,.F.,(3,3),(2,2),(0.,1.),(0.,0.0149999999999997),
 .UNSPECIFIED.);
#56814=B_SPLINE_SURFACE_WITH_KNOTS('',2,1,((#82471,#82472),(#82473,#82474),
(#82475,#82476)),.UNSPECIFIED.,.F.,.F.,.F.,(3,3),(2,2),(0.,1.),(0.,0.0149999999999997),
 .UNSPECIFIED.);
#56815=B_SPLINE_SURFACE_WITH_KNOTS('',2,1,((#82486,#82487),(#82488,#82489),
(#82490,#82491)),.UNSPECIFIED.,.F.,.F.,.F.,(3,3),(2,2),(0.,1.),(0.,0.0149999999999997),
 .UNSPECIFIED.);
#56816=B_SPLINE_SURFACE_WITH_KNOTS('',2,1,((#82499,#82500),(#82501,#82502),
(#82503,#82504)),.UNSPECIFIED.,.F.,.F.,.F.,(3,3),(2,2),(0.,1.),(0.,0.0149999999999997),
 .UNSPECIFIED.);
#56817=B_SPLINE_SURFACE_WITH_KNOTS('',2,1,((#82517,#82518),(#82519,#82520),
(#82521,#82522)),.UNSPECIFIED.,.F.,.F.,.F.,(3,3),(2,2),(0.,1.),(0.,0.0149999999999997),
 .UNSPECIFIED.);
#56818=B_SPLINE_SURFACE_WITH_KNOTS('',2,1,((#82532,#82533),(#82534,#82535),
(#82536,#82537)),.UNSPECIFIED.,.F.,.F.,.F.,(3,3),(2,2),(0.,1.),(0.,0.0149999999999997),
 .UNSPECIFIED.);
#56819=B_SPLINE_SURFACE_WITH_KNOTS('',2,1,((#82547,#82548),(#82549,#82550),
(#82551,#82552)),.UNSPECIFIED.,.F.,.F.,.F.,(3,3),(2,2),(0.,1.),(0.,0.0149999999999997),
 .UNSPECIFIED.);
#56820=B_SPLINE_SURFACE_WITH_KNOTS('',2,1,((#82562,#82563),(#82564,#82565),
(#82566,#82567)),.UNSPECIFIED.,.F.,.F.,.F.,(3,3),(2,2),(0.,1.),(0.,0.0149999999999997),
 .UNSPECIFIED.);
#56821=B_SPLINE_SURFACE_WITH_KNOTS('',2,1,((#82577,#82578),(#82579,#82580),
(#82581,#82582)),.UNSPECIFIED.,.F.,.F.,.F.,(3,3),(2,2),(0.,1.),(0.,0.0149999999999997),
 .UNSPECIFIED.);
#56822=B_SPLINE_SURFACE_WITH_KNOTS('',2,1,((#82592,#82593),(#82594,#82595),
(#82596,#82597)),.UNSPECIFIED.,.F.,.F.,.F.,(3,3),(2,2),(0.,1.),(0.,0.0149999999999997),
 .UNSPECIFIED.);
#56823=B_SPLINE_SURFACE_WITH_KNOTS('',2,1,((#82607,#82608),(#82609,#82610),
(#82611,#82612)),.UNSPECIFIED.,.F.,.F.,.F.,(3,3),(2,2),(0.,1.),(0.,0.0149999999999997),
 .UNSPECIFIED.);
#56824=B_SPLINE_SURFACE_WITH_KNOTS('',2,1,((#82622,#82623),(#82624,#82625),
(#82626,#82627)),.UNSPECIFIED.,.F.,.F.,.F.,(3,3),(2,2),(0.,1.),(0.,0.0149999999999997),
 .UNSPECIFIED.);
#56825=B_SPLINE_SURFACE_WITH_KNOTS('',2,1,((#82643,#82644),(#82645,#82646),
(#82647,#82648)),.UNSPECIFIED.,.F.,.F.,.F.,(3,3),(2,2),(0.,1.),(0.,0.0149999999999997),
 .UNSPECIFIED.);
#56826=B_SPLINE_SURFACE_WITH_KNOTS('',2,1,((#82658,#82659),(#82660,#82661),
(#82662,#82663)),.UNSPECIFIED.,.F.,.F.,.F.,(3,3),(2,2),(0.,1.),(0.,0.0149999999999997),
 .UNSPECIFIED.);
#56827=B_SPLINE_SURFACE_WITH_KNOTS('',2,1,((#82673,#82674),(#82675,#82676),
(#82677,#82678)),.UNSPECIFIED.,.F.,.F.,.F.,(3,3),(2,2),(0.,1.),(0.,0.0149999999999997),
 .UNSPECIFIED.);
#56828=B_SPLINE_SURFACE_WITH_KNOTS('',2,1,((#82688,#82689),(#82690,#82691),
(#82692,#82693)),.UNSPECIFIED.,.F.,.F.,.F.,(3,3),(2,2),(0.,1.),(0.,0.0149999999999997),
 .UNSPECIFIED.);
#56829=B_SPLINE_SURFACE_WITH_KNOTS('',2,1,((#82703,#82704),(#82705,#82706),
(#82707,#82708)),.UNSPECIFIED.,.F.,.F.,.F.,(3,3),(2,2),(0.,1.),(0.,0.0149999999999997),
 .UNSPECIFIED.);
#56830=B_SPLINE_SURFACE_WITH_KNOTS('',2,1,((#82718,#82719),(#82720,#82721),
(#82722,#82723)),.UNSPECIFIED.,.F.,.F.,.F.,(3,3),(2,2),(0.,1.),(0.,0.0149999999999997),
 .UNSPECIFIED.);
#56831=B_SPLINE_SURFACE_WITH_KNOTS('',2,1,((#82733,#82734),(#82735,#82736),
(#82737,#82738)),.UNSPECIFIED.,.F.,.F.,.F.,(3,3),(2,2),(0.,1.),(0.,0.0149999999999997),
 .UNSPECIFIED.);
#56832=B_SPLINE_SURFACE_WITH_KNOTS('',2,1,((#82748,#82749),(#82750,#82751),
(#82752,#82753)),.UNSPECIFIED.,.F.,.F.,.F.,(3,3),(2,2),(0.,1.),(0.,0.0149999999999997),
 .UNSPECIFIED.);
#56833=B_SPLINE_SURFACE_WITH_KNOTS('',2,1,((#82763,#82764),(#82765,#82766),
(#82767,#82768)),.UNSPECIFIED.,.F.,.F.,.F.,(3,3),(2,2),(0.,1.),(0.,0.0149999999999997),
 .UNSPECIFIED.);
#56834=B_SPLINE_SURFACE_WITH_KNOTS('',2,1,((#82795,#82796),(#82797,#82798),
(#82799,#82800)),.UNSPECIFIED.,.F.,.F.,.F.,(3,3),(2,2),(0.,1.),(0.,0.0149999999999997),
 .UNSPECIFIED.);
#56835=B_SPLINE_SURFACE_WITH_KNOTS('',2,1,((#82813,#82814),(#82815,#82816),
(#82817,#82818)),.UNSPECIFIED.,.F.,.F.,.F.,(3,3),(2,2),(0.,1.),(0.,0.0149999999999997),
 .UNSPECIFIED.);
#56836=B_SPLINE_SURFACE_WITH_KNOTS('',2,1,((#82828,#82829),(#82830,#82831),
(#82832,#82833)),.UNSPECIFIED.,.F.,.F.,.F.,(3,3),(2,2),(0.,1.),(0.,0.0149999999999997),
 .UNSPECIFIED.);
#56837=B_SPLINE_SURFACE_WITH_KNOTS('',2,1,((#82843,#82844),(#82845,#82846),
(#82847,#82848)),.UNSPECIFIED.,.F.,.F.,.F.,(3,3),(2,2),(0.,1.),(0.,0.0149999999999997),
 .UNSPECIFIED.);
#56838=B_SPLINE_SURFACE_WITH_KNOTS('',2,1,((#82858,#82859),(#82860,#82861),
(#82862,#82863)),.UNSPECIFIED.,.F.,.F.,.F.,(3,3),(2,2),(0.,1.),(0.,0.0149999999999997),
 .UNSPECIFIED.);
#56839=B_SPLINE_SURFACE_WITH_KNOTS('',2,1,((#82873,#82874),(#82875,#82876),
(#82877,#82878)),.UNSPECIFIED.,.F.,.F.,.F.,(3,3),(2,2),(0.,1.),(0.,0.0149999999999997),
 .UNSPECIFIED.);
#56840=B_SPLINE_SURFACE_WITH_KNOTS('',2,1,((#82888,#82889),(#82890,#82891),
(#82892,#82893)),.UNSPECIFIED.,.F.,.F.,.F.,(3,3),(2,2),(0.,1.),(0.,0.0149999999999997),
 .UNSPECIFIED.);
#56841=B_SPLINE_SURFACE_WITH_KNOTS('',2,1,((#82903,#82904),(#82905,#82906),
(#82907,#82908)),.UNSPECIFIED.,.F.,.F.,.F.,(3,3),(2,2),(0.,1.),(0.,0.0149999999999997),
 .UNSPECIFIED.);
#56842=B_SPLINE_SURFACE_WITH_KNOTS('',2,1,((#82915,#82916),(#82917,#82918),
(#82919,#82920)),.UNSPECIFIED.,.F.,.F.,.F.,(3,3),(2,2),(0.,1.),(0.,0.0149999999999997),
 .UNSPECIFIED.);
#56843=B_SPLINE_SURFACE_WITH_KNOTS('',2,1,((#82933,#82934),(#82935,#82936),
(#82937,#82938)),.UNSPECIFIED.,.F.,.F.,.F.,(3,3),(2,2),(0.,1.),(0.,0.0149999999999997),
 .UNSPECIFIED.);
#56844=B_SPLINE_SURFACE_WITH_KNOTS('',2,1,((#82948,#82949),(#82950,#82951),
(#82952,#82953)),.UNSPECIFIED.,.F.,.F.,.F.,(3,3),(2,2),(0.,1.),(0.,0.0149999999999997),
 .UNSPECIFIED.);
#56845=B_SPLINE_SURFACE_WITH_KNOTS('',2,1,((#82963,#82964),(#82965,#82966),
(#82967,#82968)),.UNSPECIFIED.,.F.,.F.,.F.,(3,3),(2,2),(0.,1.),(0.,0.0149999999999997),
 .UNSPECIFIED.);
#56846=B_SPLINE_SURFACE_WITH_KNOTS('',2,1,((#82978,#82979),(#82980,#82981),
(#82982,#82983)),.UNSPECIFIED.,.F.,.F.,.F.,(3,3),(2,2),(0.,1.),(0.,0.0149999999999997),
 .UNSPECIFIED.);
#56847=B_SPLINE_SURFACE_WITH_KNOTS('',2,1,((#82993,#82994),(#82995,#82996),
(#82997,#82998)),.UNSPECIFIED.,.F.,.F.,.F.,(3,3),(2,2),(0.,1.),(0.,0.0149999999999997),
 .UNSPECIFIED.);
#56848=B_SPLINE_SURFACE_WITH_KNOTS('',2,1,((#83008,#83009),(#83010,#83011),
(#83012,#83013)),.UNSPECIFIED.,.F.,.F.,.F.,(3,3),(2,2),(0.,1.),(0.,0.0149999999999997),
 .UNSPECIFIED.);
#56849=B_SPLINE_SURFACE_WITH_KNOTS('',2,1,((#83023,#83024),(#83025,#83026),
(#83027,#83028)),.UNSPECIFIED.,.F.,.F.,.F.,(3,3),(2,2),(0.,1.),(0.,0.0149999999999997),
 .UNSPECIFIED.);
#56850=B_SPLINE_SURFACE_WITH_KNOTS('',2,1,((#83038,#83039),(#83040,#83041),
(#83042,#83043)),.UNSPECIFIED.,.F.,.F.,.F.,(3,3),(2,2),(0.,1.),(0.,0.0149999999999997),
 .UNSPECIFIED.);
#56851=B_SPLINE_SURFACE_WITH_KNOTS('',2,1,((#83053,#83054),(#83055,#83056),
(#83057,#83058)),.UNSPECIFIED.,.F.,.F.,.F.,(3,3),(2,2),(0.,1.),(0.,0.0149999999999997),
 .UNSPECIFIED.);
#56852=B_SPLINE_SURFACE_WITH_KNOTS('',2,1,((#83068,#83069),(#83070,#83071),
(#83072,#83073)),.UNSPECIFIED.,.F.,.F.,.F.,(3,3),(2,2),(0.,1.),(0.,0.0149999999999997),
 .UNSPECIFIED.);
#56853=B_SPLINE_SURFACE_WITH_KNOTS('',2,1,((#83083,#83084),(#83085,#83086),
(#83087,#83088)),.UNSPECIFIED.,.F.,.F.,.F.,(3,3),(2,2),(0.,1.),(0.,0.0149999999999997),
 .UNSPECIFIED.);
#56854=B_SPLINE_SURFACE_WITH_KNOTS('',2,1,((#83096,#83097),(#83098,#83099),
(#83100,#83101)),.UNSPECIFIED.,.F.,.F.,.F.,(3,3),(2,2),(0.,1.),(0.,0.0149999999999997),
 .UNSPECIFIED.);
#56855=B_SPLINE_SURFACE_WITH_KNOTS('',2,1,((#83114,#83115),(#83116,#83117),
(#83118,#83119)),.UNSPECIFIED.,.F.,.F.,.F.,(3,3),(2,2),(0.,1.),(0.,0.0149999999999997),
 .UNSPECIFIED.);
#56856=B_SPLINE_SURFACE_WITH_KNOTS('',2,1,((#83129,#83130),(#83131,#83132),
(#83133,#83134)),.UNSPECIFIED.,.F.,.F.,.F.,(3,3),(2,2),(0.,1.),(0.,0.0149999999999997),
 .UNSPECIFIED.);
#56857=B_SPLINE_SURFACE_WITH_KNOTS('',2,1,((#83144,#83145),(#83146,#83147),
(#83148,#83149)),.UNSPECIFIED.,.F.,.F.,.F.,(3,3),(2,2),(0.,1.),(0.,0.0149999999999997),
 .UNSPECIFIED.);
#56858=B_SPLINE_SURFACE_WITH_KNOTS('',2,1,((#83159,#83160),(#83161,#83162),
(#83163,#83164)),.UNSPECIFIED.,.F.,.F.,.F.,(3,3),(2,2),(0.,1.),(0.,0.0149999999999997),
 .UNSPECIFIED.);
#56859=B_SPLINE_SURFACE_WITH_KNOTS('',2,1,((#83174,#83175),(#83176,#83177),
(#83178,#83179)),.UNSPECIFIED.,.F.,.F.,.F.,(3,3),(2,2),(0.,1.),(0.,0.0149999999999997),
 .UNSPECIFIED.);
#56860=B_SPLINE_SURFACE_WITH_KNOTS('',2,1,((#83189,#83190),(#83191,#83192),
(#83193,#83194)),.UNSPECIFIED.,.F.,.F.,.F.,(3,3),(2,2),(0.,1.),(0.,0.0149999999999997),
 .UNSPECIFIED.);
#56861=B_SPLINE_SURFACE_WITH_KNOTS('',2,1,((#83204,#83205),(#83206,#83207),
(#83208,#83209)),.UNSPECIFIED.,.F.,.F.,.F.,(3,3),(2,2),(0.,1.),(0.,0.0149999999999997),
 .UNSPECIFIED.);
#56862=B_SPLINE_SURFACE_WITH_KNOTS('',2,1,((#83219,#83220),(#83221,#83222),
(#83223,#83224)),.UNSPECIFIED.,.F.,.F.,.F.,(3,3),(2,2),(0.,1.),(0.,0.0149999999999997),
 .UNSPECIFIED.);
#56863=B_SPLINE_SURFACE_WITH_KNOTS('',2,1,((#83234,#83235),(#83236,#83237),
(#83238,#83239)),.UNSPECIFIED.,.F.,.F.,.F.,(3,3),(2,2),(0.,1.),(0.,0.0149999999999997),
 .UNSPECIFIED.);
#56864=B_SPLINE_SURFACE_WITH_KNOTS('',2,1,((#83249,#83250),(#83251,#83252),
(#83253,#83254)),.UNSPECIFIED.,.F.,.F.,.F.,(3,3),(2,2),(0.,1.),(0.,0.0149999999999997),
 .UNSPECIFIED.);
#56865=B_SPLINE_SURFACE_WITH_KNOTS('',2,1,((#83264,#83265),(#83266,#83267),
(#83268,#83269)),.UNSPECIFIED.,.F.,.F.,.F.,(3,3),(2,2),(0.,1.),(0.,0.0149999999999997),
 .UNSPECIFIED.);
#56866=B_SPLINE_SURFACE_WITH_KNOTS('',2,1,((#83285,#83286),(#83287,#83288),
(#83289,#83290)),.UNSPECIFIED.,.F.,.F.,.F.,(3,3),(2,2),(0.,1.),(0.,0.0149999999999997),
 .UNSPECIFIED.);
#56867=B_SPLINE_SURFACE_WITH_KNOTS('',2,1,((#83300,#83301),(#83302,#83303),
(#83304,#83305)),.UNSPECIFIED.,.F.,.F.,.F.,(3,3),(2,2),(0.,1.),(0.,0.0149999999999997),
 .UNSPECIFIED.);
#56868=B_SPLINE_SURFACE_WITH_KNOTS('',2,1,((#83315,#83316),(#83317,#83318),
(#83319,#83320)),.UNSPECIFIED.,.F.,.F.,.F.,(3,3),(2,2),(0.,1.),(0.,0.0149999999999997),
 .UNSPECIFIED.);
#56869=B_SPLINE_SURFACE_WITH_KNOTS('',2,1,((#83330,#83331),(#83332,#83333),
(#83334,#83335)),.UNSPECIFIED.,.F.,.F.,.F.,(3,3),(2,2),(0.,1.),(0.,0.0149999999999997),
 .UNSPECIFIED.);
#56870=B_SPLINE_SURFACE_WITH_KNOTS('',2,1,((#83345,#83346),(#83347,#83348),
(#83349,#83350)),.UNSPECIFIED.,.F.,.F.,.F.,(3,3),(2,2),(0.,1.),(0.,0.0149999999999997),
 .UNSPECIFIED.);
#56871=B_SPLINE_SURFACE_WITH_KNOTS('',2,1,((#83360,#83361),(#83362,#83363),
(#83364,#83365)),.UNSPECIFIED.,.F.,.F.,.F.,(3,3),(2,2),(0.,1.),(0.,0.0149999999999997),
 .UNSPECIFIED.);
#56872=B_SPLINE_SURFACE_WITH_KNOTS('',2,1,((#83375,#83376),(#83377,#83378),
(#83379,#83380)),.UNSPECIFIED.,.F.,.F.,.F.,(3,3),(2,2),(0.,1.),(0.,0.0149999999999997),
 .UNSPECIFIED.);
#56873=B_SPLINE_SURFACE_WITH_KNOTS('',2,1,((#83396,#83397),(#83398,#83399),
(#83400,#83401)),.UNSPECIFIED.,.F.,.F.,.F.,(3,3),(2,2),(0.,1.),(0.,0.0149999999999997),
 .UNSPECIFIED.);
#56874=B_SPLINE_SURFACE_WITH_KNOTS('',2,1,((#83411,#83412),(#83413,#83414),
(#83415,#83416)),.UNSPECIFIED.,.F.,.F.,.F.,(3,3),(2,2),(0.,1.),(0.,0.0149999999999997),
 .UNSPECIFIED.);
#56875=B_SPLINE_SURFACE_WITH_KNOTS('',2,1,((#83426,#83427),(#83428,#83429),
(#83430,#83431)),.UNSPECIFIED.,.F.,.F.,.F.,(3,3),(2,2),(0.,1.),(0.,0.0149999999999997),
 .UNSPECIFIED.);
#56876=B_SPLINE_SURFACE_WITH_KNOTS('',2,1,((#83441,#83442),(#83443,#83444),
(#83445,#83446)),.UNSPECIFIED.,.F.,.F.,.F.,(3,3),(2,2),(0.,1.),(0.,0.0149999999999997),
 .UNSPECIFIED.);
#56877=B_SPLINE_SURFACE_WITH_KNOTS('',2,1,((#83456,#83457),(#83458,#83459),
(#83460,#83461)),.UNSPECIFIED.,.F.,.F.,.F.,(3,3),(2,2),(0.,1.),(0.,0.0149999999999997),
 .UNSPECIFIED.);
#56878=B_SPLINE_SURFACE_WITH_KNOTS('',2,1,((#83471,#83472),(#83473,#83474),
(#83475,#83476)),.UNSPECIFIED.,.F.,.F.,.F.,(3,3),(2,2),(0.,1.),(0.,0.0149999999999997),
 .UNSPECIFIED.);
#56879=B_SPLINE_SURFACE_WITH_KNOTS('',2,1,((#83486,#83487),(#83488,#83489),
(#83490,#83491)),.UNSPECIFIED.,.F.,.F.,.F.,(3,3),(2,2),(0.,1.),(0.,0.0149999999999997),
 .UNSPECIFIED.);
#56880=B_SPLINE_SURFACE_WITH_KNOTS('',2,1,((#83507,#83508),(#83509,#83510),
(#83511,#83512)),.UNSPECIFIED.,.F.,.F.,.F.,(3,3),(2,2),(0.,1.),(0.,0.0149999999999997),
 .UNSPECIFIED.);
#56881=B_SPLINE_SURFACE_WITH_KNOTS('',2,1,((#83521,#83522),(#83523,#83524),
(#83525,#83526)),.UNSPECIFIED.,.F.,.F.,.F.,(3,3),(2,2),(0.,1.),(0.,0.0149999999999997),
 .UNSPECIFIED.);
#56882=B_SPLINE_SURFACE_WITH_KNOTS('',2,1,((#83539,#83540),(#83541,#83542),
(#83543,#83544)),.UNSPECIFIED.,.F.,.F.,.F.,(3,3),(2,2),(0.,1.),(0.,0.0149999999999997),
 .UNSPECIFIED.);
#56883=B_SPLINE_SURFACE_WITH_KNOTS('',2,1,((#83554,#83555),(#83556,#83557),
(#83558,#83559)),.UNSPECIFIED.,.F.,.F.,.F.,(3,3),(2,2),(0.,1.),(0.,0.0149999999999997),
 .UNSPECIFIED.);
#56884=B_SPLINE_SURFACE_WITH_KNOTS('',2,1,((#83569,#83570),(#83571,#83572),
(#83573,#83574)),.UNSPECIFIED.,.F.,.F.,.F.,(3,3),(2,2),(0.,1.),(0.,0.0149999999999997),
 .UNSPECIFIED.);
#56885=B_SPLINE_SURFACE_WITH_KNOTS('',2,1,((#83584,#83585),(#83586,#83587),
(#83588,#83589)),.UNSPECIFIED.,.F.,.F.,.F.,(3,3),(2,2),(0.,1.),(0.,0.0149999999999997),
 .UNSPECIFIED.);
#56886=B_SPLINE_SURFACE_WITH_KNOTS('',2,1,((#83599,#83600),(#83601,#83602),
(#83603,#83604)),.UNSPECIFIED.,.F.,.F.,.F.,(3,3),(2,2),(0.,1.),(0.,0.0149999999999997),
 .UNSPECIFIED.);
#56887=B_SPLINE_SURFACE_WITH_KNOTS('',2,1,((#83614,#83615),(#83616,#83617),
(#83618,#83619)),.UNSPECIFIED.,.F.,.F.,.F.,(3,3),(2,2),(0.,1.),(0.,0.0149999999999997),
 .UNSPECIFIED.);
#56888=B_SPLINE_SURFACE_WITH_KNOTS('',2,1,((#83629,#83630),(#83631,#83632),
(#83633,#83634)),.UNSPECIFIED.,.F.,.F.,.F.,(3,3),(2,2),(0.,1.),(0.,0.0149999999999997),
 .UNSPECIFIED.);
#56889=B_SPLINE_SURFACE_WITH_KNOTS('',2,1,((#83641,#83642),(#83643,#83644),
(#83645,#83646)),.UNSPECIFIED.,.F.,.F.,.F.,(3,3),(2,2),(0.,1.),(0.,0.0149999999999997),
 .UNSPECIFIED.);
#56890=B_SPLINE_SURFACE_WITH_KNOTS('',2,1,((#83659,#83660),(#83661,#83662),
(#83663,#83664)),.UNSPECIFIED.,.F.,.F.,.F.,(3,3),(2,2),(0.,1.),(0.,0.0149999999999997),
 .UNSPECIFIED.);
#56891=B_SPLINE_SURFACE_WITH_KNOTS('',2,1,((#83674,#83675),(#83676,#83677),
(#83678,#83679)),.UNSPECIFIED.,.F.,.F.,.F.,(3,3),(2,2),(0.,1.),(0.,0.0149999999999997),
 .UNSPECIFIED.);
#56892=B_SPLINE_SURFACE_WITH_KNOTS('',2,1,((#83689,#83690),(#83691,#83692),
(#83693,#83694)),.UNSPECIFIED.,.F.,.F.,.F.,(3,3),(2,2),(0.,1.),(0.,0.0149999999999997),
 .UNSPECIFIED.);
#56893=B_SPLINE_SURFACE_WITH_KNOTS('',2,1,((#83704,#83705),(#83706,#83707),
(#83708,#83709)),.UNSPECIFIED.,.F.,.F.,.F.,(3,3),(2,2),(0.,1.),(0.,0.0149999999999997),
 .UNSPECIFIED.);
#56894=B_SPLINE_SURFACE_WITH_KNOTS('',2,1,((#83719,#83720),(#83721,#83722),
(#83723,#83724)),.UNSPECIFIED.,.F.,.F.,.F.,(3,3),(2,2),(0.,1.),(0.,0.0149999999999997),
 .UNSPECIFIED.);
#56895=B_SPLINE_SURFACE_WITH_KNOTS('',2,1,((#83734,#83735),(#83736,#83737),
(#83738,#83739)),.UNSPECIFIED.,.F.,.F.,.F.,(3,3),(2,2),(0.,1.),(0.,0.0149999999999997),
 .UNSPECIFIED.);
#56896=B_SPLINE_SURFACE_WITH_KNOTS('',2,1,((#83749,#83750),(#83751,#83752),
(#83753,#83754)),.UNSPECIFIED.,.F.,.F.,.F.,(3,3),(2,2),(0.,1.),(0.,0.0149999999999997),
 .UNSPECIFIED.);
#56897=B_SPLINE_SURFACE_WITH_KNOTS('',2,1,((#83764,#83765),(#83766,#83767),
(#83768,#83769)),.UNSPECIFIED.,.F.,.F.,.F.,(3,3),(2,2),(0.,1.),(0.,0.0149999999999997),
 .UNSPECIFIED.);
#56898=B_SPLINE_SURFACE_WITH_KNOTS('',2,1,((#83779,#83780),(#83781,#83782),
(#83783,#83784)),.UNSPECIFIED.,.F.,.F.,.F.,(3,3),(2,2),(0.,1.),(0.,0.0149999999999997),
 .UNSPECIFIED.);
#56899=B_SPLINE_SURFACE_WITH_KNOTS('',2,1,((#83794,#83795),(#83796,#83797),
(#83798,#83799)),.UNSPECIFIED.,.F.,.F.,.F.,(3,3),(2,2),(0.,1.),(0.,0.0149999999999997),
 .UNSPECIFIED.);
#56900=B_SPLINE_SURFACE_WITH_KNOTS('',2,1,((#83809,#83810),(#83811,#83812),
(#83813,#83814)),.UNSPECIFIED.,.F.,.F.,.F.,(3,3),(2,2),(0.,1.),(0.,0.0149999999999997),
 .UNSPECIFIED.);
#56901=B_SPLINE_SURFACE_WITH_KNOTS('',2,1,((#83909,#83910),(#83911,#83912),
(#83913,#83914)),.UNSPECIFIED.,.F.,.F.,.F.,(3,3),(2,2),(0.,1.),(0.,0.0149999999999997),
 .UNSPECIFIED.);
#56902=B_SPLINE_SURFACE_WITH_KNOTS('',2,1,((#83927,#83928),(#83929,#83930),
(#83931,#83932)),.UNSPECIFIED.,.F.,.F.,.F.,(3,3),(2,2),(0.,1.),(0.,0.0149999999999997),
 .UNSPECIFIED.);
#56903=B_SPLINE_SURFACE_WITH_KNOTS('',2,1,((#83942,#83943),(#83944,#83945),
(#83946,#83947)),.UNSPECIFIED.,.F.,.F.,.F.,(3,3),(2,2),(0.,1.),(0.,0.0149999999999997),
 .UNSPECIFIED.);
#56904=B_SPLINE_SURFACE_WITH_KNOTS('',2,1,((#83957,#83958),(#83959,#83960),
(#83961,#83962)),.UNSPECIFIED.,.F.,.F.,.F.,(3,3),(2,2),(0.,1.),(0.,0.0149999999999997),
 .UNSPECIFIED.);
#56905=B_SPLINE_SURFACE_WITH_KNOTS('',2,1,((#83972,#83973),(#83974,#83975),
(#83976,#83977)),.UNSPECIFIED.,.F.,.F.,.F.,(3,3),(2,2),(0.,1.),(0.,0.0149999999999997),
 .UNSPECIFIED.);
#56906=B_SPLINE_SURFACE_WITH_KNOTS('',2,1,((#83987,#83988),(#83989,#83990),
(#83991,#83992)),.UNSPECIFIED.,.F.,.F.,.F.,(3,3),(2,2),(0.,1.),(0.,0.0149999999999997),
 .UNSPECIFIED.);
#56907=B_SPLINE_SURFACE_WITH_KNOTS('',2,1,((#84002,#84003),(#84004,#84005),
(#84006,#84007)),.UNSPECIFIED.,.F.,.F.,.F.,(3,3),(2,2),(0.,1.),(0.,0.0149999999999997),
 .UNSPECIFIED.);
#56908=B_SPLINE_SURFACE_WITH_KNOTS('',2,1,((#84017,#84018),(#84019,#84020),
(#84021,#84022)),.UNSPECIFIED.,.F.,.F.,.F.,(3,3),(2,2),(0.,1.),(0.,0.0149999999999997),
 .UNSPECIFIED.);
#56909=B_SPLINE_SURFACE_WITH_KNOTS('',2,1,((#84029,#84030),(#84031,#84032),
(#84033,#84034)),.UNSPECIFIED.,.F.,.F.,.F.,(3,3),(2,2),(0.,1.),(0.,0.0149999999999997),
 .UNSPECIFIED.);
#56910=B_SPLINE_SURFACE_WITH_KNOTS('',2,1,((#84047,#84048),(#84049,#84050),
(#84051,#84052)),.UNSPECIFIED.,.F.,.F.,.F.,(3,3),(2,2),(0.,1.),(0.,0.0149999999999997),
 .UNSPECIFIED.);
#56911=B_SPLINE_SURFACE_WITH_KNOTS('',2,1,((#84062,#84063),(#84064,#84065),
(#84066,#84067)),.UNSPECIFIED.,.F.,.F.,.F.,(3,3),(2,2),(0.,1.),(0.,0.0149999999999997),
 .UNSPECIFIED.);
#56912=B_SPLINE_SURFACE_WITH_KNOTS('',2,1,((#84077,#84078),(#84079,#84080),
(#84081,#84082)),.UNSPECIFIED.,.F.,.F.,.F.,(3,3),(2,2),(0.,1.),(0.,0.0149999999999997),
 .UNSPECIFIED.);
#56913=B_SPLINE_SURFACE_WITH_KNOTS('',2,1,((#84092,#84093),(#84094,#84095),
(#84096,#84097)),.UNSPECIFIED.,.F.,.F.,.F.,(3,3),(2,2),(0.,1.),(0.,0.0149999999999997),
 .UNSPECIFIED.);
#56914=B_SPLINE_SURFACE_WITH_KNOTS('',2,1,((#84107,#84108),(#84109,#84110),
(#84111,#84112)),.UNSPECIFIED.,.F.,.F.,.F.,(3,3),(2,2),(0.,1.),(0.,0.0149999999999997),
 .UNSPECIFIED.);
#56915=B_SPLINE_SURFACE_WITH_KNOTS('',2,1,((#84122,#84123),(#84124,#84125),
(#84126,#84127)),.UNSPECIFIED.,.F.,.F.,.F.,(3,3),(2,2),(0.,1.),(0.,0.0149999999999997),
 .UNSPECIFIED.);
#56916=B_SPLINE_SURFACE_WITH_KNOTS('',2,1,((#84137,#84138),(#84139,#84140),
(#84141,#84142)),.UNSPECIFIED.,.F.,.F.,.F.,(3,3),(2,2),(0.,1.),(0.,0.0149999999999997),
 .UNSPECIFIED.);
#56917=B_SPLINE_SURFACE_WITH_KNOTS('',2,1,((#84152,#84153),(#84154,#84155),
(#84156,#84157)),.UNSPECIFIED.,.F.,.F.,.F.,(3,3),(2,2),(0.,1.),(0.,0.0149999999999997),
 .UNSPECIFIED.);
#56918=B_SPLINE_SURFACE_WITH_KNOTS('',2,1,((#84167,#84168),(#84169,#84170),
(#84171,#84172)),.UNSPECIFIED.,.F.,.F.,.F.,(3,3),(2,2),(0.,1.),(0.,0.0149999999999997),
 .UNSPECIFIED.);
#56919=B_SPLINE_SURFACE_WITH_KNOTS('',2,1,((#84182,#84183),(#84184,#84185),
(#84186,#84187)),.UNSPECIFIED.,.F.,.F.,.F.,(3,3),(2,2),(0.,1.),(0.,0.0149999999999997),
 .UNSPECIFIED.);
#56920=B_SPLINE_SURFACE_WITH_KNOTS('',2,1,((#84197,#84198),(#84199,#84200),
(#84201,#84202)),.UNSPECIFIED.,.F.,.F.,.F.,(3,3),(2,2),(0.,1.),(0.,0.0149999999999997),
 .UNSPECIFIED.);
#56921=B_SPLINE_SURFACE_WITH_KNOTS('',2,1,((#84210,#84211),(#84212,#84213),
(#84214,#84215)),.UNSPECIFIED.,.F.,.F.,.F.,(3,3),(2,2),(0.,1.),(0.,0.0149999999999997),
 .UNSPECIFIED.);
#56922=B_SPLINE_SURFACE_WITH_KNOTS('',2,1,((#84228,#84229),(#84230,#84231),
(#84232,#84233)),.UNSPECIFIED.,.F.,.F.,.F.,(3,3),(2,2),(0.,1.),(0.,0.0149999999999997),
 .UNSPECIFIED.);
#56923=B_SPLINE_SURFACE_WITH_KNOTS('',2,1,((#84243,#84244),(#84245,#84246),
(#84247,#84248)),.UNSPECIFIED.,.F.,.F.,.F.,(3,3),(2,2),(0.,1.),(0.,0.0149999999999997),
 .UNSPECIFIED.);
#56924=B_SPLINE_SURFACE_WITH_KNOTS('',2,1,((#84258,#84259),(#84260,#84261),
(#84262,#84263)),.UNSPECIFIED.,.F.,.F.,.F.,(3,3),(2,2),(0.,1.),(0.,0.0149999999999997),
 .UNSPECIFIED.);
#56925=B_SPLINE_SURFACE_WITH_KNOTS('',2,1,((#84273,#84274),(#84275,#84276),
(#84277,#84278)),.UNSPECIFIED.,.F.,.F.,.F.,(3,3),(2,2),(0.,1.),(0.,0.0149999999999997),
 .UNSPECIFIED.);
#56926=B_SPLINE_SURFACE_WITH_KNOTS('',2,1,((#84288,#84289),(#84290,#84291),
(#84292,#84293)),.UNSPECIFIED.,.F.,.F.,.F.,(3,3),(2,2),(0.,1.),(0.,0.0149999999999997),
 .UNSPECIFIED.);
#56927=B_SPLINE_SURFACE_WITH_KNOTS('',2,1,((#84339,#84340),(#84341,#84342),
(#84343,#84344)),.UNSPECIFIED.,.F.,.F.,.F.,(3,3),(2,2),(0.,1.),(0.,0.0149999999999997),
 .UNSPECIFIED.);
#56928=B_SPLINE_SURFACE_WITH_KNOTS('',2,1,((#84354,#84355),(#84356,#84357),
(#84358,#84359)),.UNSPECIFIED.,.F.,.F.,.F.,(3,3),(2,2),(0.,1.),(0.,0.0149999999999997),
 .UNSPECIFIED.);
#56929=B_SPLINE_SURFACE_WITH_KNOTS('',2,1,((#84369,#84370),(#84371,#84372),
(#84373,#84374)),.UNSPECIFIED.,.F.,.F.,.F.,(3,3),(2,2),(0.,1.),(0.,0.0149999999999997),
 .UNSPECIFIED.);
#56930=B_SPLINE_SURFACE_WITH_KNOTS('',2,1,((#84384,#84385),(#84386,#84387),
(#84388,#84389)),.UNSPECIFIED.,.F.,.F.,.F.,(3,3),(2,2),(0.,1.),(0.,0.0149999999999997),
 .UNSPECIFIED.);
#56931=B_SPLINE_SURFACE_WITH_KNOTS('',2,1,((#84399,#84400),(#84401,#84402),
(#84403,#84404)),.UNSPECIFIED.,.F.,.F.,.F.,(3,3),(2,2),(0.,1.),(0.,0.0149999999999997),
 .UNSPECIFIED.);
#56932=B_SPLINE_SURFACE_WITH_KNOTS('',2,1,((#84414,#84415),(#84416,#84417),
(#84418,#84419)),.UNSPECIFIED.,.F.,.F.,.F.,(3,3),(2,2),(0.,1.),(0.,0.0149999999999997),
 .UNSPECIFIED.);
#56933=B_SPLINE_SURFACE_WITH_KNOTS('',2,1,((#84429,#84430),(#84431,#84432),
(#84433,#84434)),.UNSPECIFIED.,.F.,.F.,.F.,(3,3),(2,2),(0.,1.),(0.,0.0149999999999997),
 .UNSPECIFIED.);
#56934=B_SPLINE_SURFACE_WITH_KNOTS('',2,1,((#84444,#84445),(#84446,#84447),
(#84448,#84449)),.UNSPECIFIED.,.F.,.F.,.F.,(3,3),(2,2),(0.,1.),(0.,0.0149999999999997),
 .UNSPECIFIED.);
#56935=B_SPLINE_SURFACE_WITH_KNOTS('',2,1,((#84465,#84466),(#84467,#84468),
(#84469,#84470)),.UNSPECIFIED.,.F.,.F.,.F.,(3,3),(2,2),(0.,1.),(0.,0.0149999999999997),
 .UNSPECIFIED.);
#56936=B_SPLINE_SURFACE_WITH_KNOTS('',2,1,((#84479,#84480),(#84481,#84482),
(#84483,#84484)),.UNSPECIFIED.,.F.,.F.,.F.,(3,3),(2,2),(0.,1.),(0.,0.0149999999999997),
 .UNSPECIFIED.);
#56937=B_SPLINE_SURFACE_WITH_KNOTS('',2,1,((#84497,#84498),(#84499,#84500),
(#84501,#84502)),.UNSPECIFIED.,.F.,.F.,.F.,(3,3),(2,2),(0.,1.),(0.,0.0149999999999997),
 .UNSPECIFIED.);
#56938=B_SPLINE_SURFACE_WITH_KNOTS('',2,1,((#84512,#84513),(#84514,#84515),
(#84516,#84517)),.UNSPECIFIED.,.F.,.F.,.F.,(3,3),(2,2),(0.,1.),(0.,0.0149999999999997),
 .UNSPECIFIED.);
#56939=B_SPLINE_SURFACE_WITH_KNOTS('',2,1,((#84527,#84528),(#84529,#84530),
(#84531,#84532)),.UNSPECIFIED.,.F.,.F.,.F.,(3,3),(2,2),(0.,1.),(0.,0.0149999999999997),
 .UNSPECIFIED.);
#56940=B_SPLINE_SURFACE_WITH_KNOTS('',2,1,((#84542,#84543),(#84544,#84545),
(#84546,#84547)),.UNSPECIFIED.,.F.,.F.,.F.,(3,3),(2,2),(0.,1.),(0.,0.0149999999999997),
 .UNSPECIFIED.);
#56941=B_SPLINE_SURFACE_WITH_KNOTS('',2,1,((#84557,#84558),(#84559,#84560),
(#84561,#84562)),.UNSPECIFIED.,.F.,.F.,.F.,(3,3),(2,2),(0.,1.),(0.,0.0149999999999997),
 .UNSPECIFIED.);
#56942=B_SPLINE_SURFACE_WITH_KNOTS('',2,1,((#84572,#84573),(#84574,#84575),
(#84576,#84577)),.UNSPECIFIED.,.F.,.F.,.F.,(3,3),(2,2),(0.,1.),(0.,0.0149999999999997),
 .UNSPECIFIED.);
#56943=B_SPLINE_SURFACE_WITH_KNOTS('',2,1,((#84587,#84588),(#84589,#84590),
(#84591,#84592)),.UNSPECIFIED.,.F.,.F.,.F.,(3,3),(2,2),(0.,1.),(0.,0.0149999999999997),
 .UNSPECIFIED.);
#56944=B_SPLINE_SURFACE_WITH_KNOTS('',2,1,((#84599,#84600),(#84601,#84602),
(#84603,#84604)),.UNSPECIFIED.,.F.,.F.,.F.,(3,3),(2,2),(0.,1.),(0.,0.0149999999999997),
 .UNSPECIFIED.);
#56945=B_SPLINE_SURFACE_WITH_KNOTS('',2,1,((#84617,#84618),(#84619,#84620),
(#84621,#84622)),.UNSPECIFIED.,.F.,.F.,.F.,(3,3),(2,2),(0.,1.),(0.,0.0149999999999997),
 .UNSPECIFIED.);
#56946=B_SPLINE_SURFACE_WITH_KNOTS('',2,1,((#84632,#84633),(#84634,#84635),
(#84636,#84637)),.UNSPECIFIED.,.F.,.F.,.F.,(3,3),(2,2),(0.,1.),(0.,0.0149999999999997),
 .UNSPECIFIED.);
#56947=B_SPLINE_SURFACE_WITH_KNOTS('',2,1,((#84647,#84648),(#84649,#84650),
(#84651,#84652)),.UNSPECIFIED.,.F.,.F.,.F.,(3,3),(2,2),(0.,1.),(0.,0.0149999999999997),
 .UNSPECIFIED.);
#56948=B_SPLINE_SURFACE_WITH_KNOTS('',2,1,((#84662,#84663),(#84664,#84665),
(#84666,#84667)),.UNSPECIFIED.,.F.,.F.,.F.,(3,3),(2,2),(0.,1.),(0.,0.0149999999999997),
 .UNSPECIFIED.);
#56949=B_SPLINE_SURFACE_WITH_KNOTS('',2,1,((#84677,#84678),(#84679,#84680),
(#84681,#84682)),.UNSPECIFIED.,.F.,.F.,.F.,(3,3),(2,2),(0.,1.),(0.,0.0149999999999997),
 .UNSPECIFIED.);
#56950=B_SPLINE_SURFACE_WITH_KNOTS('',2,1,((#84692,#84693),(#84694,#84695),
(#84696,#84697)),.UNSPECIFIED.,.F.,.F.,.F.,(3,3),(2,2),(0.,1.),(0.,0.0149999999999997),
 .UNSPECIFIED.);
#56951=B_SPLINE_SURFACE_WITH_KNOTS('',2,1,((#84707,#84708),(#84709,#84710),
(#84711,#84712)),.UNSPECIFIED.,.F.,.F.,.F.,(3,3),(2,2),(0.,1.),(0.,0.0149999999999997),
 .UNSPECIFIED.);
#56952=B_SPLINE_SURFACE_WITH_KNOTS('',2,1,((#84722,#84723),(#84724,#84725),
(#84726,#84727)),.UNSPECIFIED.,.F.,.F.,.F.,(3,3),(2,2),(0.,1.),(0.,0.0149999999999997),
 .UNSPECIFIED.);
#56953=B_SPLINE_SURFACE_WITH_KNOTS('',2,1,((#84737,#84738),(#84739,#84740),
(#84741,#84742)),.UNSPECIFIED.,.F.,.F.,.F.,(3,3),(2,2),(0.,1.),(0.,0.0149999999999997),
 .UNSPECIFIED.);
#56954=B_SPLINE_SURFACE_WITH_KNOTS('',2,1,((#84752,#84753),(#84754,#84755),
(#84756,#84757)),.UNSPECIFIED.,.F.,.F.,.F.,(3,3),(2,2),(0.,1.),(0.,0.0149999999999997),
 .UNSPECIFIED.);
#56955=B_SPLINE_SURFACE_WITH_KNOTS('',2,1,((#84767,#84768),(#84769,#84770),
(#84771,#84772)),.UNSPECIFIED.,.F.,.F.,.F.,(3,3),(2,2),(0.,1.),(0.,0.0149999999999997),
 .UNSPECIFIED.);
#56956=B_SPLINE_SURFACE_WITH_KNOTS('',2,1,((#84780,#84781),(#84782,#84783),
(#84784,#84785)),.UNSPECIFIED.,.F.,.F.,.F.,(3,3),(2,2),(0.,1.),(0.,0.0149999999999997),
 .UNSPECIFIED.);
#56957=B_SPLINE_SURFACE_WITH_KNOTS('',2,1,((#84798,#84799),(#84800,#84801),
(#84802,#84803)),.UNSPECIFIED.,.F.,.F.,.F.,(3,3),(2,2),(0.,1.),(0.,0.0149999999999997),
 .UNSPECIFIED.);
#56958=B_SPLINE_SURFACE_WITH_KNOTS('',2,1,((#84813,#84814),(#84815,#84816),
(#84817,#84818)),.UNSPECIFIED.,.F.,.F.,.F.,(3,3),(2,2),(0.,1.),(0.,0.0149999999999997),
 .UNSPECIFIED.);
#56959=B_SPLINE_SURFACE_WITH_KNOTS('',2,1,((#84828,#84829),(#84830,#84831),
(#84832,#84833)),.UNSPECIFIED.,.F.,.F.,.F.,(3,3),(2,2),(0.,1.),(0.,0.0149999999999997),
 .UNSPECIFIED.);
#56960=B_SPLINE_SURFACE_WITH_KNOTS('',2,1,((#84843,#84844),(#84845,#84846),
(#84847,#84848)),.UNSPECIFIED.,.F.,.F.,.F.,(3,3),(2,2),(0.,1.),(0.,0.0149999999999997),
 .UNSPECIFIED.);
#56961=B_SPLINE_SURFACE_WITH_KNOTS('',2,1,((#84858,#84859),(#84860,#84861),
(#84862,#84863)),.UNSPECIFIED.,.F.,.F.,.F.,(3,3),(2,2),(0.,1.),(0.,0.0149999999999997),
 .UNSPECIFIED.);
#56962=B_SPLINE_SURFACE_WITH_KNOTS('',2,1,((#84873,#84874),(#84875,#84876),
(#84877,#84878)),.UNSPECIFIED.,.F.,.F.,.F.,(3,3),(2,2),(0.,1.),(0.,0.0149999999999997),
 .UNSPECIFIED.);
#56963=B_SPLINE_SURFACE_WITH_KNOTS('',2,1,((#84888,#84889),(#84890,#84891),
(#84892,#84893)),.UNSPECIFIED.,.F.,.F.,.F.,(3,3),(2,2),(0.,1.),(0.,0.0149999999999997),
 .UNSPECIFIED.);
#56964=B_SPLINE_SURFACE_WITH_KNOTS('',2,1,((#84903,#84904),(#84905,#84906),
(#84907,#84908)),.UNSPECIFIED.,.F.,.F.,.F.,(3,3),(2,2),(0.,1.),(0.,0.0149999999999997),
 .UNSPECIFIED.);
#56965=B_SPLINE_SURFACE_WITH_KNOTS('',2,1,((#84915,#84916),(#84917,#84918),
(#84919,#84920)),.UNSPECIFIED.,.F.,.F.,.F.,(3,3),(2,2),(0.,1.),(0.,0.0149999999999997),
 .UNSPECIFIED.);
#56966=B_SPLINE_SURFACE_WITH_KNOTS('',2,1,((#84933,#84934),(#84935,#84936),
(#84937,#84938)),.UNSPECIFIED.,.F.,.F.,.F.,(3,3),(2,2),(0.,1.),(0.,0.0149999999999997),
 .UNSPECIFIED.);
#56967=B_SPLINE_SURFACE_WITH_KNOTS('',2,1,((#84948,#84949),(#84950,#84951),
(#84952,#84953)),.UNSPECIFIED.,.F.,.F.,.F.,(3,3),(2,2),(0.,1.),(0.,0.0149999999999997),
 .UNSPECIFIED.);
#56968=B_SPLINE_SURFACE_WITH_KNOTS('',2,1,((#84963,#84964),(#84965,#84966),
(#84967,#84968)),.UNSPECIFIED.,.F.,.F.,.F.,(3,3),(2,2),(0.,1.),(0.,0.0149999999999997),
 .UNSPECIFIED.);
#56969=B_SPLINE_SURFACE_WITH_KNOTS('',2,1,((#84978,#84979),(#84980,#84981),
(#84982,#84983)),.UNSPECIFIED.,.F.,.F.,.F.,(3,3),(2,2),(0.,1.),(0.,0.0149999999999997),
 .UNSPECIFIED.);
#56970=B_SPLINE_SURFACE_WITH_KNOTS('',2,1,((#84993,#84994),(#84995,#84996),
(#84997,#84998)),.UNSPECIFIED.,.F.,.F.,.F.,(3,3),(2,2),(0.,1.),(0.,0.0149999999999997),
 .UNSPECIFIED.);
#56971=B_SPLINE_SURFACE_WITH_KNOTS('',2,1,((#85008,#85009),(#85010,#85011),
(#85012,#85013)),.UNSPECIFIED.,.F.,.F.,.F.,(3,3),(2,2),(0.,1.),(0.,0.0149999999999997),
 .UNSPECIFIED.);
#56972=B_SPLINE_SURFACE_WITH_KNOTS('',2,1,((#85023,#85024),(#85025,#85026),
(#85027,#85028)),.UNSPECIFIED.,.F.,.F.,.F.,(3,3),(2,2),(0.,1.),(0.,0.0149999999999997),
 .UNSPECIFIED.);
#56973=B_SPLINE_SURFACE_WITH_KNOTS('',2,1,((#85038,#85039),(#85040,#85041),
(#85042,#85043)),.UNSPECIFIED.,.F.,.F.,.F.,(3,3),(2,2),(0.,1.),(0.,0.0149999999999997),
 .UNSPECIFIED.);
#56974=B_SPLINE_SURFACE_WITH_KNOTS('',2,1,((#85053,#85054),(#85055,#85056),
(#85057,#85058)),.UNSPECIFIED.,.F.,.F.,.F.,(3,3),(2,2),(0.,1.),(0.,0.0149999999999997),
 .UNSPECIFIED.);
#56975=B_SPLINE_SURFACE_WITH_KNOTS('',2,1,((#85068,#85069),(#85070,#85071),
(#85072,#85073)),.UNSPECIFIED.,.F.,.F.,.F.,(3,3),(2,2),(0.,1.),(0.,0.0149999999999997),
 .UNSPECIFIED.);
#56976=B_SPLINE_SURFACE_WITH_KNOTS('',2,1,((#85083,#85084),(#85085,#85086),
(#85087,#85088)),.UNSPECIFIED.,.F.,.F.,.F.,(3,3),(2,2),(0.,1.),(0.,0.0149999999999997),
 .UNSPECIFIED.);
#56977=B_SPLINE_SURFACE_WITH_KNOTS('',2,1,((#85098,#85099),(#85100,#85101),
(#85102,#85103)),.UNSPECIFIED.,.F.,.F.,.F.,(3,3),(2,2),(0.,1.),(0.,0.0149999999999997),
 .UNSPECIFIED.);
#56978=B_SPLINE_SURFACE_WITH_KNOTS('',2,1,((#85113,#85114),(#85115,#85116),
(#85117,#85118)),.UNSPECIFIED.,.F.,.F.,.F.,(3,3),(2,2),(0.,1.),(0.,0.0149999999999997),
 .UNSPECIFIED.);
#56979=B_SPLINE_SURFACE_WITH_KNOTS('',2,1,((#85128,#85129),(#85130,#85131),
(#85132,#85133)),.UNSPECIFIED.,.F.,.F.,.F.,(3,3),(2,2),(0.,1.),(0.,0.0149999999999997),
 .UNSPECIFIED.);
#56980=B_SPLINE_SURFACE_WITH_KNOTS('',2,1,((#85143,#85144),(#85145,#85146),
(#85147,#85148)),.UNSPECIFIED.,.F.,.F.,.F.,(3,3),(2,2),(0.,1.),(0.,0.0149999999999997),
 .UNSPECIFIED.);
#56981=B_SPLINE_SURFACE_WITH_KNOTS('',2,1,((#85158,#85159),(#85160,#85161),
(#85162,#85163)),.UNSPECIFIED.,.F.,.F.,.F.,(3,3),(2,2),(0.,1.),(0.,0.0149999999999997),
 .UNSPECIFIED.);
#56982=B_SPLINE_SURFACE_WITH_KNOTS('',2,1,((#85179,#85180),(#85181,#85182),
(#85183,#85184)),.UNSPECIFIED.,.F.,.F.,.F.,(3,3),(2,2),(0.,1.),(0.,0.0149999999999997),
 .UNSPECIFIED.);
#56983=B_SPLINE_SURFACE_WITH_KNOTS('',2,1,((#85194,#85195),(#85196,#85197),
(#85198,#85199)),.UNSPECIFIED.,.F.,.F.,.F.,(3,3),(2,2),(0.,1.),(0.,0.0149999999999997),
 .UNSPECIFIED.);
#56984=B_SPLINE_SURFACE_WITH_KNOTS('',2,1,((#85212,#85213),(#85214,#85215),
(#85216,#85217)),.UNSPECIFIED.,.F.,.F.,.F.,(3,3),(2,2),(0.,1.),(0.,0.0149999999999997),
 .UNSPECIFIED.);
#56985=B_SPLINE_SURFACE_WITH_KNOTS('',2,1,((#85227,#85228),(#85229,#85230),
(#85231,#85232)),.UNSPECIFIED.,.F.,.F.,.F.,(3,3),(2,2),(0.,1.),(0.,0.0149999999999997),
 .UNSPECIFIED.);
#56986=B_SPLINE_SURFACE_WITH_KNOTS('',2,1,((#85242,#85243),(#85244,#85245),
(#85246,#85247)),.UNSPECIFIED.,.F.,.F.,.F.,(3,3),(2,2),(0.,1.),(0.,0.0149999999999997),
 .UNSPECIFIED.);
#56987=B_SPLINE_SURFACE_WITH_KNOTS('',2,1,((#85257,#85258),(#85259,#85260),
(#85261,#85262)),.UNSPECIFIED.,.F.,.F.,.F.,(3,3),(2,2),(0.,1.),(0.,0.0149999999999997),
 .UNSPECIFIED.);
#56988=B_SPLINE_SURFACE_WITH_KNOTS('',2,1,((#85272,#85273),(#85274,#85275),
(#85276,#85277)),.UNSPECIFIED.,.F.,.F.,.F.,(3,3),(2,2),(0.,1.),(0.,0.0149999999999997),
 .UNSPECIFIED.);
#56989=B_SPLINE_SURFACE_WITH_KNOTS('',2,1,((#85287,#85288),(#85289,#85290),
(#85291,#85292)),.UNSPECIFIED.,.F.,.F.,.F.,(3,3),(2,2),(0.,1.),(0.,0.0149999999999997),
 .UNSPECIFIED.);
#56990=B_SPLINE_SURFACE_WITH_KNOTS('',2,1,((#85302,#85303),(#85304,#85305),
(#85306,#85307)),.UNSPECIFIED.,.F.,.F.,.F.,(3,3),(2,2),(0.,1.),(0.,0.0149999999999997),
 .UNSPECIFIED.);
#56991=B_SPLINE_SURFACE_WITH_KNOTS('',2,1,((#85314,#85315),(#85316,#85317),
(#85318,#85319)),.UNSPECIFIED.,.F.,.F.,.F.,(3,3),(2,2),(0.,1.),(0.,0.0149999999999997),
 .UNSPECIFIED.);
#56992=B_SPLINE_SURFACE_WITH_KNOTS('',2,1,((#85332,#85333),(#85334,#85335),
(#85336,#85337)),.UNSPECIFIED.,.F.,.F.,.F.,(3,3),(2,2),(0.,1.),(0.,0.0149999999999997),
 .UNSPECIFIED.);
#56993=B_SPLINE_SURFACE_WITH_KNOTS('',2,1,((#85347,#85348),(#85349,#85350),
(#85351,#85352)),.UNSPECIFIED.,.F.,.F.,.F.,(3,3),(2,2),(0.,1.),(0.,0.0149999999999997),
 .UNSPECIFIED.);
#56994=B_SPLINE_SURFACE_WITH_KNOTS('',2,1,((#85362,#85363),(#85364,#85365),
(#85366,#85367)),.UNSPECIFIED.,.F.,.F.,.F.,(3,3),(2,2),(0.,1.),(0.,0.0149999999999997),
 .UNSPECIFIED.);
#56995=B_SPLINE_SURFACE_WITH_KNOTS('',2,1,((#85377,#85378),(#85379,#85380),
(#85381,#85382)),.UNSPECIFIED.,.F.,.F.,.F.,(3,3),(2,2),(0.,1.),(0.,0.0149999999999997),
 .UNSPECIFIED.);
#56996=B_SPLINE_SURFACE_WITH_KNOTS('',2,1,((#85392,#85393),(#85394,#85395),
(#85396,#85397)),.UNSPECIFIED.,.F.,.F.,.F.,(3,3),(2,2),(0.,1.),(0.,0.0149999999999997),
 .UNSPECIFIED.);
#56997=B_SPLINE_SURFACE_WITH_KNOTS('',2,1,((#85407,#85408),(#85409,#85410),
(#85411,#85412)),.UNSPECIFIED.,.F.,.F.,.F.,(3,3),(2,2),(0.,1.),(0.,0.0149999999999997),
 .UNSPECIFIED.);
#56998=B_SPLINE_SURFACE_WITH_KNOTS('',2,1,((#85422,#85423),(#85424,#85425),
(#85426,#85427)),.UNSPECIFIED.,.F.,.F.,.F.,(3,3),(2,2),(0.,1.),(0.,0.0149999999999997),
 .UNSPECIFIED.);
#56999=B_SPLINE_SURFACE_WITH_KNOTS('',2,1,((#85437,#85438),(#85439,#85440),
(#85441,#85442)),.UNSPECIFIED.,.F.,.F.,.F.,(3,3),(2,2),(0.,1.),(0.,0.0149999999999997),
 .UNSPECIFIED.);
#57000=B_SPLINE_SURFACE_WITH_KNOTS('',2,1,((#85452,#85453),(#85454,#85455),
(#85456,#85457)),.UNSPECIFIED.,.F.,.F.,.F.,(3,3),(2,2),(0.,1.),(0.,0.0149999999999997),
 .UNSPECIFIED.);
#57001=B_SPLINE_SURFACE_WITH_KNOTS('',2,1,((#85467,#85468),(#85469,#85470),
(#85471,#85472)),.UNSPECIFIED.,.F.,.F.,.F.,(3,3),(2,2),(0.,1.),(0.,0.0149999999999997),
 .UNSPECIFIED.);
#57002=B_SPLINE_SURFACE_WITH_KNOTS('',2,1,((#85482,#85483),(#85484,#85485),
(#85486,#85487)),.UNSPECIFIED.,.F.,.F.,.F.,(3,3),(2,2),(0.,1.),(0.,0.0149999999999997),
 .UNSPECIFIED.);
#57003=B_SPLINE_SURFACE_WITH_KNOTS('',2,1,((#85495,#85496),(#85497,#85498),
(#85499,#85500)),.UNSPECIFIED.,.F.,.F.,.F.,(3,3),(2,2),(0.,1.),(0.,0.0149999999999997),
 .UNSPECIFIED.);
#57004=B_SPLINE_SURFACE_WITH_KNOTS('',2,1,((#85513,#85514),(#85515,#85516),
(#85517,#85518)),.UNSPECIFIED.,.F.,.F.,.F.,(3,3),(2,2),(0.,1.),(0.,0.0149999999999997),
 .UNSPECIFIED.);
#57005=B_SPLINE_SURFACE_WITH_KNOTS('',2,1,((#85528,#85529),(#85530,#85531),
(#85532,#85533)),.UNSPECIFIED.,.F.,.F.,.F.,(3,3),(2,2),(0.,1.),(0.,0.0149999999999997),
 .UNSPECIFIED.);
#57006=B_SPLINE_SURFACE_WITH_KNOTS('',2,1,((#85549,#85550),(#85551,#85552),
(#85553,#85554)),.UNSPECIFIED.,.F.,.F.,.F.,(3,3),(2,2),(0.,1.),(0.,0.0149999999999997),
 .UNSPECIFIED.);
#57007=B_SPLINE_SURFACE_WITH_KNOTS('',2,1,((#85564,#85565),(#85566,#85567),
(#85568,#85569)),.UNSPECIFIED.,.F.,.F.,.F.,(3,3),(2,2),(0.,1.),(0.,0.0149999999999997),
 .UNSPECIFIED.);
#57008=B_SPLINE_SURFACE_WITH_KNOTS('',2,1,((#85579,#85580),(#85581,#85582),
(#85583,#85584)),.UNSPECIFIED.,.F.,.F.,.F.,(3,3),(2,2),(0.,1.),(0.,0.0149999999999997),
 .UNSPECIFIED.);
#57009=B_SPLINE_SURFACE_WITH_KNOTS('',2,1,((#85617,#85618),(#85619,#85620),
(#85621,#85622)),.UNSPECIFIED.,.F.,.F.,.F.,(3,3),(2,2),(0.,1.),(0.,0.0149999999999997),
 .UNSPECIFIED.);
#57010=B_SPLINE_SURFACE_WITH_KNOTS('',2,1,((#85635,#85636),(#85637,#85638),
(#85639,#85640)),.UNSPECIFIED.,.F.,.F.,.F.,(3,3),(2,2),(0.,1.),(0.,0.0149999999999997),
 .UNSPECIFIED.);
#57011=B_SPLINE_SURFACE_WITH_KNOTS('',2,1,((#85650,#85651),(#85652,#85653),
(#85654,#85655)),.UNSPECIFIED.,.F.,.F.,.F.,(3,3),(2,2),(0.,1.),(0.,0.0149999999999997),
 .UNSPECIFIED.);
#57012=B_SPLINE_SURFACE_WITH_KNOTS('',2,1,((#85665,#85666),(#85667,#85668),
(#85669,#85670)),.UNSPECIFIED.,.F.,.F.,.F.,(3,3),(2,2),(0.,1.),(0.,0.0149999999999997),
 .UNSPECIFIED.);
#57013=B_SPLINE_SURFACE_WITH_KNOTS('',2,1,((#85680,#85681),(#85682,#85683),
(#85684,#85685)),.UNSPECIFIED.,.F.,.F.,.F.,(3,3),(2,2),(0.,1.),(0.,0.0149999999999997),
 .UNSPECIFIED.);
#57014=B_SPLINE_SURFACE_WITH_KNOTS('',2,1,((#85695,#85696),(#85697,#85698),
(#85699,#85700)),.UNSPECIFIED.,.F.,.F.,.F.,(3,3),(2,2),(0.,1.),(0.,0.0149999999999997),
 .UNSPECIFIED.);
#57015=B_SPLINE_SURFACE_WITH_KNOTS('',2,1,((#85710,#85711),(#85712,#85713),
(#85714,#85715)),.UNSPECIFIED.,.F.,.F.,.F.,(3,3),(2,2),(0.,1.),(0.,0.0149999999999997),
 .UNSPECIFIED.);
#57016=B_SPLINE_SURFACE_WITH_KNOTS('',2,1,((#85725,#85726),(#85727,#85728),
(#85729,#85730)),.UNSPECIFIED.,.F.,.F.,.F.,(3,3),(2,2),(0.,1.),(0.,0.0149999999999997),
 .UNSPECIFIED.);
#57017=B_SPLINE_SURFACE_WITH_KNOTS('',2,1,((#85737,#85738),(#85739,#85740),
(#85741,#85742)),.UNSPECIFIED.,.F.,.F.,.F.,(3,3),(2,2),(0.,1.),(0.,0.0149999999999997),
 .UNSPECIFIED.);
#57018=B_SPLINE_SURFACE_WITH_KNOTS('',2,1,((#85755,#85756),(#85757,#85758),
(#85759,#85760)),.UNSPECIFIED.,.F.,.F.,.F.,(3,3),(2,2),(0.,1.),(0.,0.0149999999999997),
 .UNSPECIFIED.);
#57019=B_SPLINE_SURFACE_WITH_KNOTS('',2,1,((#85770,#85771),(#85772,#85773),
(#85774,#85775)),.UNSPECIFIED.,.F.,.F.,.F.,(3,3),(2,2),(0.,1.),(0.,0.0149999999999997),
 .UNSPECIFIED.);
#57020=B_SPLINE_SURFACE_WITH_KNOTS('',2,1,((#85785,#85786),(#85787,#85788),
(#85789,#85790)),.UNSPECIFIED.,.F.,.F.,.F.,(3,3),(2,2),(0.,1.),(0.,0.0149999999999997),
 .UNSPECIFIED.);
#57021=B_SPLINE_SURFACE_WITH_KNOTS('',2,1,((#85800,#85801),(#85802,#85803),
(#85804,#85805)),.UNSPECIFIED.,.F.,.F.,.F.,(3,3),(2,2),(0.,1.),(0.,0.0149999999999997),
 .UNSPECIFIED.);
#57022=B_SPLINE_SURFACE_WITH_KNOTS('',2,1,((#85815,#85816),(#85817,#85818),
(#85819,#85820)),.UNSPECIFIED.,.F.,.F.,.F.,(3,3),(2,2),(0.,1.),(0.,0.0149999999999997),
 .UNSPECIFIED.);
#57023=B_SPLINE_SURFACE_WITH_KNOTS('',2,1,((#85830,#85831),(#85832,#85833),
(#85834,#85835)),.UNSPECIFIED.,.F.,.F.,.F.,(3,3),(2,2),(0.,1.),(0.,0.0149999999999997),
 .UNSPECIFIED.);
#57024=B_SPLINE_SURFACE_WITH_KNOTS('',2,1,((#85845,#85846),(#85847,#85848),
(#85849,#85850)),.UNSPECIFIED.,.F.,.F.,.F.,(3,3),(2,2),(0.,1.),(0.,0.0149999999999997),
 .UNSPECIFIED.);
#57025=B_SPLINE_SURFACE_WITH_KNOTS('',2,1,((#85860,#85861),(#85862,#85863),
(#85864,#85865)),.UNSPECIFIED.,.F.,.F.,.F.,(3,3),(2,2),(0.,1.),(0.,0.0149999999999997),
 .UNSPECIFIED.);
#57026=B_SPLINE_SURFACE_WITH_KNOTS('',2,1,((#85875,#85876),(#85877,#85878),
(#85879,#85880)),.UNSPECIFIED.,.F.,.F.,.F.,(3,3),(2,2),(0.,1.),(0.,0.0149999999999997),
 .UNSPECIFIED.);
#57027=B_SPLINE_SURFACE_WITH_KNOTS('',2,1,((#85890,#85891),(#85892,#85893),
(#85894,#85895)),.UNSPECIFIED.,.F.,.F.,.F.,(3,3),(2,2),(0.,1.),(0.,0.0149999999999997),
 .UNSPECIFIED.);
#57028=B_SPLINE_SURFACE_WITH_KNOTS('',2,1,((#85905,#85906),(#85907,#85908),
(#85909,#85910)),.UNSPECIFIED.,.F.,.F.,.F.,(3,3),(2,2),(0.,1.),(0.,0.0149999999999997),
 .UNSPECIFIED.);
#57029=B_SPLINE_SURFACE_WITH_KNOTS('',2,1,((#85918,#85919),(#85920,#85921),
(#85922,#85923)),.UNSPECIFIED.,.F.,.F.,.F.,(3,3),(2,2),(0.,1.),(0.,0.0149999999999997),
 .UNSPECIFIED.);
#57030=B_SPLINE_SURFACE_WITH_KNOTS('',2,1,((#85936,#85937),(#85938,#85939),
(#85940,#85941)),.UNSPECIFIED.,.F.,.F.,.F.,(3,3),(2,2),(0.,1.),(0.,0.0149999999999997),
 .UNSPECIFIED.);
#57031=B_SPLINE_SURFACE_WITH_KNOTS('',2,1,((#85951,#85952),(#85953,#85954),
(#85955,#85956)),.UNSPECIFIED.,.F.,.F.,.F.,(3,3),(2,2),(0.,1.),(0.,0.0149999999999997),
 .UNSPECIFIED.);
#57032=B_SPLINE_SURFACE_WITH_KNOTS('',2,1,((#85966,#85967),(#85968,#85969),
(#85970,#85971)),.UNSPECIFIED.,.F.,.F.,.F.,(3,3),(2,2),(0.,1.),(0.,0.0149999999999997),
 .UNSPECIFIED.);
#57033=B_SPLINE_SURFACE_WITH_KNOTS('',2,1,((#85981,#85982),(#85983,#85984),
(#85985,#85986)),.UNSPECIFIED.,.F.,.F.,.F.,(3,3),(2,2),(0.,1.),(0.,0.0149999999999997),
 .UNSPECIFIED.);
#57034=B_SPLINE_SURFACE_WITH_KNOTS('',2,1,((#85996,#85997),(#85998,#85999),
(#86000,#86001)),.UNSPECIFIED.,.F.,.F.,.F.,(3,3),(2,2),(0.,1.),(0.,0.0149999999999997),
 .UNSPECIFIED.);
#57035=B_SPLINE_SURFACE_WITH_KNOTS('',2,1,((#86011,#86012),(#86013,#86014),
(#86015,#86016)),.UNSPECIFIED.,.F.,.F.,.F.,(3,3),(2,2),(0.,1.),(0.,0.0149999999999997),
 .UNSPECIFIED.);
#57036=B_SPLINE_SURFACE_WITH_KNOTS('',2,1,((#86026,#86027),(#86028,#86029),
(#86030,#86031)),.UNSPECIFIED.,.F.,.F.,.F.,(3,3),(2,2),(0.,1.),(0.,0.0149999999999997),
 .UNSPECIFIED.);
#57037=B_SPLINE_SURFACE_WITH_KNOTS('',2,1,((#86038,#86039),(#86040,#86041),
(#86042,#86043)),.UNSPECIFIED.,.F.,.F.,.F.,(3,3),(2,2),(0.,1.),(0.,0.0149999999999997),
 .UNSPECIFIED.);
#57038=B_SPLINE_SURFACE_WITH_KNOTS('',2,1,((#86056,#86057),(#86058,#86059),
(#86060,#86061)),.UNSPECIFIED.,.F.,.F.,.F.,(3,3),(2,2),(0.,1.),(0.,0.0149999999999997),
 .UNSPECIFIED.);
#57039=B_SPLINE_SURFACE_WITH_KNOTS('',2,1,((#86071,#86072),(#86073,#86074),
(#86075,#86076)),.UNSPECIFIED.,.F.,.F.,.F.,(3,3),(2,2),(0.,1.),(0.,0.0149999999999997),
 .UNSPECIFIED.);
#57040=B_SPLINE_SURFACE_WITH_KNOTS('',2,1,((#86086,#86087),(#86088,#86089),
(#86090,#86091)),.UNSPECIFIED.,.F.,.F.,.F.,(3,3),(2,2),(0.,1.),(0.,0.0149999999999997),
 .UNSPECIFIED.);
#57041=B_SPLINE_SURFACE_WITH_KNOTS('',2,1,((#86101,#86102),(#86103,#86104),
(#86105,#86106)),.UNSPECIFIED.,.F.,.F.,.F.,(3,3),(2,2),(0.,1.),(0.,0.0149999999999997),
 .UNSPECIFIED.);
#57042=B_SPLINE_SURFACE_WITH_KNOTS('',2,1,((#86116,#86117),(#86118,#86119),
(#86120,#86121)),.UNSPECIFIED.,.F.,.F.,.F.,(3,3),(2,2),(0.,1.),(0.,0.0149999999999997),
 .UNSPECIFIED.);
#57043=B_SPLINE_SURFACE_WITH_KNOTS('',2,1,((#86131,#86132),(#86133,#86134),
(#86135,#86136)),.UNSPECIFIED.,.F.,.F.,.F.,(3,3),(2,2),(0.,1.),(0.,0.0149999999999997),
 .UNSPECIFIED.);
#57044=B_SPLINE_SURFACE_WITH_KNOTS('',2,1,((#86146,#86147),(#86148,#86149),
(#86150,#86151)),.UNSPECIFIED.,.F.,.F.,.F.,(3,3),(2,2),(0.,1.),(0.,0.0149999999999997),
 .UNSPECIFIED.);
#57045=B_SPLINE_SURFACE_WITH_KNOTS('',2,1,((#86161,#86162),(#86163,#86164),
(#86165,#86166)),.UNSPECIFIED.,.F.,.F.,.F.,(3,3),(2,2),(0.,1.),(0.,0.0149999999999997),
 .UNSPECIFIED.);
#57046=B_SPLINE_SURFACE_WITH_KNOTS('',2,1,((#86173,#86174),(#86175,#86176),
(#86177,#86178)),.UNSPECIFIED.,.F.,.F.,.F.,(3,3),(2,2),(0.,1.),(0.,0.0149999999999997),
 .UNSPECIFIED.);
#57047=B_SPLINE_SURFACE_WITH_KNOTS('',2,1,((#86191,#86192),(#86193,#86194),
(#86195,#86196)),.UNSPECIFIED.,.F.,.F.,.F.,(3,3),(2,2),(0.,1.),(0.,0.0149999999999997),
 .UNSPECIFIED.);
#57048=B_SPLINE_SURFACE_WITH_KNOTS('',2,1,((#86206,#86207),(#86208,#86209),
(#86210,#86211)),.UNSPECIFIED.,.F.,.F.,.F.,(3,3),(2,2),(0.,1.),(0.,0.0149999999999997),
 .UNSPECIFIED.);
#57049=B_SPLINE_SURFACE_WITH_KNOTS('',2,1,((#86221,#86222),(#86223,#86224),
(#86225,#86226)),.UNSPECIFIED.,.F.,.F.,.F.,(3,3),(2,2),(0.,1.),(0.,0.0149999999999997),
 .UNSPECIFIED.);
#57050=B_SPLINE_SURFACE_WITH_KNOTS('',2,1,((#86236,#86237),(#86238,#86239),
(#86240,#86241)),.UNSPECIFIED.,.F.,.F.,.F.,(3,3),(2,2),(0.,1.),(0.,0.0149999999999997),
 .UNSPECIFIED.);
#57051=B_SPLINE_SURFACE_WITH_KNOTS('',2,1,((#86251,#86252),(#86253,#86254),
(#86255,#86256)),.UNSPECIFIED.,.F.,.F.,.F.,(3,3),(2,2),(0.,1.),(0.,0.0149999999999997),
 .UNSPECIFIED.);
#57052=B_SPLINE_SURFACE_WITH_KNOTS('',2,1,((#86266,#86267),(#86268,#86269),
(#86270,#86271)),.UNSPECIFIED.,.F.,.F.,.F.,(3,3),(2,2),(0.,1.),(0.,0.0149999999999997),
 .UNSPECIFIED.);
#57053=B_SPLINE_SURFACE_WITH_KNOTS('',2,1,((#86281,#86282),(#86283,#86284),
(#86285,#86286)),.UNSPECIFIED.,.F.,.F.,.F.,(3,3),(2,2),(0.,1.),(0.,0.0149999999999997),
 .UNSPECIFIED.);
#57054=B_SPLINE_SURFACE_WITH_KNOTS('',2,1,((#86296,#86297),(#86298,#86299),
(#86300,#86301)),.UNSPECIFIED.,.F.,.F.,.F.,(3,3),(2,2),(0.,1.),(0.,0.0149999999999997),
 .UNSPECIFIED.);
#57055=B_SPLINE_SURFACE_WITH_KNOTS('',2,1,((#86311,#86312),(#86313,#86314),
(#86315,#86316)),.UNSPECIFIED.,.F.,.F.,.F.,(3,3),(2,2),(0.,1.),(0.,0.0149999999999997),
 .UNSPECIFIED.);
#57056=B_SPLINE_SURFACE_WITH_KNOTS('',2,1,((#86326,#86327),(#86328,#86329),
(#86330,#86331)),.UNSPECIFIED.,.F.,.F.,.F.,(3,3),(2,2),(0.,1.),(0.,0.0149999999999997),
 .UNSPECIFIED.);
#57057=B_SPLINE_SURFACE_WITH_KNOTS('',2,1,((#86341,#86342),(#86343,#86344),
(#86345,#86346)),.UNSPECIFIED.,.F.,.F.,.F.,(3,3),(2,2),(0.,1.),(0.,0.0149999999999997),
 .UNSPECIFIED.);
#57058=B_SPLINE_SURFACE_WITH_KNOTS('',2,1,((#86356,#86357),(#86358,#86359),
(#86360,#86361)),.UNSPECIFIED.,.F.,.F.,.F.,(3,3),(2,2),(0.,1.),(0.,0.0149999999999997),
 .UNSPECIFIED.);
#57059=B_SPLINE_SURFACE_WITH_KNOTS('',2,1,((#86371,#86372),(#86373,#86374),
(#86375,#86376)),.UNSPECIFIED.,.F.,.F.,.F.,(3,3),(2,2),(0.,1.),(0.,0.0149999999999997),
 .UNSPECIFIED.);
#57060=B_SPLINE_SURFACE_WITH_KNOTS('',2,1,((#86386,#86387),(#86388,#86389),
(#86390,#86391)),.UNSPECIFIED.,.F.,.F.,.F.,(3,3),(2,2),(0.,1.),(0.,0.0149999999999997),
 .UNSPECIFIED.);
#57061=B_SPLINE_SURFACE_WITH_KNOTS('',2,1,((#86401,#86402),(#86403,#86404),
(#86405,#86406)),.UNSPECIFIED.,.F.,.F.,.F.,(3,3),(2,2),(0.,1.),(0.,0.0149999999999997),
 .UNSPECIFIED.);
#57062=B_SPLINE_SURFACE_WITH_KNOTS('',2,1,((#86417,#86418),(#86419,#86420),
(#86421,#86422)),.UNSPECIFIED.,.F.,.F.,.F.,(3,3),(2,2),(0.,1.),(0.,0.0149999999999997),
 .UNSPECIFIED.);
#57063=B_SPLINE_SURFACE_WITH_KNOTS('',2,1,((#86435,#86436),(#86437,#86438),
(#86439,#86440)),.UNSPECIFIED.,.F.,.F.,.F.,(3,3),(2,2),(0.,1.),(0.,0.0149999999999997),
 .UNSPECIFIED.);
#57064=B_SPLINE_SURFACE_WITH_KNOTS('',2,1,((#86450,#86451),(#86452,#86453),
(#86454,#86455)),.UNSPECIFIED.,.F.,.F.,.F.,(3,3),(2,2),(0.,1.),(0.,0.0149999999999997),
 .UNSPECIFIED.);
#57065=B_SPLINE_SURFACE_WITH_KNOTS('',2,1,((#86465,#86466),(#86467,#86468),
(#86469,#86470)),.UNSPECIFIED.,.F.,.F.,.F.,(3,3),(2,2),(0.,1.),(0.,0.0149999999999997),
 .UNSPECIFIED.);
#57066=B_SPLINE_SURFACE_WITH_KNOTS('',2,1,((#86480,#86481),(#86482,#86483),
(#86484,#86485)),.UNSPECIFIED.,.F.,.F.,.F.,(3,3),(2,2),(0.,1.),(0.,0.0149999999999997),
 .UNSPECIFIED.);
#57067=B_SPLINE_SURFACE_WITH_KNOTS('',2,1,((#86495,#86496),(#86497,#86498),
(#86499,#86500)),.UNSPECIFIED.,.F.,.F.,.F.,(3,3),(2,2),(0.,1.),(0.,0.0149999999999997),
 .UNSPECIFIED.);
#57068=B_SPLINE_SURFACE_WITH_KNOTS('',2,1,((#86510,#86511),(#86512,#86513),
(#86514,#86515)),.UNSPECIFIED.,.F.,.F.,.F.,(3,3),(2,2),(0.,1.),(0.,0.0149999999999997),
 .UNSPECIFIED.);
#57069=B_SPLINE_SURFACE_WITH_KNOTS('',2,1,((#86525,#86526),(#86527,#86528),
(#86529,#86530)),.UNSPECIFIED.,.F.,.F.,.F.,(3,3),(2,2),(0.,1.),(0.,0.0149999999999997),
 .UNSPECIFIED.);
#57070=B_SPLINE_SURFACE_WITH_KNOTS('',2,1,((#86537,#86538),(#86539,#86540),
(#86541,#86542)),.UNSPECIFIED.,.F.,.F.,.F.,(3,3),(2,2),(0.,1.),(0.,0.0149999999999997),
 .UNSPECIFIED.);
#57071=B_SPLINE_SURFACE_WITH_KNOTS('',2,1,((#86555,#86556),(#86557,#86558),
(#86559,#86560)),.UNSPECIFIED.,.F.,.F.,.F.,(3,3),(2,2),(0.,1.),(0.,0.0149999999999997),
 .UNSPECIFIED.);
#57072=B_SPLINE_SURFACE_WITH_KNOTS('',2,1,((#86570,#86571),(#86572,#86573),
(#86574,#86575)),.UNSPECIFIED.,.F.,.F.,.F.,(3,3),(2,2),(0.,1.),(0.,0.0149999999999997),
 .UNSPECIFIED.);
#57073=B_SPLINE_SURFACE_WITH_KNOTS('',2,1,((#86585,#86586),(#86587,#86588),
(#86589,#86590)),.UNSPECIFIED.,.F.,.F.,.F.,(3,3),(2,2),(0.,1.),(0.,0.0149999999999997),
 .UNSPECIFIED.);
#57074=B_SPLINE_SURFACE_WITH_KNOTS('',2,1,((#86600,#86601),(#86602,#86603),
(#86604,#86605)),.UNSPECIFIED.,.F.,.F.,.F.,(3,3),(2,2),(0.,1.),(0.,0.0149999999999997),
 .UNSPECIFIED.);
#57075=B_SPLINE_SURFACE_WITH_KNOTS('',2,1,((#86615,#86616),(#86617,#86618),
(#86619,#86620)),.UNSPECIFIED.,.F.,.F.,.F.,(3,3),(2,2),(0.,1.),(0.,0.0149999999999997),
 .UNSPECIFIED.);
#57076=B_SPLINE_SURFACE_WITH_KNOTS('',2,1,((#86630,#86631),(#86632,#86633),
(#86634,#86635)),.UNSPECIFIED.,.F.,.F.,.F.,(3,3),(2,2),(0.,1.),(0.,0.0149999999999997),
 .UNSPECIFIED.);
#57077=B_SPLINE_SURFACE_WITH_KNOTS('',2,1,((#86645,#86646),(#86647,#86648),
(#86649,#86650)),.UNSPECIFIED.,.F.,.F.,.F.,(3,3),(2,2),(0.,1.),(0.,0.0149999999999997),
 .UNSPECIFIED.);
#57078=B_SPLINE_SURFACE_WITH_KNOTS('',2,1,((#86660,#86661),(#86662,#86663),
(#86664,#86665)),.UNSPECIFIED.,.F.,.F.,.F.,(3,3),(2,2),(0.,1.),(0.,0.0149999999999997),
 .UNSPECIFIED.);
#57079=B_SPLINE_SURFACE_WITH_KNOTS('',2,1,((#86675,#86676),(#86677,#86678),
(#86679,#86680)),.UNSPECIFIED.,.F.,.F.,.F.,(3,3),(2,2),(0.,1.),(0.,0.0149999999999997),
 .UNSPECIFIED.);
#57080=B_SPLINE_SURFACE_WITH_KNOTS('',2,1,((#86690,#86691),(#86692,#86693),
(#86694,#86695)),.UNSPECIFIED.,.F.,.F.,.F.,(3,3),(2,2),(0.,1.),(0.,0.0149999999999997),
 .UNSPECIFIED.);
#57081=B_SPLINE_SURFACE_WITH_KNOTS('',2,1,((#86705,#86706),(#86707,#86708),
(#86709,#86710)),.UNSPECIFIED.,.F.,.F.,.F.,(3,3),(2,2),(0.,1.),(0.,0.0149999999999997),
 .UNSPECIFIED.);
#57082=B_SPLINE_SURFACE_WITH_KNOTS('',2,1,((#86718,#86719),(#86720,#86721),
(#86722,#86723)),.UNSPECIFIED.,.F.,.F.,.F.,(3,3),(2,2),(0.,1.),(0.,0.0149999999999997),
 .UNSPECIFIED.);
#57083=B_SPLINE_SURFACE_WITH_KNOTS('',2,1,((#86736,#86737),(#86738,#86739),
(#86740,#86741)),.UNSPECIFIED.,.F.,.F.,.F.,(3,3),(2,2),(0.,1.),(0.,0.0149999999999997),
 .UNSPECIFIED.);
#57084=B_SPLINE_SURFACE_WITH_KNOTS('',2,1,((#86751,#86752),(#86753,#86754),
(#86755,#86756)),.UNSPECIFIED.,.F.,.F.,.F.,(3,3),(2,2),(0.,1.),(0.,0.0149999999999997),
 .UNSPECIFIED.);
#57085=B_SPLINE_SURFACE_WITH_KNOTS('',2,1,((#86766,#86767),(#86768,#86769),
(#86770,#86771)),.UNSPECIFIED.,.F.,.F.,.F.,(3,3),(2,2),(0.,1.),(0.,0.0149999999999997),
 .UNSPECIFIED.);
#57086=B_SPLINE_SURFACE_WITH_KNOTS('',2,1,((#86781,#86782),(#86783,#86784),
(#86785,#86786)),.UNSPECIFIED.,.F.,.F.,.F.,(3,3),(2,2),(0.,1.),(0.,0.0149999999999997),
 .UNSPECIFIED.);
#57087=B_SPLINE_SURFACE_WITH_KNOTS('',2,1,((#86796,#86797),(#86798,#86799),
(#86800,#86801)),.UNSPECIFIED.,.F.,.F.,.F.,(3,3),(2,2),(0.,1.),(0.,0.0149999999999997),
 .UNSPECIFIED.);
#57088=B_SPLINE_SURFACE_WITH_KNOTS('',2,1,((#86811,#86812),(#86813,#86814),
(#86815,#86816)),.UNSPECIFIED.,.F.,.F.,.F.,(3,3),(2,2),(0.,1.),(0.,0.0149999999999997),
 .UNSPECIFIED.);
#57089=B_SPLINE_SURFACE_WITH_KNOTS('',2,1,((#86826,#86827),(#86828,#86829),
(#86830,#86831)),.UNSPECIFIED.,.F.,.F.,.F.,(3,3),(2,2),(0.,1.),(0.,0.0149999999999997),
 .UNSPECIFIED.);
#57090=B_SPLINE_SURFACE_WITH_KNOTS('',2,1,((#86838,#86839),(#86840,#86841),
(#86842,#86843)),.UNSPECIFIED.,.F.,.F.,.F.,(3,3),(2,2),(0.,1.),(0.,0.0149999999999997),
 .UNSPECIFIED.);
#57091=B_SPLINE_SURFACE_WITH_KNOTS('',2,1,((#86856,#86857),(#86858,#86859),
(#86860,#86861)),.UNSPECIFIED.,.F.,.F.,.F.,(3,3),(2,2),(0.,1.),(0.,0.0149999999999997),
 .UNSPECIFIED.);
#57092=B_SPLINE_SURFACE_WITH_KNOTS('',2,1,((#86871,#86872),(#86873,#86874),
(#86875,#86876)),.UNSPECIFIED.,.F.,.F.,.F.,(3,3),(2,2),(0.,1.),(0.,0.0149999999999997),
 .UNSPECIFIED.);
#57093=B_SPLINE_SURFACE_WITH_KNOTS('',2,1,((#86886,#86887),(#86888,#86889),
(#86890,#86891)),.UNSPECIFIED.,.F.,.F.,.F.,(3,3),(2,2),(0.,1.),(0.,0.0149999999999997),
 .UNSPECIFIED.);
#57094=B_SPLINE_SURFACE_WITH_KNOTS('',2,1,((#86901,#86902),(#86903,#86904),
(#86905,#86906)),.UNSPECIFIED.,.F.,.F.,.F.,(3,3),(2,2),(0.,1.),(0.,0.0149999999999997),
 .UNSPECIFIED.);
#57095=B_SPLINE_SURFACE_WITH_KNOTS('',2,1,((#86916,#86917),(#86918,#86919),
(#86920,#86921)),.UNSPECIFIED.,.F.,.F.,.F.,(3,3),(2,2),(0.,1.),(0.,0.0149999999999997),
 .UNSPECIFIED.);
#57096=B_SPLINE_SURFACE_WITH_KNOTS('',2,1,((#86931,#86932),(#86933,#86934),
(#86935,#86936)),.UNSPECIFIED.,.F.,.F.,.F.,(3,3),(2,2),(0.,1.),(0.,0.0149999999999997),
 .UNSPECIFIED.);
#57097=B_SPLINE_SURFACE_WITH_KNOTS('',2,1,((#86946,#86947),(#86948,#86949),
(#86950,#86951)),.UNSPECIFIED.,.F.,.F.,.F.,(3,3),(2,2),(0.,1.),(0.,0.0149999999999997),
 .UNSPECIFIED.);
#57098=B_SPLINE_SURFACE_WITH_KNOTS('',2,1,((#86961,#86962),(#86963,#86964),
(#86965,#86966)),.UNSPECIFIED.,.F.,.F.,.F.,(3,3),(2,2),(0.,1.),(0.,0.0149999999999997),
 .UNSPECIFIED.);
#57099=B_SPLINE_SURFACE_WITH_KNOTS('',2,1,((#86976,#86977),(#86978,#86979),
(#86980,#86981)),.UNSPECIFIED.,.F.,.F.,.F.,(3,3),(2,2),(0.,1.),(0.,0.0149999999999997),
 .UNSPECIFIED.);
#57100=B_SPLINE_SURFACE_WITH_KNOTS('',2,1,((#86991,#86992),(#86993,#86994),
(#86995,#86996)),.UNSPECIFIED.,.F.,.F.,.F.,(3,3),(2,2),(0.,1.),(0.,0.0149999999999997),
 .UNSPECIFIED.);
#57101=B_SPLINE_SURFACE_WITH_KNOTS('',2,1,((#87006,#87007),(#87008,#87009),
(#87010,#87011)),.UNSPECIFIED.,.F.,.F.,.F.,(3,3),(2,2),(0.,1.),(0.,0.0149999999999997),
 .UNSPECIFIED.);
#57102=B_SPLINE_SURFACE_WITH_KNOTS('',2,1,((#87021,#87022),(#87023,#87024),
(#87025,#87026)),.UNSPECIFIED.,.F.,.F.,.F.,(3,3),(2,2),(0.,1.),(0.,0.0149999999999997),
 .UNSPECIFIED.);
#57103=B_SPLINE_SURFACE_WITH_KNOTS('',2,1,((#87036,#87037),(#87038,#87039),
(#87040,#87041)),.UNSPECIFIED.,.F.,.F.,.F.,(3,3),(2,2),(0.,1.),(0.,0.0149999999999997),
 .UNSPECIFIED.);
#57104=B_SPLINE_SURFACE_WITH_KNOTS('',2,1,((#87051,#87052),(#87053,#87054),
(#87055,#87056)),.UNSPECIFIED.,.F.,.F.,.F.,(3,3),(2,2),(0.,1.),(0.,0.0149999999999997),
 .UNSPECIFIED.);
#57105=B_SPLINE_SURFACE_WITH_KNOTS('',2,1,((#87066,#87067),(#87068,#87069),
(#87070,#87071)),.UNSPECIFIED.,.F.,.F.,.F.,(3,3),(2,2),(0.,1.),(0.,0.0149999999999997),
 .UNSPECIFIED.);
#57106=B_SPLINE_SURFACE_WITH_KNOTS('',2,1,((#87081,#87082),(#87083,#87084),
(#87085,#87086)),.UNSPECIFIED.,.F.,.F.,.F.,(3,3),(2,2),(0.,1.),(0.,0.0149999999999997),
 .UNSPECIFIED.);
#57107=B_SPLINE_SURFACE_WITH_KNOTS('',2,1,((#87096,#87097),(#87098,#87099),
(#87100,#87101)),.UNSPECIFIED.,.F.,.F.,.F.,(3,3),(2,2),(0.,1.),(0.,0.0149999999999997),
 .UNSPECIFIED.);
#57108=B_SPLINE_SURFACE_WITH_KNOTS('',2,1,((#87111,#87112),(#87113,#87114),
(#87115,#87116)),.UNSPECIFIED.,.F.,.F.,.F.,(3,3),(2,2),(0.,1.),(0.,0.0149999999999997),
 .UNSPECIFIED.);
#57109=B_SPLINE_SURFACE_WITH_KNOTS('',2,1,((#87126,#87127),(#87128,#87129),
(#87130,#87131)),.UNSPECIFIED.,.F.,.F.,.F.,(3,3),(2,2),(0.,1.),(0.,0.0149999999999997),
 .UNSPECIFIED.);
#57110=B_SPLINE_SURFACE_WITH_KNOTS('',2,1,((#87147,#87148),(#87149,#87150),
(#87151,#87152)),.UNSPECIFIED.,.F.,.F.,.F.,(3,3),(2,2),(0.,1.),(0.,0.0149999999999997),
 .UNSPECIFIED.);
#57111=B_SPLINE_SURFACE_WITH_KNOTS('',3,3,((#103573,#103574,#103575,#103576,
#103577,#103578,#103579,#103580,#103581,#103582,#103583,#103584,#103585,
#103586,#103587,#103588,#103589,#103590,#103591,#103592,#103593,#103594,
#103595,#103596,#103597,#103598,#103599,#103600,#103601,#103602,#103603,
#103604,#103605,#103606,#103607,#103608,#103609,#103610,#103611,#103612,
#103613,#103614,#103615,#103616,#103617,#103618,#103619,#103620,#103621,
#103622,#103623,#103624,#103625,#103626,#103627,#103628,#103629,#103630,
#103631,#103632,#103633,#103634,#103635,#103636,#103637,#103638,#103639,
#103640,#103641,#103642,#103643,#103644),(#103645,#103646,#103647,#103648,
#103649,#103650,#103651,#103652,#103653,#103654,#103655,#103656,#103657,
#103658,#103659,#103660,#103661,#103662,#103663,#103664,#103665,#103666,
#103667,#103668,#103669,#103670,#103671,#103672,#103673,#103674,#103675,
#103676,#103677,#103678,#103679,#103680,#103681,#103682,#103683,#103684,
#103685,#103686,#103687,#103688,#103689,#103690,#103691,#103692,#103693,
#103694,#103695,#103696,#103697,#103698,#103699,#103700,#103701,#103702,
#103703,#103704,#103705,#103706,#103707,#103708,#103709,#103710,#103711,
#103712,#103713,#103714,#103715,#103716),(#103717,#103718,#103719,#103720,
#103721,#103722,#103723,#103724,#103725,#103726,#103727,#103728,#103729,
#103730,#103731,#103732,#103733,#103734,#103735,#103736,#103737,#103738,
#103739,#103740,#103741,#103742,#103743,#103744,#103745,#103746,#103747,
#103748,#103749,#103750,#103751,#103752,#103753,#103754,#103755,#103756,
#103757,#103758,#103759,#103760,#103761,#103762,#103763,#103764,#103765,
#103766,#103767,#103768,#103769,#103770,#103771,#103772,#103773,#103774,
#103775,#103776,#103777,#103778,#103779,#103780,#103781,#103782,#103783,
#103784,#103785,#103786,#103787,#103788),(#103789,#103790,#103791,#103792,
#103793,#103794,#103795,#103796,#103797,#103798,#103799,#103800,#103801,
#103802,#103803,#103804,#103805,#103806,#103807,#103808,#103809,#103810,
#103811,#103812,#103813,#103814,#103815,#103816,#103817,#103818,#103819,
#103820,#103821,#103822,#103823,#103824,#103825,#103826,#103827,#103828,
#103829,#103830,#103831,#103832,#103833,#103834,#103835,#103836,#103837,
#103838,#103839,#103840,#103841,#103842,#103843,#103844,#103845,#103846,
#103847,#103848,#103849,#103850,#103851,#103852,#103853,#103854,#103855,
#103856,#103857,#103858,#103859,#103860)),.UNSPECIFIED.,.F.,.F.,.F.,(4,
4),(4,1,1,1,1,1,1,1,1,1,1,1,1,1,1,1,1,1,1,1,1,1,1,1,1,1,1,1,1,1,1,1,1,1,
1,1,1,1,1,1,1,1,1,1,1,1,1,1,1,1,1,1,1,1,1,1,1,1,1,1,1,1,1,1,1,1,1,1,1,4),
(0.,0.0460148164544127),(8.31058692273973,9.29613303785021,10.2816791529607,
11.2672252680712,12.2527713831816,13.2383174982921,14.2238636134026,15.2094097285131,
16.1949558436235,17.180501958734,18.1660480738445,19.151594188955,20.1371403040654,
21.1226864191759,22.1082325342864,23.0937786493969,24.0793247645073,25.0648708796178,
26.0504169947283,27.0359631098388,28.0215092249492,29.0070553400597,29.9926014551702,
30.9781475702807,31.9636936853911,32.9492398005016,33.9347859156121,34.9203320307226,
35.905878145833,36.8914242609435,37.876970376054,38.8625164911645,39.8480626062749,
40.8336087213854,41.8191548364959,42.8047009516064,43.7902470667168,44.7757931818273,
45.7613392969378,46.7468854120483,47.7324315271587,48.7179776422692,49.7035237573797,
50.6890698724902,51.6746159876006,52.6601621027111,53.6457082178216,54.6312543329321,
55.6168004480425,56.602346563153,57.5878926782635,58.573438793374,59.5589849084844,
60.5445310235949,61.5300771387054,62.5156232538159,63.5011693689263,64.4867154840368,
65.4722615991473,66.4578077142578,67.4433538293682,68.4288999444787,69.4144460595892,
70.3999921746997,71.3855382898101,72.3710844049206,73.3566305200311,74.3421766351416,
75.327722750252,76.3132688653625),.UNSPECIFIED.);
#57112=B_SPLINE_SURFACE_WITH_KNOTS('',3,3,((#104066,#104067,#104068,#104069,
#104070,#104071,#104072,#104073,#104074,#104075,#104076,#104077,#104078,
#104079,#104080,#104081,#104082,#104083,#104084,#104085,#104086,#104087,
#104088,#104089,#104090,#104091,#104092,#104093,#104094,#104095,#104096,
#104097,#104098,#104099,#104100,#104101,#104102,#104103,#104104,#104105,
#104106,#104107,#104108,#104109,#104110,#104111,#104112,#104113,#104114,
#104115,#104116,#104117,#104118,#104119,#104120,#104121,#104122,#104123,
#104124,#104125,#104126,#104127,#104128,#104129,#104130,#104131,#104132,
#104133,#104134,#104135,#104136,#104137),(#104138,#104139,#104140,#104141,
#104142,#104143,#104144,#104145,#104146,#104147,#104148,#104149,#104150,
#104151,#104152,#104153,#104154,#104155,#104156,#104157,#104158,#104159,
#104160,#104161,#104162,#104163,#104164,#104165,#104166,#104167,#104168,
#104169,#104170,#104171,#104172,#104173,#104174,#104175,#104176,#104177,
#104178,#104179,#104180,#104181,#104182,#104183,#104184,#104185,#104186,
#104187,#104188,#104189,#104190,#104191,#104192,#104193,#104194,#104195,
#104196,#104197,#104198,#104199,#104200,#104201,#104202,#104203,#104204,
#104205,#104206,#104207,#104208,#104209),(#104210,#104211,#104212,#104213,
#104214,#104215,#104216,#104217,#104218,#104219,#104220,#104221,#104222,
#104223,#104224,#104225,#104226,#104227,#104228,#104229,#104230,#104231,
#104232,#104233,#104234,#104235,#104236,#104237,#104238,#104239,#104240,
#104241,#104242,#104243,#104244,#104245,#104246,#104247,#104248,#104249,
#104250,#104251,#104252,#104253,#104254,#104255,#104256,#104257,#104258,
#104259,#104260,#104261,#104262,#104263,#104264,#104265,#104266,#104267,
#104268,#104269,#104270,#104271,#104272,#104273,#104274,#104275,#104276,
#104277,#104278,#104279,#104280,#104281),(#104282,#104283,#104284,#104285,
#104286,#104287,#104288,#104289,#104290,#104291,#104292,#104293,#104294,
#104295,#104296,#104297,#104298,#104299,#104300,#104301,#104302,#104303,
#104304,#104305,#104306,#104307,#104308,#104309,#104310,#104311,#104312,
#104313,#104314,#104315,#104316,#104317,#104318,#104319,#104320,#104321,
#104322,#104323,#104324,#104325,#104326,#104327,#104328,#104329,#104330,
#104331,#104332,#104333,#104334,#104335,#104336,#104337,#104338,#104339,
#104340,#104341,#104342,#104343,#104344,#104345,#104346,#104347,#104348,
#104349,#104350,#104351,#104352,#104353)),.UNSPECIFIED.,.F.,.F.,.F.,(4,
4),(4,1,1,1,1,1,1,1,1,1,1,1,1,1,1,1,1,1,1,1,1,1,1,1,1,1,1,1,1,1,1,1,1,1,
1,1,1,1,1,1,1,1,1,1,1,1,1,1,1,1,1,1,1,1,1,1,1,1,1,1,1,1,1,1,1,1,1,1,1,4),
(0.,0.0460148164544127),(11.6154215191106,12.6009676342211,13.5865137493315,
14.572059864442,15.5576059795525,16.543152094663,17.5286982097734,18.5142443248839,
19.4997904399944,20.4853365551049,21.4708826702153,22.4564287853258,23.4419749004363,
24.4275210155468,25.4130671306572,26.3986132457677,27.3841593608782,28.3697054759887,
29.3552515910991,30.3407977062096,31.3263438213201,32.3118899364306,33.297436051541,
34.2829821666515,35.268528281762,36.2540743968725,37.2396205119829,38.2251666270934,
39.2107127422039,40.1962588573144,41.1818049724248,42.1673510875353,43.1528972026458,
44.1384433177563,45.1239894328667,46.1095355479772,47.0950816630877,48.0806277781982,
49.0661738933086,50.0517200084191,51.0372661235296,52.0228122386401,53.0083583537505,
53.993904468861,54.9794505839715,55.964996699082,56.9505428141924,57.9360889293029,
58.9216350444134,59.9071811595239,60.8927272746343,61.8782733897448,62.8638195048553,
63.8493656199658,64.8349117350762,65.8204578501867,66.8060039652972,67.7915500804077,
68.7770961955181,69.7626423106286,70.7481884257391,71.7337345408496,72.71928065596,
73.7048267710705,74.690372886181,75.6759190012915,76.6614651164019,77.6470112315124,
78.6325573466229,79.6181034617334),.UNSPECIFIED.);
#57113=B_SPLINE_SURFACE_WITH_KNOTS('',3,3,((#104918,#104919,#104920,#104921,
#104922,#104923,#104924,#104925,#104926,#104927,#104928,#104929,#104930,
#104931,#104932,#104933,#104934,#104935,#104936,#104937,#104938,#104939,
#104940,#104941,#104942,#104943,#104944,#104945,#104946,#104947,#104948,
#104949,#104950,#104951),(#104952,#104953,#104954,#104955,#104956,#104957,
#104958,#104959,#104960,#104961,#104962,#104963,#104964,#104965,#104966,
#104967,#104968,#104969,#104970,#104971,#104972,#104973,#104974,#104975,
#104976,#104977,#104978,#104979,#104980,#104981,#104982,#104983,#104984,
#104985),(#104986,#104987,#104988,#104989,#104990,#104991,#104992,#104993,
#104994,#104995,#104996,#104997,#104998,#104999,#105000,#105001,#105002,
#105003,#105004,#105005,#105006,#105007,#105008,#105009,#105010,#105011,
#105012,#105013,#105014,#105015,#105016,#105017,#105018,#105019),(#105020,
#105021,#105022,#105023,#105024,#105025,#105026,#105027,#105028,#105029,
#105030,#105031,#105032,#105033,#105034,#105035,#105036,#105037,#105038,
#105039,#105040,#105041,#105042,#105043,#105044,#105045,#105046,#105047,
#105048,#105049,#105050,#105051,#105052,#105053)),.UNSPECIFIED.,.F.,.F.,
 .F.,(4,4),(4,1,1,1,1,1,1,1,1,1,1,1,1,1,1,1,1,1,1,1,1,1,1,1,1,1,1,1,1,1,
1,4),(0.,0.032995567884187),(8.30203615430844,9.2903114149458,10.2785866755832,
11.2668619362205,12.2551371968579,13.2434124574953,14.2316877181326,15.21996297877,
16.2082382394074,17.1965135000447,18.1847887606821,19.1730640213194,20.1613392819568,
21.1496145425942,22.1378898032315,23.1261650638689,24.1144403245063,25.1027155851436,
26.090990845781,27.0792661064184,28.0675413670557,29.0558166276931,30.0440918883304,
31.0323671489678,32.0206424096052,33.0089176702425,33.9971929308799,34.9854681915173,
35.9737434521546,36.962018712792,37.9502939734294,38.9385692340667),
 .UNSPECIFIED.);
#57114=B_SPLINE_SURFACE_WITH_KNOTS('',3,3,((#105256,#105257,#105258,#105259,
#105260,#105261,#105262,#105263,#105264,#105265,#105266,#105267,#105268,
#105269,#105270,#105271,#105272,#105273,#105274,#105275,#105276,#105277,
#105278,#105279,#105280,#105281,#105282,#105283,#105284,#105285,#105286,
#105287,#105288,#105289),(#105290,#105291,#105292,#105293,#105294,#105295,
#105296,#105297,#105298,#105299,#105300,#105301,#105302,#105303,#105304,
#105305,#105306,#105307,#105308,#105309,#105310,#105311,#105312,#105313,
#105314,#105315,#105316,#105317,#105318,#105319,#105320,#105321,#105322,
#105323),(#105324,#105325,#105326,#105327,#105328,#105329,#105330,#105331,
#105332,#105333,#105334,#105335,#105336,#105337,#105338,#105339,#105340,
#105341,#105342,#105343,#105344,#105345,#105346,#105347,#105348,#105349,
#105350,#105351,#105352,#105353,#105354,#105355,#105356,#105357),(#105358,
#105359,#105360,#105361,#105362,#105363,#105364,#105365,#105366,#105367,
#105368,#105369,#105370,#105371,#105372,#105373,#105374,#105375,#105376,
#105377,#105378,#105379,#105380,#105381,#105382,#105383,#105384,#105385,
#105386,#105387,#105388,#105389,#105390,#105391)),.UNSPECIFIED.,.F.,.F.,
 .F.,(4,4),(4,1,1,1,1,1,1,1,1,1,1,1,1,1,1,1,1,1,1,1,1,1,1,1,1,1,1,1,1,1,
1,4),(0.,0.032995567884187),(11.6159397475005,12.6042150081378,13.5924902687752,
14.5807655294126,15.5690407900499,16.5573160506873,17.5455913113246,18.533866571962,
19.5221418325994,20.5104170932367,21.4986923538741,22.4869676145115,23.4752428751488,
24.4635181357862,25.4517933964236,26.4400686570609,27.4283439176983,28.4166191783357,
29.404894438973,30.3931696996104,31.3814449602478,32.3697202208851,33.3579954815225,
34.3462707421599,35.3345460027972,36.3228212634346,37.311096524072,38.2993717847093,
39.2876470453467,40.2759223059841,41.2641975666214,42.2524728272588),
 .UNSPECIFIED.);
#57115=B_SPLINE_SURFACE_WITH_KNOTS('',3,3,((#105958,#105959,#105960,#105961,
#105962,#105963,#105964,#105965,#105966,#105967,#105968,#105969,#105970,
#105971,#105972,#105973,#105974,#105975,#105976,#105977,#105978,#105979,
#105980,#105981,#105982,#105983),(#105984,#105985,#105986,#105987,#105988,
#105989,#105990,#105991,#105992,#105993,#105994,#105995,#105996,#105997,
#105998,#105999,#106000,#106001,#106002,#106003,#106004,#106005,#106006,
#106007,#106008,#106009),(#106010,#106011,#106012,#106013,#106014,#106015,
#106016,#106017,#106018,#106019,#106020,#106021,#106022,#106023,#106024,
#106025,#106026,#106027,#106028,#106029,#106030,#106031,#106032,#106033,
#106034,#106035),(#106036,#106037,#106038,#106039,#106040,#106041,#106042,
#106043,#106044,#106045,#106046,#106047,#106048,#106049,#106050,#106051,
#106052,#106053,#106054,#106055,#106056,#106057,#106058,#106059,#106060,
#106061)),.UNSPECIFIED.,.F.,.F.,.F.,(4,4),(4,1,1,1,1,1,1,1,1,1,1,1,1,1,
1,1,1,1,1,1,1,1,1,4),(0.,0.026298304761587),(8.3092913517653,9.30503384311121,
10.3007763344571,11.296518825803,12.2922613171489,13.2880038084949,14.2837462998408,
15.2794887911867,16.2752312825326,17.2709737738785,18.2667162652244,19.2624587565703,
20.2582012479163,21.2539437392622,22.2496862306081,23.245428721954,24.2411712132999,
25.2369137046458,26.2326561959917,27.2283986873376,28.2241411786836,29.2198836700295,
30.2156261613754,31.2113686527213),.UNSPECIFIED.);
#57116=B_SPLINE_SURFACE_WITH_KNOTS('',3,3,((#106240,#106241,#106242,#106243,
#106244,#106245,#106246,#106247,#106248,#106249,#106250,#106251,#106252,
#106253,#106254,#106255,#106256,#106257,#106258,#106259,#106260,#106261,
#106262,#106263,#106264,#106265),(#106266,#106267,#106268,#106269,#106270,
#106271,#106272,#106273,#106274,#106275,#106276,#106277,#106278,#106279,
#106280,#106281,#106282,#106283,#106284,#106285,#106286,#106287,#106288,
#106289,#106290,#106291),(#106292,#106293,#106294,#106295,#106296,#106297,
#106298,#106299,#106300,#106301,#106302,#106303,#106304,#106305,#106306,
#106307,#106308,#106309,#106310,#106311,#106312,#106313,#106314,#106315,
#106316,#106317),(#106318,#106319,#106320,#106321,#106322,#106323,#106324,
#106325,#106326,#106327,#106328,#106329,#106330,#106331,#106332,#106333,
#106334,#106335,#106336,#106337,#106338,#106339,#106340,#106341,#106342,
#106343)),.UNSPECIFIED.,.F.,.F.,.F.,(4,4),(4,1,1,1,1,1,1,1,1,1,1,1,1,1,
1,1,1,1,1,1,1,1,1,4),(0.,0.026298304761587),(11.6163931973415,12.6121356886874,
13.6078781800333,14.6036206713792,15.5993631627251,16.595105654071,17.590848145417,
18.5865906367629,19.5823331281088,20.5780756194547,21.5738181108006,22.5695606021465,
23.5653030934924,24.5610455848383,25.5567880761843,26.5525305675302,27.5482730588761,
28.544015550222,29.5397580415679,30.5355005329138,31.5312430242597,32.5269855156056,
33.5227280069516,34.5184704982975),.UNSPECIFIED.);
#57117=B_SPLINE_SURFACE_WITH_KNOTS('',3,3,((#107449,#107450,#107451,#107452,
#107453,#107454,#107455,#107456,#107457,#107458,#107459,#107460,#107461,
#107462,#107463,#107464,#107465,#107466,#107467,#107468,#107469,#107470,
#107471,#107472,#107473,#107474,#107475,#107476,#107477,#107478,#107479,
#107480,#107481,#107482,#107483,#107484,#107485,#107486,#107487,#107488,
#107489,#107490,#107491,#107492,#107493,#107494,#107495,#107496,#107497,
#107498,#107499,#107500,#107501,#107502,#107503,#107504,#107505,#107506,
#107507,#107508,#107509,#107510,#107511,#107512,#107513,#107514,#107515,
#107516,#107517,#107518,#107519,#107520),(#107521,#107522,#107523,#107524,
#107525,#107526,#107527,#107528,#107529,#107530,#107531,#107532,#107533,
#107534,#107535,#107536,#107537,#107538,#107539,#107540,#107541,#107542,
#107543,#107544,#107545,#107546,#107547,#107548,#107549,#107550,#107551,
#107552,#107553,#107554,#107555,#107556,#107557,#107558,#107559,#107560,
#107561,#107562,#107563,#107564,#107565,#107566,#107567,#107568,#107569,
#107570,#107571,#107572,#107573,#107574,#107575,#107576,#107577,#107578,
#107579,#107580,#107581,#107582,#107583,#107584,#107585,#107586,#107587,
#107588,#107589,#107590,#107591,#107592),(#107593,#107594,#107595,#107596,
#107597,#107598,#107599,#107600,#107601,#107602,#107603,#107604,#107605,
#107606,#107607,#107608,#107609,#107610,#107611,#107612,#107613,#107614,
#107615,#107616,#107617,#107618,#107619,#107620,#107621,#107622,#107623,
#107624,#107625,#107626,#107627,#107628,#107629,#107630,#107631,#107632,
#107633,#107634,#107635,#107636,#107637,#107638,#107639,#107640,#107641,
#107642,#107643,#107644,#107645,#107646,#107647,#107648,#107649,#107650,
#107651,#107652,#107653,#107654,#107655,#107656,#107657,#107658,#107659,
#107660,#107661,#107662,#107663,#107664),(#107665,#107666,#107667,#107668,
#107669,#107670,#107671,#107672,#107673,#107674,#107675,#107676,#107677,
#107678,#107679,#107680,#107681,#107682,#107683,#107684,#107685,#107686,
#107687,#107688,#107689,#107690,#107691,#107692,#107693,#107694,#107695,
#107696,#107697,#107698,#107699,#107700,#107701,#107702,#107703,#107704,
#107705,#107706,#107707,#107708,#107709,#107710,#107711,#107712,#107713,
#107714,#107715,#107716,#107717,#107718,#107719,#107720,#107721,#107722,
#107723,#107724,#107725,#107726,#107727,#107728,#107729,#107730,#107731,
#107732,#107733,#107734,#107735,#107736)),.UNSPECIFIED.,.F.,.F.,.F.,(4,
4),(4,1,1,1,1,1,1,1,1,1,1,1,1,1,1,1,1,1,1,1,1,1,1,1,1,1,1,1,1,1,1,1,1,1,
1,1,1,1,1,1,1,1,1,1,1,1,1,1,1,1,1,1,1,1,1,1,1,1,1,1,1,1,1,1,1,1,1,1,1,4),
(0.,0.0329955678841871),(8.30203615430834,9.29240781985667,10.282779485405,
11.2731511509533,12.2635228165017,13.25389448205,14.2442661475984,15.2346378131467,
16.225009478695,17.2153811442434,18.2057528097917,19.19612447534,20.1864961408884,
21.1768678064367,22.1672394719851,23.1576111375334,24.1479828030817,25.1383544686301,
26.1287261341784,27.1190977997268,28.1094694652751,29.0998411308234,30.0902127963718,
31.0805844619201,32.0709561274684,33.0613277930168,34.0516994585651,35.0420711241134,
36.0324427896618,37.0228144552101,38.0131861207585,39.0035577863068,39.9939294518551,
40.9843011174035,41.9746727829518,42.9650444485002,43.9554161140485,44.9457877795968,
45.9361594451452,46.9265311106935,47.9169027762418,48.9072744417902,49.8976461073385,
50.8880177728869,51.8783894384352,52.8687611039835,53.8591327695319,54.8495044350802,
55.8398761006285,56.8302477661769,57.8206194317252,58.8109910972736,59.8013627628219,
60.7917344283702,61.7821060939186,62.7724777594669,63.7628494250152,64.7532210905636,
65.7435927561119,66.7339644216603,67.7243360872086,68.7147077527569,69.7050794183053,
70.6954510838536,71.685822749402,72.6761944149503,73.6665660804986,74.656937746047,
75.6473094115953,76.6376810771436),.UNSPECIFIED.);
#57118=B_SPLINE_SURFACE_WITH_KNOTS('',3,3,((#107939,#107940,#107941,#107942,
#107943,#107944,#107945,#107946,#107947,#107948,#107949,#107950,#107951,
#107952,#107953,#107954,#107955,#107956,#107957,#107958,#107959,#107960,
#107961,#107962,#107963,#107964,#107965,#107966,#107967,#107968,#107969,
#107970,#107971,#107972,#107973,#107974,#107975,#107976,#107977,#107978,
#107979,#107980,#107981,#107982,#107983,#107984,#107985,#107986,#107987,
#107988,#107989,#107990,#107991,#107992,#107993,#107994,#107995,#107996,
#107997,#107998,#107999,#108000,#108001,#108002,#108003,#108004,#108005,
#108006,#108007,#108008,#108009,#108010),(#108011,#108012,#108013,#108014,
#108015,#108016,#108017,#108018,#108019,#108020,#108021,#108022,#108023,
#108024,#108025,#108026,#108027,#108028,#108029,#108030,#108031,#108032,
#108033,#108034,#108035,#108036,#108037,#108038,#108039,#108040,#108041,
#108042,#108043,#108044,#108045,#108046,#108047,#108048,#108049,#108050,
#108051,#108052,#108053,#108054,#108055,#108056,#108057,#108058,#108059,
#108060,#108061,#108062,#108063,#108064,#108065,#108066,#108067,#108068,
#108069,#108070,#108071,#108072,#108073,#108074,#108075,#108076,#108077,
#108078,#108079,#108080,#108081,#108082),(#108083,#108084,#108085,#108086,
#108087,#108088,#108089,#108090,#108091,#108092,#108093,#108094,#108095,
#108096,#108097,#108098,#108099,#108100,#108101,#108102,#108103,#108104,
#108105,#108106,#108107,#108108,#108109,#108110,#108111,#108112,#108113,
#108114,#108115,#108116,#108117,#108118,#108119,#108120,#108121,#108122,
#108123,#108124,#108125,#108126,#108127,#108128,#108129,#108130,#108131,
#108132,#108133,#108134,#108135,#108136,#108137,#108138,#108139,#108140,
#108141,#108142,#108143,#108144,#108145,#108146,#108147,#108148,#108149,
#108150,#108151,#108152,#108153,#108154),(#108155,#108156,#108157,#108158,
#108159,#108160,#108161,#108162,#108163,#108164,#108165,#108166,#108167,
#108168,#108169,#108170,#108171,#108172,#108173,#108174,#108175,#108176,
#108177,#108178,#108179,#108180,#108181,#108182,#108183,#108184,#108185,
#108186,#108187,#108188,#108189,#108190,#108191,#108192,#108193,#108194,
#108195,#108196,#108197,#108198,#108199,#108200,#108201,#108202,#108203,
#108204,#108205,#108206,#108207,#108208,#108209,#108210,#108211,#108212,
#108213,#108214,#108215,#108216,#108217,#108218,#108219,#108220,#108221,
#108222,#108223,#108224,#108225,#108226)),.UNSPECIFIED.,.F.,.F.,.F.,(4,
4),(4,1,1,1,1,1,1,1,1,1,1,1,1,1,1,1,1,1,1,1,1,1,1,1,1,1,1,1,1,1,1,1,1,1,
1,1,1,1,1,1,1,1,1,1,1,1,1,1,1,1,1,1,1,1,1,1,1,1,1,1,1,1,1,1,1,1,1,1,1,4),
(0.,0.0329955678841871),(11.6159397475004,12.6063114130487,13.596683078597,
14.5870547441454,15.5774264096937,16.5677980752421,17.5581697407904,18.5485414063387,
19.5389130718871,20.5292847374354,21.5196564029837,22.5100280685321,23.5003997340804,
24.4907713996288,25.4811430651771,26.4715147307254,27.4618863962738,28.4522580618221,
29.4426297273704,30.4330013929188,31.4233730584671,32.4137447240155,33.4041163895638,
34.3944880551121,35.3848597206605,36.3752313862088,37.3656030517571,38.3559747173055,
39.3463463828538,40.3367180484022,41.3270897139505,42.3174613794988,43.3078330450472,
44.2982047105955,45.2885763761439,46.2789480416922,47.2693197072405,48.2596913727889,
49.2500630383372,50.2404347038855,51.2308063694339,52.2211780349822,53.2115497005306,
54.2019213660789,55.1922930316272,56.1826646971756,57.1730363627239,58.1634080282722,
59.1537796938206,60.1441513593689,61.1345230249173,62.1248946904656,63.1152663560139,
64.1056380215623,65.0960096871106,66.0863813526589,67.0767530182073,68.0671246837556,
69.057496349304,70.0478680148523,71.0382396804006,72.028611345949,73.0189830114973,
74.0093546770456,74.999726342594,75.9900980081423,76.9804696736907,77.970841339239,
78.9612130047873,79.9515846703357),.UNSPECIFIED.);
#57119=B_SPLINE_SURFACE_WITH_KNOTS('',3,3,((#108958,#108959,#108960,#108961,
#108962,#108963,#108964,#108965,#108966,#108967,#108968,#108969,#108970,
#108971,#108972,#108973,#108974,#108975,#108976,#108977,#108978,#108979,
#108980,#108981,#108982,#108983,#108984,#108985,#108986,#108987,#108988,
#108989,#108990,#108991,#108992,#108993,#108994,#108995,#108996,#108997,
#108998,#108999),(#109000,#109001,#109002,#109003,#109004,#109005,#109006,
#109007,#109008,#109009,#109010,#109011,#109012,#109013,#109014,#109015,
#109016,#109017,#109018,#109019,#109020,#109021,#109022,#109023,#109024,
#109025,#109026,#109027,#109028,#109029,#109030,#109031,#109032,#109033,
#109034,#109035,#109036,#109037,#109038,#109039,#109040,#109041),(#109042,
#109043,#109044,#109045,#109046,#109047,#109048,#109049,#109050,#109051,
#109052,#109053,#109054,#109055,#109056,#109057,#109058,#109059,#109060,
#109061,#109062,#109063,#109064,#109065,#109066,#109067,#109068,#109069,
#109070,#109071,#109072,#109073,#109074,#109075,#109076,#109077,#109078,
#109079,#109080,#109081,#109082,#109083),(#109084,#109085,#109086,#109087,
#109088,#109089,#109090,#109091,#109092,#109093,#109094,#109095,#109096,
#109097,#109098,#109099,#109100,#109101,#109102,#109103,#109104,#109105,
#109106,#109107,#109108,#109109,#109110,#109111,#109112,#109113,#109114,
#109115,#109116,#109117,#109118,#109119,#109120,#109121,#109122,#109123,
#109124,#109125)),.UNSPECIFIED.,.F.,.F.,.F.,(4,4),(4,1,1,1,1,1,1,1,1,1,
1,1,1,1,1,1,1,1,1,1,1,1,1,1,1,1,1,1,1,1,1,1,1,1,1,1,1,1,1,4),(0.,0.026298304761587),
(8.3092913517653,9.29929239199363,10.289293432222,11.2792944724503,12.2692955126786,
13.2592965529069,14.2492975931353,15.2392986333636,16.2292996735919,17.2193007138202,
18.2093017540486,19.1993027942769,20.1893038345052,21.1793048747336,22.1693059149619,
23.1593069551902,24.1493079954185,25.1393090356469,26.1293100758752,27.1193111161035,
28.1093121563318,29.0993131965602,30.0893142367885,31.0793152770168,32.0693163172452,
33.0593173574735,34.0493183977018,35.0393194379301,36.0293204781585,37.0193215183868,
38.0093225586151,38.9993235988434,39.9893246390718,40.9793256793001,41.9693267195284,
42.9593277597568,43.9493287999851,44.9393298402134,45.9293308804417,46.9193319206701),
 .UNSPECIFIED.);
#57120=B_SPLINE_SURFACE_WITH_KNOTS('',3,3,((#109316,#109317,#109318,#109319,
#109320,#109321,#109322,#109323,#109324,#109325,#109326,#109327,#109328,
#109329,#109330,#109331,#109332,#109333,#109334,#109335,#109336,#109337,
#109338,#109339,#109340,#109341,#109342,#109343,#109344,#109345,#109346,
#109347,#109348,#109349,#109350,#109351,#109352,#109353,#109354,#109355,
#109356,#109357),(#109358,#109359,#109360,#109361,#109362,#109363,#109364,
#109365,#109366,#109367,#109368,#109369,#109370,#109371,#109372,#109373,
#109374,#109375,#109376,#109377,#109378,#109379,#109380,#109381,#109382,
#109383,#109384,#109385,#109386,#109387,#109388,#109389,#109390,#109391,
#109392,#109393,#109394,#109395,#109396,#109397,#109398,#109399),(#109400,
#109401,#109402,#109403,#109404,#109405,#109406,#109407,#109408,#109409,
#109410,#109411,#109412,#109413,#109414,#109415,#109416,#109417,#109418,
#109419,#109420,#109421,#109422,#109423,#109424,#109425,#109426,#109427,
#109428,#109429,#109430,#109431,#109432,#109433,#109434,#109435,#109436,
#109437,#109438,#109439,#109440,#109441),(#109442,#109443,#109444,#109445,
#109446,#109447,#109448,#109449,#109450,#109451,#109452,#109453,#109454,
#109455,#109456,#109457,#109458,#109459,#109460,#109461,#109462,#109463,
#109464,#109465,#109466,#109467,#109468,#109469,#109470,#109471,#109472,
#109473,#109474,#109475,#109476,#109477,#109478,#109479,#109480,#109481,
#109482,#109483)),.UNSPECIFIED.,.F.,.F.,.F.,(4,4),(4,1,1,1,1,1,1,1,1,1,
1,1,1,1,1,1,1,1,1,1,1,1,1,1,1,1,1,1,1,1,1,1,1,1,1,1,1,1,1,4),(0.,0.026298304761587),
(11.6163931973415,12.6063942375698,13.5963952777981,14.5863963180265,15.5763973582548,
16.5663983984831,17.5563994387115,18.5464004789398,19.5364015191681,20.5264025593964,
21.5164035996248,22.5064046398531,23.4964056800814,24.4864067203097,25.4764077605381,
26.4664088007664,27.4564098409947,28.4464108812231,29.4364119214514,30.4264129616797,
31.416414001908,32.4064150421364,33.3964160823647,34.386417122593,35.3764181628213,
36.3664192030497,37.356420243278,38.3464212835063,39.3364223237347,40.326423363963,
41.3164244041913,42.3064254444196,43.296426484648,44.2864275248763,45.2764285651046,
46.2664296053329,47.2564306455613,48.2464316857896,49.2364327260179,50.2264337662462),
 .UNSPECIFIED.);
#57121=B_SPLINE_SURFACE_WITH_KNOTS('',3,3,((#110352,#110353,#110354,#110355,
#110356,#110357,#110358,#110359,#110360,#110361,#110362,#110363,#110364,
#110365,#110366,#110367,#110368,#110369,#110370,#110371,#110372,#110373,
#110374,#110375,#110376,#110377,#110378,#110379,#110380,#110381,#110382,
#110383,#110384,#110385,#110386,#110387,#110388,#110389,#110390,#110391,
#110392,#110393,#110394,#110395,#110396,#110397,#110398,#110399,#110400,
#110401,#110402),(#110403,#110404,#110405,#110406,#110407,#110408,#110409,
#110410,#110411,#110412,#110413,#110414,#110415,#110416,#110417,#110418,
#110419,#110420,#110421,#110422,#110423,#110424,#110425,#110426,#110427,
#110428,#110429,#110430,#110431,#110432,#110433,#110434,#110435,#110436,
#110437,#110438,#110439,#110440,#110441,#110442,#110443,#110444,#110445,
#110446,#110447,#110448,#110449,#110450,#110451,#110452,#110453),(#110454,
#110455,#110456,#110457,#110458,#110459,#110460,#110461,#110462,#110463,
#110464,#110465,#110466,#110467,#110468,#110469,#110470,#110471,#110472,
#110473,#110474,#110475,#110476,#110477,#110478,#110479,#110480,#110481,
#110482,#110483,#110484,#110485,#110486,#110487,#110488,#110489,#110490,
#110491,#110492,#110493,#110494,#110495,#110496,#110497,#110498,#110499,
#110500,#110501,#110502,#110503,#110504),(#110505,#110506,#110507,#110508,
#110509,#110510,#110511,#110512,#110513,#110514,#110515,#110516,#110517,
#110518,#110519,#110520,#110521,#110522,#110523,#110524,#110525,#110526,
#110527,#110528,#110529,#110530,#110531,#110532,#110533,#110534,#110535,
#110536,#110537,#110538,#110539,#110540,#110541,#110542,#110543,#110544,
#110545,#110546,#110547,#110548,#110549,#110550,#110551,#110552,#110553,
#110554,#110555)),.UNSPECIFIED.,.F.,.F.,.F.,(4,4),(4,1,1,1,1,1,1,1,1,1,
1,1,1,1,1,1,1,1,1,1,1,1,1,1,1,1,1,1,1,1,1,1,1,1,1,1,1,1,1,1,1,1,1,1,1,1,
1,1,4),(0.,0.0262983047615868),(8.30929135176535,9.30134463307939,10.2933979143934,
11.2854511957075,12.2775044770215,13.2695577583356,14.2616110396496,15.2536643209636,
16.2457176022777,17.2377708835917,18.2298241649058,19.2218774462198,20.2139307275338,
21.2059840088479,22.1980372901619,23.1900905714759,24.18214385279,25.174197134104,
26.1662504154181,27.1583036967321,28.1503569780461,29.1424102593602,30.1344635406742,
31.1265168219883,32.1185701033023,33.1106233846163,34.1026766659304,35.0947299472444,
36.0867832285585,37.0788365098725,38.0708897911865,39.0629430725006,40.0549963538146,
41.0470496351287,42.0391029164427,43.0311561977567,44.0232094790708,45.0152627603848,
46.0073160416989,46.9993693230129,47.9914226043269,48.983475885641,49.975529166955,
50.967582448269,51.9596357295831,52.9516890108971,53.9437422922112,54.9357955735252,
55.9278488548392),.UNSPECIFIED.);
#57122=B_SPLINE_SURFACE_WITH_KNOTS('',3,3,((#110734,#110735,#110736,#110737,
#110738,#110739,#110740,#110741,#110742,#110743,#110744,#110745,#110746,
#110747,#110748,#110749,#110750,#110751,#110752,#110753,#110754,#110755,
#110756,#110757,#110758,#110759,#110760,#110761,#110762,#110763,#110764,
#110765,#110766,#110767,#110768,#110769,#110770,#110771,#110772,#110773,
#110774,#110775,#110776,#110777,#110778,#110779,#110780,#110781,#110782,
#110783,#110784),(#110785,#110786,#110787,#110788,#110789,#110790,#110791,
#110792,#110793,#110794,#110795,#110796,#110797,#110798,#110799,#110800,
#110801,#110802,#110803,#110804,#110805,#110806,#110807,#110808,#110809,
#110810,#110811,#110812,#110813,#110814,#110815,#110816,#110817,#110818,
#110819,#110820,#110821,#110822,#110823,#110824,#110825,#110826,#110827,
#110828,#110829,#110830,#110831,#110832,#110833,#110834,#110835),(#110836,
#110837,#110838,#110839,#110840,#110841,#110842,#110843,#110844,#110845,
#110846,#110847,#110848,#110849,#110850,#110851,#110852,#110853,#110854,
#110855,#110856,#110857,#110858,#110859,#110860,#110861,#110862,#110863,
#110864,#110865,#110866,#110867,#110868,#110869,#110870,#110871,#110872,
#110873,#110874,#110875,#110876,#110877,#110878,#110879,#110880,#110881,
#110882,#110883,#110884,#110885,#110886),(#110887,#110888,#110889,#110890,
#110891,#110892,#110893,#110894,#110895,#110896,#110897,#110898,#110899,
#110900,#110901,#110902,#110903,#110904,#110905,#110906,#110907,#110908,
#110909,#110910,#110911,#110912,#110913,#110914,#110915,#110916,#110917,
#110918,#110919,#110920,#110921,#110922,#110923,#110924,#110925,#110926,
#110927,#110928,#110929,#110930,#110931,#110932,#110933,#110934,#110935,
#110936,#110937)),.UNSPECIFIED.,.F.,.F.,.F.,(4,4),(4,1,1,1,1,1,1,1,1,1,
1,1,1,1,1,1,1,1,1,1,1,1,1,1,1,1,1,1,1,1,1,1,1,1,1,1,1,1,1,1,1,1,1,1,1,1,
1,1,4),(0.,0.0262983047615868),(11.6163931973415,12.6084464786556,13.6004997599696,
14.5925530412836,15.5846063225977,16.5766596039117,17.5687128852257,18.5607661665398,
19.5528194478538,20.5448727291679,21.5369260104819,22.5289792917959,23.52103257311,
24.513085854424,25.5051391357381,26.4971924170521,27.4892456983661,28.4812989796802,
29.4733522609942,30.4654055423083,31.4574588236223,32.4495121049363,33.4415653862504,
34.4336186675644,35.4256719488784,36.4177252301925,37.4097785115065,38.4018317928206,
39.3938850741346,40.3859383554486,41.3779916367627,42.3700449180767,43.3620981993908,
44.3541514807048,45.3462047620188,46.3382580433329,47.3303113246469,48.322364605961,
49.314417887275,50.306471168589,51.2985244499031,52.2905777312171,53.2826310125312,
54.2746842938452,55.2667375751592,56.2587908564733,57.2508441377873,58.2428974191013,
59.2349507004154),.UNSPECIFIED.);
#57123=B_SPLINE_SURFACE_WITH_KNOTS('',3,3,((#112068,#112069,#112070,#112071,
#112072,#112073,#112074,#112075,#112076,#112077,#112078,#112079,#112080,
#112081,#112082,#112083,#112084,#112085,#112086,#112087,#112088,#112089,
#112090,#112091,#112092,#112093,#112094,#112095,#112096,#112097,#112098,
#112099,#112100,#112101,#112102,#112103,#112104,#112105,#112106,#112107,
#112108,#112109,#112110,#112111,#112112,#112113,#112114,#112115,#112116,
#112117,#112118,#112119,#112120,#112121,#112122,#112123,#112124,#112125,
#112126,#112127,#112128,#112129,#112130,#112131,#112132,#112133,#112134,
#112135,#112136,#112137,#112138,#112139,#112140,#112141,#112142,#112143,
#112144,#112145,#112146,#112147,#112148,#112149,#112150),(#112151,#112152,
#112153,#112154,#112155,#112156,#112157,#112158,#112159,#112160,#112161,
#112162,#112163,#112164,#112165,#112166,#112167,#112168,#112169,#112170,
#112171,#112172,#112173,#112174,#112175,#112176,#112177,#112178,#112179,
#112180,#112181,#112182,#112183,#112184,#112185,#112186,#112187,#112188,
#112189,#112190,#112191,#112192,#112193,#112194,#112195,#112196,#112197,
#112198,#112199,#112200,#112201,#112202,#112203,#112204,#112205,#112206,
#112207,#112208,#112209,#112210,#112211,#112212,#112213,#112214,#112215,
#112216,#112217,#112218,#112219,#112220,#112221,#112222,#112223,#112224,
#112225,#112226,#112227,#112228,#112229,#112230,#112231,#112232,#112233),
(#112234,#112235,#112236,#112237,#112238,#112239,#112240,#112241,#112242,
#112243,#112244,#112245,#112246,#112247,#112248,#112249,#112250,#112251,
#112252,#112253,#112254,#112255,#112256,#112257,#112258,#112259,#112260,
#112261,#112262,#112263,#112264,#112265,#112266,#112267,#112268,#112269,
#112270,#112271,#112272,#112273,#112274,#112275,#112276,#112277,#112278,
#112279,#112280,#112281,#112282,#112283,#112284,#112285,#112286,#112287,
#112288,#112289,#112290,#112291,#112292,#112293,#112294,#112295,#112296,
#112297,#112298,#112299,#112300,#112301,#112302,#112303,#112304,#112305,
#112306,#112307,#112308,#112309,#112310,#112311,#112312,#112313,#112314,
#112315,#112316),(#112317,#112318,#112319,#112320,#112321,#112322,#112323,
#112324,#112325,#112326,#112327,#112328,#112329,#112330,#112331,#112332,
#112333,#112334,#112335,#112336,#112337,#112338,#112339,#112340,#112341,
#112342,#112343,#112344,#112345,#112346,#112347,#112348,#112349,#112350,
#112351,#112352,#112353,#112354,#112355,#112356,#112357,#112358,#112359,
#112360,#112361,#112362,#112363,#112364,#112365,#112366,#112367,#112368,
#112369,#112370,#112371,#112372,#112373,#112374,#112375,#112376,#112377,
#112378,#112379,#112380,#112381,#112382,#112383,#112384,#112385,#112386,
#112387,#112388,#112389,#112390,#112391,#112392,#112393,#112394,#112395,
#112396,#112397,#112398,#112399)),.UNSPECIFIED.,.F.,.F.,.F.,(4,4),(4,1,
1,1,1,1,1,1,1,1,1,1,1,1,1,1,1,1,1,1,1,1,1,1,1,1,1,1,1,1,1,1,1,1,1,1,1,1,
1,1,1,1,1,1,1,1,1,1,1,1,1,1,1,1,1,1,1,1,1,1,1,1,1,1,1,1,1,1,1,1,1,1,1,1,
1,1,1,1,1,1,4),(0.,0.0296469363228873),(8.30626835282486,9.30079792027989,
10.2953274877349,11.2898570551899,12.284386622645,13.2789161901,14.273445757555,
15.26797532501,16.2625048924651,17.2570344599201,18.2515640273751,19.2460935948302,
20.2406231622852,21.2351527297402,22.2296822971952,23.2242118646503,24.2187414321053,
25.2132709995603,26.2078005670153,27.2023301344704,28.1968597019254,29.1913892693804,
30.1859188368355,31.1804484042905,32.1749779717455,33.1695075392005,34.1640371066556,
35.1585666741106,36.1530962415656,37.1476258090206,38.1421553764757,39.1366849439307,
40.1312145113857,41.1257440788408,42.1202736462958,43.1148032137508,44.1093327812058,
45.1038623486609,46.0983919161159,47.0929214835709,48.0874510510259,49.081980618481,
50.076510185936,51.071039753391,52.0655693208461,53.0600988883011,54.0546284557561,
55.0491580232111,56.0436875906662,57.0382171581212,58.0327467255762,59.0272762930312,
60.0218058604863,61.0163354279413,62.0108649953963,63.0053945628514,63.9999241303064,
64.9944536977614,65.9889832652164,66.9835128326715,67.9780424001265,68.9725719675815,
69.9671015350365,70.9616311024916,71.9561606699466,72.9506902374016,73.9452198048566,
74.9397493723117,75.9342789397667,76.9288085072217,77.9233380746768,78.9178676421318,
79.9123972095868,80.9069267770418,81.9014563444969,82.8959859119519,83.8905154794069,
84.8850450468619,85.879574614317,86.874104181772,87.868633749227),
 .UNSPECIFIED.);
#57124=B_SPLINE_SURFACE_WITH_KNOTS('',3,3,((#112596,#112597,#112598,#112599,
#112600,#112601,#112602,#112603,#112604,#112605,#112606,#112607,#112608,
#112609,#112610,#112611,#112612,#112613,#112614,#112615,#112616,#112617,
#112618,#112619,#112620,#112621,#112622,#112623,#112624,#112625,#112626,
#112627,#112628,#112629,#112630,#112631,#112632,#112633,#112634,#112635,
#112636,#112637,#112638,#112639,#112640,#112641,#112642,#112643,#112644,
#112645,#112646,#112647,#112648,#112649,#112650,#112651,#112652,#112653,
#112654,#112655,#112656,#112657,#112658,#112659,#112660,#112661,#112662,
#112663,#112664,#112665,#112666,#112667,#112668,#112669,#112670,#112671,
#112672,#112673,#112674,#112675,#112676,#112677,#112678),(#112679,#112680,
#112681,#112682,#112683,#112684,#112685,#112686,#112687,#112688,#112689,
#112690,#112691,#112692,#112693,#112694,#112695,#112696,#112697,#112698,
#112699,#112700,#112701,#112702,#112703,#112704,#112705,#112706,#112707,
#112708,#112709,#112710,#112711,#112712,#112713,#112714,#112715,#112716,
#112717,#112718,#112719,#112720,#112721,#112722,#112723,#112724,#112725,
#112726,#112727,#112728,#112729,#112730,#112731,#112732,#112733,#112734,
#112735,#112736,#112737,#112738,#112739,#112740,#112741,#112742,#112743,
#112744,#112745,#112746,#112747,#112748,#112749,#112750,#112751,#112752,
#112753,#112754,#112755,#112756,#112757,#112758,#112759,#112760,#112761),
(#112762,#112763,#112764,#112765,#112766,#112767,#112768,#112769,#112770,
#112771,#112772,#112773,#112774,#112775,#112776,#112777,#112778,#112779,
#112780,#112781,#112782,#112783,#112784,#112785,#112786,#112787,#112788,
#112789,#112790,#112791,#112792,#112793,#112794,#112795,#112796,#112797,
#112798,#112799,#112800,#112801,#112802,#112803,#112804,#112805,#112806,
#112807,#112808,#112809,#112810,#112811,#112812,#112813,#112814,#112815,
#112816,#112817,#112818,#112819,#112820,#112821,#112822,#112823,#112824,
#112825,#112826,#112827,#112828,#112829,#112830,#112831,#112832,#112833,
#112834,#112835,#112836,#112837,#112838,#112839,#112840,#112841,#112842,
#112843,#112844),(#112845,#112846,#112847,#112848,#112849,#112850,#112851,
#112852,#112853,#112854,#112855,#112856,#112857,#112858,#112859,#112860,
#112861,#112862,#112863,#112864,#112865,#112866,#112867,#112868,#112869,
#112870,#112871,#112872,#112873,#112874,#112875,#112876,#112877,#112878,
#112879,#112880,#112881,#112882,#112883,#112884,#112885,#112886,#112887,
#112888,#112889,#112890,#112891,#112892,#112893,#112894,#112895,#112896,
#112897,#112898,#112899,#112900,#112901,#112902,#112903,#112904,#112905,
#112906,#112907,#112908,#112909,#112910,#112911,#112912,#112913,#112914,
#112915,#112916,#112917,#112918,#112919,#112920,#112921,#112922,#112923,
#112924,#112925,#112926,#112927)),.UNSPECIFIED.,.F.,.F.,.F.,(4,4),(4,1,
1,1,1,1,1,1,1,1,1,1,1,1,1,1,1,1,1,1,1,1,1,1,1,1,1,1,1,1,1,1,1,1,1,1,1,1,
1,1,1,1,1,1,1,1,1,1,1,1,1,1,1,1,1,1,1,1,1,1,1,1,1,1,1,1,1,1,1,1,1,1,1,1,
1,1,1,1,1,1,4),(0.,0.0296469363228873),(11.6151336144496,12.6096631819046,
13.6041927493596,14.5987223168147,15.5932518842697,16.5877814517247,17.5823110191797,
18.5768405866348,19.5713701540898,20.5658997215448,21.5604292889998,22.5549588564549,
23.5494884239099,24.5440179913649,25.53854755882,26.533077126275,27.52760669373,
28.522136261185,29.5166658286401,30.5111953960951,31.5057249635501,32.5002545310051,
33.4947840984602,34.4893136659152,35.4838432333702,36.4783728008253,37.4729023682803,
38.4674319357353,39.4619615031903,40.4564910706454,41.4510206381004,42.4455502055554,
43.4400797730104,44.4346093404655,45.4291389079205,46.4236684753755,47.4181980428306,
48.4127276102856,49.4072571777406,50.4017867451956,51.3963163126507,52.3908458801057,
53.3853754475607,54.3799050150157,55.3744345824708,56.3689641499258,57.3634937173808,
58.3580232848359,59.3525528522909,60.3470824197459,61.3416119872009,62.336141554656,
63.330671122111,64.325200689566,65.319730257021,66.3142598244761,67.3087893919311,
68.3033189593861,69.2978485268412,70.2923780942962,71.2869076617512,72.2814372292062,
73.2759667966613,74.2704963641163,75.2650259315713,76.2595554990263,77.2540850664814,
78.2486146339364,79.2431442013914,80.2376737688465,81.2322033363015,82.2267329037565,
83.2212624712115,84.2157920386666,85.2103216061216,86.2048511735766,87.1993807410316,
88.1939103084867,89.1884398759417,90.1829694433967,91.1774990108518),
 .UNSPECIFIED.);
#57125=ADVANCED_FACE('',(#4025),#56413,.F.);
#57126=ADVANCED_FACE('',(#4026),#56414,.F.);
#57127=ADVANCED_FACE('',(#4027),#56415,.F.);
#57128=ADVANCED_FACE('',(#4028),#56416,.F.);
#57129=ADVANCED_FACE('',(#4029),#56417,.F.);
#57130=ADVANCED_FACE('',(#4030),#56418,.F.);
#57131=ADVANCED_FACE('',(#4031),#56419,.F.);
#57132=ADVANCED_FACE('',(#4032),#56420,.F.);
#57133=ADVANCED_FACE('',(#4033),#56421,.F.);
#57134=ADVANCED_FACE('',(#4034),#56422,.F.);
#57135=ADVANCED_FACE('',(#4035),#56423,.F.);
#57136=ADVANCED_FACE('',(#4036),#56424,.F.);
#57137=ADVANCED_FACE('',(#4037),#56425,.F.);
#57138=ADVANCED_FACE('',(#4038),#56426,.F.);
#57139=ADVANCED_FACE('',(#4039),#56427,.F.);
#57140=ADVANCED_FACE('',(#4040),#56428,.F.);
#57141=ADVANCED_FACE('',(#4041),#56429,.F.);
#57142=ADVANCED_FACE('',(#4042),#56430,.F.);
#57143=ADVANCED_FACE('',(#4043),#56431,.F.);
#57144=ADVANCED_FACE('',(#4044),#56432,.F.);
#57145=ADVANCED_FACE('',(#4045,#1542),#1859,.T.);
#57146=ADVANCED_FACE('',(#4046),#56433,.F.);
#57147=ADVANCED_FACE('',(#4047),#56434,.F.);
#57148=ADVANCED_FACE('',(#4048),#56435,.F.);
#57149=ADVANCED_FACE('',(#4049),#56436,.F.);
#57150=ADVANCED_FACE('',(#4050),#56437,.F.);
#57151=ADVANCED_FACE('',(#4051),#56438,.F.);
#57152=ADVANCED_FACE('',(#4052),#56439,.F.);
#57153=ADVANCED_FACE('',(#4053),#56440,.F.);
#57154=ADVANCED_FACE('',(#4054),#56441,.F.);
#57155=ADVANCED_FACE('',(#4055),#56442,.F.);
#57156=ADVANCED_FACE('',(#4056),#56443,.F.);
#57157=ADVANCED_FACE('',(#4057),#56444,.F.);
#57158=ADVANCED_FACE('',(#4058),#56445,.F.);
#57159=ADVANCED_FACE('',(#4059),#56446,.F.);
#57160=ADVANCED_FACE('',(#4060),#56447,.F.);
#57161=ADVANCED_FACE('',(#4061),#56448,.F.);
#57162=ADVANCED_FACE('',(#4062),#56449,.F.);
#57163=ADVANCED_FACE('',(#4063),#56450,.F.);
#57164=ADVANCED_FACE('',(#4064),#56451,.F.);
#57165=ADVANCED_FACE('',(#4065),#56452,.F.);
#57166=ADVANCED_FACE('',(#4066),#56453,.F.);
#57167=ADVANCED_FACE('',(#4067),#56454,.F.);
#57168=ADVANCED_FACE('',(#4068),#56455,.F.);
#57169=ADVANCED_FACE('',(#4069),#56456,.F.);
#57170=ADVANCED_FACE('',(#4070),#56457,.F.);
#57171=ADVANCED_FACE('',(#4071),#56458,.F.);
#57172=ADVANCED_FACE('',(#4072),#56459,.F.);
#57173=ADVANCED_FACE('',(#4073),#56460,.F.);
#57174=ADVANCED_FACE('',(#4074),#1860,.F.);
#57175=ADVANCED_FACE('',(#4075),#56461,.F.);
#57176=ADVANCED_FACE('',(#4076,#1543),#1861,.T.);
#57177=ADVANCED_FACE('',(#4077),#1862,.T.);
#57178=ADVANCED_FACE('',(#4078),#1863,.T.);
#57179=ADVANCED_FACE('',(#4079),#56462,.F.);
#57180=ADVANCED_FACE('',(#4080),#56463,.F.);
#57181=ADVANCED_FACE('',(#4081),#56464,.F.);
#57182=ADVANCED_FACE('',(#4082),#56465,.F.);
#57183=ADVANCED_FACE('',(#4083),#56466,.F.);
#57184=ADVANCED_FACE('',(#4084),#56467,.F.);
#57185=ADVANCED_FACE('',(#4085),#56468,.F.);
#57186=ADVANCED_FACE('',(#4086),#56469,.F.);
#57187=ADVANCED_FACE('',(#4087),#56470,.F.);
#57188=ADVANCED_FACE('',(#4088),#56471,.F.);
#57189=ADVANCED_FACE('',(#4089),#56472,.F.);
#57190=ADVANCED_FACE('',(#4090),#56473,.F.);
#57191=ADVANCED_FACE('',(#4091),#56474,.F.);
#57192=ADVANCED_FACE('',(#4092),#56475,.F.);
#57193=ADVANCED_FACE('',(#4093),#56476,.F.);
#57194=ADVANCED_FACE('',(#4094),#56477,.F.);
#57195=ADVANCED_FACE('',(#4095),#56478,.F.);
#57196=ADVANCED_FACE('',(#4096),#56479,.F.);
#57197=ADVANCED_FACE('',(#4097),#56480,.F.);
#57198=ADVANCED_FACE('',(#4098),#56481,.F.);
#57199=ADVANCED_FACE('',(#4099,#1544),#1864,.T.);
#57200=ADVANCED_FACE('',(#4100),#56482,.F.);
#57201=ADVANCED_FACE('',(#4101),#56483,.F.);
#57202=ADVANCED_FACE('',(#4102),#56484,.F.);
#57203=ADVANCED_FACE('',(#4103),#56485,.F.);
#57204=ADVANCED_FACE('',(#4104),#56486,.F.);
#57205=ADVANCED_FACE('',(#4105),#56487,.F.);
#57206=ADVANCED_FACE('',(#4106),#56488,.F.);
#57207=ADVANCED_FACE('',(#4107),#56489,.F.);
#57208=ADVANCED_FACE('',(#4108),#56490,.F.);
#57209=ADVANCED_FACE('',(#4109),#56491,.F.);
#57210=ADVANCED_FACE('',(#4110),#56492,.F.);
#57211=ADVANCED_FACE('',(#4111),#56493,.F.);
#57212=ADVANCED_FACE('',(#4112),#56494,.F.);
#57213=ADVANCED_FACE('',(#4113),#56495,.F.);
#57214=ADVANCED_FACE('',(#4114),#56496,.F.);
#57215=ADVANCED_FACE('',(#4115),#56497,.F.);
#57216=ADVANCED_FACE('',(#4116),#56498,.F.);
#57217=ADVANCED_FACE('',(#4117),#56499,.F.);
#57218=ADVANCED_FACE('',(#4118),#56500,.F.);
#57219=ADVANCED_FACE('',(#4119),#56501,.F.);
#57220=ADVANCED_FACE('',(#4120),#56502,.F.);
#57221=ADVANCED_FACE('',(#4121),#56503,.F.);
#57222=ADVANCED_FACE('',(#4122),#56504,.F.);
#57223=ADVANCED_FACE('',(#4123),#56505,.F.);
#57224=ADVANCED_FACE('',(#4124),#56506,.F.);
#57225=ADVANCED_FACE('',(#4125),#56507,.F.);
#57226=ADVANCED_FACE('',(#4126),#56508,.F.);
#57227=ADVANCED_FACE('',(#4127),#56509,.F.);
#57228=ADVANCED_FACE('',(#4128),#56510,.F.);
#57229=ADVANCED_FACE('',(#4129),#56511,.F.);
#57230=ADVANCED_FACE('',(#4130),#56512,.F.);
#57231=ADVANCED_FACE('',(#4131),#56513,.F.);
#57232=ADVANCED_FACE('',(#4132),#56514,.F.);
#57233=ADVANCED_FACE('',(#4133,#1545,#1546),#1865,.T.);
#57234=ADVANCED_FACE('',(#4134),#1866,.T.);
#57235=ADVANCED_FACE('',(#4135),#1867,.T.);
#57236=ADVANCED_FACE('',(#4136),#1868,.T.);
#57237=ADVANCED_FACE('',(#4137),#56515,.F.);
#57238=ADVANCED_FACE('',(#4138),#56516,.F.);
#57239=ADVANCED_FACE('',(#4139),#56517,.F.);
#57240=ADVANCED_FACE('',(#4140),#56518,.F.);
#57241=ADVANCED_FACE('',(#4141),#56519,.F.);
#57242=ADVANCED_FACE('',(#4142),#56520,.F.);
#57243=ADVANCED_FACE('',(#4143),#56521,.F.);
#57244=ADVANCED_FACE('',(#4144),#56522,.F.);
#57245=ADVANCED_FACE('',(#4145),#56523,.F.);
#57246=ADVANCED_FACE('',(#4146),#56524,.F.);
#57247=ADVANCED_FACE('',(#4147),#56525,.F.);
#57248=ADVANCED_FACE('',(#4148),#56526,.F.);
#57249=ADVANCED_FACE('',(#4149),#56527,.F.);
#57250=ADVANCED_FACE('',(#4150),#56528,.F.);
#57251=ADVANCED_FACE('',(#4151),#56529,.F.);
#57252=ADVANCED_FACE('',(#4152),#56530,.F.);
#57253=ADVANCED_FACE('',(#4153),#56531,.F.);
#57254=ADVANCED_FACE('',(#4154),#56532,.F.);
#57255=ADVANCED_FACE('',(#4155),#56533,.F.);
#57256=ADVANCED_FACE('',(#4156),#56534,.F.);
#57257=ADVANCED_FACE('',(#4157,#1547),#1869,.T.);
#57258=ADVANCED_FACE('',(#4158),#56535,.F.);
#57259=ADVANCED_FACE('',(#4159),#56536,.F.);
#57260=ADVANCED_FACE('',(#4160),#56537,.F.);
#57261=ADVANCED_FACE('',(#4161),#1870,.F.);
#57262=ADVANCED_FACE('',(#4162),#56538,.F.);
#57263=ADVANCED_FACE('',(#4163),#56539,.F.);
#57264=ADVANCED_FACE('',(#4164),#56540,.F.);
#57265=ADVANCED_FACE('',(#4165),#1871,.F.);
#57266=ADVANCED_FACE('',(#4166),#1872,.F.);
#57267=ADVANCED_FACE('',(#4167),#1873,.F.);
#57268=ADVANCED_FACE('',(#4168),#1874,.F.);
#57269=ADVANCED_FACE('',(#4169),#1875,.T.);
#57270=ADVANCED_FACE('',(#4170),#1876,.T.);
#57271=ADVANCED_FACE('',(#4171),#56541,.F.);
#57272=ADVANCED_FACE('',(#4172),#56542,.F.);
#57273=ADVANCED_FACE('',(#4173),#56543,.F.);
#57274=ADVANCED_FACE('',(#4174),#56544,.F.);
#57275=ADVANCED_FACE('',(#4175),#56545,.F.);
#57276=ADVANCED_FACE('',(#4176),#56546,.F.);
#57277=ADVANCED_FACE('',(#4177),#56547,.F.);
#57278=ADVANCED_FACE('',(#4178),#56548,.F.);
#57279=ADVANCED_FACE('',(#4179),#56549,.F.);
#57280=ADVANCED_FACE('',(#4180),#56550,.F.);
#57281=ADVANCED_FACE('',(#4181),#56551,.F.);
#57282=ADVANCED_FACE('',(#4182),#56552,.F.);
#57283=ADVANCED_FACE('',(#4183),#56553,.F.);
#57284=ADVANCED_FACE('',(#4184),#56554,.F.);
#57285=ADVANCED_FACE('',(#4185),#56555,.F.);
#57286=ADVANCED_FACE('',(#4186),#56556,.F.);
#57287=ADVANCED_FACE('',(#4187),#56557,.F.);
#57288=ADVANCED_FACE('',(#4188),#56558,.F.);
#57289=ADVANCED_FACE('',(#4189),#56559,.F.);
#57290=ADVANCED_FACE('',(#4190),#56560,.F.);
#57291=ADVANCED_FACE('',(#4191,#1548),#1877,.T.);
#57292=ADVANCED_FACE('',(#4192),#56561,.F.);
#57293=ADVANCED_FACE('',(#4193),#56562,.F.);
#57294=ADVANCED_FACE('',(#4194),#56563,.F.);
#57295=ADVANCED_FACE('',(#4195),#56564,.F.);
#57296=ADVANCED_FACE('',(#4196),#56565,.F.);
#57297=ADVANCED_FACE('',(#4197),#56566,.F.);
#57298=ADVANCED_FACE('',(#4198),#56567,.F.);
#57299=ADVANCED_FACE('',(#4199),#56568,.F.);
#57300=ADVANCED_FACE('',(#4200),#56569,.F.);
#57301=ADVANCED_FACE('',(#4201),#56570,.F.);
#57302=ADVANCED_FACE('',(#4202),#56571,.F.);
#57303=ADVANCED_FACE('',(#4203),#56572,.F.);
#57304=ADVANCED_FACE('',(#4204),#56573,.F.);
#57305=ADVANCED_FACE('',(#4205),#56574,.F.);
#57306=ADVANCED_FACE('',(#4206),#56575,.F.);
#57307=ADVANCED_FACE('',(#4207),#56576,.F.);
#57308=ADVANCED_FACE('',(#4208),#56577,.F.);
#57309=ADVANCED_FACE('',(#4209),#56578,.F.);
#57310=ADVANCED_FACE('',(#4210),#56579,.F.);
#57311=ADVANCED_FACE('',(#4211),#56580,.F.);
#57312=ADVANCED_FACE('',(#4212),#56581,.F.);
#57313=ADVANCED_FACE('',(#4213),#56582,.F.);
#57314=ADVANCED_FACE('',(#4214),#56583,.F.);
#57315=ADVANCED_FACE('',(#4215),#56584,.F.);
#57316=ADVANCED_FACE('',(#4216),#56585,.F.);
#57317=ADVANCED_FACE('',(#4217),#56586,.F.);
#57318=ADVANCED_FACE('',(#4218),#1878,.F.);
#57319=ADVANCED_FACE('',(#4219),#56587,.F.);
#57320=ADVANCED_FACE('',(#4220,#1549),#1879,.T.);
#57321=ADVANCED_FACE('',(#4221),#1880,.T.);
#57322=ADVANCED_FACE('',(#4222),#1881,.T.);
#57323=ADVANCED_FACE('',(#4223),#56588,.F.);
#57324=ADVANCED_FACE('',(#4224),#56589,.F.);
#57325=ADVANCED_FACE('',(#4225),#56590,.F.);
#57326=ADVANCED_FACE('',(#4226),#56591,.F.);
#57327=ADVANCED_FACE('',(#4227),#56592,.F.);
#57328=ADVANCED_FACE('',(#4228),#56593,.F.);
#57329=ADVANCED_FACE('',(#4229),#56594,.F.);
#57330=ADVANCED_FACE('',(#4230),#56595,.F.);
#57331=ADVANCED_FACE('',(#4231),#56596,.F.);
#57332=ADVANCED_FACE('',(#4232),#56597,.F.);
#57333=ADVANCED_FACE('',(#4233),#56598,.F.);
#57334=ADVANCED_FACE('',(#4234),#56599,.F.);
#57335=ADVANCED_FACE('',(#4235),#56600,.F.);
#57336=ADVANCED_FACE('',(#4236),#56601,.F.);
#57337=ADVANCED_FACE('',(#4237),#56602,.F.);
#57338=ADVANCED_FACE('',(#4238),#56603,.F.);
#57339=ADVANCED_FACE('',(#4239),#56604,.F.);
#57340=ADVANCED_FACE('',(#4240),#56605,.F.);
#57341=ADVANCED_FACE('',(#4241),#56606,.F.);
#57342=ADVANCED_FACE('',(#4242),#56607,.F.);
#57343=ADVANCED_FACE('',(#4243,#1550),#1882,.T.);
#57344=ADVANCED_FACE('',(#4244),#56608,.F.);
#57345=ADVANCED_FACE('',(#4245),#56609,.F.);
#57346=ADVANCED_FACE('',(#4246),#56610,.F.);
#57347=ADVANCED_FACE('',(#4247),#56611,.F.);
#57348=ADVANCED_FACE('',(#4248),#56612,.F.);
#57349=ADVANCED_FACE('',(#4249),#56613,.F.);
#57350=ADVANCED_FACE('',(#4250),#1883,.F.);
#57351=ADVANCED_FACE('',(#4251),#1884,.F.);
#57352=ADVANCED_FACE('',(#4252),#1885,.F.);
#57353=ADVANCED_FACE('',(#4253),#1886,.F.);
#57354=ADVANCED_FACE('',(#4254),#1887,.F.);
#57355=ADVANCED_FACE('',(#4255),#1888,.F.);
#57356=ADVANCED_FACE('',(#4256),#56614,.F.);
#57357=ADVANCED_FACE('',(#4257),#56615,.F.);
#57358=ADVANCED_FACE('',(#4258),#56616,.F.);
#57359=ADVANCED_FACE('',(#4259),#56617,.F.);
#57360=ADVANCED_FACE('',(#4260),#56618,.F.);
#57361=ADVANCED_FACE('',(#4261),#56619,.F.);
#57362=ADVANCED_FACE('',(#4262),#56620,.F.);
#57363=ADVANCED_FACE('',(#4263),#56621,.F.);
#57364=ADVANCED_FACE('',(#4264),#1889,.F.);
#57365=ADVANCED_FACE('',(#4265),#56622,.F.);
#57366=ADVANCED_FACE('',(#4266),#1890,.T.);
#57367=ADVANCED_FACE('',(#4267),#1891,.T.);
#57368=ADVANCED_FACE('',(#4268),#56623,.F.);
#57369=ADVANCED_FACE('',(#4269),#56624,.F.);
#57370=ADVANCED_FACE('',(#4270),#56625,.F.);
#57371=ADVANCED_FACE('',(#4271),#56626,.F.);
#57372=ADVANCED_FACE('',(#4272),#56627,.F.);
#57373=ADVANCED_FACE('',(#4273),#56628,.F.);
#57374=ADVANCED_FACE('',(#4274),#56629,.F.);
#57375=ADVANCED_FACE('',(#4275),#56630,.F.);
#57376=ADVANCED_FACE('',(#4276),#56631,.F.);
#57377=ADVANCED_FACE('',(#4277),#56632,.F.);
#57378=ADVANCED_FACE('',(#4278),#56633,.F.);
#57379=ADVANCED_FACE('',(#4279),#56634,.F.);
#57380=ADVANCED_FACE('',(#4280),#56635,.F.);
#57381=ADVANCED_FACE('',(#4281),#56636,.F.);
#57382=ADVANCED_FACE('',(#4282),#56637,.F.);
#57383=ADVANCED_FACE('',(#4283),#56638,.F.);
#57384=ADVANCED_FACE('',(#4284),#56639,.F.);
#57385=ADVANCED_FACE('',(#4285),#56640,.F.);
#57386=ADVANCED_FACE('',(#4286),#56641,.F.);
#57387=ADVANCED_FACE('',(#4287),#56642,.F.);
#57388=ADVANCED_FACE('',(#4288,#1551),#1892,.T.);
#57389=ADVANCED_FACE('',(#4289),#1893,.F.);
#57390=ADVANCED_FACE('',(#4290),#1894,.F.);
#57391=ADVANCED_FACE('',(#4291),#1895,.F.);
#57392=ADVANCED_FACE('',(#4292),#1896,.F.);
#57393=ADVANCED_FACE('',(#4293),#1897,.F.);
#57394=ADVANCED_FACE('',(#4294),#1898,.F.);
#57395=ADVANCED_FACE('',(#4295),#1899,.F.);
#57396=ADVANCED_FACE('',(#4296),#1900,.F.);
#57397=ADVANCED_FACE('',(#4297),#1901,.F.);
#57398=ADVANCED_FACE('',(#4298),#1902,.F.);
#57399=ADVANCED_FACE('',(#4299),#1903,.F.);
#57400=ADVANCED_FACE('',(#4300),#1904,.F.);
#57401=ADVANCED_FACE('',(#4301),#1905,.F.);
#57402=ADVANCED_FACE('',(#4302),#1906,.F.);
#57403=ADVANCED_FACE('',(#4303,#1552),#1907,.F.);
#57404=ADVANCED_FACE('',(#4304),#1908,.T.);
#57405=ADVANCED_FACE('',(#4305),#1909,.T.);
#57406=ADVANCED_FACE('',(#4306),#56643,.F.);
#57407=ADVANCED_FACE('',(#4307),#56644,.F.);
#57408=ADVANCED_FACE('',(#4308),#56645,.F.);
#57409=ADVANCED_FACE('',(#4309),#56646,.F.);
#57410=ADVANCED_FACE('',(#4310),#56647,.F.);
#57411=ADVANCED_FACE('',(#4311),#56648,.F.);
#57412=ADVANCED_FACE('',(#4312),#56649,.F.);
#57413=ADVANCED_FACE('',(#4313),#56650,.F.);
#57414=ADVANCED_FACE('',(#4314),#56651,.F.);
#57415=ADVANCED_FACE('',(#4315),#56652,.F.);
#57416=ADVANCED_FACE('',(#4316),#56653,.F.);
#57417=ADVANCED_FACE('',(#4317),#56654,.F.);
#57418=ADVANCED_FACE('',(#4318),#56655,.F.);
#57419=ADVANCED_FACE('',(#4319),#56656,.F.);
#57420=ADVANCED_FACE('',(#4320),#56657,.F.);
#57421=ADVANCED_FACE('',(#4321),#56658,.F.);
#57422=ADVANCED_FACE('',(#4322),#56659,.F.);
#57423=ADVANCED_FACE('',(#4323),#56660,.F.);
#57424=ADVANCED_FACE('',(#4324),#56661,.F.);
#57425=ADVANCED_FACE('',(#4325),#56662,.F.);
#57426=ADVANCED_FACE('',(#4326,#1553),#1910,.T.);
#57427=ADVANCED_FACE('',(#4327),#56663,.F.);
#57428=ADVANCED_FACE('',(#4328),#56664,.F.);
#57429=ADVANCED_FACE('',(#4329),#56665,.F.);
#57430=ADVANCED_FACE('',(#4330),#56666,.F.);
#57431=ADVANCED_FACE('',(#4331),#56667,.F.);
#57432=ADVANCED_FACE('',(#4332),#56668,.F.);
#57433=ADVANCED_FACE('',(#4333),#56669,.F.);
#57434=ADVANCED_FACE('',(#4334),#56670,.F.);
#57435=ADVANCED_FACE('',(#4335),#56671,.F.);
#57436=ADVANCED_FACE('',(#4336),#56672,.F.);
#57437=ADVANCED_FACE('',(#4337),#56673,.F.);
#57438=ADVANCED_FACE('',(#4338),#56674,.F.);
#57439=ADVANCED_FACE('',(#4339),#1911,.F.);
#57440=ADVANCED_FACE('',(#4340),#56675,.F.);
#57441=ADVANCED_FACE('',(#4341),#56676,.F.);
#57442=ADVANCED_FACE('',(#4342),#56677,.F.);
#57443=ADVANCED_FACE('',(#4343),#56678,.F.);
#57444=ADVANCED_FACE('',(#4344),#56679,.F.);
#57445=ADVANCED_FACE('',(#4345),#56680,.F.);
#57446=ADVANCED_FACE('',(#4346),#56681,.F.);
#57447=ADVANCED_FACE('',(#4347),#1912,.F.);
#57448=ADVANCED_FACE('',(#4348),#56682,.F.);
#57449=ADVANCED_FACE('',(#4349),#56683,.F.);
#57450=ADVANCED_FACE('',(#4350),#56684,.F.);
#57451=ADVANCED_FACE('',(#4351),#56685,.F.);
#57452=ADVANCED_FACE('',(#4352),#56686,.F.);
#57453=ADVANCED_FACE('',(#4353),#56687,.F.);
#57454=ADVANCED_FACE('',(#4354),#56688,.F.);
#57455=ADVANCED_FACE('',(#4355),#1913,.F.);
#57456=ADVANCED_FACE('',(#4356),#56689,.F.);
#57457=ADVANCED_FACE('',(#4357),#1914,.T.);
#57458=ADVANCED_FACE('',(#4358),#1915,.T.);
#57459=ADVANCED_FACE('',(#4359),#56690,.F.);
#57460=ADVANCED_FACE('',(#4360),#56691,.F.);
#57461=ADVANCED_FACE('',(#4361),#56692,.F.);
#57462=ADVANCED_FACE('',(#4362),#56693,.F.);
#57463=ADVANCED_FACE('',(#4363),#56694,.F.);
#57464=ADVANCED_FACE('',(#4364),#56695,.F.);
#57465=ADVANCED_FACE('',(#4365),#56696,.F.);
#57466=ADVANCED_FACE('',(#4366),#56697,.F.);
#57467=ADVANCED_FACE('',(#4367),#56698,.F.);
#57468=ADVANCED_FACE('',(#4368),#56699,.F.);
#57469=ADVANCED_FACE('',(#4369),#56700,.F.);
#57470=ADVANCED_FACE('',(#4370),#56701,.F.);
#57471=ADVANCED_FACE('',(#4371),#56702,.F.);
#57472=ADVANCED_FACE('',(#4372),#56703,.F.);
#57473=ADVANCED_FACE('',(#4373),#56704,.F.);
#57474=ADVANCED_FACE('',(#4374),#56705,.F.);
#57475=ADVANCED_FACE('',(#4375),#56706,.F.);
#57476=ADVANCED_FACE('',(#4376),#56707,.F.);
#57477=ADVANCED_FACE('',(#4377),#56708,.F.);
#57478=ADVANCED_FACE('',(#4378),#56709,.F.);
#57479=ADVANCED_FACE('',(#4379,#1554),#1916,.T.);
#57480=ADVANCED_FACE('',(#4380),#56710,.F.);
#57481=ADVANCED_FACE('',(#4381),#56711,.F.);
#57482=ADVANCED_FACE('',(#4382),#56712,.F.);
#57483=ADVANCED_FACE('',(#4383),#56713,.F.);
#57484=ADVANCED_FACE('',(#4384),#56714,.F.);
#57485=ADVANCED_FACE('',(#4385),#56715,.F.);
#57486=ADVANCED_FACE('',(#4386),#56716,.F.);
#57487=ADVANCED_FACE('',(#4387),#56717,.F.);
#57488=ADVANCED_FACE('',(#4388),#56718,.F.);
#57489=ADVANCED_FACE('',(#4389),#1917,.F.);
#57490=ADVANCED_FACE('',(#4390),#56719,.F.);
#57491=ADVANCED_FACE('',(#4391),#56720,.F.);
#57492=ADVANCED_FACE('',(#4392),#56721,.F.);
#57493=ADVANCED_FACE('',(#4393),#56722,.F.);
#57494=ADVANCED_FACE('',(#4394),#56723,.F.);
#57495=ADVANCED_FACE('',(#4395),#56724,.F.);
#57496=ADVANCED_FACE('',(#4396),#56725,.F.);
#57497=ADVANCED_FACE('',(#4397),#56726,.F.);
#57498=ADVANCED_FACE('',(#4398),#56727,.F.);
#57499=ADVANCED_FACE('',(#4399),#1918,.F.);
#57500=ADVANCED_FACE('',(#4400),#1919,.F.);
#57501=ADVANCED_FACE('',(#4401),#1920,.F.);
#57502=ADVANCED_FACE('',(#4402),#1921,.T.);
#57503=ADVANCED_FACE('',(#4403),#1922,.T.);
#57504=ADVANCED_FACE('',(#4404),#56728,.F.);
#57505=ADVANCED_FACE('',(#4405),#56729,.F.);
#57506=ADVANCED_FACE('',(#4406),#56730,.F.);
#57507=ADVANCED_FACE('',(#4407),#56731,.F.);
#57508=ADVANCED_FACE('',(#4408),#56732,.F.);
#57509=ADVANCED_FACE('',(#4409),#56733,.F.);
#57510=ADVANCED_FACE('',(#4410),#56734,.F.);
#57511=ADVANCED_FACE('',(#4411),#56735,.F.);
#57512=ADVANCED_FACE('',(#4412),#56736,.F.);
#57513=ADVANCED_FACE('',(#4413),#56737,.F.);
#57514=ADVANCED_FACE('',(#4414),#56738,.F.);
#57515=ADVANCED_FACE('',(#4415),#56739,.F.);
#57516=ADVANCED_FACE('',(#4416),#56740,.F.);
#57517=ADVANCED_FACE('',(#4417),#56741,.F.);
#57518=ADVANCED_FACE('',(#4418),#56742,.F.);
#57519=ADVANCED_FACE('',(#4419),#56743,.F.);
#57520=ADVANCED_FACE('',(#4420),#56744,.F.);
#57521=ADVANCED_FACE('',(#4421),#56745,.F.);
#57522=ADVANCED_FACE('',(#4422),#56746,.F.);
#57523=ADVANCED_FACE('',(#4423),#56747,.F.);
#57524=ADVANCED_FACE('',(#4424,#1555),#1923,.T.);
#57525=ADVANCED_FACE('',(#4425),#1924,.F.);
#57526=ADVANCED_FACE('',(#4426),#56748,.F.);
#57527=ADVANCED_FACE('',(#4427),#56749,.F.);
#57528=ADVANCED_FACE('',(#4428),#1925,.F.);
#57529=ADVANCED_FACE('',(#4429),#56750,.F.);
#57530=ADVANCED_FACE('',(#4430),#56751,.F.);
#57531=ADVANCED_FACE('',(#4431),#1926,.F.);
#57532=ADVANCED_FACE('',(#4432),#1927,.F.);
#57533=ADVANCED_FACE('',(#4433),#1928,.F.);
#57534=ADVANCED_FACE('',(#4434),#1929,.T.);
#57535=ADVANCED_FACE('',(#4435),#1930,.T.);
#57536=ADVANCED_FACE('',(#4436),#56752,.F.);
#57537=ADVANCED_FACE('',(#4437),#56753,.F.);
#57538=ADVANCED_FACE('',(#4438),#56754,.F.);
#57539=ADVANCED_FACE('',(#4439),#56755,.F.);
#57540=ADVANCED_FACE('',(#4440),#56756,.F.);
#57541=ADVANCED_FACE('',(#4441),#56757,.F.);
#57542=ADVANCED_FACE('',(#4442),#56758,.F.);
#57543=ADVANCED_FACE('',(#4443),#56759,.F.);
#57544=ADVANCED_FACE('',(#4444),#56760,.F.);
#57545=ADVANCED_FACE('',(#4445),#56761,.F.);
#57546=ADVANCED_FACE('',(#4446),#56762,.F.);
#57547=ADVANCED_FACE('',(#4447),#56763,.F.);
#57548=ADVANCED_FACE('',(#4448),#56764,.F.);
#57549=ADVANCED_FACE('',(#4449),#56765,.F.);
#57550=ADVANCED_FACE('',(#4450),#56766,.F.);
#57551=ADVANCED_FACE('',(#4451),#56767,.F.);
#57552=ADVANCED_FACE('',(#4452),#56768,.F.);
#57553=ADVANCED_FACE('',(#4453),#56769,.F.);
#57554=ADVANCED_FACE('',(#4454),#56770,.F.);
#57555=ADVANCED_FACE('',(#4455),#56771,.F.);
#57556=ADVANCED_FACE('',(#4456,#1556),#1931,.T.);
#57557=ADVANCED_FACE('',(#4457),#1932,.T.);
#57558=ADVANCED_FACE('',(#4458),#56772,.F.);
#57559=ADVANCED_FACE('',(#4459),#56773,.F.);
#57560=ADVANCED_FACE('',(#4460),#56774,.F.);
#57561=ADVANCED_FACE('',(#4461),#56775,.F.);
#57562=ADVANCED_FACE('',(#4462),#56776,.F.);
#57563=ADVANCED_FACE('',(#4463),#56777,.F.);
#57564=ADVANCED_FACE('',(#4464),#56778,.F.);
#57565=ADVANCED_FACE('',(#4465),#56779,.F.);
#57566=ADVANCED_FACE('',(#4466),#56780,.F.);
#57567=ADVANCED_FACE('',(#4467),#56781,.F.);
#57568=ADVANCED_FACE('',(#4468),#56782,.F.);
#57569=ADVANCED_FACE('',(#4469),#56783,.F.);
#57570=ADVANCED_FACE('',(#4470),#56784,.F.);
#57571=ADVANCED_FACE('',(#4471),#56785,.F.);
#57572=ADVANCED_FACE('',(#4472),#56786,.F.);
#57573=ADVANCED_FACE('',(#4473),#56787,.F.);
#57574=ADVANCED_FACE('',(#4474),#56788,.F.);
#57575=ADVANCED_FACE('',(#4475),#56789,.F.);
#57576=ADVANCED_FACE('',(#4476),#56790,.F.);
#57577=ADVANCED_FACE('',(#4477),#56791,.F.);
#57578=ADVANCED_FACE('',(#4478,#1557),#1933,.T.);
#57579=ADVANCED_FACE('',(#4479),#1934,.F.);
#57580=ADVANCED_FACE('',(#4480),#56792,.F.);
#57581=ADVANCED_FACE('',(#4481),#56793,.F.);
#57582=ADVANCED_FACE('',(#4482),#1935,.F.);
#57583=ADVANCED_FACE('',(#4483),#56794,.F.);
#57584=ADVANCED_FACE('',(#4484),#56795,.F.);
#57585=ADVANCED_FACE('',(#4485),#1936,.F.);
#57586=ADVANCED_FACE('',(#4486),#1937,.F.);
#57587=ADVANCED_FACE('',(#4487),#1938,.F.);
#57588=ADVANCED_FACE('',(#4488),#1939,.T.);
#57589=ADVANCED_FACE('',(#4489),#1940,.T.);
#57590=ADVANCED_FACE('',(#4490),#56796,.F.);
#57591=ADVANCED_FACE('',(#4491),#56797,.F.);
#57592=ADVANCED_FACE('',(#4492),#56798,.F.);
#57593=ADVANCED_FACE('',(#4493),#56799,.F.);
#57594=ADVANCED_FACE('',(#4494),#56800,.F.);
#57595=ADVANCED_FACE('',(#4495),#56801,.F.);
#57596=ADVANCED_FACE('',(#4496),#56802,.F.);
#57597=ADVANCED_FACE('',(#4497),#56803,.F.);
#57598=ADVANCED_FACE('',(#4498),#56804,.F.);
#57599=ADVANCED_FACE('',(#4499),#56805,.F.);
#57600=ADVANCED_FACE('',(#4500),#56806,.F.);
#57601=ADVANCED_FACE('',(#4501),#56807,.F.);
#57602=ADVANCED_FACE('',(#4502),#56808,.F.);
#57603=ADVANCED_FACE('',(#4503),#56809,.F.);
#57604=ADVANCED_FACE('',(#4504),#56810,.F.);
#57605=ADVANCED_FACE('',(#4505),#56811,.F.);
#57606=ADVANCED_FACE('',(#4506),#56812,.F.);
#57607=ADVANCED_FACE('',(#4507),#56813,.F.);
#57608=ADVANCED_FACE('',(#4508),#56814,.F.);
#57609=ADVANCED_FACE('',(#4509),#56815,.F.);
#57610=ADVANCED_FACE('',(#4510,#1558),#1941,.T.);
#57611=ADVANCED_FACE('',(#4511),#56816,.F.);
#57612=ADVANCED_FACE('',(#4512),#56817,.F.);
#57613=ADVANCED_FACE('',(#4513),#56818,.F.);
#57614=ADVANCED_FACE('',(#4514),#56819,.F.);
#57615=ADVANCED_FACE('',(#4515),#56820,.F.);
#57616=ADVANCED_FACE('',(#4516),#56821,.F.);
#57617=ADVANCED_FACE('',(#4517),#56822,.F.);
#57618=ADVANCED_FACE('',(#4518),#56823,.F.);
#57619=ADVANCED_FACE('',(#4519),#56824,.F.);
#57620=ADVANCED_FACE('',(#4520),#1942,.F.);
#57621=ADVANCED_FACE('',(#4521),#56825,.F.);
#57622=ADVANCED_FACE('',(#4522),#56826,.F.);
#57623=ADVANCED_FACE('',(#4523),#56827,.F.);
#57624=ADVANCED_FACE('',(#4524),#56828,.F.);
#57625=ADVANCED_FACE('',(#4525),#56829,.F.);
#57626=ADVANCED_FACE('',(#4526),#56830,.F.);
#57627=ADVANCED_FACE('',(#4527),#56831,.F.);
#57628=ADVANCED_FACE('',(#4528),#56832,.F.);
#57629=ADVANCED_FACE('',(#4529),#56833,.F.);
#57630=ADVANCED_FACE('',(#4530),#1943,.F.);
#57631=ADVANCED_FACE('',(#4531),#1944,.F.);
#57632=ADVANCED_FACE('',(#4532),#1945,.F.);
#57633=ADVANCED_FACE('',(#4533),#1946,.T.);
#57634=ADVANCED_FACE('',(#4534),#1947,.T.);
#57635=ADVANCED_FACE('',(#4535),#56834,.F.);
#57636=ADVANCED_FACE('',(#4536),#56835,.F.);
#57637=ADVANCED_FACE('',(#4537),#56836,.F.);
#57638=ADVANCED_FACE('',(#4538),#56837,.F.);
#57639=ADVANCED_FACE('',(#4539),#56838,.F.);
#57640=ADVANCED_FACE('',(#4540),#56839,.F.);
#57641=ADVANCED_FACE('',(#4541),#56840,.F.);
#57642=ADVANCED_FACE('',(#4542),#56841,.F.);
#57643=ADVANCED_FACE('',(#4543),#56842,.F.);
#57644=ADVANCED_FACE('',(#4544),#56843,.F.);
#57645=ADVANCED_FACE('',(#4545),#56844,.F.);
#57646=ADVANCED_FACE('',(#4546),#56845,.F.);
#57647=ADVANCED_FACE('',(#4547),#56846,.F.);
#57648=ADVANCED_FACE('',(#4548),#56847,.F.);
#57649=ADVANCED_FACE('',(#4549),#56848,.F.);
#57650=ADVANCED_FACE('',(#4550),#56849,.F.);
#57651=ADVANCED_FACE('',(#4551),#56850,.F.);
#57652=ADVANCED_FACE('',(#4552),#56851,.F.);
#57653=ADVANCED_FACE('',(#4553),#56852,.F.);
#57654=ADVANCED_FACE('',(#4554),#56853,.F.);
#57655=ADVANCED_FACE('',(#4555,#1559),#1948,.T.);
#57656=ADVANCED_FACE('',(#4556),#56854,.F.);
#57657=ADVANCED_FACE('',(#4557),#56855,.F.);
#57658=ADVANCED_FACE('',(#4558),#56856,.F.);
#57659=ADVANCED_FACE('',(#4559),#56857,.F.);
#57660=ADVANCED_FACE('',(#4560),#56858,.F.);
#57661=ADVANCED_FACE('',(#4561),#56859,.F.);
#57662=ADVANCED_FACE('',(#4562),#56860,.F.);
#57663=ADVANCED_FACE('',(#4563),#56861,.F.);
#57664=ADVANCED_FACE('',(#4564),#56862,.F.);
#57665=ADVANCED_FACE('',(#4565),#56863,.F.);
#57666=ADVANCED_FACE('',(#4566),#56864,.F.);
#57667=ADVANCED_FACE('',(#4567),#56865,.F.);
#57668=ADVANCED_FACE('',(#4568),#1949,.F.);
#57669=ADVANCED_FACE('',(#4569),#56866,.F.);
#57670=ADVANCED_FACE('',(#4570),#56867,.F.);
#57671=ADVANCED_FACE('',(#4571),#56868,.F.);
#57672=ADVANCED_FACE('',(#4572),#56869,.F.);
#57673=ADVANCED_FACE('',(#4573),#56870,.F.);
#57674=ADVANCED_FACE('',(#4574),#56871,.F.);
#57675=ADVANCED_FACE('',(#4575),#56872,.F.);
#57676=ADVANCED_FACE('',(#4576),#1950,.F.);
#57677=ADVANCED_FACE('',(#4577),#56873,.F.);
#57678=ADVANCED_FACE('',(#4578),#56874,.F.);
#57679=ADVANCED_FACE('',(#4579),#56875,.F.);
#57680=ADVANCED_FACE('',(#4580),#56876,.F.);
#57681=ADVANCED_FACE('',(#4581),#56877,.F.);
#57682=ADVANCED_FACE('',(#4582),#56878,.F.);
#57683=ADVANCED_FACE('',(#4583),#56879,.F.);
#57684=ADVANCED_FACE('',(#4584),#1951,.F.);
#57685=ADVANCED_FACE('',(#4585),#56880,.F.);
#57686=ADVANCED_FACE('',(#4586),#1952,.T.);
#57687=ADVANCED_FACE('',(#4587),#1953,.T.);
#57688=ADVANCED_FACE('',(#4588),#56881,.F.);
#57689=ADVANCED_FACE('',(#4589),#56882,.F.);
#57690=ADVANCED_FACE('',(#4590),#56883,.F.);
#57691=ADVANCED_FACE('',(#4591),#56884,.F.);
#57692=ADVANCED_FACE('',(#4592),#56885,.F.);
#57693=ADVANCED_FACE('',(#4593),#56886,.F.);
#57694=ADVANCED_FACE('',(#4594),#56887,.F.);
#57695=ADVANCED_FACE('',(#4595),#56888,.F.);
#57696=ADVANCED_FACE('',(#4596),#56889,.F.);
#57697=ADVANCED_FACE('',(#4597),#56890,.F.);
#57698=ADVANCED_FACE('',(#4598),#56891,.F.);
#57699=ADVANCED_FACE('',(#4599),#56892,.F.);
#57700=ADVANCED_FACE('',(#4600),#56893,.F.);
#57701=ADVANCED_FACE('',(#4601),#56894,.F.);
#57702=ADVANCED_FACE('',(#4602),#56895,.F.);
#57703=ADVANCED_FACE('',(#4603),#56896,.F.);
#57704=ADVANCED_FACE('',(#4604),#56897,.F.);
#57705=ADVANCED_FACE('',(#4605),#56898,.F.);
#57706=ADVANCED_FACE('',(#4606),#56899,.F.);
#57707=ADVANCED_FACE('',(#4607),#56900,.F.);
#57708=ADVANCED_FACE('',(#4608,#1560),#1954,.T.);
#57709=ADVANCED_FACE('',(#4609),#1955,.F.);
#57710=ADVANCED_FACE('',(#4610),#1956,.F.);
#57711=ADVANCED_FACE('',(#4611),#1957,.F.);
#57712=ADVANCED_FACE('',(#4612),#1958,.F.);
#57713=ADVANCED_FACE('',(#4613),#1959,.F.);
#57714=ADVANCED_FACE('',(#4614),#1960,.F.);
#57715=ADVANCED_FACE('',(#4615),#1961,.F.);
#57716=ADVANCED_FACE('',(#4616),#1962,.F.);
#57717=ADVANCED_FACE('',(#4617),#1963,.F.);
#57718=ADVANCED_FACE('',(#4618),#1964,.F.);
#57719=ADVANCED_FACE('',(#4619),#1965,.F.);
#57720=ADVANCED_FACE('',(#4620),#1966,.F.);
#57721=ADVANCED_FACE('',(#4621),#1967,.F.);
#57722=ADVANCED_FACE('',(#4622),#1968,.F.);
#57723=ADVANCED_FACE('',(#4623,#1561),#1969,.F.);
#57724=ADVANCED_FACE('',(#4624),#1970,.T.);
#57725=ADVANCED_FACE('',(#4625),#1971,.T.);
#57726=ADVANCED_FACE('',(#4626),#56901,.F.);
#57727=ADVANCED_FACE('',(#4627),#56902,.F.);
#57728=ADVANCED_FACE('',(#4628),#56903,.F.);
#57729=ADVANCED_FACE('',(#4629),#56904,.F.);
#57730=ADVANCED_FACE('',(#4630),#56905,.F.);
#57731=ADVANCED_FACE('',(#4631),#56906,.F.);
#57732=ADVANCED_FACE('',(#4632),#56907,.F.);
#57733=ADVANCED_FACE('',(#4633),#56908,.F.);
#57734=ADVANCED_FACE('',(#4634),#56909,.F.);
#57735=ADVANCED_FACE('',(#4635),#56910,.F.);
#57736=ADVANCED_FACE('',(#4636),#56911,.F.);
#57737=ADVANCED_FACE('',(#4637),#56912,.F.);
#57738=ADVANCED_FACE('',(#4638),#56913,.F.);
#57739=ADVANCED_FACE('',(#4639),#56914,.F.);
#57740=ADVANCED_FACE('',(#4640),#56915,.F.);
#57741=ADVANCED_FACE('',(#4641),#56916,.F.);
#57742=ADVANCED_FACE('',(#4642),#56917,.F.);
#57743=ADVANCED_FACE('',(#4643),#56918,.F.);
#57744=ADVANCED_FACE('',(#4644),#56919,.F.);
#57745=ADVANCED_FACE('',(#4645),#56920,.F.);
#57746=ADVANCED_FACE('',(#4646,#1562),#1972,.T.);
#57747=ADVANCED_FACE('',(#4647),#56921,.F.);
#57748=ADVANCED_FACE('',(#4648),#56922,.F.);
#57749=ADVANCED_FACE('',(#4649),#56923,.F.);
#57750=ADVANCED_FACE('',(#4650),#56924,.F.);
#57751=ADVANCED_FACE('',(#4651),#56925,.F.);
#57752=ADVANCED_FACE('',(#4652),#56926,.F.);
#57753=ADVANCED_FACE('',(#4653),#1973,.F.);
#57754=ADVANCED_FACE('',(#4654),#1974,.F.);
#57755=ADVANCED_FACE('',(#4655),#1975,.F.);
#57756=ADVANCED_FACE('',(#4656),#1976,.F.);
#57757=ADVANCED_FACE('',(#4657),#1977,.F.);
#57758=ADVANCED_FACE('',(#4658),#1978,.F.);
#57759=ADVANCED_FACE('',(#4659),#56927,.F.);
#57760=ADVANCED_FACE('',(#4660),#56928,.F.);
#57761=ADVANCED_FACE('',(#4661),#56929,.F.);
#57762=ADVANCED_FACE('',(#4662),#56930,.F.);
#57763=ADVANCED_FACE('',(#4663),#56931,.F.);
#57764=ADVANCED_FACE('',(#4664),#56932,.F.);
#57765=ADVANCED_FACE('',(#4665),#56933,.F.);
#57766=ADVANCED_FACE('',(#4666),#56934,.F.);
#57767=ADVANCED_FACE('',(#4667),#1979,.F.);
#57768=ADVANCED_FACE('',(#4668),#56935,.F.);
#57769=ADVANCED_FACE('',(#4669),#1980,.T.);
#57770=ADVANCED_FACE('',(#4670),#1981,.T.);
#57771=ADVANCED_FACE('',(#4671),#56936,.F.);
#57772=ADVANCED_FACE('',(#4672),#56937,.F.);
#57773=ADVANCED_FACE('',(#4673),#56938,.F.);
#57774=ADVANCED_FACE('',(#4674),#56939,.F.);
#57775=ADVANCED_FACE('',(#4675),#56940,.F.);
#57776=ADVANCED_FACE('',(#4676),#56941,.F.);
#57777=ADVANCED_FACE('',(#4677),#56942,.F.);
#57778=ADVANCED_FACE('',(#4678),#56943,.F.);
#57779=ADVANCED_FACE('',(#4679),#56944,.F.);
#57780=ADVANCED_FACE('',(#4680),#56945,.F.);
#57781=ADVANCED_FACE('',(#4681),#56946,.F.);
#57782=ADVANCED_FACE('',(#4682),#56947,.F.);
#57783=ADVANCED_FACE('',(#4683),#56948,.F.);
#57784=ADVANCED_FACE('',(#4684),#56949,.F.);
#57785=ADVANCED_FACE('',(#4685),#56950,.F.);
#57786=ADVANCED_FACE('',(#4686),#56951,.F.);
#57787=ADVANCED_FACE('',(#4687),#56952,.F.);
#57788=ADVANCED_FACE('',(#4688),#56953,.F.);
#57789=ADVANCED_FACE('',(#4689),#56954,.F.);
#57790=ADVANCED_FACE('',(#4690),#56955,.F.);
#57791=ADVANCED_FACE('',(#4691,#1563),#1982,.T.);
#57792=ADVANCED_FACE('',(#4692),#56956,.F.);
#57793=ADVANCED_FACE('',(#4693),#56957,.F.);
#57794=ADVANCED_FACE('',(#4694),#56958,.F.);
#57795=ADVANCED_FACE('',(#4695),#56959,.F.);
#57796=ADVANCED_FACE('',(#4696),#56960,.F.);
#57797=ADVANCED_FACE('',(#4697),#56961,.F.);
#57798=ADVANCED_FACE('',(#4698),#56962,.F.);
#57799=ADVANCED_FACE('',(#4699),#56963,.F.);
#57800=ADVANCED_FACE('',(#4700),#56964,.F.);
#57801=ADVANCED_FACE('',(#4701),#56965,.F.);
#57802=ADVANCED_FACE('',(#4702),#56966,.F.);
#57803=ADVANCED_FACE('',(#4703),#56967,.F.);
#57804=ADVANCED_FACE('',(#4704),#56968,.F.);
#57805=ADVANCED_FACE('',(#4705),#56969,.F.);
#57806=ADVANCED_FACE('',(#4706),#56970,.F.);
#57807=ADVANCED_FACE('',(#4707),#56971,.F.);
#57808=ADVANCED_FACE('',(#4708),#56972,.F.);
#57809=ADVANCED_FACE('',(#4709),#56973,.F.);
#57810=ADVANCED_FACE('',(#4710),#56974,.F.);
#57811=ADVANCED_FACE('',(#4711),#56975,.F.);
#57812=ADVANCED_FACE('',(#4712),#56976,.F.);
#57813=ADVANCED_FACE('',(#4713),#56977,.F.);
#57814=ADVANCED_FACE('',(#4714),#56978,.F.);
#57815=ADVANCED_FACE('',(#4715),#56979,.F.);
#57816=ADVANCED_FACE('',(#4716),#56980,.F.);
#57817=ADVANCED_FACE('',(#4717),#56981,.F.);
#57818=ADVANCED_FACE('',(#4718),#1983,.F.);
#57819=ADVANCED_FACE('',(#4719),#56982,.F.);
#57820=ADVANCED_FACE('',(#4720,#1564),#1984,.T.);
#57821=ADVANCED_FACE('',(#4721),#1985,.T.);
#57822=ADVANCED_FACE('',(#4722),#1986,.T.);
#57823=ADVANCED_FACE('',(#4723),#56983,.F.);
#57824=ADVANCED_FACE('',(#4724),#56984,.F.);
#57825=ADVANCED_FACE('',(#4725),#56985,.F.);
#57826=ADVANCED_FACE('',(#4726),#56986,.F.);
#57827=ADVANCED_FACE('',(#4727),#56987,.F.);
#57828=ADVANCED_FACE('',(#4728),#56988,.F.);
#57829=ADVANCED_FACE('',(#4729),#56989,.F.);
#57830=ADVANCED_FACE('',(#4730),#56990,.F.);
#57831=ADVANCED_FACE('',(#4731),#56991,.F.);
#57832=ADVANCED_FACE('',(#4732),#56992,.F.);
#57833=ADVANCED_FACE('',(#4733),#56993,.F.);
#57834=ADVANCED_FACE('',(#4734),#56994,.F.);
#57835=ADVANCED_FACE('',(#4735),#56995,.F.);
#57836=ADVANCED_FACE('',(#4736),#56996,.F.);
#57837=ADVANCED_FACE('',(#4737),#56997,.F.);
#57838=ADVANCED_FACE('',(#4738),#56998,.F.);
#57839=ADVANCED_FACE('',(#4739),#56999,.F.);
#57840=ADVANCED_FACE('',(#4740),#57000,.F.);
#57841=ADVANCED_FACE('',(#4741),#57001,.F.);
#57842=ADVANCED_FACE('',(#4742),#57002,.F.);
#57843=ADVANCED_FACE('',(#4743,#1565),#1987,.T.);
#57844=ADVANCED_FACE('',(#4744),#57003,.F.);
#57845=ADVANCED_FACE('',(#4745),#57004,.F.);
#57846=ADVANCED_FACE('',(#4746),#57005,.F.);
#57847=ADVANCED_FACE('',(#4747),#1988,.F.);
#57848=ADVANCED_FACE('',(#4748),#57006,.F.);
#57849=ADVANCED_FACE('',(#4749),#57007,.F.);
#57850=ADVANCED_FACE('',(#4750),#57008,.F.);
#57851=ADVANCED_FACE('',(#4751),#1989,.F.);
#57852=ADVANCED_FACE('',(#4752),#1990,.F.);
#57853=ADVANCED_FACE('',(#4753),#1991,.F.);
#57854=ADVANCED_FACE('',(#4754),#1992,.F.);
#57855=ADVANCED_FACE('',(#4755),#1993,.T.);
#57856=ADVANCED_FACE('',(#4756),#1994,.T.);
#57857=ADVANCED_FACE('',(#4757),#57009,.F.);
#57858=ADVANCED_FACE('',(#4758),#57010,.F.);
#57859=ADVANCED_FACE('',(#4759),#57011,.F.);
#57860=ADVANCED_FACE('',(#4760),#57012,.F.);
#57861=ADVANCED_FACE('',(#4761),#57013,.F.);
#57862=ADVANCED_FACE('',(#4762),#57014,.F.);
#57863=ADVANCED_FACE('',(#4763),#57015,.F.);
#57864=ADVANCED_FACE('',(#4764),#57016,.F.);
#57865=ADVANCED_FACE('',(#4765),#57017,.F.);
#57866=ADVANCED_FACE('',(#4766),#57018,.F.);
#57867=ADVANCED_FACE('',(#4767),#57019,.F.);
#57868=ADVANCED_FACE('',(#4768),#57020,.F.);
#57869=ADVANCED_FACE('',(#4769),#57021,.F.);
#57870=ADVANCED_FACE('',(#4770),#57022,.F.);
#57871=ADVANCED_FACE('',(#4771),#57023,.F.);
#57872=ADVANCED_FACE('',(#4772),#57024,.F.);
#57873=ADVANCED_FACE('',(#4773),#57025,.F.);
#57874=ADVANCED_FACE('',(#4774),#57026,.F.);
#57875=ADVANCED_FACE('',(#4775),#57027,.F.);
#57876=ADVANCED_FACE('',(#4776),#57028,.F.);
#57877=ADVANCED_FACE('',(#4777,#1566),#1995,.T.);
#57878=ADVANCED_FACE('',(#4778),#57029,.F.);
#57879=ADVANCED_FACE('',(#4779),#57030,.F.);
#57880=ADVANCED_FACE('',(#4780),#57031,.F.);
#57881=ADVANCED_FACE('',(#4781),#57032,.F.);
#57882=ADVANCED_FACE('',(#4782),#57033,.F.);
#57883=ADVANCED_FACE('',(#4783),#57034,.F.);
#57884=ADVANCED_FACE('',(#4784),#57035,.F.);
#57885=ADVANCED_FACE('',(#4785),#57036,.F.);
#57886=ADVANCED_FACE('',(#4786),#57037,.F.);
#57887=ADVANCED_FACE('',(#4787),#57038,.F.);
#57888=ADVANCED_FACE('',(#4788),#57039,.F.);
#57889=ADVANCED_FACE('',(#4789),#57040,.F.);
#57890=ADVANCED_FACE('',(#4790),#57041,.F.);
#57891=ADVANCED_FACE('',(#4791),#57042,.F.);
#57892=ADVANCED_FACE('',(#4792),#57043,.F.);
#57893=ADVANCED_FACE('',(#4793),#57044,.F.);
#57894=ADVANCED_FACE('',(#4794),#57045,.F.);
#57895=ADVANCED_FACE('',(#4795),#57046,.F.);
#57896=ADVANCED_FACE('',(#4796),#57047,.F.);
#57897=ADVANCED_FACE('',(#4797),#57048,.F.);
#57898=ADVANCED_FACE('',(#4798),#57049,.F.);
#57899=ADVANCED_FACE('',(#4799),#57050,.F.);
#57900=ADVANCED_FACE('',(#4800),#57051,.F.);
#57901=ADVANCED_FACE('',(#4801),#57052,.F.);
#57902=ADVANCED_FACE('',(#4802),#57053,.F.);
#57903=ADVANCED_FACE('',(#4803),#57054,.F.);
#57904=ADVANCED_FACE('',(#4804),#57055,.F.);
#57905=ADVANCED_FACE('',(#4805),#57056,.F.);
#57906=ADVANCED_FACE('',(#4806),#57057,.F.);
#57907=ADVANCED_FACE('',(#4807),#57058,.F.);
#57908=ADVANCED_FACE('',(#4808),#57059,.F.);
#57909=ADVANCED_FACE('',(#4809),#57060,.F.);
#57910=ADVANCED_FACE('',(#4810),#57061,.F.);
#57911=ADVANCED_FACE('',(#4811,#1567,#1568),#1996,.T.);
#57912=ADVANCED_FACE('',(#4812),#1997,.T.);
#57913=ADVANCED_FACE('',(#4813),#1998,.T.);
#57914=ADVANCED_FACE('',(#4814),#1999,.T.);
#57915=ADVANCED_FACE('',(#4815),#57062,.F.);
#57916=ADVANCED_FACE('',(#4816),#57063,.F.);
#57917=ADVANCED_FACE('',(#4817),#57064,.F.);
#57918=ADVANCED_FACE('',(#4818),#57065,.F.);
#57919=ADVANCED_FACE('',(#4819),#57066,.F.);
#57920=ADVANCED_FACE('',(#4820),#57067,.F.);
#57921=ADVANCED_FACE('',(#4821),#57068,.F.);
#57922=ADVANCED_FACE('',(#4822),#57069,.F.);
#57923=ADVANCED_FACE('',(#4823),#57070,.F.);
#57924=ADVANCED_FACE('',(#4824),#57071,.F.);
#57925=ADVANCED_FACE('',(#4825),#57072,.F.);
#57926=ADVANCED_FACE('',(#4826),#57073,.F.);
#57927=ADVANCED_FACE('',(#4827),#57074,.F.);
#57928=ADVANCED_FACE('',(#4828),#57075,.F.);
#57929=ADVANCED_FACE('',(#4829),#57076,.F.);
#57930=ADVANCED_FACE('',(#4830),#57077,.F.);
#57931=ADVANCED_FACE('',(#4831),#57078,.F.);
#57932=ADVANCED_FACE('',(#4832),#57079,.F.);
#57933=ADVANCED_FACE('',(#4833),#57080,.F.);
#57934=ADVANCED_FACE('',(#4834),#57081,.F.);
#57935=ADVANCED_FACE('',(#4835,#1569),#2000,.T.);
#57936=ADVANCED_FACE('',(#4836),#57082,.F.);
#57937=ADVANCED_FACE('',(#4837),#57083,.F.);
#57938=ADVANCED_FACE('',(#4838),#57084,.F.);
#57939=ADVANCED_FACE('',(#4839),#57085,.F.);
#57940=ADVANCED_FACE('',(#4840),#57086,.F.);
#57941=ADVANCED_FACE('',(#4841),#57087,.F.);
#57942=ADVANCED_FACE('',(#4842),#57088,.F.);
#57943=ADVANCED_FACE('',(#4843),#57089,.F.);
#57944=ADVANCED_FACE('',(#4844),#57090,.F.);
#57945=ADVANCED_FACE('',(#4845),#57091,.F.);
#57946=ADVANCED_FACE('',(#4846),#57092,.F.);
#57947=ADVANCED_FACE('',(#4847),#57093,.F.);
#57948=ADVANCED_FACE('',(#4848),#57094,.F.);
#57949=ADVANCED_FACE('',(#4849),#57095,.F.);
#57950=ADVANCED_FACE('',(#4850),#57096,.F.);
#57951=ADVANCED_FACE('',(#4851),#57097,.F.);
#57952=ADVANCED_FACE('',(#4852),#57098,.F.);
#57953=ADVANCED_FACE('',(#4853),#57099,.F.);
#57954=ADVANCED_FACE('',(#4854),#57100,.F.);
#57955=ADVANCED_FACE('',(#4855),#57101,.F.);
#57956=ADVANCED_FACE('',(#4856),#57102,.F.);
#57957=ADVANCED_FACE('',(#4857),#57103,.F.);
#57958=ADVANCED_FACE('',(#4858),#57104,.F.);
#57959=ADVANCED_FACE('',(#4859),#57105,.F.);
#57960=ADVANCED_FACE('',(#4860),#57106,.F.);
#57961=ADVANCED_FACE('',(#4861),#57107,.F.);
#57962=ADVANCED_FACE('',(#4862),#57108,.F.);
#57963=ADVANCED_FACE('',(#4863),#57109,.F.);
#57964=ADVANCED_FACE('',(#4864),#2001,.F.);
#57965=ADVANCED_FACE('',(#4865),#57110,.F.);
#57966=ADVANCED_FACE('',(#4866,#1570),#2002,.T.);
#57967=ADVANCED_FACE('',(#4867),#2003,.T.);
#57968=ADVANCED_FACE('',(#4868),#2004,.T.);
#57969=ADVANCED_FACE('',(#4869),#2005,.F.);
#57970=ADVANCED_FACE('',(#4870),#2006,.F.);
#57971=ADVANCED_FACE('',(#4871),#2007,.F.);
#57972=ADVANCED_FACE('',(#4872),#2008,.F.);
#57973=ADVANCED_FACE('',(#4873),#2009,.F.);
#57974=ADVANCED_FACE('',(#4874),#2010,.F.);
#57975=ADVANCED_FACE('',(#4875),#2011,.F.);
#57976=ADVANCED_FACE('',(#4876),#2012,.F.);
#57977=ADVANCED_FACE('',(#4877),#2013,.F.);
#57978=ADVANCED_FACE('',(#4878),#2014,.F.);
#57979=ADVANCED_FACE('',(#4879),#2015,.F.);
#57980=ADVANCED_FACE('',(#4880),#2016,.F.);
#57981=ADVANCED_FACE('',(#4881),#2017,.F.);
#57982=ADVANCED_FACE('',(#4882),#2018,.F.);
#57983=ADVANCED_FACE('',(#4883),#2019,.F.);
#57984=ADVANCED_FACE('',(#4884),#2020,.F.);
#57985=ADVANCED_FACE('',(#4885),#2021,.F.);
#57986=ADVANCED_FACE('',(#4886),#2022,.F.);
#57987=ADVANCED_FACE('',(#4887),#2023,.F.);
#57988=ADVANCED_FACE('',(#4888),#2024,.F.);
#57989=ADVANCED_FACE('',(#4889),#2025,.F.);
#57990=ADVANCED_FACE('',(#4890),#2026,.F.);
#57991=ADVANCED_FACE('',(#4891),#2027,.F.);
#57992=ADVANCED_FACE('',(#4892),#2028,.F.);
#57993=ADVANCED_FACE('',(#4893),#2029,.F.);
#57994=ADVANCED_FACE('',(#4894),#2030,.F.);
#57995=ADVANCED_FACE('',(#4895),#2031,.F.);
#57996=ADVANCED_FACE('',(#4896),#2032,.F.);
#57997=ADVANCED_FACE('',(#4897),#2033,.F.);
#57998=ADVANCED_FACE('',(#4898),#2034,.F.);
#57999=ADVANCED_FACE('',(#4899),#2035,.F.);
#58000=ADVANCED_FACE('',(#4900),#2036,.F.);
#58001=ADVANCED_FACE('',(#4901),#2037,.F.);
#58002=ADVANCED_FACE('',(#4902),#2038,.F.);
#58003=ADVANCED_FACE('',(#4903),#2039,.F.);
#58004=ADVANCED_FACE('',(#4904),#2040,.F.);
#58005=ADVANCED_FACE('',(#4905),#2041,.F.);
#58006=ADVANCED_FACE('',(#4906),#2042,.F.);
#58007=ADVANCED_FACE('',(#4907),#2043,.F.);
#58008=ADVANCED_FACE('',(#4908),#2044,.F.);
#58009=ADVANCED_FACE('',(#4909),#2045,.F.);
#58010=ADVANCED_FACE('',(#4910),#2046,.F.);
#58011=ADVANCED_FACE('',(#4911),#2047,.F.);
#58012=ADVANCED_FACE('',(#4912),#2048,.F.);
#58013=ADVANCED_FACE('',(#4913),#2049,.F.);
#58014=ADVANCED_FACE('',(#4914),#2050,.F.);
#58015=ADVANCED_FACE('',(#4915),#2051,.F.);
#58016=ADVANCED_FACE('',(#4916),#2052,.F.);
#58017=ADVANCED_FACE('',(#4917),#2053,.F.);
#58018=ADVANCED_FACE('',(#4918),#2054,.F.);
#58019=ADVANCED_FACE('',(#4919),#2055,.F.);
#58020=ADVANCED_FACE('',(#4920),#2056,.F.);
#58021=ADVANCED_FACE('',(#4921),#2057,.F.);
#58022=ADVANCED_FACE('',(#4922),#2058,.F.);
#58023=ADVANCED_FACE('',(#4923),#2059,.F.);
#58024=ADVANCED_FACE('',(#4924),#2060,.F.);
#58025=ADVANCED_FACE('',(#4925),#2061,.F.);
#58026=ADVANCED_FACE('',(#4926),#2062,.F.);
#58027=ADVANCED_FACE('',(#4927),#2063,.F.);
#58028=ADVANCED_FACE('',(#4928),#2064,.F.);
#58029=ADVANCED_FACE('',(#4929),#2065,.F.);
#58030=ADVANCED_FACE('',(#4930),#2066,.F.);
#58031=ADVANCED_FACE('',(#4931),#2067,.F.);
#58032=ADVANCED_FACE('',(#4932),#2068,.F.);
#58033=ADVANCED_FACE('',(#4933),#2069,.F.);
#58034=ADVANCED_FACE('',(#4934),#2070,.F.);
#58035=ADVANCED_FACE('',(#4935),#2071,.F.);
#58036=ADVANCED_FACE('',(#4936),#2072,.F.);
#58037=ADVANCED_FACE('',(#4937),#2073,.F.);
#58038=ADVANCED_FACE('',(#4938),#2074,.F.);
#58039=ADVANCED_FACE('',(#4939),#2075,.F.);
#58040=ADVANCED_FACE('',(#4940),#2076,.F.);
#58041=ADVANCED_FACE('',(#4941),#2077,.F.);
#58042=ADVANCED_FACE('',(#4942),#2078,.F.);
#58043=ADVANCED_FACE('',(#4943),#2079,.F.);
#58044=ADVANCED_FACE('',(#4944),#2080,.F.);
#58045=ADVANCED_FACE('',(#4945),#2081,.F.);
#58046=ADVANCED_FACE('',(#4946),#2082,.F.);
#58047=ADVANCED_FACE('',(#4947),#2083,.F.);
#58048=ADVANCED_FACE('',(#4948),#2084,.F.);
#58049=ADVANCED_FACE('',(#4949),#2085,.F.);
#58050=ADVANCED_FACE('',(#4950),#2086,.F.);
#58051=ADVANCED_FACE('',(#4951),#2087,.F.);
#58052=ADVANCED_FACE('',(#4952),#2088,.F.);
#58053=ADVANCED_FACE('',(#4953),#2089,.F.);
#58054=ADVANCED_FACE('',(#4954),#2090,.F.);
#58055=ADVANCED_FACE('',(#4955),#2091,.F.);
#58056=ADVANCED_FACE('',(#4956),#2092,.F.);
#58057=ADVANCED_FACE('',(#4957),#2093,.F.);
#58058=ADVANCED_FACE('',(#4958),#2094,.F.);
#58059=ADVANCED_FACE('',(#4959),#2095,.F.);
#58060=ADVANCED_FACE('',(#4960),#2096,.F.);
#58061=ADVANCED_FACE('',(#4961),#2097,.F.);
#58062=ADVANCED_FACE('',(#4962),#2098,.F.);
#58063=ADVANCED_FACE('',(#4963),#2099,.F.);
#58064=ADVANCED_FACE('',(#4964),#2100,.F.);
#58065=ADVANCED_FACE('',(#4965),#2101,.F.);
#58066=ADVANCED_FACE('',(#4966),#2102,.F.);
#58067=ADVANCED_FACE('',(#4967),#2103,.F.);
#58068=ADVANCED_FACE('',(#4968),#2104,.F.);
#58069=ADVANCED_FACE('',(#4969),#2105,.F.);
#58070=ADVANCED_FACE('',(#4970),#2106,.F.);
#58071=ADVANCED_FACE('',(#4971),#2107,.F.);
#58072=ADVANCED_FACE('',(#4972),#2108,.F.);
#58073=ADVANCED_FACE('',(#4973),#2109,.F.);
#58074=ADVANCED_FACE('',(#4974),#2110,.F.);
#58075=ADVANCED_FACE('',(#4975),#2111,.F.);
#58076=ADVANCED_FACE('',(#4976),#2112,.F.);
#58077=ADVANCED_FACE('',(#4977),#2113,.F.);
#58078=ADVANCED_FACE('',(#4978),#2114,.F.);
#58079=ADVANCED_FACE('',(#4979),#2115,.F.);
#58080=ADVANCED_FACE('',(#4980),#2116,.F.);
#58081=ADVANCED_FACE('',(#4981),#2117,.F.);
#58082=ADVANCED_FACE('',(#4982),#2118,.F.);
#58083=ADVANCED_FACE('',(#4983),#2119,.F.);
#58084=ADVANCED_FACE('',(#4984),#2120,.F.);
#58085=ADVANCED_FACE('',(#4985),#2121,.F.);
#58086=ADVANCED_FACE('',(#4986),#2122,.F.);
#58087=ADVANCED_FACE('',(#4987),#2123,.F.);
#58088=ADVANCED_FACE('',(#4988),#2124,.F.);
#58089=ADVANCED_FACE('',(#4989),#2125,.F.);
#58090=ADVANCED_FACE('',(#4990),#2126,.F.);
#58091=ADVANCED_FACE('',(#4991),#2127,.F.);
#58092=ADVANCED_FACE('',(#4992),#2128,.F.);
#58093=ADVANCED_FACE('',(#4993),#2129,.F.);
#58094=ADVANCED_FACE('',(#4994),#2130,.F.);
#58095=ADVANCED_FACE('',(#4995),#2131,.F.);
#58096=ADVANCED_FACE('',(#4996),#2132,.F.);
#58097=ADVANCED_FACE('',(#4997),#2133,.F.);
#58098=ADVANCED_FACE('',(#4998),#2134,.F.);
#58099=ADVANCED_FACE('',(#4999),#2135,.F.);
#58100=ADVANCED_FACE('',(#5000),#2136,.F.);
#58101=ADVANCED_FACE('',(#5001),#2137,.F.);
#58102=ADVANCED_FACE('',(#5002),#2138,.F.);
#58103=ADVANCED_FACE('',(#5003),#2139,.F.);
#58104=ADVANCED_FACE('',(#5004),#2140,.F.);
#58105=ADVANCED_FACE('',(#5005),#2141,.F.);
#58106=ADVANCED_FACE('',(#5006),#2142,.F.);
#58107=ADVANCED_FACE('',(#5007),#2143,.F.);
#58108=ADVANCED_FACE('',(#5008),#2144,.F.);
#58109=ADVANCED_FACE('',(#5009),#2145,.F.);
#58110=ADVANCED_FACE('',(#5010),#2146,.F.);
#58111=ADVANCED_FACE('',(#5011),#2147,.F.);
#58112=ADVANCED_FACE('',(#5012),#2148,.F.);
#58113=ADVANCED_FACE('',(#5013),#2149,.F.);
#58114=ADVANCED_FACE('',(#5014),#2150,.F.);
#58115=ADVANCED_FACE('',(#5015),#2151,.F.);
#58116=ADVANCED_FACE('',(#5016),#2152,.F.);
#58117=ADVANCED_FACE('',(#5017),#2153,.F.);
#58118=ADVANCED_FACE('',(#5018),#2154,.F.);
#58119=ADVANCED_FACE('',(#5019),#2155,.F.);
#58120=ADVANCED_FACE('',(#5020),#2156,.F.);
#58121=ADVANCED_FACE('',(#5021),#2157,.F.);
#58122=ADVANCED_FACE('',(#5022),#2158,.F.);
#58123=ADVANCED_FACE('',(#5023),#2159,.F.);
#58124=ADVANCED_FACE('',(#5024),#2160,.F.);
#58125=ADVANCED_FACE('',(#5025),#2161,.F.);
#58126=ADVANCED_FACE('',(#5026),#2162,.F.);
#58127=ADVANCED_FACE('',(#5027),#2163,.F.);
#58128=ADVANCED_FACE('',(#5028),#2164,.F.);
#58129=ADVANCED_FACE('',(#5029),#2165,.F.);
#58130=ADVANCED_FACE('',(#5030),#2166,.F.);
#58131=ADVANCED_FACE('',(#5031),#2167,.F.);
#58132=ADVANCED_FACE('',(#5032),#2168,.F.);
#58133=ADVANCED_FACE('',(#5033),#2169,.F.);
#58134=ADVANCED_FACE('',(#5034),#2170,.F.);
#58135=ADVANCED_FACE('',(#5035),#2171,.F.);
#58136=ADVANCED_FACE('',(#5036),#2172,.F.);
#58137=ADVANCED_FACE('',(#5037),#2173,.F.);
#58138=ADVANCED_FACE('',(#5038),#2174,.F.);
#58139=ADVANCED_FACE('',(#5039),#2175,.F.);
#58140=ADVANCED_FACE('',(#5040),#2176,.F.);
#58141=ADVANCED_FACE('',(#5041),#2177,.F.);
#58142=ADVANCED_FACE('',(#5042),#2178,.F.);
#58143=ADVANCED_FACE('',(#5043),#2179,.F.);
#58144=ADVANCED_FACE('',(#5044),#2180,.F.);
#58145=ADVANCED_FACE('',(#5045),#2181,.F.);
#58146=ADVANCED_FACE('',(#5046),#2182,.F.);
#58147=ADVANCED_FACE('',(#5047),#2183,.F.);
#58148=ADVANCED_FACE('',(#5048),#2184,.F.);
#58149=ADVANCED_FACE('',(#5049),#2185,.F.);
#58150=ADVANCED_FACE('',(#5050),#2186,.F.);
#58151=ADVANCED_FACE('',(#5051),#2187,.F.);
#58152=ADVANCED_FACE('',(#5052),#2188,.F.);
#58153=ADVANCED_FACE('',(#5053),#2189,.F.);
#58154=ADVANCED_FACE('',(#5054),#2190,.F.);
#58155=ADVANCED_FACE('',(#5055),#2191,.F.);
#58156=ADVANCED_FACE('',(#5056),#2192,.F.);
#58157=ADVANCED_FACE('',(#5057),#2193,.F.);
#58158=ADVANCED_FACE('',(#5058),#2194,.F.);
#58159=ADVANCED_FACE('',(#5059),#2195,.F.);
#58160=ADVANCED_FACE('',(#5060),#2196,.F.);
#58161=ADVANCED_FACE('',(#5061),#2197,.F.);
#58162=ADVANCED_FACE('',(#5062),#2198,.F.);
#58163=ADVANCED_FACE('',(#5063),#2199,.F.);
#58164=ADVANCED_FACE('',(#5064),#2200,.F.);
#58165=ADVANCED_FACE('',(#5065),#2201,.F.);
#58166=ADVANCED_FACE('',(#5066),#2202,.F.);
#58167=ADVANCED_FACE('',(#5067),#2203,.F.);
#58168=ADVANCED_FACE('',(#5068),#2204,.F.);
#58169=ADVANCED_FACE('',(#5069),#2205,.F.);
#58170=ADVANCED_FACE('',(#5070),#2206,.F.);
#58171=ADVANCED_FACE('',(#5071),#2207,.F.);
#58172=ADVANCED_FACE('',(#5072),#2208,.F.);
#58173=ADVANCED_FACE('',(#5073),#2209,.F.);
#58174=ADVANCED_FACE('',(#5074),#2210,.F.);
#58175=ADVANCED_FACE('',(#5075),#2211,.F.);
#58176=ADVANCED_FACE('',(#5076),#2212,.F.);
#58177=ADVANCED_FACE('',(#5077),#2213,.F.);
#58178=ADVANCED_FACE('',(#5078),#2214,.F.);
#58179=ADVANCED_FACE('',(#5079),#2215,.F.);
#58180=ADVANCED_FACE('',(#5080),#2216,.F.);
#58181=ADVANCED_FACE('',(#5081),#2217,.F.);
#58182=ADVANCED_FACE('',(#5082),#2218,.F.);
#58183=ADVANCED_FACE('',(#5083),#2219,.F.);
#58184=ADVANCED_FACE('',(#5084),#2220,.F.);
#58185=ADVANCED_FACE('',(#5085),#2221,.F.);
#58186=ADVANCED_FACE('',(#5086),#2222,.F.);
#58187=ADVANCED_FACE('',(#5087),#2223,.F.);
#58188=ADVANCED_FACE('',(#5088),#2224,.F.);
#58189=ADVANCED_FACE('',(#5089),#2225,.F.);
#58190=ADVANCED_FACE('',(#5090),#2226,.F.);
#58191=ADVANCED_FACE('',(#5091),#2227,.F.);
#58192=ADVANCED_FACE('',(#5092),#2228,.F.);
#58193=ADVANCED_FACE('',(#5093),#2229,.F.);
#58194=ADVANCED_FACE('',(#5094),#2230,.F.);
#58195=ADVANCED_FACE('',(#5095),#2231,.F.);
#58196=ADVANCED_FACE('',(#5096),#2232,.F.);
#58197=ADVANCED_FACE('',(#5097),#2233,.F.);
#58198=ADVANCED_FACE('',(#5098),#2234,.F.);
#58199=ADVANCED_FACE('',(#5099),#2235,.F.);
#58200=ADVANCED_FACE('',(#5100),#2236,.F.);
#58201=ADVANCED_FACE('',(#5101),#2237,.F.);
#58202=ADVANCED_FACE('',(#5102),#2238,.F.);
#58203=ADVANCED_FACE('',(#5103),#2239,.F.);
#58204=ADVANCED_FACE('',(#5104),#2240,.F.);
#58205=ADVANCED_FACE('',(#5105),#2241,.F.);
#58206=ADVANCED_FACE('',(#5106),#2242,.F.);
#58207=ADVANCED_FACE('',(#5107),#2243,.F.);
#58208=ADVANCED_FACE('',(#5108),#2244,.F.);
#58209=ADVANCED_FACE('',(#5109),#2245,.F.);
#58210=ADVANCED_FACE('',(#5110),#2246,.F.);
#58211=ADVANCED_FACE('',(#5111),#2247,.F.);
#58212=ADVANCED_FACE('',(#5112),#2248,.F.);
#58213=ADVANCED_FACE('',(#5113),#2249,.F.);
#58214=ADVANCED_FACE('',(#5114),#2250,.F.);
#58215=ADVANCED_FACE('',(#5115),#2251,.F.);
#58216=ADVANCED_FACE('',(#5116),#2252,.F.);
#58217=ADVANCED_FACE('',(#5117),#2253,.F.);
#58218=ADVANCED_FACE('',(#5118),#2254,.F.);
#58219=ADVANCED_FACE('',(#5119),#2255,.F.);
#58220=ADVANCED_FACE('',(#5120),#2256,.F.);
#58221=ADVANCED_FACE('',(#5121),#2257,.F.);
#58222=ADVANCED_FACE('',(#5122),#2258,.F.);
#58223=ADVANCED_FACE('',(#5123),#2259,.F.);
#58224=ADVANCED_FACE('',(#5124),#2260,.F.);
#58225=ADVANCED_FACE('',(#5125),#2261,.F.);
#58226=ADVANCED_FACE('',(#5126),#2262,.F.);
#58227=ADVANCED_FACE('',(#5127),#2263,.F.);
#58228=ADVANCED_FACE('',(#5128),#2264,.F.);
#58229=ADVANCED_FACE('',(#5129),#2265,.F.);
#58230=ADVANCED_FACE('',(#5130),#2266,.F.);
#58231=ADVANCED_FACE('',(#5131),#2267,.F.);
#58232=ADVANCED_FACE('',(#5132),#2268,.F.);
#58233=ADVANCED_FACE('',(#5133),#2269,.F.);
#58234=ADVANCED_FACE('',(#5134),#2270,.F.);
#58235=ADVANCED_FACE('',(#5135),#2271,.F.);
#58236=ADVANCED_FACE('',(#5136),#2272,.F.);
#58237=ADVANCED_FACE('',(#5137),#2273,.F.);
#58238=ADVANCED_FACE('',(#5138),#2274,.F.);
#58239=ADVANCED_FACE('',(#5139),#2275,.F.);
#58240=ADVANCED_FACE('',(#5140),#2276,.F.);
#58241=ADVANCED_FACE('',(#5141),#2277,.F.);
#58242=ADVANCED_FACE('',(#5142),#2278,.F.);
#58243=ADVANCED_FACE('',(#5143),#2279,.F.);
#58244=ADVANCED_FACE('',(#5144),#2280,.F.);
#58245=ADVANCED_FACE('',(#5145),#2281,.F.);
#58246=ADVANCED_FACE('',(#5146),#2282,.F.);
#58247=ADVANCED_FACE('',(#5147),#2283,.F.);
#58248=ADVANCED_FACE('',(#5148),#2284,.F.);
#58249=ADVANCED_FACE('',(#5149),#2285,.F.);
#58250=ADVANCED_FACE('',(#5150),#2286,.F.);
#58251=ADVANCED_FACE('',(#5151),#2287,.F.);
#58252=ADVANCED_FACE('',(#5152),#2288,.F.);
#58253=ADVANCED_FACE('',(#5153),#2289,.F.);
#58254=ADVANCED_FACE('',(#5154),#2290,.F.);
#58255=ADVANCED_FACE('',(#5155),#2291,.F.);
#58256=ADVANCED_FACE('',(#5156),#2292,.F.);
#58257=ADVANCED_FACE('',(#5157),#2293,.F.);
#58258=ADVANCED_FACE('',(#5158),#2294,.F.);
#58259=ADVANCED_FACE('',(#5159),#2295,.F.);
#58260=ADVANCED_FACE('',(#5160),#2296,.F.);
#58261=ADVANCED_FACE('',(#5161),#2297,.F.);
#58262=ADVANCED_FACE('',(#5162),#2298,.F.);
#58263=ADVANCED_FACE('',(#5163),#2299,.F.);
#58264=ADVANCED_FACE('',(#5164),#2300,.F.);
#58265=ADVANCED_FACE('',(#5165),#2301,.F.);
#58266=ADVANCED_FACE('',(#5166),#2302,.F.);
#58267=ADVANCED_FACE('',(#5167),#2303,.F.);
#58268=ADVANCED_FACE('',(#5168),#2304,.F.);
#58269=ADVANCED_FACE('',(#5169),#2305,.F.);
#58270=ADVANCED_FACE('',(#5170),#2306,.F.);
#58271=ADVANCED_FACE('',(#5171),#2307,.F.);
#58272=ADVANCED_FACE('',(#5172),#2308,.F.);
#58273=ADVANCED_FACE('',(#5173),#2309,.F.);
#58274=ADVANCED_FACE('',(#5174),#2310,.F.);
#58275=ADVANCED_FACE('',(#5175),#2311,.F.);
#58276=ADVANCED_FACE('',(#5176),#2312,.F.);
#58277=ADVANCED_FACE('',(#5177),#2313,.F.);
#58278=ADVANCED_FACE('',(#5178),#2314,.F.);
#58279=ADVANCED_FACE('',(#5179),#2315,.F.);
#58280=ADVANCED_FACE('',(#5180),#2316,.F.);
#58281=ADVANCED_FACE('',(#5181),#2317,.F.);
#58282=ADVANCED_FACE('',(#5182),#2318,.F.);
#58283=ADVANCED_FACE('',(#5183),#2319,.F.);
#58284=ADVANCED_FACE('',(#5184),#2320,.F.);
#58285=ADVANCED_FACE('',(#5185),#2321,.F.);
#58286=ADVANCED_FACE('',(#5186),#2322,.F.);
#58287=ADVANCED_FACE('',(#5187),#2323,.F.);
#58288=ADVANCED_FACE('',(#5188),#2324,.F.);
#58289=ADVANCED_FACE('',(#5189),#2325,.F.);
#58290=ADVANCED_FACE('',(#5190),#2326,.F.);
#58291=ADVANCED_FACE('',(#5191),#2327,.F.);
#58292=ADVANCED_FACE('',(#5192),#2328,.F.);
#58293=ADVANCED_FACE('',(#5193),#2329,.F.);
#58294=ADVANCED_FACE('',(#5194),#2330,.F.);
#58295=ADVANCED_FACE('',(#5195),#2331,.F.);
#58296=ADVANCED_FACE('',(#5196),#2332,.F.);
#58297=ADVANCED_FACE('',(#5197),#2333,.F.);
#58298=ADVANCED_FACE('',(#5198),#2334,.F.);
#58299=ADVANCED_FACE('',(#5199),#2335,.F.);
#58300=ADVANCED_FACE('',(#5200),#2336,.F.);
#58301=ADVANCED_FACE('',(#5201),#2337,.F.);
#58302=ADVANCED_FACE('',(#5202),#2338,.F.);
#58303=ADVANCED_FACE('',(#5203),#2339,.F.);
#58304=ADVANCED_FACE('',(#5204),#2340,.F.);
#58305=ADVANCED_FACE('',(#5205),#2341,.F.);
#58306=ADVANCED_FACE('',(#5206),#2342,.F.);
#58307=ADVANCED_FACE('',(#5207),#2343,.F.);
#58308=ADVANCED_FACE('',(#5208),#2344,.F.);
#58309=ADVANCED_FACE('',(#5209),#2345,.F.);
#58310=ADVANCED_FACE('',(#5210),#2346,.F.);
#58311=ADVANCED_FACE('',(#5211),#2347,.F.);
#58312=ADVANCED_FACE('',(#5212),#2348,.F.);
#58313=ADVANCED_FACE('',(#5213),#2349,.F.);
#58314=ADVANCED_FACE('',(#5214),#2350,.F.);
#58315=ADVANCED_FACE('',(#5215),#2351,.F.);
#58316=ADVANCED_FACE('',(#5216),#2352,.F.);
#58317=ADVANCED_FACE('',(#5217),#2353,.F.);
#58318=ADVANCED_FACE('',(#5218),#2354,.F.);
#58319=ADVANCED_FACE('',(#5219),#2355,.F.);
#58320=ADVANCED_FACE('',(#5220),#2356,.F.);
#58321=ADVANCED_FACE('',(#5221),#2357,.F.);
#58322=ADVANCED_FACE('',(#5222),#2358,.F.);
#58323=ADVANCED_FACE('',(#5223),#2359,.F.);
#58324=ADVANCED_FACE('',(#5224),#2360,.F.);
#58325=ADVANCED_FACE('',(#5225),#2361,.F.);
#58326=ADVANCED_FACE('',(#5226),#2362,.F.);
#58327=ADVANCED_FACE('',(#5227),#2363,.F.);
#58328=ADVANCED_FACE('',(#5228),#2364,.F.);
#58329=ADVANCED_FACE('',(#5229),#2365,.F.);
#58330=ADVANCED_FACE('',(#5230),#2366,.F.);
#58331=ADVANCED_FACE('',(#5231),#2367,.F.);
#58332=ADVANCED_FACE('',(#5232),#2368,.F.);
#58333=ADVANCED_FACE('',(#5233),#2369,.F.);
#58334=ADVANCED_FACE('',(#5234),#2370,.F.);
#58335=ADVANCED_FACE('',(#5235),#2371,.F.);
#58336=ADVANCED_FACE('',(#5236),#2372,.F.);
#58337=ADVANCED_FACE('',(#5237),#2373,.F.);
#58338=ADVANCED_FACE('',(#5238),#2374,.F.);
#58339=ADVANCED_FACE('',(#5239),#2375,.F.);
#58340=ADVANCED_FACE('',(#5240),#2376,.F.);
#58341=ADVANCED_FACE('',(#5241),#2377,.F.);
#58342=ADVANCED_FACE('',(#5242),#2378,.F.);
#58343=ADVANCED_FACE('',(#5243),#2379,.F.);
#58344=ADVANCED_FACE('',(#5244),#2380,.F.);
#58345=ADVANCED_FACE('',(#5245),#2381,.F.);
#58346=ADVANCED_FACE('',(#5246),#2382,.F.);
#58347=ADVANCED_FACE('',(#5247),#2383,.F.);
#58348=ADVANCED_FACE('',(#5248),#2384,.F.);
#58349=ADVANCED_FACE('',(#5249),#2385,.F.);
#58350=ADVANCED_FACE('',(#5250),#2386,.F.);
#58351=ADVANCED_FACE('',(#5251),#2387,.F.);
#58352=ADVANCED_FACE('',(#5252),#2388,.F.);
#58353=ADVANCED_FACE('',(#5253),#2389,.F.);
#58354=ADVANCED_FACE('',(#5254),#2390,.F.);
#58355=ADVANCED_FACE('',(#5255),#2391,.F.);
#58356=ADVANCED_FACE('',(#5256),#2392,.F.);
#58357=ADVANCED_FACE('',(#5257),#2393,.F.);
#58358=ADVANCED_FACE('',(#5258),#2394,.F.);
#58359=ADVANCED_FACE('',(#5259),#2395,.F.);
#58360=ADVANCED_FACE('',(#5260),#2396,.F.);
#58361=ADVANCED_FACE('',(#5261),#2397,.F.);
#58362=ADVANCED_FACE('',(#5262),#2398,.F.);
#58363=ADVANCED_FACE('',(#5263),#2399,.F.);
#58364=ADVANCED_FACE('',(#5264),#2400,.F.);
#58365=ADVANCED_FACE('',(#5265),#2401,.F.);
#58366=ADVANCED_FACE('',(#5266),#2402,.F.);
#58367=ADVANCED_FACE('',(#5267),#2403,.F.);
#58368=ADVANCED_FACE('',(#5268),#2404,.F.);
#58369=ADVANCED_FACE('',(#5269),#2405,.F.);
#58370=ADVANCED_FACE('',(#5270),#2406,.F.);
#58371=ADVANCED_FACE('',(#5271),#2407,.F.);
#58372=ADVANCED_FACE('',(#5272),#2408,.F.);
#58373=ADVANCED_FACE('',(#5273),#2409,.F.);
#58374=ADVANCED_FACE('',(#5274),#2410,.F.);
#58375=ADVANCED_FACE('',(#5275),#2411,.F.);
#58376=ADVANCED_FACE('',(#5276),#2412,.F.);
#58377=ADVANCED_FACE('',(#5277),#2413,.F.);
#58378=ADVANCED_FACE('',(#5278),#2414,.F.);
#58379=ADVANCED_FACE('',(#5279),#2415,.F.);
#58380=ADVANCED_FACE('',(#5280),#2416,.F.);
#58381=ADVANCED_FACE('',(#5281),#2417,.F.);
#58382=ADVANCED_FACE('',(#5282),#2418,.F.);
#58383=ADVANCED_FACE('',(#5283),#2419,.F.);
#58384=ADVANCED_FACE('',(#5284),#2420,.F.);
#58385=ADVANCED_FACE('',(#5285),#2421,.F.);
#58386=ADVANCED_FACE('',(#5286),#2422,.F.);
#58387=ADVANCED_FACE('',(#5287),#2423,.F.);
#58388=ADVANCED_FACE('',(#5288),#2424,.F.);
#58389=ADVANCED_FACE('',(#5289),#2425,.F.);
#58390=ADVANCED_FACE('',(#5290),#2426,.F.);
#58391=ADVANCED_FACE('',(#5291),#2427,.F.);
#58392=ADVANCED_FACE('',(#5292),#2428,.F.);
#58393=ADVANCED_FACE('',(#5293),#2429,.F.);
#58394=ADVANCED_FACE('',(#5294),#2430,.F.);
#58395=ADVANCED_FACE('',(#5295),#2431,.F.);
#58396=ADVANCED_FACE('',(#5296),#2432,.F.);
#58397=ADVANCED_FACE('',(#5297),#2433,.F.);
#58398=ADVANCED_FACE('',(#5298),#2434,.F.);
#58399=ADVANCED_FACE('',(#5299),#2435,.F.);
#58400=ADVANCED_FACE('',(#5300),#2436,.F.);
#58401=ADVANCED_FACE('',(#5301),#2437,.F.);
#58402=ADVANCED_FACE('',(#5302),#2438,.F.);
#58403=ADVANCED_FACE('',(#5303),#2439,.F.);
#58404=ADVANCED_FACE('',(#5304),#2440,.F.);
#58405=ADVANCED_FACE('',(#5305),#2441,.F.);
#58406=ADVANCED_FACE('',(#5306),#2442,.F.);
#58407=ADVANCED_FACE('',(#5307),#2443,.F.);
#58408=ADVANCED_FACE('',(#5308),#2444,.F.);
#58409=ADVANCED_FACE('',(#5309),#2445,.F.);
#58410=ADVANCED_FACE('',(#5310),#2446,.F.);
#58411=ADVANCED_FACE('',(#5311),#2447,.F.);
#58412=ADVANCED_FACE('',(#5312),#2448,.F.);
#58413=ADVANCED_FACE('',(#5313),#2449,.F.);
#58414=ADVANCED_FACE('',(#5314),#2450,.F.);
#58415=ADVANCED_FACE('',(#5315),#2451,.F.);
#58416=ADVANCED_FACE('',(#5316),#2452,.F.);
#58417=ADVANCED_FACE('',(#5317),#2453,.F.);
#58418=ADVANCED_FACE('',(#5318),#2454,.F.);
#58419=ADVANCED_FACE('',(#5319),#2455,.F.);
#58420=ADVANCED_FACE('',(#5320),#2456,.F.);
#58421=ADVANCED_FACE('',(#5321),#2457,.F.);
#58422=ADVANCED_FACE('',(#5322),#2458,.F.);
#58423=ADVANCED_FACE('',(#5323),#2459,.F.);
#58424=ADVANCED_FACE('',(#5324),#2460,.F.);
#58425=ADVANCED_FACE('',(#5325),#2461,.F.);
#58426=ADVANCED_FACE('',(#5326),#2462,.F.);
#58427=ADVANCED_FACE('',(#5327),#2463,.F.);
#58428=ADVANCED_FACE('',(#5328),#2464,.F.);
#58429=ADVANCED_FACE('',(#5329),#2465,.F.);
#58430=ADVANCED_FACE('',(#5330),#2466,.F.);
#58431=ADVANCED_FACE('',(#5331),#2467,.F.);
#58432=ADVANCED_FACE('',(#5332),#2468,.F.);
#58433=ADVANCED_FACE('',(#5333),#2469,.F.);
#58434=ADVANCED_FACE('',(#5334),#2470,.F.);
#58435=ADVANCED_FACE('',(#5335),#2471,.F.);
#58436=ADVANCED_FACE('',(#5336),#2472,.F.);
#58437=ADVANCED_FACE('',(#5337),#2473,.F.);
#58438=ADVANCED_FACE('',(#5338),#2474,.F.);
#58439=ADVANCED_FACE('',(#5339),#2475,.F.);
#58440=ADVANCED_FACE('',(#5340),#2476,.F.);
#58441=ADVANCED_FACE('',(#5341),#2477,.F.);
#58442=ADVANCED_FACE('',(#5342),#2478,.F.);
#58443=ADVANCED_FACE('',(#5343),#2479,.F.);
#58444=ADVANCED_FACE('',(#5344),#2480,.F.);
#58445=ADVANCED_FACE('',(#5345),#2481,.F.);
#58446=ADVANCED_FACE('',(#5346),#2482,.F.);
#58447=ADVANCED_FACE('',(#5347),#2483,.F.);
#58448=ADVANCED_FACE('',(#5348),#2484,.F.);
#58449=ADVANCED_FACE('',(#5349),#2485,.F.);
#58450=ADVANCED_FACE('',(#5350),#2486,.F.);
#58451=ADVANCED_FACE('',(#5351),#2487,.F.);
#58452=ADVANCED_FACE('',(#5352),#2488,.F.);
#58453=ADVANCED_FACE('',(#5353),#2489,.F.);
#58454=ADVANCED_FACE('',(#5354),#2490,.F.);
#58455=ADVANCED_FACE('',(#5355),#2491,.F.);
#58456=ADVANCED_FACE('',(#5356),#2492,.F.);
#58457=ADVANCED_FACE('',(#5357),#2493,.F.);
#58458=ADVANCED_FACE('',(#5358),#2494,.F.);
#58459=ADVANCED_FACE('',(#5359),#2495,.F.);
#58460=ADVANCED_FACE('',(#5360),#2496,.F.);
#58461=ADVANCED_FACE('',(#5361),#2497,.F.);
#58462=ADVANCED_FACE('',(#5362),#2498,.F.);
#58463=ADVANCED_FACE('',(#5363),#2499,.F.);
#58464=ADVANCED_FACE('',(#5364),#2500,.F.);
#58465=ADVANCED_FACE('',(#5365),#2501,.F.);
#58466=ADVANCED_FACE('',(#5366),#2502,.F.);
#58467=ADVANCED_FACE('',(#5367),#2503,.F.);
#58468=ADVANCED_FACE('',(#5368),#2504,.F.);
#58469=ADVANCED_FACE('',(#5369),#2505,.F.);
#58470=ADVANCED_FACE('',(#5370),#2506,.F.);
#58471=ADVANCED_FACE('',(#5371),#2507,.F.);
#58472=ADVANCED_FACE('',(#5372),#2508,.F.);
#58473=ADVANCED_FACE('',(#5373),#2509,.F.);
#58474=ADVANCED_FACE('',(#5374),#2510,.F.);
#58475=ADVANCED_FACE('',(#5375),#2511,.F.);
#58476=ADVANCED_FACE('',(#5376),#2512,.F.);
#58477=ADVANCED_FACE('',(#5377),#2513,.F.);
#58478=ADVANCED_FACE('',(#5378),#2514,.F.);
#58479=ADVANCED_FACE('',(#5379),#2515,.F.);
#58480=ADVANCED_FACE('',(#5380),#2516,.F.);
#58481=ADVANCED_FACE('',(#5381),#2517,.F.);
#58482=ADVANCED_FACE('',(#5382),#2518,.F.);
#58483=ADVANCED_FACE('',(#5383),#2519,.F.);
#58484=ADVANCED_FACE('',(#5384),#2520,.F.);
#58485=ADVANCED_FACE('',(#5385),#2521,.F.);
#58486=ADVANCED_FACE('',(#5386),#2522,.F.);
#58487=ADVANCED_FACE('',(#5387),#2523,.F.);
#58488=ADVANCED_FACE('',(#5388),#2524,.F.);
#58489=ADVANCED_FACE('',(#5389),#2525,.F.);
#58490=ADVANCED_FACE('',(#5390),#2526,.F.);
#58491=ADVANCED_FACE('',(#5391),#2527,.F.);
#58492=ADVANCED_FACE('',(#5392),#2528,.F.);
#58493=ADVANCED_FACE('',(#5393),#2529,.F.);
#58494=ADVANCED_FACE('',(#5394),#2530,.F.);
#58495=ADVANCED_FACE('',(#5395),#2531,.F.);
#58496=ADVANCED_FACE('',(#5396),#2532,.F.);
#58497=ADVANCED_FACE('',(#5397),#2533,.F.);
#58498=ADVANCED_FACE('',(#5398),#2534,.F.);
#58499=ADVANCED_FACE('',(#5399),#2535,.F.);
#58500=ADVANCED_FACE('',(#5400),#2536,.F.);
#58501=ADVANCED_FACE('',(#5401),#2537,.F.);
#58502=ADVANCED_FACE('',(#5402),#2538,.F.);
#58503=ADVANCED_FACE('',(#5403),#2539,.F.);
#58504=ADVANCED_FACE('',(#5404),#2540,.F.);
#58505=ADVANCED_FACE('',(#5405),#2541,.F.);
#58506=ADVANCED_FACE('',(#5406),#2542,.F.);
#58507=ADVANCED_FACE('',(#5407),#2543,.F.);
#58508=ADVANCED_FACE('',(#5408),#2544,.F.);
#58509=ADVANCED_FACE('',(#5409),#2545,.F.);
#58510=ADVANCED_FACE('',(#5410),#2546,.F.);
#58511=ADVANCED_FACE('',(#5411),#2547,.F.);
#58512=ADVANCED_FACE('',(#5412),#2548,.F.);
#58513=ADVANCED_FACE('',(#5413),#2549,.F.);
#58514=ADVANCED_FACE('',(#5414),#2550,.F.);
#58515=ADVANCED_FACE('',(#5415),#2551,.F.);
#58516=ADVANCED_FACE('',(#5416),#2552,.F.);
#58517=ADVANCED_FACE('',(#5417),#2553,.F.);
#58518=ADVANCED_FACE('',(#5418),#2554,.F.);
#58519=ADVANCED_FACE('',(#5419),#2555,.F.);
#58520=ADVANCED_FACE('',(#5420),#2556,.F.);
#58521=ADVANCED_FACE('',(#5421),#2557,.F.);
#58522=ADVANCED_FACE('',(#5422),#2558,.F.);
#58523=ADVANCED_FACE('',(#5423),#2559,.F.);
#58524=ADVANCED_FACE('',(#5424),#2560,.F.);
#58525=ADVANCED_FACE('',(#5425),#2561,.F.);
#58526=ADVANCED_FACE('',(#5426),#2562,.F.);
#58527=ADVANCED_FACE('',(#5427),#2563,.F.);
#58528=ADVANCED_FACE('',(#5428),#2564,.F.);
#58529=ADVANCED_FACE('',(#5429),#2565,.F.);
#58530=ADVANCED_FACE('',(#5430),#2566,.F.);
#58531=ADVANCED_FACE('',(#5431),#2567,.F.);
#58532=ADVANCED_FACE('',(#5432),#2568,.F.);
#58533=ADVANCED_FACE('',(#5433),#2569,.F.);
#58534=ADVANCED_FACE('',(#5434),#2570,.F.);
#58535=ADVANCED_FACE('',(#5435),#2571,.F.);
#58536=ADVANCED_FACE('',(#5436),#2572,.F.);
#58537=ADVANCED_FACE('',(#5437),#2573,.F.);
#58538=ADVANCED_FACE('',(#5438),#2574,.F.);
#58539=ADVANCED_FACE('',(#5439),#2575,.F.);
#58540=ADVANCED_FACE('',(#5440),#2576,.F.);
#58541=ADVANCED_FACE('',(#5441),#2577,.F.);
#58542=ADVANCED_FACE('',(#5442),#2578,.F.);
#58543=ADVANCED_FACE('',(#5443),#2579,.F.);
#58544=ADVANCED_FACE('',(#5444),#2580,.F.);
#58545=ADVANCED_FACE('',(#5445),#2581,.F.);
#58546=ADVANCED_FACE('',(#5446),#2582,.F.);
#58547=ADVANCED_FACE('',(#5447),#2583,.F.);
#58548=ADVANCED_FACE('',(#5448),#2584,.F.);
#58549=ADVANCED_FACE('',(#5449),#2585,.F.);
#58550=ADVANCED_FACE('',(#5450),#2586,.F.);
#58551=ADVANCED_FACE('',(#5451),#2587,.F.);
#58552=ADVANCED_FACE('',(#5452),#2588,.F.);
#58553=ADVANCED_FACE('',(#5453),#2589,.F.);
#58554=ADVANCED_FACE('',(#5454),#2590,.F.);
#58555=ADVANCED_FACE('',(#5455),#2591,.F.);
#58556=ADVANCED_FACE('',(#5456),#2592,.F.);
#58557=ADVANCED_FACE('',(#5457),#2593,.F.);
#58558=ADVANCED_FACE('',(#5458),#2594,.F.);
#58559=ADVANCED_FACE('',(#5459),#2595,.F.);
#58560=ADVANCED_FACE('',(#5460),#2596,.F.);
#58561=ADVANCED_FACE('',(#5461),#2597,.F.);
#58562=ADVANCED_FACE('',(#5462),#2598,.F.);
#58563=ADVANCED_FACE('',(#5463),#2599,.F.);
#58564=ADVANCED_FACE('',(#5464),#2600,.F.);
#58565=ADVANCED_FACE('',(#5465),#2601,.F.);
#58566=ADVANCED_FACE('',(#5466),#2602,.F.);
#58567=ADVANCED_FACE('',(#5467),#2603,.F.);
#58568=ADVANCED_FACE('',(#5468),#2604,.F.);
#58569=ADVANCED_FACE('',(#5469),#2605,.F.);
#58570=ADVANCED_FACE('',(#5470),#2606,.F.);
#58571=ADVANCED_FACE('',(#5471),#2607,.F.);
#58572=ADVANCED_FACE('',(#5472),#2608,.F.);
#58573=ADVANCED_FACE('',(#5473),#2609,.F.);
#58574=ADVANCED_FACE('',(#5474),#2610,.F.);
#58575=ADVANCED_FACE('',(#5475),#2611,.F.);
#58576=ADVANCED_FACE('',(#5476),#2612,.F.);
#58577=ADVANCED_FACE('',(#5477),#2613,.F.);
#58578=ADVANCED_FACE('',(#5478),#2614,.F.);
#58579=ADVANCED_FACE('',(#5479),#2615,.F.);
#58580=ADVANCED_FACE('',(#5480),#2616,.F.);
#58581=ADVANCED_FACE('',(#5481),#2617,.F.);
#58582=ADVANCED_FACE('',(#5482),#2618,.F.);
#58583=ADVANCED_FACE('',(#5483),#2619,.F.);
#58584=ADVANCED_FACE('',(#5484),#2620,.F.);
#58585=ADVANCED_FACE('',(#5485),#2621,.F.);
#58586=ADVANCED_FACE('',(#5486),#2622,.F.);
#58587=ADVANCED_FACE('',(#5487),#2623,.F.);
#58588=ADVANCED_FACE('',(#5488),#2624,.F.);
#58589=ADVANCED_FACE('',(#5489),#2625,.F.);
#58590=ADVANCED_FACE('',(#5490),#2626,.F.);
#58591=ADVANCED_FACE('',(#5491),#2627,.F.);
#58592=ADVANCED_FACE('',(#5492),#2628,.F.);
#58593=ADVANCED_FACE('',(#5493),#2629,.F.);
#58594=ADVANCED_FACE('',(#5494),#2630,.F.);
#58595=ADVANCED_FACE('',(#5495),#2631,.F.);
#58596=ADVANCED_FACE('',(#5496),#2632,.F.);
#58597=ADVANCED_FACE('',(#5497),#2633,.F.);
#58598=ADVANCED_FACE('',(#5498),#2634,.F.);
#58599=ADVANCED_FACE('',(#5499),#2635,.F.);
#58600=ADVANCED_FACE('',(#5500),#2636,.F.);
#58601=ADVANCED_FACE('',(#5501),#2637,.F.);
#58602=ADVANCED_FACE('',(#5502),#2638,.F.);
#58603=ADVANCED_FACE('',(#5503),#2639,.F.);
#58604=ADVANCED_FACE('',(#5504),#2640,.F.);
#58605=ADVANCED_FACE('',(#5505),#2641,.F.);
#58606=ADVANCED_FACE('',(#5506),#2642,.F.);
#58607=ADVANCED_FACE('',(#5507),#2643,.F.);
#58608=ADVANCED_FACE('',(#5508),#2644,.F.);
#58609=ADVANCED_FACE('',(#5509),#2645,.F.);
#58610=ADVANCED_FACE('',(#5510),#2646,.F.);
#58611=ADVANCED_FACE('',(#5511),#2647,.F.);
#58612=ADVANCED_FACE('',(#5512),#2648,.F.);
#58613=ADVANCED_FACE('',(#5513),#2649,.F.);
#58614=ADVANCED_FACE('',(#5514),#2650,.F.);
#58615=ADVANCED_FACE('',(#5515),#2651,.F.);
#58616=ADVANCED_FACE('',(#5516),#2652,.F.);
#58617=ADVANCED_FACE('',(#5517),#2653,.F.);
#58618=ADVANCED_FACE('',(#5518),#2654,.F.);
#58619=ADVANCED_FACE('',(#5519),#2655,.F.);
#58620=ADVANCED_FACE('',(#5520),#2656,.F.);
#58621=ADVANCED_FACE('',(#5521),#2657,.F.);
#58622=ADVANCED_FACE('',(#5522),#2658,.F.);
#58623=ADVANCED_FACE('',(#5523),#2659,.F.);
#58624=ADVANCED_FACE('',(#5524),#2660,.F.);
#58625=ADVANCED_FACE('',(#5525),#2661,.F.);
#58626=ADVANCED_FACE('',(#5526),#2662,.F.);
#58627=ADVANCED_FACE('',(#5527),#2663,.F.);
#58628=ADVANCED_FACE('',(#5528),#2664,.F.);
#58629=ADVANCED_FACE('',(#5529),#2665,.F.);
#58630=ADVANCED_FACE('',(#5530),#2666,.F.);
#58631=ADVANCED_FACE('',(#5531),#2667,.F.);
#58632=ADVANCED_FACE('',(#5532),#2668,.F.);
#58633=ADVANCED_FACE('',(#5533),#2669,.F.);
#58634=ADVANCED_FACE('',(#5534),#2670,.F.);
#58635=ADVANCED_FACE('',(#5535),#2671,.F.);
#58636=ADVANCED_FACE('',(#5536),#2672,.F.);
#58637=ADVANCED_FACE('',(#5537),#2673,.F.);
#58638=ADVANCED_FACE('',(#5538),#2674,.F.);
#58639=ADVANCED_FACE('',(#5539),#2675,.F.);
#58640=ADVANCED_FACE('',(#5540),#2676,.F.);
#58641=ADVANCED_FACE('',(#5541),#2677,.F.);
#58642=ADVANCED_FACE('',(#5542),#2678,.F.);
#58643=ADVANCED_FACE('',(#5543),#2679,.F.);
#58644=ADVANCED_FACE('',(#5544),#2680,.F.);
#58645=ADVANCED_FACE('',(#5545),#2681,.F.);
#58646=ADVANCED_FACE('',(#5546),#2682,.F.);
#58647=ADVANCED_FACE('',(#5547),#2683,.F.);
#58648=ADVANCED_FACE('',(#5548),#2684,.F.);
#58649=ADVANCED_FACE('',(#5549),#2685,.F.);
#58650=ADVANCED_FACE('',(#5550),#2686,.F.);
#58651=ADVANCED_FACE('',(#5551),#2687,.F.);
#58652=ADVANCED_FACE('',(#5552),#2688,.F.);
#58653=ADVANCED_FACE('',(#5553),#2689,.F.);
#58654=ADVANCED_FACE('',(#5554),#2690,.F.);
#58655=ADVANCED_FACE('',(#5555),#2691,.F.);
#58656=ADVANCED_FACE('',(#5556),#2692,.F.);
#58657=ADVANCED_FACE('',(#5557),#2693,.F.);
#58658=ADVANCED_FACE('',(#5558),#2694,.F.);
#58659=ADVANCED_FACE('',(#5559),#2695,.F.);
#58660=ADVANCED_FACE('',(#5560),#2696,.F.);
#58661=ADVANCED_FACE('',(#5561),#2697,.F.);
#58662=ADVANCED_FACE('',(#5562),#2698,.F.);
#58663=ADVANCED_FACE('',(#5563),#2699,.F.);
#58664=ADVANCED_FACE('',(#5564),#2700,.F.);
#58665=ADVANCED_FACE('',(#5565),#2701,.F.);
#58666=ADVANCED_FACE('',(#5566),#2702,.F.);
#58667=ADVANCED_FACE('',(#5567),#2703,.F.);
#58668=ADVANCED_FACE('',(#5568),#2704,.F.);
#58669=ADVANCED_FACE('',(#5569),#2705,.F.);
#58670=ADVANCED_FACE('',(#5570),#2706,.F.);
#58671=ADVANCED_FACE('',(#5571),#2707,.F.);
#58672=ADVANCED_FACE('',(#5572),#2708,.F.);
#58673=ADVANCED_FACE('',(#5573),#2709,.F.);
#58674=ADVANCED_FACE('',(#5574),#2710,.F.);
#58675=ADVANCED_FACE('',(#5575),#2711,.F.);
#58676=ADVANCED_FACE('',(#5576),#2712,.F.);
#58677=ADVANCED_FACE('',(#5577),#2713,.F.);
#58678=ADVANCED_FACE('',(#5578),#2714,.F.);
#58679=ADVANCED_FACE('',(#5579),#2715,.F.);
#58680=ADVANCED_FACE('',(#5580),#2716,.F.);
#58681=ADVANCED_FACE('',(#5581),#2717,.F.);
#58682=ADVANCED_FACE('',(#5582),#2718,.F.);
#58683=ADVANCED_FACE('',(#5583),#2719,.F.);
#58684=ADVANCED_FACE('',(#5584),#2720,.F.);
#58685=ADVANCED_FACE('',(#5585),#2721,.F.);
#58686=ADVANCED_FACE('',(#5586),#2722,.F.);
#58687=ADVANCED_FACE('',(#5587),#2723,.F.);
#58688=ADVANCED_FACE('',(#5588),#2724,.F.);
#58689=ADVANCED_FACE('',(#5589),#2725,.F.);
#58690=ADVANCED_FACE('',(#5590),#2726,.F.);
#58691=ADVANCED_FACE('',(#5591),#2727,.F.);
#58692=ADVANCED_FACE('',(#5592),#2728,.F.);
#58693=ADVANCED_FACE('',(#5593),#2729,.F.);
#58694=ADVANCED_FACE('',(#5594),#2730,.F.);
#58695=ADVANCED_FACE('',(#5595),#2731,.F.);
#58696=ADVANCED_FACE('',(#5596),#2732,.F.);
#58697=ADVANCED_FACE('',(#5597),#2733,.F.);
#58698=ADVANCED_FACE('',(#5598),#2734,.F.);
#58699=ADVANCED_FACE('',(#5599),#2735,.F.);
#58700=ADVANCED_FACE('',(#5600),#2736,.F.);
#58701=ADVANCED_FACE('',(#5601),#2737,.F.);
#58702=ADVANCED_FACE('',(#5602),#2738,.F.);
#58703=ADVANCED_FACE('',(#5603),#2739,.F.);
#58704=ADVANCED_FACE('',(#5604),#2740,.F.);
#58705=ADVANCED_FACE('',(#5605),#2741,.F.);
#58706=ADVANCED_FACE('',(#5606),#2742,.F.);
#58707=ADVANCED_FACE('',(#5607),#2743,.F.);
#58708=ADVANCED_FACE('',(#5608),#2744,.F.);
#58709=ADVANCED_FACE('',(#5609),#2745,.F.);
#58710=ADVANCED_FACE('',(#5610),#2746,.F.);
#58711=ADVANCED_FACE('',(#5611),#2747,.F.);
#58712=ADVANCED_FACE('',(#5612),#2748,.F.);
#58713=ADVANCED_FACE('',(#5613),#2749,.F.);
#58714=ADVANCED_FACE('',(#5614),#2750,.F.);
#58715=ADVANCED_FACE('',(#5615),#2751,.F.);
#58716=ADVANCED_FACE('',(#5616),#2752,.F.);
#58717=ADVANCED_FACE('',(#5617),#2753,.F.);
#58718=ADVANCED_FACE('',(#5618),#2754,.F.);
#58719=ADVANCED_FACE('',(#5619),#2755,.F.);
#58720=ADVANCED_FACE('',(#5620),#2756,.F.);
#58721=ADVANCED_FACE('',(#5621),#2757,.F.);
#58722=ADVANCED_FACE('',(#5622),#2758,.F.);
#58723=ADVANCED_FACE('',(#5623),#2759,.F.);
#58724=ADVANCED_FACE('',(#5624),#2760,.F.);
#58725=ADVANCED_FACE('',(#5625),#2761,.F.);
#58726=ADVANCED_FACE('',(#5626),#2762,.F.);
#58727=ADVANCED_FACE('',(#5627),#2763,.F.);
#58728=ADVANCED_FACE('',(#5628),#2764,.F.);
#58729=ADVANCED_FACE('',(#5629),#2765,.F.);
#58730=ADVANCED_FACE('',(#5630),#2766,.F.);
#58731=ADVANCED_FACE('',(#5631),#2767,.F.);
#58732=ADVANCED_FACE('',(#5632),#2768,.F.);
#58733=ADVANCED_FACE('',(#5633),#2769,.F.);
#58734=ADVANCED_FACE('',(#5634),#2770,.F.);
#58735=ADVANCED_FACE('',(#5635),#2771,.F.);
#58736=ADVANCED_FACE('',(#5636),#2772,.F.);
#58737=ADVANCED_FACE('',(#5637),#2773,.F.);
#58738=ADVANCED_FACE('',(#5638),#2774,.F.);
#58739=ADVANCED_FACE('',(#5639),#2775,.F.);
#58740=ADVANCED_FACE('',(#5640),#2776,.F.);
#58741=ADVANCED_FACE('',(#5641),#2777,.F.);
#58742=ADVANCED_FACE('',(#5642),#2778,.F.);
#58743=ADVANCED_FACE('',(#5643),#2779,.F.);
#58744=ADVANCED_FACE('',(#5644),#2780,.F.);
#58745=ADVANCED_FACE('',(#5645),#2781,.F.);
#58746=ADVANCED_FACE('',(#5646),#2782,.F.);
#58747=ADVANCED_FACE('',(#5647),#2783,.F.);
#58748=ADVANCED_FACE('',(#5648),#2784,.F.);
#58749=ADVANCED_FACE('',(#5649),#2785,.F.);
#58750=ADVANCED_FACE('',(#5650),#2786,.F.);
#58751=ADVANCED_FACE('',(#5651),#2787,.F.);
#58752=ADVANCED_FACE('',(#5652),#2788,.F.);
#58753=ADVANCED_FACE('',(#5653),#2789,.F.);
#58754=ADVANCED_FACE('',(#5654),#2790,.F.);
#58755=ADVANCED_FACE('',(#5655),#2791,.F.);
#58756=ADVANCED_FACE('',(#5656),#2792,.F.);
#58757=ADVANCED_FACE('',(#5657),#2793,.F.);
#58758=ADVANCED_FACE('',(#5658),#2794,.F.);
#58759=ADVANCED_FACE('',(#5659),#2795,.F.);
#58760=ADVANCED_FACE('',(#5660),#2796,.F.);
#58761=ADVANCED_FACE('',(#5661),#2797,.F.);
#58762=ADVANCED_FACE('',(#5662),#2798,.F.);
#58763=ADVANCED_FACE('',(#5663),#2799,.F.);
#58764=ADVANCED_FACE('',(#5664),#2800,.F.);
#58765=ADVANCED_FACE('',(#5665),#2801,.F.);
#58766=ADVANCED_FACE('',(#5666),#2802,.F.);
#58767=ADVANCED_FACE('',(#5667),#2803,.F.);
#58768=ADVANCED_FACE('',(#5668),#2804,.F.);
#58769=ADVANCED_FACE('',(#5669),#2805,.F.);
#58770=ADVANCED_FACE('',(#5670),#2806,.F.);
#58771=ADVANCED_FACE('',(#5671),#2807,.F.);
#58772=ADVANCED_FACE('',(#5672),#2808,.F.);
#58773=ADVANCED_FACE('',(#5673),#2809,.F.);
#58774=ADVANCED_FACE('',(#5674),#2810,.F.);
#58775=ADVANCED_FACE('',(#5675),#2811,.F.);
#58776=ADVANCED_FACE('',(#5676),#2812,.F.);
#58777=ADVANCED_FACE('',(#5677),#2813,.F.);
#58778=ADVANCED_FACE('',(#5678),#2814,.F.);
#58779=ADVANCED_FACE('',(#5679),#2815,.F.);
#58780=ADVANCED_FACE('',(#5680),#2816,.F.);
#58781=ADVANCED_FACE('',(#5681),#2817,.F.);
#58782=ADVANCED_FACE('',(#5682),#2818,.F.);
#58783=ADVANCED_FACE('',(#5683),#2819,.F.);
#58784=ADVANCED_FACE('',(#5684),#2820,.F.);
#58785=ADVANCED_FACE('',(#5685),#2821,.F.);
#58786=ADVANCED_FACE('',(#5686),#2822,.F.);
#58787=ADVANCED_FACE('',(#5687),#2823,.F.);
#58788=ADVANCED_FACE('',(#5688),#2824,.F.);
#58789=ADVANCED_FACE('',(#5689),#2825,.F.);
#58790=ADVANCED_FACE('',(#5690),#2826,.F.);
#58791=ADVANCED_FACE('',(#5691),#2827,.F.);
#58792=ADVANCED_FACE('',(#5692),#2828,.F.);
#58793=ADVANCED_FACE('',(#5693),#2829,.F.);
#58794=ADVANCED_FACE('',(#5694),#2830,.F.);
#58795=ADVANCED_FACE('',(#5695),#2831,.F.);
#58796=ADVANCED_FACE('',(#5696),#2832,.F.);
#58797=ADVANCED_FACE('',(#5697),#2833,.F.);
#58798=ADVANCED_FACE('',(#5698),#2834,.F.);
#58799=ADVANCED_FACE('',(#5699),#2835,.F.);
#58800=ADVANCED_FACE('',(#5700),#2836,.F.);
#58801=ADVANCED_FACE('',(#5701),#2837,.F.);
#58802=ADVANCED_FACE('',(#5702),#2838,.F.);
#58803=ADVANCED_FACE('',(#5703),#2839,.F.);
#58804=ADVANCED_FACE('',(#5704),#2840,.F.);
#58805=ADVANCED_FACE('',(#5705),#2841,.F.);
#58806=ADVANCED_FACE('',(#5706),#2842,.F.);
#58807=ADVANCED_FACE('',(#5707),#2843,.F.);
#58808=ADVANCED_FACE('',(#5708),#2844,.F.);
#58809=ADVANCED_FACE('',(#5709),#2845,.F.);
#58810=ADVANCED_FACE('',(#5710),#2846,.F.);
#58811=ADVANCED_FACE('',(#5711),#2847,.F.);
#58812=ADVANCED_FACE('',(#5712),#2848,.F.);
#58813=ADVANCED_FACE('',(#5713),#2849,.F.);
#58814=ADVANCED_FACE('',(#5714),#2850,.F.);
#58815=ADVANCED_FACE('',(#5715),#2851,.F.);
#58816=ADVANCED_FACE('',(#5716),#2852,.F.);
#58817=ADVANCED_FACE('',(#5717),#2853,.F.);
#58818=ADVANCED_FACE('',(#5718),#2854,.F.);
#58819=ADVANCED_FACE('',(#5719),#2855,.F.);
#58820=ADVANCED_FACE('',(#5720),#2856,.F.);
#58821=ADVANCED_FACE('',(#5721),#2857,.F.);
#58822=ADVANCED_FACE('',(#5722),#2858,.F.);
#58823=ADVANCED_FACE('',(#5723),#2859,.F.);
#58824=ADVANCED_FACE('',(#5724),#2860,.F.);
#58825=ADVANCED_FACE('',(#5725),#2861,.F.);
#58826=ADVANCED_FACE('',(#5726),#2862,.F.);
#58827=ADVANCED_FACE('',(#5727),#2863,.F.);
#58828=ADVANCED_FACE('',(#5728),#2864,.F.);
#58829=ADVANCED_FACE('',(#5729),#2865,.F.);
#58830=ADVANCED_FACE('',(#5730),#2866,.F.);
#58831=ADVANCED_FACE('',(#5731),#2867,.F.);
#58832=ADVANCED_FACE('',(#5732),#2868,.F.);
#58833=ADVANCED_FACE('',(#5733),#2869,.F.);
#58834=ADVANCED_FACE('',(#5734),#2870,.F.);
#58835=ADVANCED_FACE('',(#5735),#2871,.F.);
#58836=ADVANCED_FACE('',(#5736),#2872,.F.);
#58837=ADVANCED_FACE('',(#5737),#2873,.F.);
#58838=ADVANCED_FACE('',(#5738),#2874,.F.);
#58839=ADVANCED_FACE('',(#5739),#2875,.F.);
#58840=ADVANCED_FACE('',(#5740),#2876,.F.);
#58841=ADVANCED_FACE('',(#5741),#2877,.F.);
#58842=ADVANCED_FACE('',(#5742),#2878,.F.);
#58843=ADVANCED_FACE('',(#5743),#2879,.F.);
#58844=ADVANCED_FACE('',(#5744),#2880,.F.);
#58845=ADVANCED_FACE('',(#5745),#2881,.F.);
#58846=ADVANCED_FACE('',(#5746),#2882,.F.);
#58847=ADVANCED_FACE('',(#5747),#2883,.F.);
#58848=ADVANCED_FACE('',(#5748),#2884,.F.);
#58849=ADVANCED_FACE('',(#5749),#2885,.F.);
#58850=ADVANCED_FACE('',(#5750),#2886,.F.);
#58851=ADVANCED_FACE('',(#5751),#2887,.F.);
#58852=ADVANCED_FACE('',(#5752),#2888,.F.);
#58853=ADVANCED_FACE('',(#5753),#2889,.F.);
#58854=ADVANCED_FACE('',(#5754),#2890,.F.);
#58855=ADVANCED_FACE('',(#5755),#2891,.F.);
#58856=ADVANCED_FACE('',(#5756),#2892,.F.);
#58857=ADVANCED_FACE('',(#5757),#2893,.F.);
#58858=ADVANCED_FACE('',(#5758),#2894,.F.);
#58859=ADVANCED_FACE('',(#5759),#2895,.F.);
#58860=ADVANCED_FACE('',(#5760),#2896,.F.);
#58861=ADVANCED_FACE('',(#5761),#2897,.F.);
#58862=ADVANCED_FACE('',(#5762),#2898,.F.);
#58863=ADVANCED_FACE('',(#5763),#2899,.F.);
#58864=ADVANCED_FACE('',(#5764),#2900,.F.);
#58865=ADVANCED_FACE('',(#5765),#2901,.F.);
#58866=ADVANCED_FACE('',(#5766),#2902,.F.);
#58867=ADVANCED_FACE('',(#5767),#2903,.F.);
#58868=ADVANCED_FACE('',(#5768),#2904,.F.);
#58869=ADVANCED_FACE('',(#5769),#2905,.F.);
#58870=ADVANCED_FACE('',(#5770),#2906,.F.);
#58871=ADVANCED_FACE('',(#5771),#2907,.F.);
#58872=ADVANCED_FACE('',(#5772),#2908,.F.);
#58873=ADVANCED_FACE('',(#5773),#2909,.F.);
#58874=ADVANCED_FACE('',(#5774),#2910,.F.);
#58875=ADVANCED_FACE('',(#5775),#2911,.F.);
#58876=ADVANCED_FACE('',(#5776),#2912,.F.);
#58877=ADVANCED_FACE('',(#5777),#2913,.F.);
#58878=ADVANCED_FACE('',(#5778),#2914,.T.);
#58879=ADVANCED_FACE('',(#5779),#2915,.T.);
#58880=ADVANCED_FACE('',(#5780),#2916,.T.);
#58881=ADVANCED_FACE('',(#5781,#1571,#1572,#1573),#2917,.T.);
#58882=ADVANCED_FACE('',(#5782),#875,.F.);
#58883=ADVANCED_FACE('',(#5783),#876,.F.);
#58884=ADVANCED_FACE('',(#5784),#603,.F.);
#58885=ADVANCED_FACE('',(#5785),#604,.F.);
#58886=ADVANCED_FACE('',(#5786),#877,.F.);
#58887=ADVANCED_FACE('',(#5787),#605,.F.);
#58888=ADVANCED_FACE('',(#5788,#1574,#1575),#2918,.F.);
#58889=ADVANCED_FACE('',(#5789),#878,.F.);
#58890=ADVANCED_FACE('',(#5790),#879,.F.);
#58891=ADVANCED_FACE('',(#5791),#606,.F.);
#58892=ADVANCED_FACE('',(#5792),#880,.F.);
#58893=ADVANCED_FACE('',(#5793),#607,.F.);
#58894=ADVANCED_FACE('',(#5794,#1576),#2919,.T.);
#58895=ADVANCED_FACE('',(#5795),#608,.F.);
#58896=ADVANCED_FACE('',(#5796,#1577),#2920,.T.);
#58897=ADVANCED_FACE('',(#5797),#609,.F.);
#58898=ADVANCED_FACE('',(#5798,#1578),#2921,.T.);
#58899=ADVANCED_FACE('',(#5799),#610,.F.);
#58900=ADVANCED_FACE('',(#5800,#1579),#2922,.T.);
#58901=ADVANCED_FACE('',(#5801),#611,.F.);
#58902=ADVANCED_FACE('',(#5802,#1580),#2923,.T.);
#58903=ADVANCED_FACE('',(#5803),#612,.F.);
#58904=ADVANCED_FACE('',(#5804,#1581),#2924,.T.);
#58905=ADVANCED_FACE('',(#5805),#881,.F.);
#58906=ADVANCED_FACE('',(#5806,#1582,#1583,#1584),#2925,.T.);
#58907=ADVANCED_FACE('',(#5807),#613,.F.);
#58908=ADVANCED_FACE('',(#5808),#882,.F.);
#58909=ADVANCED_FACE('',(#5809),#614,.F.);
#58910=ADVANCED_FACE('',(#5810),#883,.F.);
#58911=ADVANCED_FACE('',(#5811),#615,.F.);
#58912=ADVANCED_FACE('',(#5812),#884,.F.);
#58913=ADVANCED_FACE('',(#5813),#616,.F.);
#58914=ADVANCED_FACE('',(#5814),#885,.F.);
#58915=ADVANCED_FACE('',(#5815),#617,.F.);
#58916=ADVANCED_FACE('',(#5816),#886,.F.);
#58917=ADVANCED_FACE('',(#5817),#618,.F.);
#58918=ADVANCED_FACE('',(#5818),#2926,.T.);
#58919=ADVANCED_FACE('',(#5819),#2927,.T.);
#58920=ADVANCED_FACE('',(#5820),#2928,.T.);
#58921=ADVANCED_FACE('',(#5821),#2929,.T.);
#58922=ADVANCED_FACE('',(#5822),#2930,.T.);
#58923=ADVANCED_FACE('',(#5823),#2931,.T.);
#58924=ADVANCED_FACE('',(#5824),#2932,.T.);
#58925=ADVANCED_FACE('',(#5825),#2933,.T.);
#58926=ADVANCED_FACE('',(#5826),#2934,.T.);
#58927=ADVANCED_FACE('',(#5827),#619,.F.);
#58928=ADVANCED_FACE('',(#5828),#2935,.T.);
#58929=ADVANCED_FACE('',(#5829),#2936,.T.);
#58930=ADVANCED_FACE('',(#5830),#2937,.T.);
#58931=ADVANCED_FACE('',(#5831),#2938,.F.);
#58932=ADVANCED_FACE('',(#5832),#2939,.F.);
#58933=ADVANCED_FACE('',(#5833),#2940,.T.);
#58934=ADVANCED_FACE('',(#5834),#2941,.T.);
#58935=ADVANCED_FACE('',(#5835),#2942,.T.);
#58936=ADVANCED_FACE('',(#5836),#2943,.T.);
#58937=ADVANCED_FACE('',(#5837),#2944,.T.);
#58938=ADVANCED_FACE('',(#5838),#2945,.T.);
#58939=ADVANCED_FACE('',(#5839),#2946,.T.);
#58940=ADVANCED_FACE('',(#5840),#2947,.T.);
#58941=ADVANCED_FACE('',(#5841,#1585,#1586,#1587,#1588),#2948,.T.);
#58942=ADVANCED_FACE('',(#5842),#2949,.T.);
#58943=ADVANCED_FACE('',(#5843),#2950,.T.);
#58944=ADVANCED_FACE('',(#5844),#2951,.T.);
#58945=ADVANCED_FACE('',(#5845),#2952,.T.);
#58946=ADVANCED_FACE('',(#5846,#1589,#1590,#1591,#1592,#1593,#1594,#1595,
#1596,#1597,#1598,#1599,#1600,#1601,#1602,#1603,#1604,#1605,#1606,#1607,
#1608,#1609,#1610,#1611,#1612,#1613,#1614,#1615,#1616,#1617,#1618,#1619,
#1620,#1621,#1622,#1623,#1624,#1625,#1626,#1627,#1628,#1629,#1630,#1631,
#1632,#1633,#1634,#1635,#1636,#1637,#1638,#1639,#1640,#1641,#1642,#1643,
#1644,#1645,#1646,#1647,#1648,#1649,#1650,#1651,#1652,#1653,#1654,#1655,
#1656,#1657,#1658,#1659,#1660,#1661,#1662,#1663,#1664,#1665,#1666,#1667,
#1668,#1669,#1670,#1671,#1672,#1673,#1674,#1675,#1676,#1677,#1678,#1679,
#1680,#1681,#1682,#1683,#1684,#1685,#1686,#1687,#1688,#1689,#1690,#1691,
#1692,#1693,#1694,#1695,#1696,#1697,#1698,#1699,#1700,#1701,#1702,#1703,
#1704,#1705,#1706,#1707,#1708,#1709,#1710,#1711,#1712,#1713,#1714,#1715,
#1716,#1717,#1718,#1719,#1720,#1721,#1722,#1723,#1724,#1725,#1726,#1727,
#1728,#1729,#1730,#1731,#1732,#1733,#1734,#1735,#1736,#1737,#1738,#1739,
#1740,#1741,#1742,#1743,#1744,#1745,#1746,#1747,#1748,#1749,#1750,#1751,
#1752,#1753,#1754,#1755,#1756,#1757,#1758,#1759,#1760,#1761,#1762,#1763,
#1764,#1765,#1766,#1767,#1768,#1769,#1770,#1771,#1772,#1773,#1774,#1775,
#1776,#1777,#1778,#1779,#1780,#1781,#1782,#1783,#1784,#1785,#1786,#1787,
#1788,#1789,#1790,#1791,#1792,#1793,#1794,#1795,#1796,#1797,#1798,#1799,
#1800,#1801,#1802,#1803,#1804,#1805,#1806),#2953,.T.);
#58947=ADVANCED_FACE('',(#5847),#2954,.T.);
#58948=ADVANCED_FACE('',(#5848,#1807,#1808,#1809,#1810),#2955,.T.);
#58949=ADVANCED_FACE('',(#5849),#2956,.T.);
#58950=ADVANCED_FACE('',(#5850),#2957,.T.);
#58951=ADVANCED_FACE('',(#5851),#2958,.T.);
#58952=ADVANCED_FACE('',(#5852),#2959,.T.);
#58953=ADVANCED_FACE('',(#5853),#2960,.T.);
#58954=ADVANCED_FACE('',(#5854),#2961,.T.);
#58955=ADVANCED_FACE('',(#5855),#2962,.T.);
#58956=ADVANCED_FACE('',(#5856),#2963,.T.);
#58957=ADVANCED_FACE('',(#5857),#2964,.T.);
#58958=ADVANCED_FACE('',(#5858),#2965,.T.);
#58959=ADVANCED_FACE('',(#5859),#2966,.T.);
#58960=ADVANCED_FACE('',(#5860),#2967,.T.);
#58961=ADVANCED_FACE('',(#5861),#2968,.T.);
#58962=ADVANCED_FACE('',(#5862),#2969,.T.);
#58963=ADVANCED_FACE('',(#5863),#2970,.T.);
#58964=ADVANCED_FACE('',(#5864),#2971,.T.);
#58965=ADVANCED_FACE('',(#5865),#2972,.T.);
#58966=ADVANCED_FACE('',(#5866),#2973,.T.);
#58967=ADVANCED_FACE('',(#5867),#2974,.T.);
#58968=ADVANCED_FACE('',(#5868),#2975,.T.);
#58969=ADVANCED_FACE('',(#5869),#620,.F.);
#58970=ADVANCED_FACE('',(#5870),#2976,.T.);
#58971=ADVANCED_FACE('',(#5871),#2977,.T.);
#58972=ADVANCED_FACE('',(#5872),#887,.F.);
#58973=ADVANCED_FACE('',(#5873),#888,.F.);
#58974=ADVANCED_FACE('',(#5874,#1811),#2978,.T.);
#58975=ADVANCED_FACE('',(#5875),#621,.F.);
#58976=ADVANCED_FACE('',(#5876),#889,.F.);
#58977=ADVANCED_FACE('',(#5877),#622,.F.);
#58978=ADVANCED_FACE('',(#5878),#890,.F.);
#58979=ADVANCED_FACE('',(#5879),#891,.F.);
#58980=ADVANCED_FACE('',(#5880),#892,.F.);
#58981=ADVANCED_FACE('',(#5881),#2979,.T.);
#58982=ADVANCED_FACE('',(#5882),#623,.F.);
#58983=ADVANCED_FACE('',(#5883),#893,.F.);
#58984=ADVANCED_FACE('',(#5884),#624,.F.);
#58985=ADVANCED_FACE('',(#5885),#894,.F.);
#58986=ADVANCED_FACE('',(#5886),#625,.F.);
#58987=ADVANCED_FACE('',(#5887),#2980,.T.);
#58988=ADVANCED_FACE('',(#5888),#895,.F.);
#58989=ADVANCED_FACE('',(#5889),#2981,.T.);
#58990=ADVANCED_FACE('',(#5890),#626,.F.);
#58991=ADVANCED_FACE('',(#5891),#896,.F.);
#58992=ADVANCED_FACE('',(#5892,#1812,#1813,#1814,#1815,#1816,#1817),#2982,
 .T.);
#58993=ADVANCED_FACE('',(#5893),#627,.F.);
#58994=ADVANCED_FACE('',(#5894),#897,.F.);
#58995=ADVANCED_FACE('',(#5895),#628,.F.);
#58996=ADVANCED_FACE('',(#5896),#2983,.T.);
#58997=ADVANCED_FACE('',(#5897),#2984,.T.);
#58998=ADVANCED_FACE('',(#5898),#2985,.T.);
#58999=ADVANCED_FACE('',(#5899),#2986,.T.);
#59000=ADVANCED_FACE('',(#5900),#2987,.T.);
#59001=ADVANCED_FACE('',(#5901),#2988,.T.);
#59002=ADVANCED_FACE('',(#5902),#898,.F.);
#59003=ADVANCED_FACE('',(#5903),#629,.F.);
#59004=ADVANCED_FACE('',(#5904),#899,.F.);
#59005=ADVANCED_FACE('',(#5905),#630,.F.);
#59006=ADVANCED_FACE('',(#5906),#900,.F.);
#59007=ADVANCED_FACE('',(#5907),#631,.F.);
#59008=ADVANCED_FACE('',(#5908),#901,.F.);
#59009=ADVANCED_FACE('',(#5909),#632,.F.);
#59010=ADVANCED_FACE('',(#5910),#902,.F.);
#59011=ADVANCED_FACE('',(#5911),#903,.F.);
#59012=ADVANCED_FACE('',(#5912),#904,.F.);
#59013=ADVANCED_FACE('',(#5913),#905,.F.);
#59014=ADVANCED_FACE('',(#5914),#906,.F.);
#59015=ADVANCED_FACE('',(#5915),#633,.F.);
#59016=ADVANCED_FACE('',(#5916),#907,.F.);
#59017=ADVANCED_FACE('',(#5917),#634,.F.);
#59018=ADVANCED_FACE('',(#5918,#1818),#2989,.T.);
#59019=ADVANCED_FACE('',(#5919),#2990,.F.);
#59020=ADVANCED_FACE('',(#5920),#2991,.F.);
#59021=ADVANCED_FACE('',(#5921),#2992,.F.);
#59022=ADVANCED_FACE('',(#5922),#2993,.F.);
#59023=ADVANCED_FACE('',(#5923),#2994,.F.);
#59024=ADVANCED_FACE('',(#5924),#2995,.F.);
#59025=ADVANCED_FACE('',(#5925,#1819,#1820,#1821),#2996,.F.);
#59026=ADVANCED_FACE('',(#5926),#2997,.F.);
#59027=ADVANCED_FACE('',(#5927),#2998,.T.);
#59028=ADVANCED_FACE('',(#5928),#2999,.T.);
#59029=ADVANCED_FACE('',(#5929),#3000,.T.);
#59030=ADVANCED_FACE('',(#5930),#3001,.T.);
#59031=ADVANCED_FACE('',(#5931),#3002,.T.);
#59032=ADVANCED_FACE('',(#5932),#3003,.T.);
#59033=ADVANCED_FACE('',(#5933),#3004,.T.);
#59034=ADVANCED_FACE('',(#5934),#3005,.T.);
#59035=ADVANCED_FACE('',(#5935),#3006,.T.);
#59036=ADVANCED_FACE('',(#5936),#3007,.T.);
#59037=ADVANCED_FACE('',(#5937),#3008,.T.);
#59038=ADVANCED_FACE('',(#5938),#3009,.T.);
#59039=ADVANCED_FACE('',(#5939),#3010,.T.);
#59040=ADVANCED_FACE('',(#5940),#3011,.T.);
#59041=ADVANCED_FACE('',(#5941),#3012,.T.);
#59042=ADVANCED_FACE('',(#5942),#3013,.T.);
#59043=ADVANCED_FACE('',(#5943),#3014,.T.);
#59044=ADVANCED_FACE('',(#5944),#3015,.T.);
#59045=ADVANCED_FACE('',(#5945),#3016,.T.);
#59046=ADVANCED_FACE('',(#5946),#3017,.T.);
#59047=ADVANCED_FACE('',(#5947),#3018,.T.);
#59048=ADVANCED_FACE('',(#5948),#3019,.T.);
#59049=ADVANCED_FACE('',(#5949),#3020,.T.);
#59050=ADVANCED_FACE('',(#5950),#908,.F.);
#59051=ADVANCED_FACE('',(#5951),#909,.F.);
#59052=ADVANCED_FACE('',(#5952),#910,.F.);
#59053=ADVANCED_FACE('',(#5953),#3021,.T.);
#59054=ADVANCED_FACE('',(#5954),#3022,.T.);
#59055=ADVANCED_FACE('',(#5955),#3023,.T.);
#59056=ADVANCED_FACE('',(#5956),#3024,.T.);
#59057=ADVANCED_FACE('',(#5957),#3025,.T.);
#59058=ADVANCED_FACE('',(#5958),#3026,.T.);
#59059=ADVANCED_FACE('',(#5959),#3027,.T.);
#59060=ADVANCED_FACE('',(#5960),#3028,.T.);
#59061=ADVANCED_FACE('',(#5961),#3029,.T.);
#59062=ADVANCED_FACE('',(#5962),#3030,.T.);
#59063=ADVANCED_FACE('',(#5963),#3031,.T.);
#59064=ADVANCED_FACE('',(#5964,#1822,#1823,#1824),#3032,.T.);
#59065=ADVANCED_FACE('',(#5965),#3033,.F.);
#59066=ADVANCED_FACE('',(#5966),#3034,.T.);
#59067=ADVANCED_FACE('',(#5967),#3035,.F.);
#59068=ADVANCED_FACE('',(#5968),#3036,.F.);
#59069=ADVANCED_FACE('',(#5969),#3037,.T.);
#59070=ADVANCED_FACE('',(#5970),#3038,.F.);
#59071=ADVANCED_FACE('',(#5971),#3039,.F.);
#59072=ADVANCED_FACE('',(#5972),#3040,.T.);
#59073=ADVANCED_FACE('',(#5973),#3041,.T.);
#59074=ADVANCED_FACE('',(#5974),#911,.T.);
#59075=ADVANCED_FACE('',(#5975,#1825,#1826),#635,.T.);
#59076=ADVANCED_FACE('',(#5976),#912,.T.);
#59077=ADVANCED_FACE('',(#5977),#3042,.T.);
#59078=ADVANCED_FACE('',(#5978),#3043,.T.);
#59079=ADVANCED_FACE('',(#5979),#636,.F.);
#59080=ADVANCED_FACE('',(#5980),#3044,.T.);
#59081=ADVANCED_FACE('',(#5981),#3045,.T.);
#59082=ADVANCED_FACE('',(#5982),#3046,.T.);
#59083=ADVANCED_FACE('',(#5983),#110,.T.);
#59084=ADVANCED_FACE('',(#5984),#637,.T.);
#59085=ADVANCED_FACE('',(#5985),#111,.T.);
#59086=ADVANCED_FACE('',(#5986),#3047,.T.);
#59087=ADVANCED_FACE('',(#5987),#638,.T.);
#59088=ADVANCED_FACE('',(#5988),#3048,.T.);
#59089=ADVANCED_FACE('',(#5989),#3049,.T.);
#59090=ADVANCED_FACE('',(#5990),#112,.T.);
#59091=ADVANCED_FACE('',(#5991),#639,.T.);
#59092=ADVANCED_FACE('',(#5992),#113,.T.);
#59093=ADVANCED_FACE('',(#5993),#3050,.T.);
#59094=ADVANCED_FACE('',(#5994),#3051,.T.);
#59095=ADVANCED_FACE('',(#5995),#3052,.T.);
#59096=ADVANCED_FACE('',(#5996),#114,.T.);
#59097=ADVANCED_FACE('',(#5997),#640,.T.);
#59098=ADVANCED_FACE('',(#5998),#115,.T.);
#59099=ADVANCED_FACE('',(#5999),#3053,.T.);
#59100=ADVANCED_FACE('',(#6000),#3054,.T.);
#59101=ADVANCED_FACE('',(#6001),#3055,.T.);
#59102=ADVANCED_FACE('',(#6002),#116,.T.);
#59103=ADVANCED_FACE('',(#6003),#641,.T.);
#59104=ADVANCED_FACE('',(#6004),#117,.T.);
#59105=ADVANCED_FACE('',(#6005),#3056,.T.);
#59106=ADVANCED_FACE('',(#6006),#3057,.T.);
#59107=ADVANCED_FACE('',(#6007),#3058,.T.);
#59108=ADVANCED_FACE('',(#6008),#118,.T.);
#59109=ADVANCED_FACE('',(#6009),#642,.T.);
#59110=ADVANCED_FACE('',(#6010),#119,.T.);
#59111=ADVANCED_FACE('',(#6011),#3059,.T.);
#59112=ADVANCED_FACE('',(#6012),#3060,.T.);
#59113=ADVANCED_FACE('',(#6013),#3061,.T.);
#59114=ADVANCED_FACE('',(#6014),#120,.T.);
#59115=ADVANCED_FACE('',(#6015),#643,.T.);
#59116=ADVANCED_FACE('',(#6016),#121,.T.);
#59117=ADVANCED_FACE('',(#6017),#3062,.T.);
#59118=ADVANCED_FACE('',(#6018),#3063,.T.);
#59119=ADVANCED_FACE('',(#6019),#3064,.T.);
#59120=ADVANCED_FACE('',(#6020),#122,.T.);
#59121=ADVANCED_FACE('',(#6021),#644,.T.);
#59122=ADVANCED_FACE('',(#6022),#123,.T.);
#59123=ADVANCED_FACE('',(#6023),#3065,.T.);
#59124=ADVANCED_FACE('',(#6024),#3066,.T.);
#59125=ADVANCED_FACE('',(#6025),#3067,.T.);
#59126=ADVANCED_FACE('',(#6026),#124,.T.);
#59127=ADVANCED_FACE('',(#6027),#645,.T.);
#59128=ADVANCED_FACE('',(#6028),#125,.T.);
#59129=ADVANCED_FACE('',(#6029),#3068,.T.);
#59130=ADVANCED_FACE('',(#6030),#3069,.T.);
#59131=ADVANCED_FACE('',(#6031),#3070,.T.);
#59132=ADVANCED_FACE('',(#6032),#126,.T.);
#59133=ADVANCED_FACE('',(#6033),#646,.T.);
#59134=ADVANCED_FACE('',(#6034),#127,.T.);
#59135=ADVANCED_FACE('',(#6035),#3071,.T.);
#59136=ADVANCED_FACE('',(#6036),#3072,.T.);
#59137=ADVANCED_FACE('',(#6037),#3073,.T.);
#59138=ADVANCED_FACE('',(#6038),#128,.T.);
#59139=ADVANCED_FACE('',(#6039),#647,.T.);
#59140=ADVANCED_FACE('',(#6040),#129,.T.);
#59141=ADVANCED_FACE('',(#6041),#3074,.T.);
#59142=ADVANCED_FACE('',(#6042),#3075,.T.);
#59143=ADVANCED_FACE('',(#6043),#3076,.T.);
#59144=ADVANCED_FACE('',(#6044),#130,.T.);
#59145=ADVANCED_FACE('',(#6045),#648,.T.);
#59146=ADVANCED_FACE('',(#6046),#131,.T.);
#59147=ADVANCED_FACE('',(#6047),#3077,.T.);
#59148=ADVANCED_FACE('',(#6048),#3078,.T.);
#59149=ADVANCED_FACE('',(#6049),#3079,.T.);
#59150=ADVANCED_FACE('',(#6050),#132,.T.);
#59151=ADVANCED_FACE('',(#6051),#649,.T.);
#59152=ADVANCED_FACE('',(#6052),#133,.T.);
#59153=ADVANCED_FACE('',(#6053),#3080,.T.);
#59154=ADVANCED_FACE('',(#6054),#3081,.T.);
#59155=ADVANCED_FACE('',(#6055),#3082,.T.);
#59156=ADVANCED_FACE('',(#6056),#134,.T.);
#59157=ADVANCED_FACE('',(#6057),#650,.T.);
#59158=ADVANCED_FACE('',(#6058),#135,.T.);
#59159=ADVANCED_FACE('',(#6059),#3083,.T.);
#59160=ADVANCED_FACE('',(#6060),#3084,.T.);
#59161=ADVANCED_FACE('',(#6061),#3085,.T.);
#59162=ADVANCED_FACE('',(#6062),#136,.T.);
#59163=ADVANCED_FACE('',(#6063),#651,.T.);
#59164=ADVANCED_FACE('',(#6064),#137,.T.);
#59165=ADVANCED_FACE('',(#6065),#3086,.T.);
#59166=ADVANCED_FACE('',(#6066),#3087,.T.);
#59167=ADVANCED_FACE('',(#6067),#3088,.T.);
#59168=ADVANCED_FACE('',(#6068),#138,.T.);
#59169=ADVANCED_FACE('',(#6069),#652,.T.);
#59170=ADVANCED_FACE('',(#6070),#139,.T.);
#59171=ADVANCED_FACE('',(#6071),#3089,.T.);
#59172=ADVANCED_FACE('',(#6072),#3090,.T.);
#59173=ADVANCED_FACE('',(#6073),#140,.T.);
#59174=ADVANCED_FACE('',(#6074),#653,.T.);
#59175=ADVANCED_FACE('',(#6075),#141,.T.);
#59176=ADVANCED_FACE('',(#6076),#3091,.T.);
#59177=ADVANCED_FACE('',(#6077),#3092,.T.);
#59178=ADVANCED_FACE('',(#6078,#1827),#654,.F.);
#59179=ADVANCED_FACE('',(#6079,#1828),#3093,.T.);
#59180=ADVANCED_FACE('',(#6080,#1829),#3094,.T.);
#59181=ADVANCED_FACE('',(#6081,#1830),#655,.T.);
#59182=ADVANCED_FACE('',(#6082),#913,.T.);
#59183=ADVANCED_FACE('',(#6083,#1831),#3095,.T.);
#59184=ADVANCED_FACE('',(#6084),#3096,.T.);
#59185=ADVANCED_FACE('',(#6085),#656,.F.);
#59186=ADVANCED_FACE('',(#6086),#3097,.T.);
#59187=ADVANCED_FACE('',(#6087),#3098,.F.);
#59188=ADVANCED_FACE('',(#6088),#3099,.F.);
#59189=ADVANCED_FACE('',(#6089),#914,.T.);
#59190=ADVANCED_FACE('',(#6090),#657,.T.);
#59191=ADVANCED_FACE('',(#6091),#658,.T.);
#59192=ADVANCED_FACE('',(#6092),#3100,.F.);
#59193=ADVANCED_FACE('',(#6093),#3101,.F.);
#59194=ADVANCED_FACE('',(#6094),#659,.T.);
#59195=ADVANCED_FACE('',(#6095),#915,.T.);
#59196=ADVANCED_FACE('',(#6096),#3102,.F.);
#59197=ADVANCED_FACE('',(#6097),#3103,.F.);
#59198=ADVANCED_FACE('',(#6098),#3104,.F.);
#59199=ADVANCED_FACE('',(#6099),#3105,.F.);
#59200=ADVANCED_FACE('',(#6100),#660,.T.);
#59201=ADVANCED_FACE('',(#6101),#661,.T.);
#59202=ADVANCED_FACE('',(#6102),#3106,.F.);
#59203=ADVANCED_FACE('',(#6103),#3107,.F.);
#59204=ADVANCED_FACE('',(#6104),#662,.T.);
#59205=ADVANCED_FACE('',(#6105),#3108,.F.);
#59206=ADVANCED_FACE('',(#6106),#3109,.F.);
#59207=ADVANCED_FACE('',(#6107),#3110,.F.);
#59208=ADVANCED_FACE('',(#6108),#3111,.F.);
#59209=ADVANCED_FACE('',(#6109),#663,.T.);
#59210=ADVANCED_FACE('',(#6110),#664,.T.);
#59211=ADVANCED_FACE('',(#6111),#3112,.F.);
#59212=ADVANCED_FACE('',(#6112),#3113,.F.);
#59213=ADVANCED_FACE('',(#6113),#665,.T.);
#59214=ADVANCED_FACE('',(#6114),#3114,.F.);
#59215=ADVANCED_FACE('',(#6115),#3115,.F.);
#59216=ADVANCED_FACE('',(#6116),#3116,.F.);
#59217=ADVANCED_FACE('',(#6117),#3117,.F.);
#59218=ADVANCED_FACE('',(#6118),#666,.T.);
#59219=ADVANCED_FACE('',(#6119),#667,.T.);
#59220=ADVANCED_FACE('',(#6120),#3118,.F.);
#59221=ADVANCED_FACE('',(#6121),#3119,.F.);
#59222=ADVANCED_FACE('',(#6122),#668,.T.);
#59223=ADVANCED_FACE('',(#6123),#3120,.F.);
#59224=ADVANCED_FACE('',(#6124),#3121,.F.);
#59225=ADVANCED_FACE('',(#6125),#3122,.F.);
#59226=ADVANCED_FACE('',(#6126),#3123,.F.);
#59227=ADVANCED_FACE('',(#6127),#669,.T.);
#59228=ADVANCED_FACE('',(#6128),#670,.T.);
#59229=ADVANCED_FACE('',(#6129),#3124,.F.);
#59230=ADVANCED_FACE('',(#6130),#3125,.F.);
#59231=ADVANCED_FACE('',(#6131),#671,.T.);
#59232=ADVANCED_FACE('',(#6132),#3126,.F.);
#59233=ADVANCED_FACE('',(#6133),#3127,.F.);
#59234=ADVANCED_FACE('',(#6134),#3128,.F.);
#59235=ADVANCED_FACE('',(#6135),#3129,.F.);
#59236=ADVANCED_FACE('',(#6136),#672,.T.);
#59237=ADVANCED_FACE('',(#6137),#673,.T.);
#59238=ADVANCED_FACE('',(#6138),#3130,.F.);
#59239=ADVANCED_FACE('',(#6139),#3131,.F.);
#59240=ADVANCED_FACE('',(#6140),#674,.T.);
#59241=ADVANCED_FACE('',(#6141),#3132,.F.);
#59242=ADVANCED_FACE('',(#6142),#3133,.F.);
#59243=ADVANCED_FACE('',(#6143),#3134,.F.);
#59244=ADVANCED_FACE('',(#6144),#3135,.F.);
#59245=ADVANCED_FACE('',(#6145),#675,.T.);
#59246=ADVANCED_FACE('',(#6146),#676,.T.);
#59247=ADVANCED_FACE('',(#6147),#3136,.F.);
#59248=ADVANCED_FACE('',(#6148),#3137,.F.);
#59249=ADVANCED_FACE('',(#6149),#677,.T.);
#59250=ADVANCED_FACE('',(#6150),#3138,.F.);
#59251=ADVANCED_FACE('',(#6151),#3139,.F.);
#59252=ADVANCED_FACE('',(#6152),#3140,.F.);
#59253=ADVANCED_FACE('',(#6153),#3141,.F.);
#59254=ADVANCED_FACE('',(#6154),#678,.T.);
#59255=ADVANCED_FACE('',(#6155),#679,.T.);
#59256=ADVANCED_FACE('',(#6156),#3142,.F.);
#59257=ADVANCED_FACE('',(#6157),#3143,.F.);
#59258=ADVANCED_FACE('',(#6158),#680,.T.);
#59259=ADVANCED_FACE('',(#6159),#3144,.F.);
#59260=ADVANCED_FACE('',(#6160),#3145,.F.);
#59261=ADVANCED_FACE('',(#6161),#3146,.F.);
#59262=ADVANCED_FACE('',(#6162),#3147,.F.);
#59263=ADVANCED_FACE('',(#6163),#681,.T.);
#59264=ADVANCED_FACE('',(#6164),#682,.T.);
#59265=ADVANCED_FACE('',(#6165),#3148,.F.);
#59266=ADVANCED_FACE('',(#6166),#3149,.F.);
#59267=ADVANCED_FACE('',(#6167),#683,.T.);
#59268=ADVANCED_FACE('',(#6168),#3150,.F.);
#59269=ADVANCED_FACE('',(#6169),#3151,.F.);
#59270=ADVANCED_FACE('',(#6170),#3152,.F.);
#59271=ADVANCED_FACE('',(#6171),#3153,.F.);
#59272=ADVANCED_FACE('',(#6172),#684,.T.);
#59273=ADVANCED_FACE('',(#6173),#685,.T.);
#59274=ADVANCED_FACE('',(#6174),#3154,.F.);
#59275=ADVANCED_FACE('',(#6175),#3155,.F.);
#59276=ADVANCED_FACE('',(#6176),#686,.T.);
#59277=ADVANCED_FACE('',(#6177),#3156,.F.);
#59278=ADVANCED_FACE('',(#6178),#3157,.F.);
#59279=ADVANCED_FACE('',(#6179),#3158,.F.);
#59280=ADVANCED_FACE('',(#6180),#3159,.F.);
#59281=ADVANCED_FACE('',(#6181),#687,.T.);
#59282=ADVANCED_FACE('',(#6182),#688,.T.);
#59283=ADVANCED_FACE('',(#6183),#3160,.F.);
#59284=ADVANCED_FACE('',(#6184),#3161,.F.);
#59285=ADVANCED_FACE('',(#6185),#689,.T.);
#59286=ADVANCED_FACE('',(#6186),#3162,.F.);
#59287=ADVANCED_FACE('',(#6187),#3163,.F.);
#59288=ADVANCED_FACE('',(#6188),#3164,.F.);
#59289=ADVANCED_FACE('',(#6189),#3165,.F.);
#59290=ADVANCED_FACE('',(#6190),#690,.T.);
#59291=ADVANCED_FACE('',(#6191),#691,.T.);
#59292=ADVANCED_FACE('',(#6192),#3166,.F.);
#59293=ADVANCED_FACE('',(#6193),#3167,.F.);
#59294=ADVANCED_FACE('',(#6194),#692,.T.);
#59295=ADVANCED_FACE('',(#6195),#3168,.F.);
#59296=ADVANCED_FACE('',(#6196),#3169,.F.);
#59297=ADVANCED_FACE('',(#6197),#3170,.F.);
#59298=ADVANCED_FACE('',(#6198),#3171,.F.);
#59299=ADVANCED_FACE('',(#6199),#693,.T.);
#59300=ADVANCED_FACE('',(#6200),#694,.T.);
#59301=ADVANCED_FACE('',(#6201),#3172,.F.);
#59302=ADVANCED_FACE('',(#6202),#3173,.F.);
#59303=ADVANCED_FACE('',(#6203),#695,.T.);
#59304=ADVANCED_FACE('',(#6204),#3174,.F.);
#59305=ADVANCED_FACE('',(#6205),#3175,.F.);
#59306=ADVANCED_FACE('',(#6206),#3176,.F.);
#59307=ADVANCED_FACE('',(#6207),#3177,.F.);
#59308=ADVANCED_FACE('',(#6208),#916,.F.);
#59309=ADVANCED_FACE('',(#6209,#1832),#3178,.T.);
#59310=ADVANCED_FACE('',(#6210),#917,.T.);
#59311=ADVANCED_FACE('',(#6211),#696,.T.);
#59312=ADVANCED_FACE('',(#6212),#918,.T.);
#59313=ADVANCED_FACE('',(#6213,#1833),#3179,.T.);
#59314=ADVANCED_FACE('',(#6214,#1834),#697,.T.);
#59315=ADVANCED_FACE('',(#6215),#919,.T.);
#59316=ADVANCED_FACE('',(#6216,#1835),#3180,.T.);
#59317=ADVANCED_FACE('',(#6217),#698,.T.);
#59318=ADVANCED_FACE('',(#6218,#1836),#3181,.T.);
#59319=ADVANCED_FACE('',(#6219),#920,.F.);
#59320=ADVANCED_FACE('',(#6220),#3182,.T.);
#59321=ADVANCED_FACE('',(#6221),#921,.F.);
#59322=ADVANCED_FACE('',(#6222,#1837),#699,.F.);
#59323=ADVANCED_FACE('',(#6223),#922,.F.);
#59324=ADVANCED_FACE('',(#6224,#1838),#3183,.T.);
#59325=ADVANCED_FACE('',(#6225),#923,.T.);
#59326=ADVANCED_FACE('',(#6226),#700,.T.);
#59327=ADVANCED_FACE('',(#6227,#1839),#3184,.T.);
#59328=ADVANCED_FACE('',(#6228),#924,.T.);
#59329=ADVANCED_FACE('',(#6229),#701,.T.);
#59330=ADVANCED_FACE('',(#6230,#1840),#3185,.T.);
#59331=ADVANCED_FACE('',(#6231),#925,.F.);
#59332=ADVANCED_FACE('',(#6232),#702,.F.);
#59333=ADVANCED_FACE('',(#6233),#926,.F.);
#59334=ADVANCED_FACE('',(#6234),#703,.F.);
#59335=ADVANCED_FACE('',(#6235,#1841),#3186,.T.);
#59336=ADVANCED_FACE('',(#6236),#927,.F.);
#59337=ADVANCED_FACE('',(#6237),#704,.F.);
#59338=ADVANCED_FACE('',(#6238,#1842),#3187,.T.);
#59339=ADVANCED_FACE('',(#6239,#1843),#3188,.T.);
#59340=ADVANCED_FACE('',(#6240,#1844),#3189,.T.);
#59341=ADVANCED_FACE('',(#6241),#705,.F.);
#59342=ADVANCED_FACE('',(#6242),#706,.F.);
#59343=ADVANCED_FACE('',(#6243),#3190,.T.);
#59344=ADVANCED_FACE('',(#6244),#3191,.T.);
#59345=ADVANCED_FACE('',(#6245,#1845,#1846),#3192,.T.);
#59346=ADVANCED_FACE('',(#6246),#3193,.T.);
#59347=ADVANCED_FACE('',(#6247),#3194,.T.);
#59348=ADVANCED_FACE('',(#6248),#3195,.T.);
#59349=ADVANCED_FACE('',(#6249),#3196,.T.);
#59350=ADVANCED_FACE('',(#6250),#3197,.T.);
#59351=ADVANCED_FACE('',(#6251),#3198,.T.);
#59352=ADVANCED_FACE('',(#6252),#3199,.T.);
#59353=ADVANCED_FACE('',(#6253),#3200,.T.);
#59354=ADVANCED_FACE('',(#6254),#3201,.T.);
#59355=ADVANCED_FACE('',(#6255),#3202,.T.);
#59356=ADVANCED_FACE('',(#6256),#3203,.T.);
#59357=ADVANCED_FACE('',(#6257),#3204,.T.);
#59358=ADVANCED_FACE('',(#6258),#3205,.T.);
#59359=ADVANCED_FACE('',(#6259),#3206,.T.);
#59360=ADVANCED_FACE('',(#6260),#3207,.T.);
#59361=ADVANCED_FACE('',(#6261),#3208,.T.);
#59362=ADVANCED_FACE('',(#6262),#3209,.T.);
#59363=ADVANCED_FACE('',(#6263),#3210,.T.);
#59364=ADVANCED_FACE('',(#6264),#3211,.T.);
#59365=ADVANCED_FACE('',(#6265),#3212,.T.);
#59366=ADVANCED_FACE('',(#6266),#3213,.T.);
#59367=ADVANCED_FACE('',(#6267),#3214,.T.);
#59368=ADVANCED_FACE('',(#6268),#3215,.T.);
#59369=ADVANCED_FACE('',(#6269),#3216,.T.);
#59370=ADVANCED_FACE('',(#6270),#3217,.T.);
#59371=ADVANCED_FACE('',(#6271),#3218,.T.);
#59372=ADVANCED_FACE('',(#6272),#3219,.T.);
#59373=ADVANCED_FACE('',(#6273),#3220,.T.);
#59374=ADVANCED_FACE('',(#6274),#3221,.T.);
#59375=ADVANCED_FACE('',(#6275),#3222,.T.);
#59376=ADVANCED_FACE('',(#6276),#3223,.T.);
#59377=ADVANCED_FACE('',(#6277),#3224,.T.);
#59378=ADVANCED_FACE('',(#6278),#3225,.T.);
#59379=ADVANCED_FACE('',(#6279),#3226,.T.);
#59380=ADVANCED_FACE('',(#6280),#3227,.T.);
#59381=ADVANCED_FACE('',(#6281),#3228,.T.);
#59382=ADVANCED_FACE('',(#6282),#3229,.T.);
#59383=ADVANCED_FACE('',(#6283),#3230,.T.);
#59384=ADVANCED_FACE('',(#6284),#3231,.T.);
#59385=ADVANCED_FACE('',(#6285),#3232,.T.);
#59386=ADVANCED_FACE('',(#6286),#3233,.T.);
#59387=ADVANCED_FACE('',(#6287),#3234,.T.);
#59388=ADVANCED_FACE('',(#6288),#3235,.T.);
#59389=ADVANCED_FACE('',(#6289),#3236,.T.);
#59390=ADVANCED_FACE('',(#6290),#3237,.T.);
#59391=ADVANCED_FACE('',(#6291),#3238,.T.);
#59392=ADVANCED_FACE('',(#6292),#3239,.T.);
#59393=ADVANCED_FACE('',(#6293),#3240,.T.);
#59394=ADVANCED_FACE('',(#6294),#3241,.T.);
#59395=ADVANCED_FACE('',(#6295),#3242,.T.);
#59396=ADVANCED_FACE('',(#6296),#3243,.T.);
#59397=ADVANCED_FACE('',(#6297),#3244,.T.);
#59398=ADVANCED_FACE('',(#6298),#3245,.T.);
#59399=ADVANCED_FACE('',(#6299),#3246,.T.);
#59400=ADVANCED_FACE('',(#6300),#3247,.T.);
#59401=ADVANCED_FACE('',(#6301),#3248,.T.);
#59402=ADVANCED_FACE('',(#6302),#3249,.T.);
#59403=ADVANCED_FACE('',(#6303),#3250,.T.);
#59404=ADVANCED_FACE('',(#6304),#3251,.T.);
#59405=ADVANCED_FACE('',(#6305),#3252,.T.);
#59406=ADVANCED_FACE('',(#6306),#3253,.T.);
#59407=ADVANCED_FACE('',(#6307),#3254,.T.);
#59408=ADVANCED_FACE('',(#6308),#3255,.T.);
#59409=ADVANCED_FACE('',(#6309),#3256,.T.);
#59410=ADVANCED_FACE('',(#6310),#3257,.T.);
#59411=ADVANCED_FACE('',(#6311),#3258,.T.);
#59412=ADVANCED_FACE('',(#6312),#3259,.T.);
#59413=ADVANCED_FACE('',(#6313),#3260,.T.);
#59414=ADVANCED_FACE('',(#6314),#3261,.T.);
#59415=ADVANCED_FACE('',(#6315),#3262,.T.);
#59416=ADVANCED_FACE('',(#6316),#3263,.T.);
#59417=ADVANCED_FACE('',(#6317),#3264,.T.);
#59418=ADVANCED_FACE('',(#6318),#3265,.T.);
#59419=ADVANCED_FACE('',(#6319),#3266,.T.);
#59420=ADVANCED_FACE('',(#6320),#3267,.T.);
#59421=ADVANCED_FACE('',(#6321),#3268,.T.);
#59422=ADVANCED_FACE('',(#6322),#3269,.T.);
#59423=ADVANCED_FACE('',(#6323),#3270,.T.);
#59424=ADVANCED_FACE('',(#6324),#3271,.T.);
#59425=ADVANCED_FACE('',(#6325),#3272,.T.);
#59426=ADVANCED_FACE('',(#6326),#3273,.T.);
#59427=ADVANCED_FACE('',(#6327),#3274,.T.);
#59428=ADVANCED_FACE('',(#6328),#3275,.T.);
#59429=ADVANCED_FACE('',(#6329),#3276,.T.);
#59430=ADVANCED_FACE('',(#6330),#3277,.T.);
#59431=ADVANCED_FACE('',(#6331),#3278,.T.);
#59432=ADVANCED_FACE('',(#6332),#3279,.T.);
#59433=ADVANCED_FACE('',(#6333),#3280,.T.);
#59434=ADVANCED_FACE('',(#6334),#3281,.T.);
#59435=ADVANCED_FACE('',(#6335),#3282,.T.);
#59436=ADVANCED_FACE('',(#6336),#3283,.T.);
#59437=ADVANCED_FACE('',(#6337),#3284,.T.);
#59438=ADVANCED_FACE('',(#6338),#3285,.T.);
#59439=ADVANCED_FACE('',(#6339),#3286,.T.);
#59440=ADVANCED_FACE('',(#6340),#3287,.T.);
#59441=ADVANCED_FACE('',(#6341),#3288,.T.);
#59442=ADVANCED_FACE('',(#6342),#3289,.T.);
#59443=ADVANCED_FACE('',(#6343),#3290,.T.);
#59444=ADVANCED_FACE('',(#6344),#3291,.T.);
#59445=ADVANCED_FACE('',(#6345),#3292,.T.);
#59446=ADVANCED_FACE('',(#6346),#3293,.T.);
#59447=ADVANCED_FACE('',(#6347),#3294,.T.);
#59448=ADVANCED_FACE('',(#6348),#3295,.T.);
#59449=ADVANCED_FACE('',(#6349),#3296,.T.);
#59450=ADVANCED_FACE('',(#6350),#3297,.T.);
#59451=ADVANCED_FACE('',(#6351),#3298,.T.);
#59452=ADVANCED_FACE('',(#6352),#3299,.T.);
#59453=ADVANCED_FACE('',(#6353),#3300,.T.);
#59454=ADVANCED_FACE('',(#6354),#3301,.T.);
#59455=ADVANCED_FACE('',(#6355),#3302,.T.);
#59456=ADVANCED_FACE('',(#6356),#3303,.T.);
#59457=ADVANCED_FACE('',(#6357),#3304,.T.);
#59458=ADVANCED_FACE('',(#6358),#3305,.T.);
#59459=ADVANCED_FACE('',(#6359),#3306,.T.);
#59460=ADVANCED_FACE('',(#6360),#3307,.T.);
#59461=ADVANCED_FACE('',(#6361),#3308,.T.);
#59462=ADVANCED_FACE('',(#6362),#3309,.T.);
#59463=ADVANCED_FACE('',(#6363),#3310,.T.);
#59464=ADVANCED_FACE('',(#6364),#3311,.T.);
#59465=ADVANCED_FACE('',(#6365),#3312,.T.);
#59466=ADVANCED_FACE('',(#6366),#3313,.T.);
#59467=ADVANCED_FACE('',(#6367),#3314,.T.);
#59468=ADVANCED_FACE('',(#6368),#3315,.T.);
#59469=ADVANCED_FACE('',(#6369),#3316,.T.);
#59470=ADVANCED_FACE('',(#6370),#3317,.T.);
#59471=ADVANCED_FACE('',(#6371),#3318,.T.);
#59472=ADVANCED_FACE('',(#6372),#3319,.T.);
#59473=ADVANCED_FACE('',(#6373),#3320,.T.);
#59474=ADVANCED_FACE('',(#6374),#3321,.T.);
#59475=ADVANCED_FACE('',(#6375),#3322,.T.);
#59476=ADVANCED_FACE('',(#6376),#3323,.T.);
#59477=ADVANCED_FACE('',(#6377),#3324,.T.);
#59478=ADVANCED_FACE('',(#6378),#3325,.T.);
#59479=ADVANCED_FACE('',(#6379),#3326,.T.);
#59480=ADVANCED_FACE('',(#6380),#3327,.T.);
#59481=ADVANCED_FACE('',(#6381),#3328,.T.);
#59482=ADVANCED_FACE('',(#6382),#3329,.T.);
#59483=ADVANCED_FACE('',(#6383),#3330,.T.);
#59484=ADVANCED_FACE('',(#6384),#3331,.T.);
#59485=ADVANCED_FACE('',(#6385),#3332,.T.);
#59486=ADVANCED_FACE('',(#6386),#3333,.T.);
#59487=ADVANCED_FACE('',(#6387),#3334,.T.);
#59488=ADVANCED_FACE('',(#6388),#3335,.T.);
#59489=ADVANCED_FACE('',(#6389),#3336,.T.);
#59490=ADVANCED_FACE('',(#6390),#3337,.T.);
#59491=ADVANCED_FACE('',(#6391),#3338,.T.);
#59492=ADVANCED_FACE('',(#6392),#3339,.T.);
#59493=ADVANCED_FACE('',(#6393),#3340,.T.);
#59494=ADVANCED_FACE('',(#6394),#3341,.T.);
#59495=ADVANCED_FACE('',(#6395),#3342,.T.);
#59496=ADVANCED_FACE('',(#6396),#3343,.T.);
#59497=ADVANCED_FACE('',(#6397),#3344,.T.);
#59498=ADVANCED_FACE('',(#6398),#3345,.T.);
#59499=ADVANCED_FACE('',(#6399),#3346,.T.);
#59500=ADVANCED_FACE('',(#6400),#3347,.T.);
#59501=ADVANCED_FACE('',(#6401),#3348,.T.);
#59502=ADVANCED_FACE('',(#6402),#3349,.T.);
#59503=ADVANCED_FACE('',(#6403),#3350,.T.);
#59504=ADVANCED_FACE('',(#6404),#3351,.T.);
#59505=ADVANCED_FACE('',(#6405),#3352,.T.);
#59506=ADVANCED_FACE('',(#6406),#3353,.T.);
#59507=ADVANCED_FACE('',(#6407),#3354,.T.);
#59508=ADVANCED_FACE('',(#6408),#3355,.T.);
#59509=ADVANCED_FACE('',(#6409),#3356,.T.);
#59510=ADVANCED_FACE('',(#6410),#3357,.T.);
#59511=ADVANCED_FACE('',(#6411),#3358,.T.);
#59512=ADVANCED_FACE('',(#6412),#3359,.T.);
#59513=ADVANCED_FACE('',(#6413),#3360,.T.);
#59514=ADVANCED_FACE('',(#6414),#3361,.T.);
#59515=ADVANCED_FACE('',(#6415),#3362,.T.);
#59516=ADVANCED_FACE('',(#6416),#3363,.T.);
#59517=ADVANCED_FACE('',(#6417),#3364,.T.);
#59518=ADVANCED_FACE('',(#6418),#3365,.T.);
#59519=ADVANCED_FACE('',(#6419),#3366,.T.);
#59520=ADVANCED_FACE('',(#6420),#3367,.T.);
#59521=ADVANCED_FACE('',(#6421),#3368,.T.);
#59522=ADVANCED_FACE('',(#6422),#3369,.T.);
#59523=ADVANCED_FACE('',(#6423),#3370,.T.);
#59524=ADVANCED_FACE('',(#6424),#3371,.T.);
#59525=ADVANCED_FACE('',(#6425),#3372,.T.);
#59526=ADVANCED_FACE('',(#6426),#3373,.T.);
#59527=ADVANCED_FACE('',(#6427),#3374,.T.);
#59528=ADVANCED_FACE('',(#6428),#3375,.T.);
#59529=ADVANCED_FACE('',(#6429),#3376,.T.);
#59530=ADVANCED_FACE('',(#6430),#3377,.T.);
#59531=ADVANCED_FACE('',(#6431),#3378,.T.);
#59532=ADVANCED_FACE('',(#6432),#3379,.T.);
#59533=ADVANCED_FACE('',(#6433),#3380,.T.);
#59534=ADVANCED_FACE('',(#6434),#3381,.T.);
#59535=ADVANCED_FACE('',(#6435),#3382,.T.);
#59536=ADVANCED_FACE('',(#6436),#3383,.T.);
#59537=ADVANCED_FACE('',(#6437),#3384,.T.);
#59538=ADVANCED_FACE('',(#6438),#3385,.T.);
#59539=ADVANCED_FACE('',(#6439),#3386,.T.);
#59540=ADVANCED_FACE('',(#6440),#3387,.T.);
#59541=ADVANCED_FACE('',(#6441),#3388,.T.);
#59542=ADVANCED_FACE('',(#6442),#3389,.T.);
#59543=ADVANCED_FACE('',(#6443),#3390,.T.);
#59544=ADVANCED_FACE('',(#6444),#3391,.T.);
#59545=ADVANCED_FACE('',(#6445),#3392,.T.);
#59546=ADVANCED_FACE('',(#6446),#3393,.T.);
#59547=ADVANCED_FACE('',(#6447),#3394,.T.);
#59548=ADVANCED_FACE('',(#6448),#3395,.T.);
#59549=ADVANCED_FACE('',(#6449),#3396,.T.);
#59550=ADVANCED_FACE('',(#6450),#3397,.T.);
#59551=ADVANCED_FACE('',(#6451),#3398,.T.);
#59552=ADVANCED_FACE('',(#6452),#3399,.T.);
#59553=ADVANCED_FACE('',(#6453),#3400,.T.);
#59554=ADVANCED_FACE('',(#6454),#3401,.T.);
#59555=ADVANCED_FACE('',(#6455),#3402,.T.);
#59556=ADVANCED_FACE('',(#6456),#3403,.T.);
#59557=ADVANCED_FACE('',(#6457),#3404,.T.);
#59558=ADVANCED_FACE('',(#6458),#3405,.T.);
#59559=ADVANCED_FACE('',(#6459),#3406,.T.);
#59560=ADVANCED_FACE('',(#6460),#3407,.T.);
#59561=ADVANCED_FACE('',(#6461),#3408,.T.);
#59562=ADVANCED_FACE('',(#6462),#3409,.T.);
#59563=ADVANCED_FACE('',(#6463),#3410,.T.);
#59564=ADVANCED_FACE('',(#6464),#3411,.T.);
#59565=ADVANCED_FACE('',(#6465),#3412,.T.);
#59566=ADVANCED_FACE('',(#6466),#3413,.T.);
#59567=ADVANCED_FACE('',(#6467),#3414,.T.);
#59568=ADVANCED_FACE('',(#6468),#3415,.T.);
#59569=ADVANCED_FACE('',(#6469),#3416,.T.);
#59570=ADVANCED_FACE('',(#6470),#3417,.T.);
#59571=ADVANCED_FACE('',(#6471),#3418,.T.);
#59572=ADVANCED_FACE('',(#6472),#3419,.T.);
#59573=ADVANCED_FACE('',(#6473),#3420,.T.);
#59574=ADVANCED_FACE('',(#6474),#3421,.T.);
#59575=ADVANCED_FACE('',(#6475),#3422,.T.);
#59576=ADVANCED_FACE('',(#6476),#3423,.T.);
#59577=ADVANCED_FACE('',(#6477),#3424,.T.);
#59578=ADVANCED_FACE('',(#6478),#3425,.T.);
#59579=ADVANCED_FACE('',(#6479),#3426,.T.);
#59580=ADVANCED_FACE('',(#6480),#3427,.T.);
#59581=ADVANCED_FACE('',(#6481),#3428,.T.);
#59582=ADVANCED_FACE('',(#6482),#3429,.T.);
#59583=ADVANCED_FACE('',(#6483),#3430,.T.);
#59584=ADVANCED_FACE('',(#6484),#3431,.T.);
#59585=ADVANCED_FACE('',(#6485),#3432,.T.);
#59586=ADVANCED_FACE('',(#6486),#3433,.T.);
#59587=ADVANCED_FACE('',(#6487),#3434,.T.);
#59588=ADVANCED_FACE('',(#6488),#3435,.T.);
#59589=ADVANCED_FACE('',(#6489),#3436,.T.);
#59590=ADVANCED_FACE('',(#6490),#3437,.T.);
#59591=ADVANCED_FACE('',(#6491),#3438,.T.);
#59592=ADVANCED_FACE('',(#6492),#3439,.T.);
#59593=ADVANCED_FACE('',(#6493),#3440,.T.);
#59594=ADVANCED_FACE('',(#6494),#3441,.T.);
#59595=ADVANCED_FACE('',(#6495),#3442,.T.);
#59596=ADVANCED_FACE('',(#6496),#3443,.T.);
#59597=ADVANCED_FACE('',(#6497),#3444,.T.);
#59598=ADVANCED_FACE('',(#6498),#3445,.T.);
#59599=ADVANCED_FACE('',(#6499),#3446,.T.);
#59600=ADVANCED_FACE('',(#6500),#3447,.T.);
#59601=ADVANCED_FACE('',(#6501),#3448,.T.);
#59602=ADVANCED_FACE('',(#6502),#3449,.T.);
#59603=ADVANCED_FACE('',(#6503),#3450,.T.);
#59604=ADVANCED_FACE('',(#6504),#3451,.T.);
#59605=ADVANCED_FACE('',(#6505),#3452,.T.);
#59606=ADVANCED_FACE('',(#6506),#3453,.T.);
#59607=ADVANCED_FACE('',(#6507),#3454,.T.);
#59608=ADVANCED_FACE('',(#6508),#3455,.T.);
#59609=ADVANCED_FACE('',(#6509),#3456,.T.);
#59610=ADVANCED_FACE('',(#6510),#3457,.T.);
#59611=ADVANCED_FACE('',(#6511),#3458,.T.);
#59612=ADVANCED_FACE('',(#6512),#3459,.T.);
#59613=ADVANCED_FACE('',(#6513),#3460,.T.);
#59614=ADVANCED_FACE('',(#6514),#3461,.T.);
#59615=ADVANCED_FACE('',(#6515),#3462,.T.);
#59616=ADVANCED_FACE('',(#6516),#3463,.T.);
#59617=ADVANCED_FACE('',(#6517),#3464,.T.);
#59618=ADVANCED_FACE('',(#6518),#3465,.T.);
#59619=ADVANCED_FACE('',(#6519),#3466,.T.);
#59620=ADVANCED_FACE('',(#6520),#3467,.T.);
#59621=ADVANCED_FACE('',(#6521),#3468,.T.);
#59622=ADVANCED_FACE('',(#6522),#3469,.T.);
#59623=ADVANCED_FACE('',(#6523),#3470,.T.);
#59624=ADVANCED_FACE('',(#6524),#3471,.T.);
#59625=ADVANCED_FACE('',(#6525),#3472,.T.);
#59626=ADVANCED_FACE('',(#6526),#3473,.T.);
#59627=ADVANCED_FACE('',(#6527),#3474,.T.);
#59628=ADVANCED_FACE('',(#6528),#3475,.T.);
#59629=ADVANCED_FACE('',(#6529),#3476,.T.);
#59630=ADVANCED_FACE('',(#6530),#3477,.T.);
#59631=ADVANCED_FACE('',(#6531),#3478,.T.);
#59632=ADVANCED_FACE('',(#6532),#3479,.T.);
#59633=ADVANCED_FACE('',(#6533),#3480,.T.);
#59634=ADVANCED_FACE('',(#6534),#3481,.T.);
#59635=ADVANCED_FACE('',(#6535),#3482,.T.);
#59636=ADVANCED_FACE('',(#6536),#3483,.T.);
#59637=ADVANCED_FACE('',(#6537),#3484,.T.);
#59638=ADVANCED_FACE('',(#6538),#3485,.T.);
#59639=ADVANCED_FACE('',(#6539),#3486,.T.);
#59640=ADVANCED_FACE('',(#6540),#3487,.T.);
#59641=ADVANCED_FACE('',(#6541),#3488,.T.);
#59642=ADVANCED_FACE('',(#6542),#3489,.T.);
#59643=ADVANCED_FACE('',(#6543),#3490,.T.);
#59644=ADVANCED_FACE('',(#6544),#3491,.T.);
#59645=ADVANCED_FACE('',(#6545),#3492,.T.);
#59646=ADVANCED_FACE('',(#6546),#3493,.T.);
#59647=ADVANCED_FACE('',(#6547),#3494,.T.);
#59648=ADVANCED_FACE('',(#6548),#3495,.T.);
#59649=ADVANCED_FACE('',(#6549),#3496,.T.);
#59650=ADVANCED_FACE('',(#6550),#3497,.T.);
#59651=ADVANCED_FACE('',(#6551),#3498,.T.);
#59652=ADVANCED_FACE('',(#6552),#3499,.T.);
#59653=ADVANCED_FACE('',(#6553),#3500,.T.);
#59654=ADVANCED_FACE('',(#6554),#3501,.T.);
#59655=ADVANCED_FACE('',(#6555),#3502,.T.);
#59656=ADVANCED_FACE('',(#6556),#3503,.T.);
#59657=ADVANCED_FACE('',(#6557),#3504,.T.);
#59658=ADVANCED_FACE('',(#6558),#3505,.T.);
#59659=ADVANCED_FACE('',(#6559),#3506,.T.);
#59660=ADVANCED_FACE('',(#6560),#3507,.T.);
#59661=ADVANCED_FACE('',(#6561),#3508,.T.);
#59662=ADVANCED_FACE('',(#6562),#3509,.T.);
#59663=ADVANCED_FACE('',(#6563),#3510,.T.);
#59664=ADVANCED_FACE('',(#6564),#3511,.T.);
#59665=ADVANCED_FACE('',(#6565),#3512,.T.);
#59666=ADVANCED_FACE('',(#6566),#3513,.T.);
#59667=ADVANCED_FACE('',(#6567),#3514,.T.);
#59668=ADVANCED_FACE('',(#6568),#3515,.T.);
#59669=ADVANCED_FACE('',(#6569),#3516,.T.);
#59670=ADVANCED_FACE('',(#6570),#3517,.T.);
#59671=ADVANCED_FACE('',(#6571),#3518,.T.);
#59672=ADVANCED_FACE('',(#6572),#3519,.T.);
#59673=ADVANCED_FACE('',(#6573),#3520,.T.);
#59674=ADVANCED_FACE('',(#6574),#3521,.T.);
#59675=ADVANCED_FACE('',(#6575),#3522,.T.);
#59676=ADVANCED_FACE('',(#6576),#3523,.T.);
#59677=ADVANCED_FACE('',(#6577),#3524,.T.);
#59678=ADVANCED_FACE('',(#6578),#3525,.T.);
#59679=ADVANCED_FACE('',(#6579),#3526,.T.);
#59680=ADVANCED_FACE('',(#6580),#3527,.T.);
#59681=ADVANCED_FACE('',(#6581),#3528,.T.);
#59682=ADVANCED_FACE('',(#6582),#3529,.T.);
#59683=ADVANCED_FACE('',(#6583),#3530,.T.);
#59684=ADVANCED_FACE('',(#6584),#3531,.T.);
#59685=ADVANCED_FACE('',(#6585),#3532,.T.);
#59686=ADVANCED_FACE('',(#6586),#3533,.T.);
#59687=ADVANCED_FACE('',(#6587),#3534,.T.);
#59688=ADVANCED_FACE('',(#6588),#3535,.T.);
#59689=ADVANCED_FACE('',(#6589),#3536,.T.);
#59690=ADVANCED_FACE('',(#6590),#3537,.T.);
#59691=ADVANCED_FACE('',(#6591),#3538,.T.);
#59692=ADVANCED_FACE('',(#6592),#3539,.T.);
#59693=ADVANCED_FACE('',(#6593),#3540,.T.);
#59694=ADVANCED_FACE('',(#6594),#3541,.T.);
#59695=ADVANCED_FACE('',(#6595),#3542,.T.);
#59696=ADVANCED_FACE('',(#6596),#3543,.T.);
#59697=ADVANCED_FACE('',(#6597),#3544,.T.);
#59698=ADVANCED_FACE('',(#6598),#3545,.T.);
#59699=ADVANCED_FACE('',(#6599),#3546,.T.);
#59700=ADVANCED_FACE('',(#6600),#3547,.T.);
#59701=ADVANCED_FACE('',(#6601),#3548,.T.);
#59702=ADVANCED_FACE('',(#6602),#3549,.T.);
#59703=ADVANCED_FACE('',(#6603),#3550,.T.);
#59704=ADVANCED_FACE('',(#6604),#3551,.T.);
#59705=ADVANCED_FACE('',(#6605),#3552,.T.);
#59706=ADVANCED_FACE('',(#6606),#3553,.T.);
#59707=ADVANCED_FACE('',(#6607),#3554,.T.);
#59708=ADVANCED_FACE('',(#6608),#3555,.T.);
#59709=ADVANCED_FACE('',(#6609),#3556,.T.);
#59710=ADVANCED_FACE('',(#6610),#3557,.T.);
#59711=ADVANCED_FACE('',(#6611),#3558,.T.);
#59712=ADVANCED_FACE('',(#6612),#3559,.T.);
#59713=ADVANCED_FACE('',(#6613),#3560,.T.);
#59714=ADVANCED_FACE('',(#6614),#3561,.T.);
#59715=ADVANCED_FACE('',(#6615),#3562,.T.);
#59716=ADVANCED_FACE('',(#6616),#3563,.T.);
#59717=ADVANCED_FACE('',(#6617),#3564,.T.);
#59718=ADVANCED_FACE('',(#6618),#3565,.T.);
#59719=ADVANCED_FACE('',(#6619),#3566,.T.);
#59720=ADVANCED_FACE('',(#6620),#3567,.T.);
#59721=ADVANCED_FACE('',(#6621),#3568,.T.);
#59722=ADVANCED_FACE('',(#6622),#3569,.T.);
#59723=ADVANCED_FACE('',(#6623),#3570,.T.);
#59724=ADVANCED_FACE('',(#6624),#3571,.T.);
#59725=ADVANCED_FACE('',(#6625),#3572,.T.);
#59726=ADVANCED_FACE('',(#6626),#3573,.T.);
#59727=ADVANCED_FACE('',(#6627),#3574,.T.);
#59728=ADVANCED_FACE('',(#6628),#3575,.T.);
#59729=ADVANCED_FACE('',(#6629),#3576,.T.);
#59730=ADVANCED_FACE('',(#6630),#3577,.T.);
#59731=ADVANCED_FACE('',(#6631),#3578,.T.);
#59732=ADVANCED_FACE('',(#6632),#3579,.T.);
#59733=ADVANCED_FACE('',(#6633),#3580,.T.);
#59734=ADVANCED_FACE('',(#6634),#3581,.T.);
#59735=ADVANCED_FACE('',(#6635),#3582,.T.);
#59736=ADVANCED_FACE('',(#6636),#3583,.T.);
#59737=ADVANCED_FACE('',(#6637),#3584,.T.);
#59738=ADVANCED_FACE('',(#6638),#3585,.T.);
#59739=ADVANCED_FACE('',(#6639),#3586,.T.);
#59740=ADVANCED_FACE('',(#6640),#3587,.T.);
#59741=ADVANCED_FACE('',(#6641),#3588,.T.);
#59742=ADVANCED_FACE('',(#6642),#3589,.T.);
#59743=ADVANCED_FACE('',(#6643),#3590,.T.);
#59744=ADVANCED_FACE('',(#6644),#3591,.T.);
#59745=ADVANCED_FACE('',(#6645),#3592,.T.);
#59746=ADVANCED_FACE('',(#6646),#3593,.T.);
#59747=ADVANCED_FACE('',(#6647),#3594,.T.);
#59748=ADVANCED_FACE('',(#6648),#3595,.T.);
#59749=ADVANCED_FACE('',(#6649),#3596,.T.);
#59750=ADVANCED_FACE('',(#6650),#3597,.T.);
#59751=ADVANCED_FACE('',(#6651),#3598,.T.);
#59752=ADVANCED_FACE('',(#6652),#3599,.T.);
#59753=ADVANCED_FACE('',(#6653),#3600,.T.);
#59754=ADVANCED_FACE('',(#6654),#3601,.T.);
#59755=ADVANCED_FACE('',(#6655),#3602,.T.);
#59756=ADVANCED_FACE('',(#6656),#3603,.T.);
#59757=ADVANCED_FACE('',(#6657),#3604,.T.);
#59758=ADVANCED_FACE('',(#6658),#3605,.T.);
#59759=ADVANCED_FACE('',(#6659),#3606,.T.);
#59760=ADVANCED_FACE('',(#6660),#3607,.T.);
#59761=ADVANCED_FACE('',(#6661),#3608,.T.);
#59762=ADVANCED_FACE('',(#6662),#3609,.T.);
#59763=ADVANCED_FACE('',(#6663),#3610,.T.);
#59764=ADVANCED_FACE('',(#6664),#3611,.T.);
#59765=ADVANCED_FACE('',(#6665),#3612,.T.);
#59766=ADVANCED_FACE('',(#6666),#3613,.T.);
#59767=ADVANCED_FACE('',(#6667),#3614,.T.);
#59768=ADVANCED_FACE('',(#6668),#3615,.T.);
#59769=ADVANCED_FACE('',(#6669),#3616,.T.);
#59770=ADVANCED_FACE('',(#6670),#3617,.T.);
#59771=ADVANCED_FACE('',(#6671),#3618,.T.);
#59772=ADVANCED_FACE('',(#6672),#3619,.T.);
#59773=ADVANCED_FACE('',(#6673),#3620,.T.);
#59774=ADVANCED_FACE('',(#6674),#3621,.T.);
#59775=ADVANCED_FACE('',(#6675),#3622,.T.);
#59776=ADVANCED_FACE('',(#6676),#3623,.T.);
#59777=ADVANCED_FACE('',(#6677),#3624,.T.);
#59778=ADVANCED_FACE('',(#6678),#3625,.T.);
#59779=ADVANCED_FACE('',(#6679),#3626,.T.);
#59780=ADVANCED_FACE('',(#6680),#3627,.T.);
#59781=ADVANCED_FACE('',(#6681),#3628,.T.);
#59782=ADVANCED_FACE('',(#6682),#3629,.T.);
#59783=ADVANCED_FACE('',(#6683),#3630,.T.);
#59784=ADVANCED_FACE('',(#6684),#3631,.T.);
#59785=ADVANCED_FACE('',(#6685),#3632,.T.);
#59786=ADVANCED_FACE('',(#6686),#3633,.T.);
#59787=ADVANCED_FACE('',(#6687),#3634,.T.);
#59788=ADVANCED_FACE('',(#6688),#3635,.T.);
#59789=ADVANCED_FACE('',(#6689),#3636,.T.);
#59790=ADVANCED_FACE('',(#6690),#3637,.T.);
#59791=ADVANCED_FACE('',(#6691),#3638,.T.);
#59792=ADVANCED_FACE('',(#6692),#3639,.T.);
#59793=ADVANCED_FACE('',(#6693),#3640,.T.);
#59794=ADVANCED_FACE('',(#6694),#3641,.T.);
#59795=ADVANCED_FACE('',(#6695),#3642,.T.);
#59796=ADVANCED_FACE('',(#6696),#3643,.T.);
#59797=ADVANCED_FACE('',(#6697),#3644,.T.);
#59798=ADVANCED_FACE('',(#6698),#3645,.T.);
#59799=ADVANCED_FACE('',(#6699),#3646,.T.);
#59800=ADVANCED_FACE('',(#6700),#3647,.T.);
#59801=ADVANCED_FACE('',(#6701),#3648,.T.);
#59802=ADVANCED_FACE('',(#6702),#3649,.T.);
#59803=ADVANCED_FACE('',(#6703),#3650,.T.);
#59804=ADVANCED_FACE('',(#6704),#3651,.T.);
#59805=ADVANCED_FACE('',(#6705),#3652,.T.);
#59806=ADVANCED_FACE('',(#6706),#3653,.T.);
#59807=ADVANCED_FACE('',(#6707),#3654,.T.);
#59808=ADVANCED_FACE('',(#6708),#3655,.T.);
#59809=ADVANCED_FACE('',(#6709),#3656,.T.);
#59810=ADVANCED_FACE('',(#6710),#3657,.T.);
#59811=ADVANCED_FACE('',(#6711),#3658,.T.);
#59812=ADVANCED_FACE('',(#6712),#3659,.T.);
#59813=ADVANCED_FACE('',(#6713),#3660,.T.);
#59814=ADVANCED_FACE('',(#6714),#3661,.T.);
#59815=ADVANCED_FACE('',(#6715),#3662,.T.);
#59816=ADVANCED_FACE('',(#6716),#3663,.T.);
#59817=ADVANCED_FACE('',(#6717),#3664,.T.);
#59818=ADVANCED_FACE('',(#6718),#3665,.T.);
#59819=ADVANCED_FACE('',(#6719),#3666,.T.);
#59820=ADVANCED_FACE('',(#6720),#3667,.T.);
#59821=ADVANCED_FACE('',(#6721),#3668,.T.);
#59822=ADVANCED_FACE('',(#6722),#3669,.T.);
#59823=ADVANCED_FACE('',(#6723),#3670,.T.);
#59824=ADVANCED_FACE('',(#6724),#3671,.T.);
#59825=ADVANCED_FACE('',(#6725),#3672,.T.);
#59826=ADVANCED_FACE('',(#6726),#3673,.T.);
#59827=ADVANCED_FACE('',(#6727),#3674,.T.);
#59828=ADVANCED_FACE('',(#6728),#3675,.T.);
#59829=ADVANCED_FACE('',(#6729),#3676,.T.);
#59830=ADVANCED_FACE('',(#6730),#3677,.T.);
#59831=ADVANCED_FACE('',(#6731),#3678,.T.);
#59832=ADVANCED_FACE('',(#6732),#3679,.T.);
#59833=ADVANCED_FACE('',(#6733),#3680,.T.);
#59834=ADVANCED_FACE('',(#6734),#3681,.T.);
#59835=ADVANCED_FACE('',(#6735),#3682,.T.);
#59836=ADVANCED_FACE('',(#6736),#3683,.T.);
#59837=ADVANCED_FACE('',(#6737),#3684,.T.);
#59838=ADVANCED_FACE('',(#6738),#3685,.T.);
#59839=ADVANCED_FACE('',(#6739),#3686,.T.);
#59840=ADVANCED_FACE('',(#6740),#3687,.T.);
#59841=ADVANCED_FACE('',(#6741),#3688,.T.);
#59842=ADVANCED_FACE('',(#6742),#3689,.T.);
#59843=ADVANCED_FACE('',(#6743),#3690,.T.);
#59844=ADVANCED_FACE('',(#6744),#3691,.T.);
#59845=ADVANCED_FACE('',(#6745),#3692,.T.);
#59846=ADVANCED_FACE('',(#6746),#3693,.T.);
#59847=ADVANCED_FACE('',(#6747),#3694,.T.);
#59848=ADVANCED_FACE('',(#6748),#3695,.F.);
#59849=ADVANCED_FACE('',(#6749),#707,.F.);
#59850=ADVANCED_FACE('',(#6750),#708,.T.);
#59851=ADVANCED_FACE('',(#6751),#709,.F.);
#59852=ADVANCED_FACE('',(#6752),#3696,.T.);
#59853=ADVANCED_FACE('',(#6753),#710,.T.);
#59854=ADVANCED_FACE('',(#6754),#3697,.T.);
#59855=ADVANCED_FACE('',(#6755),#3698,.T.);
#59856=ADVANCED_FACE('',(#6756),#711,.T.);
#59857=ADVANCED_FACE('',(#6757,#1847),#3699,.F.);
#59858=ADVANCED_FACE('',(#6758),#712,.F.);
#59859=ADVANCED_FACE('',(#6759),#3700,.T.);
#59860=ADVANCED_FACE('',(#6760),#3701,.T.);
#59861=ADVANCED_FACE('',(#6761),#3702,.T.);
#59862=ADVANCED_FACE('',(#6762),#3703,.T.);
#59863=ADVANCED_FACE('',(#6763),#3704,.T.);
#59864=ADVANCED_FACE('',(#6764),#3705,.T.);
#59865=ADVANCED_FACE('',(#6765),#713,.F.);
#59866=ADVANCED_FACE('',(#6766),#3706,.T.);
#59867=ADVANCED_FACE('',(#6767,#1848),#3707,.T.);
#59868=ADVANCED_FACE('',(#6768),#3708,.F.);
#59869=ADVANCED_FACE('',(#6769),#3709,.F.);
#59870=ADVANCED_FACE('',(#6770),#3710,.F.);
#59871=ADVANCED_FACE('',(#6771),#3711,.F.);
#59872=ADVANCED_FACE('',(#6772),#3712,.F.);
#59873=ADVANCED_FACE('',(#6773),#3713,.F.);
#59874=ADVANCED_FACE('',(#6774),#3714,.F.);
#59875=ADVANCED_FACE('',(#6775),#3715,.F.);
#59876=ADVANCED_FACE('',(#6776),#3716,.F.);
#59877=ADVANCED_FACE('',(#6777),#3717,.F.);
#59878=ADVANCED_FACE('',(#6778),#3718,.F.);
#59879=ADVANCED_FACE('',(#6779),#3719,.F.);
#59880=ADVANCED_FACE('',(#6780),#3720,.F.);
#59881=ADVANCED_FACE('',(#6781),#3721,.F.);
#59882=ADVANCED_FACE('',(#6782),#3722,.F.);
#59883=ADVANCED_FACE('',(#6783),#3723,.F.);
#59884=ADVANCED_FACE('',(#6784),#3724,.F.);
#59885=ADVANCED_FACE('',(#6785),#3725,.F.);
#59886=ADVANCED_FACE('',(#6786),#3726,.F.);
#59887=ADVANCED_FACE('',(#6787),#3727,.F.);
#59888=ADVANCED_FACE('',(#6788),#3728,.F.);
#59889=ADVANCED_FACE('',(#6789),#3729,.F.);
#59890=ADVANCED_FACE('',(#6790),#3730,.F.);
#59891=ADVANCED_FACE('',(#6791),#3731,.F.);
#59892=ADVANCED_FACE('',(#6792),#3732,.F.);
#59893=ADVANCED_FACE('',(#6793),#3733,.F.);
#59894=ADVANCED_FACE('',(#6794),#3734,.F.);
#59895=ADVANCED_FACE('',(#6795),#3735,.F.);
#59896=ADVANCED_FACE('',(#6796),#3736,.F.);
#59897=ADVANCED_FACE('',(#6797),#3737,.F.);
#59898=ADVANCED_FACE('',(#6798),#3738,.F.);
#59899=ADVANCED_FACE('',(#6799),#3739,.F.);
#59900=ADVANCED_FACE('',(#6800),#3740,.F.);
#59901=ADVANCED_FACE('',(#6801),#3741,.F.);
#59902=ADVANCED_FACE('',(#6802),#3742,.F.);
#59903=ADVANCED_FACE('',(#6803),#3743,.F.);
#59904=ADVANCED_FACE('',(#6804),#3744,.F.);
#59905=ADVANCED_FACE('',(#6805),#3745,.F.);
#59906=ADVANCED_FACE('',(#6806),#3746,.F.);
#59907=ADVANCED_FACE('',(#6807),#3747,.F.);
#59908=ADVANCED_FACE('',(#6808),#3748,.F.);
#59909=ADVANCED_FACE('',(#6809),#3749,.F.);
#59910=ADVANCED_FACE('',(#6810),#3750,.F.);
#59911=ADVANCED_FACE('',(#6811),#3751,.F.);
#59912=ADVANCED_FACE('',(#6812),#3752,.F.);
#59913=ADVANCED_FACE('',(#6813),#3753,.F.);
#59914=ADVANCED_FACE('',(#6814),#3754,.F.);
#59915=ADVANCED_FACE('',(#6815),#3755,.F.);
#59916=ADVANCED_FACE('',(#6816),#3756,.F.);
#59917=ADVANCED_FACE('',(#6817),#3757,.F.);
#59918=ADVANCED_FACE('',(#6818),#3758,.F.);
#59919=ADVANCED_FACE('',(#6819),#3759,.F.);
#59920=ADVANCED_FACE('',(#6820),#3760,.F.);
#59921=ADVANCED_FACE('',(#6821),#3761,.F.);
#59922=ADVANCED_FACE('',(#6822),#3762,.F.);
#59923=ADVANCED_FACE('',(#6823),#3763,.F.);
#59924=ADVANCED_FACE('',(#6824),#3764,.F.);
#59925=ADVANCED_FACE('',(#6825),#3765,.F.);
#59926=ADVANCED_FACE('',(#6826),#3766,.F.);
#59927=ADVANCED_FACE('',(#6827),#3767,.F.);
#59928=ADVANCED_FACE('',(#6828),#3768,.F.);
#59929=ADVANCED_FACE('',(#6829),#3769,.F.);
#59930=ADVANCED_FACE('',(#6830),#3770,.F.);
#59931=ADVANCED_FACE('',(#6831),#3771,.F.);
#59932=ADVANCED_FACE('',(#6832),#3772,.F.);
#59933=ADVANCED_FACE('',(#6833),#3773,.F.);
#59934=ADVANCED_FACE('',(#6834),#3774,.T.);
#59935=ADVANCED_FACE('',(#6835),#3775,.T.);
#59936=ADVANCED_FACE('',(#6836),#3776,.T.);
#59937=ADVANCED_FACE('',(#6837),#714,.F.);
#59938=ADVANCED_FACE('',(#6838),#928,.F.);
#59939=ADVANCED_FACE('',(#6839),#3777,.T.);
#59940=ADVANCED_FACE('',(#6840),#3778,.T.);
#59941=ADVANCED_FACE('',(#6841),#715,.F.);
#59942=ADVANCED_FACE('',(#6842),#929,.F.);
#59943=ADVANCED_FACE('',(#6843),#3779,.T.);
#59944=ADVANCED_FACE('',(#6844),#716,.T.);
#59945=ADVANCED_FACE('',(#6845),#3780,.T.);
#59946=ADVANCED_FACE('',(#6846),#717,.T.);
#59947=ADVANCED_FACE('',(#6847),#3781,.T.);
#59948=ADVANCED_FACE('',(#6848),#3782,.T.);
#59949=ADVANCED_FACE('',(#6849,#1849,#1850),#3783,.F.);
#59950=ADVANCED_FACE('',(#6850),#718,.T.);
#59951=ADVANCED_FACE('',(#6851),#719,.T.);
#59952=ADVANCED_FACE('',(#6852),#720,.T.);
#59953=ADVANCED_FACE('',(#6853),#721,.T.);
#59954=ADVANCED_FACE('',(#6854),#722,.T.);
#59955=ADVANCED_FACE('',(#6855),#723,.T.);
#59956=ADVANCED_FACE('',(#6856),#724,.T.);
#59957=ADVANCED_FACE('',(#6857),#725,.T.);
#59958=ADVANCED_FACE('',(#6858),#726,.T.);
#59959=ADVANCED_FACE('',(#6859),#727,.T.);
#59960=ADVANCED_FACE('',(#6860),#728,.T.);
#59961=ADVANCED_FACE('',(#6861),#729,.T.);
#59962=ADVANCED_FACE('',(#6862),#730,.T.);
#59963=ADVANCED_FACE('',(#6863),#731,.T.);
#59964=ADVANCED_FACE('',(#6864),#732,.T.);
#59965=ADVANCED_FACE('',(#6865),#733,.T.);
#59966=ADVANCED_FACE('',(#6866),#734,.T.);
#59967=ADVANCED_FACE('',(#6867),#735,.T.);
#59968=ADVANCED_FACE('',(#6868),#736,.T.);
#59969=ADVANCED_FACE('',(#6869),#737,.T.);
#59970=ADVANCED_FACE('',(#6870),#738,.T.);
#59971=ADVANCED_FACE('',(#6871),#3784,.F.);
#59972=ADVANCED_FACE('',(#6872),#57111,.F.);
#59973=ADVANCED_FACE('',(#6873),#3785,.T.);
#59974=ADVANCED_FACE('',(#6874),#739,.T.);
#59975=ADVANCED_FACE('',(#6875),#57112,.F.);
#59976=ADVANCED_FACE('',(#6876),#107,.F.);
#59977=ADVANCED_FACE('',(#6877,#1851),#3786,.T.);
#59978=ADVANCED_FACE('',(#6878),#740,.T.);
#59979=ADVANCED_FACE('',(#6879),#3787,.F.);
#59980=ADVANCED_FACE('',(#6880),#3788,.F.);
#59981=ADVANCED_FACE('',(#6881),#3789,.F.);
#59982=ADVANCED_FACE('',(#6882),#930,.T.);
#59983=ADVANCED_FACE('',(#6883),#931,.T.);
#59984=ADVANCED_FACE('',(#6884),#3790,.T.);
#59985=ADVANCED_FACE('',(#6885),#3791,.T.);
#59986=ADVANCED_FACE('',(#6886),#741,.T.);
#59987=ADVANCED_FACE('',(#6887),#932,.T.);
#59988=ADVANCED_FACE('',(#6888),#3792,.T.);
#59989=ADVANCED_FACE('',(#6889),#742,.T.);
#59990=ADVANCED_FACE('',(#6890),#743,.T.);
#59991=ADVANCED_FACE('',(#6891),#744,.T.);
#59992=ADVANCED_FACE('',(#6892),#745,.T.);
#59993=ADVANCED_FACE('',(#6893),#746,.T.);
#59994=ADVANCED_FACE('',(#6894),#747,.T.);
#59995=ADVANCED_FACE('',(#6895),#748,.T.);
#59996=ADVANCED_FACE('',(#6896),#749,.T.);
#59997=ADVANCED_FACE('',(#6897),#750,.T.);
#59998=ADVANCED_FACE('',(#6898),#3793,.T.);
#59999=ADVANCED_FACE('',(#6899),#57113,.F.);
#60000=ADVANCED_FACE('',(#6900),#3794,.F.);
#60001=ADVANCED_FACE('',(#6901),#751,.T.);
#60002=ADVANCED_FACE('',(#6902),#57114,.F.);
#60003=ADVANCED_FACE('',(#6903),#933,.F.);
#60004=ADVANCED_FACE('',(#6904),#752,.T.);
#60005=ADVANCED_FACE('',(#6905),#753,.T.);
#60006=ADVANCED_FACE('',(#6906),#754,.T.);
#60007=ADVANCED_FACE('',(#6907),#755,.T.);
#60008=ADVANCED_FACE('',(#6908),#756,.T.);
#60009=ADVANCED_FACE('',(#6909),#757,.T.);
#60010=ADVANCED_FACE('',(#6910),#3795,.F.);
#60011=ADVANCED_FACE('',(#6911),#3796,.F.);
#60012=ADVANCED_FACE('',(#6912),#3797,.F.);
#60013=ADVANCED_FACE('',(#6913),#3798,.T.);
#60014=ADVANCED_FACE('',(#6914),#3799,.T.);
#60015=ADVANCED_FACE('',(#6915),#3800,.T.);
#60016=ADVANCED_FACE('',(#6916),#3801,.T.);
#60017=ADVANCED_FACE('',(#6917),#3802,.T.);
#60018=ADVANCED_FACE('',(#6918),#3803,.T.);
#60019=ADVANCED_FACE('',(#6919),#3804,.F.);
#60020=ADVANCED_FACE('',(#6920),#3805,.F.);
#60021=ADVANCED_FACE('',(#6921),#3806,.F.);
#60022=ADVANCED_FACE('',(#6922),#3807,.F.);
#60023=ADVANCED_FACE('',(#6923),#3808,.F.);
#60024=ADVANCED_FACE('',(#6924),#3809,.F.);
#60025=ADVANCED_FACE('',(#6925),#934,.F.);
#60026=ADVANCED_FACE('',(#6926),#3810,.F.);
#60027=ADVANCED_FACE('',(#6927),#3811,.F.);
#60028=ADVANCED_FACE('',(#6928),#3812,.F.);
#60029=ADVANCED_FACE('',(#6929,#1852),#3813,.T.);
#60030=ADVANCED_FACE('',(#6930),#935,.T.);
#60031=ADVANCED_FACE('',(#6931),#758,.T.);
#60032=ADVANCED_FACE('',(#6932),#936,.T.);
#60033=ADVANCED_FACE('',(#6933),#3814,.T.);
#60034=ADVANCED_FACE('',(#6934),#759,.T.);
#60035=ADVANCED_FACE('',(#6935),#760,.T.);
#60036=ADVANCED_FACE('',(#6936),#761,.T.);
#60037=ADVANCED_FACE('',(#6937),#762,.T.);
#60038=ADVANCED_FACE('',(#6938),#763,.T.);
#60039=ADVANCED_FACE('',(#6939),#764,.T.);
#60040=ADVANCED_FACE('',(#6940),#765,.T.);
#60041=ADVANCED_FACE('',(#6941),#3815,.T.);
#60042=ADVANCED_FACE('',(#6942),#57115,.F.);
#60043=ADVANCED_FACE('',(#6943),#3816,.F.);
#60044=ADVANCED_FACE('',(#6944),#766,.T.);
#60045=ADVANCED_FACE('',(#6945),#57116,.F.);
#60046=ADVANCED_FACE('',(#6946),#937,.F.);
#60047=ADVANCED_FACE('',(#6947),#767,.T.);
#60048=ADVANCED_FACE('',(#6948),#768,.T.);
#60049=ADVANCED_FACE('',(#6949),#769,.T.);
#60050=ADVANCED_FACE('',(#6950),#770,.T.);
#60051=ADVANCED_FACE('',(#6951),#771,.T.);
#60052=ADVANCED_FACE('',(#6952),#772,.T.);
#60053=ADVANCED_FACE('',(#6953),#3817,.F.);
#60054=ADVANCED_FACE('',(#6954),#3818,.F.);
#60055=ADVANCED_FACE('',(#6955),#3819,.F.);
#60056=ADVANCED_FACE('',(#6956),#3820,.T.);
#60057=ADVANCED_FACE('',(#6957),#3821,.T.);
#60058=ADVANCED_FACE('',(#6958),#3822,.T.);
#60059=ADVANCED_FACE('',(#6959),#3823,.T.);
#60060=ADVANCED_FACE('',(#6960),#3824,.T.);
#60061=ADVANCED_FACE('',(#6961),#3825,.T.);
#60062=ADVANCED_FACE('',(#6962),#3826,.F.);
#60063=ADVANCED_FACE('',(#6963),#3827,.F.);
#60064=ADVANCED_FACE('',(#6964),#3828,.F.);
#60065=ADVANCED_FACE('',(#6965),#3829,.F.);
#60066=ADVANCED_FACE('',(#6966),#3830,.F.);
#60067=ADVANCED_FACE('',(#6967),#3831,.F.);
#60068=ADVANCED_FACE('',(#6968),#938,.F.);
#60069=ADVANCED_FACE('',(#6969),#3832,.F.);
#60070=ADVANCED_FACE('',(#6970),#3833,.F.);
#60071=ADVANCED_FACE('',(#6971),#3834,.F.);
#60072=ADVANCED_FACE('',(#6972,#1853),#3835,.T.);
#60073=ADVANCED_FACE('',(#6973),#939,.T.);
#60074=ADVANCED_FACE('',(#6974),#773,.T.);
#60075=ADVANCED_FACE('',(#6975),#940,.T.);
#60076=ADVANCED_FACE('',(#6976),#3836,.T.);
#60077=ADVANCED_FACE('',(#6977),#774,.T.);
#60078=ADVANCED_FACE('',(#6978),#775,.T.);
#60079=ADVANCED_FACE('',(#6979),#776,.T.);
#60080=ADVANCED_FACE('',(#6980),#777,.T.);
#60081=ADVANCED_FACE('',(#6981),#778,.T.);
#60082=ADVANCED_FACE('',(#6982),#779,.T.);
#60083=ADVANCED_FACE('',(#6983),#780,.T.);
#60084=ADVANCED_FACE('',(#6984),#781,.T.);
#60085=ADVANCED_FACE('',(#6985),#782,.T.);
#60086=ADVANCED_FACE('',(#6986),#783,.T.);
#60087=ADVANCED_FACE('',(#6987),#784,.T.);
#60088=ADVANCED_FACE('',(#6988),#785,.T.);
#60089=ADVANCED_FACE('',(#6989),#786,.T.);
#60090=ADVANCED_FACE('',(#6990),#787,.T.);
#60091=ADVANCED_FACE('',(#6991),#788,.T.);
#60092=ADVANCED_FACE('',(#6992),#789,.T.);
#60093=ADVANCED_FACE('',(#6993),#790,.T.);
#60094=ADVANCED_FACE('',(#6994),#791,.T.);
#60095=ADVANCED_FACE('',(#6995),#792,.T.);
#60096=ADVANCED_FACE('',(#6996),#793,.T.);
#60097=ADVANCED_FACE('',(#6997),#794,.T.);
#60098=ADVANCED_FACE('',(#6998),#3837,.F.);
#60099=ADVANCED_FACE('',(#6999),#57117,.F.);
#60100=ADVANCED_FACE('',(#7000),#3838,.T.);
#60101=ADVANCED_FACE('',(#7001),#795,.T.);
#60102=ADVANCED_FACE('',(#7002),#57118,.F.);
#60103=ADVANCED_FACE('',(#7003),#941,.F.);
#60104=ADVANCED_FACE('',(#7004),#796,.T.);
#60105=ADVANCED_FACE('',(#7005),#797,.T.);
#60106=ADVANCED_FACE('',(#7006),#798,.T.);
#60107=ADVANCED_FACE('',(#7007),#799,.T.);
#60108=ADVANCED_FACE('',(#7008),#800,.T.);
#60109=ADVANCED_FACE('',(#7009),#801,.T.);
#60110=ADVANCED_FACE('',(#7010),#3839,.F.);
#60111=ADVANCED_FACE('',(#7011),#3840,.F.);
#60112=ADVANCED_FACE('',(#7012),#3841,.F.);
#60113=ADVANCED_FACE('',(#7013),#3842,.T.);
#60114=ADVANCED_FACE('',(#7014),#3843,.T.);
#60115=ADVANCED_FACE('',(#7015),#3844,.T.);
#60116=ADVANCED_FACE('',(#7016),#3845,.T.);
#60117=ADVANCED_FACE('',(#7017),#3846,.T.);
#60118=ADVANCED_FACE('',(#7018),#3847,.T.);
#60119=ADVANCED_FACE('',(#7019),#3848,.F.);
#60120=ADVANCED_FACE('',(#7020),#3849,.F.);
#60121=ADVANCED_FACE('',(#7021),#3850,.F.);
#60122=ADVANCED_FACE('',(#7022),#3851,.F.);
#60123=ADVANCED_FACE('',(#7023),#3852,.F.);
#60124=ADVANCED_FACE('',(#7024),#3853,.F.);
#60125=ADVANCED_FACE('',(#7025),#942,.F.);
#60126=ADVANCED_FACE('',(#7026),#3854,.F.);
#60127=ADVANCED_FACE('',(#7027),#3855,.F.);
#60128=ADVANCED_FACE('',(#7028),#3856,.F.);
#60129=ADVANCED_FACE('',(#7029,#1854),#3857,.T.);
#60130=ADVANCED_FACE('',(#7030),#943,.T.);
#60131=ADVANCED_FACE('',(#7031),#802,.T.);
#60132=ADVANCED_FACE('',(#7032),#944,.T.);
#60133=ADVANCED_FACE('',(#7033),#3858,.T.);
#60134=ADVANCED_FACE('',(#7034),#803,.T.);
#60135=ADVANCED_FACE('',(#7035),#804,.T.);
#60136=ADVANCED_FACE('',(#7036),#805,.T.);
#60137=ADVANCED_FACE('',(#7037),#806,.T.);
#60138=ADVANCED_FACE('',(#7038),#807,.T.);
#60139=ADVANCED_FACE('',(#7039),#808,.T.);
#60140=ADVANCED_FACE('',(#7040),#809,.T.);
#60141=ADVANCED_FACE('',(#7041),#810,.T.);
#60142=ADVANCED_FACE('',(#7042),#811,.T.);
#60143=ADVANCED_FACE('',(#7043),#812,.T.);
#60144=ADVANCED_FACE('',(#7044),#813,.T.);
#60145=ADVANCED_FACE('',(#7045),#814,.T.);
#60146=ADVANCED_FACE('',(#7046),#3859,.T.);
#60147=ADVANCED_FACE('',(#7047),#57119,.F.);
#60148=ADVANCED_FACE('',(#7048),#3860,.F.);
#60149=ADVANCED_FACE('',(#7049),#815,.T.);
#60150=ADVANCED_FACE('',(#7050),#57120,.F.);
#60151=ADVANCED_FACE('',(#7051),#945,.F.);
#60152=ADVANCED_FACE('',(#7052),#816,.T.);
#60153=ADVANCED_FACE('',(#7053),#817,.T.);
#60154=ADVANCED_FACE('',(#7054),#818,.T.);
#60155=ADVANCED_FACE('',(#7055),#819,.T.);
#60156=ADVANCED_FACE('',(#7056),#820,.T.);
#60157=ADVANCED_FACE('',(#7057),#821,.T.);
#60158=ADVANCED_FACE('',(#7058),#3861,.F.);
#60159=ADVANCED_FACE('',(#7059),#3862,.F.);
#60160=ADVANCED_FACE('',(#7060),#3863,.F.);
#60161=ADVANCED_FACE('',(#7061),#3864,.T.);
#60162=ADVANCED_FACE('',(#7062),#3865,.T.);
#60163=ADVANCED_FACE('',(#7063),#3866,.T.);
#60164=ADVANCED_FACE('',(#7064),#3867,.T.);
#60165=ADVANCED_FACE('',(#7065),#3868,.T.);
#60166=ADVANCED_FACE('',(#7066),#3869,.T.);
#60167=ADVANCED_FACE('',(#7067),#3870,.F.);
#60168=ADVANCED_FACE('',(#7068),#3871,.F.);
#60169=ADVANCED_FACE('',(#7069),#3872,.F.);
#60170=ADVANCED_FACE('',(#7070),#3873,.F.);
#60171=ADVANCED_FACE('',(#7071),#3874,.F.);
#60172=ADVANCED_FACE('',(#7072),#3875,.F.);
#60173=ADVANCED_FACE('',(#7073),#946,.F.);
#60174=ADVANCED_FACE('',(#7074),#3876,.F.);
#60175=ADVANCED_FACE('',(#7075),#3877,.F.);
#60176=ADVANCED_FACE('',(#7076),#3878,.F.);
#60177=ADVANCED_FACE('',(#7077,#1855),#3879,.T.);
#60178=ADVANCED_FACE('',(#7078),#947,.T.);
#60179=ADVANCED_FACE('',(#7079),#822,.T.);
#60180=ADVANCED_FACE('',(#7080),#948,.T.);
#60181=ADVANCED_FACE('',(#7081),#3880,.T.);
#60182=ADVANCED_FACE('',(#7082),#823,.T.);
#60183=ADVANCED_FACE('',(#7083),#824,.T.);
#60184=ADVANCED_FACE('',(#7084),#825,.T.);
#60185=ADVANCED_FACE('',(#7085),#826,.T.);
#60186=ADVANCED_FACE('',(#7086),#827,.T.);
#60187=ADVANCED_FACE('',(#7087),#828,.T.);
#60188=ADVANCED_FACE('',(#7088),#829,.T.);
#60189=ADVANCED_FACE('',(#7089),#830,.T.);
#60190=ADVANCED_FACE('',(#7090),#831,.T.);
#60191=ADVANCED_FACE('',(#7091),#832,.T.);
#60192=ADVANCED_FACE('',(#7092),#833,.T.);
#60193=ADVANCED_FACE('',(#7093),#834,.T.);
#60194=ADVANCED_FACE('',(#7094),#835,.T.);
#60195=ADVANCED_FACE('',(#7095),#836,.T.);
#60196=ADVANCED_FACE('',(#7096),#837,.T.);
#60197=ADVANCED_FACE('',(#7097),#3881,.F.);
#60198=ADVANCED_FACE('',(#7098),#57121,.F.);
#60199=ADVANCED_FACE('',(#7099),#3882,.T.);
#60200=ADVANCED_FACE('',(#7100),#838,.T.);
#60201=ADVANCED_FACE('',(#7101),#57122,.F.);
#60202=ADVANCED_FACE('',(#7102),#3883,.F.);
#60203=ADVANCED_FACE('',(#7103),#3884,.F.);
#60204=ADVANCED_FACE('',(#7104),#3885,.F.);
#60205=ADVANCED_FACE('',(#7105),#3886,.F.);
#60206=ADVANCED_FACE('',(#7106),#3887,.F.);
#60207=ADVANCED_FACE('',(#7107),#3888,.F.);
#60208=ADVANCED_FACE('',(#7108),#3889,.F.);
#60209=ADVANCED_FACE('',(#7109),#3890,.T.);
#60210=ADVANCED_FACE('',(#7110),#949,.T.);
#60211=ADVANCED_FACE('',(#7111),#839,.T.);
#60212=ADVANCED_FACE('',(#7112),#950,.T.);
#60213=ADVANCED_FACE('',(#7113,#1856),#3891,.T.);
#60214=ADVANCED_FACE('',(#7114),#840,.T.);
#60215=ADVANCED_FACE('',(#7115),#841,.T.);
#60216=ADVANCED_FACE('',(#7116),#842,.T.);
#60217=ADVANCED_FACE('',(#7117),#843,.T.);
#60218=ADVANCED_FACE('',(#7118),#844,.T.);
#60219=ADVANCED_FACE('',(#7119),#845,.T.);
#60220=ADVANCED_FACE('',(#7120),#846,.T.);
#60221=ADVANCED_FACE('',(#7121),#847,.T.);
#60222=ADVANCED_FACE('',(#7122),#848,.T.);
#60223=ADVANCED_FACE('',(#7123),#849,.T.);
#60224=ADVANCED_FACE('',(#7124),#850,.T.);
#60225=ADVANCED_FACE('',(#7125),#851,.T.);
#60226=ADVANCED_FACE('',(#7126),#852,.T.);
#60227=ADVANCED_FACE('',(#7127),#853,.T.);
#60228=ADVANCED_FACE('',(#7128),#854,.T.);
#60229=ADVANCED_FACE('',(#7129),#855,.T.);
#60230=ADVANCED_FACE('',(#7130),#856,.T.);
#60231=ADVANCED_FACE('',(#7131),#857,.T.);
#60232=ADVANCED_FACE('',(#7132),#858,.T.);
#60233=ADVANCED_FACE('',(#7133),#859,.T.);
#60234=ADVANCED_FACE('',(#7134),#860,.T.);
#60235=ADVANCED_FACE('',(#7135),#861,.T.);
#60236=ADVANCED_FACE('',(#7136),#862,.T.);
#60237=ADVANCED_FACE('',(#7137),#863,.T.);
#60238=ADVANCED_FACE('',(#7138),#864,.T.);
#60239=ADVANCED_FACE('',(#7139),#3892,.T.);
#60240=ADVANCED_FACE('',(#7140),#57123,.F.);
#60241=ADVANCED_FACE('',(#7141),#3893,.F.);
#60242=ADVANCED_FACE('',(#7142),#865,.T.);
#60243=ADVANCED_FACE('',(#7143),#57124,.F.);
#60244=ADVANCED_FACE('',(#7144),#108,.F.);
#60245=ADVANCED_FACE('',(#7145),#866,.T.);
#60246=ADVANCED_FACE('',(#7146,#1857),#3894,.F.);
#60247=ADVANCED_FACE('',(#7147),#951,.T.);
#60248=ADVANCED_FACE('',(#7148),#3895,.F.);
#60249=ADVANCED_FACE('',(#7149),#3896,.F.);
#60250=ADVANCED_FACE('',(#7150),#3897,.F.);
#60251=ADVANCED_FACE('',(#7151),#3898,.F.);
#60252=ADVANCED_FACE('',(#7152),#867,.T.);
#60253=ADVANCED_FACE('',(#7153),#3899,.F.);
#60254=ADVANCED_FACE('',(#7154),#3900,.F.);
#60255=ADVANCED_FACE('',(#7155),#3901,.F.);
#60256=ADVANCED_FACE('',(#7156),#3902,.F.);
#60257=ADVANCED_FACE('',(#7157),#3903,.F.);
#60258=ADVANCED_FACE('',(#7158),#3904,.F.);
#60259=ADVANCED_FACE('',(#7159),#3905,.F.);
#60260=ADVANCED_FACE('',(#7160),#3906,.F.);
#60261=ADVANCED_FACE('',(#7161),#3907,.F.);
#60262=ADVANCED_FACE('',(#7162),#3908,.F.);
#60263=ADVANCED_FACE('',(#7163),#3909,.F.);
#60264=ADVANCED_FACE('',(#7164),#3910,.F.);
#60265=ADVANCED_FACE('',(#7165),#3911,.F.);
#60266=ADVANCED_FACE('',(#7166),#3912,.F.);
#60267=ADVANCED_FACE('',(#7167),#3913,.F.);
#60268=ADVANCED_FACE('',(#7168),#3914,.F.);
#60269=ADVANCED_FACE('',(#7169),#3915,.F.);
#60270=ADVANCED_FACE('',(#7170),#3916,.F.);
#60271=ADVANCED_FACE('',(#7171),#3917,.F.);
#60272=ADVANCED_FACE('',(#7172),#3918,.F.);
#60273=ADVANCED_FACE('',(#7173),#3919,.F.);
#60274=ADVANCED_FACE('',(#7174),#3920,.F.);
#60275=ADVANCED_FACE('',(#7175),#3921,.F.);
#60276=ADVANCED_FACE('',(#7176),#3922,.F.);
#60277=ADVANCED_FACE('',(#7177),#3923,.F.);
#60278=ADVANCED_FACE('',(#7178),#3924,.F.);
#60279=ADVANCED_FACE('',(#7179),#3925,.F.);
#60280=ADVANCED_FACE('',(#7180),#3926,.F.);
#60281=ADVANCED_FACE('',(#7181),#3927,.F.);
#60282=ADVANCED_FACE('',(#7182),#3928,.F.);
#60283=ADVANCED_FACE('',(#7183),#3929,.F.);
#60284=ADVANCED_FACE('',(#7184),#3930,.F.);
#60285=ADVANCED_FACE('',(#7185),#3931,.F.);
#60286=ADVANCED_FACE('',(#7186),#3932,.F.);
#60287=ADVANCED_FACE('',(#7187),#3933,.F.);
#60288=ADVANCED_FACE('',(#7188),#3934,.F.);
#60289=ADVANCED_FACE('',(#7189),#3935,.F.);
#60290=ADVANCED_FACE('',(#7190),#3936,.F.);
#60291=ADVANCED_FACE('',(#7191),#3937,.F.);
#60292=ADVANCED_FACE('',(#7192),#3938,.F.);
#60293=ADVANCED_FACE('',(#7193),#3939,.F.);
#60294=ADVANCED_FACE('',(#7194),#3940,.F.);
#60295=ADVANCED_FACE('',(#7195),#3941,.F.);
#60296=ADVANCED_FACE('',(#7196),#3942,.F.);
#60297=ADVANCED_FACE('',(#7197),#3943,.F.);
#60298=ADVANCED_FACE('',(#7198),#3944,.F.);
#60299=ADVANCED_FACE('',(#7199),#3945,.F.);
#60300=ADVANCED_FACE('',(#7200),#3946,.F.);
#60301=ADVANCED_FACE('',(#7201),#3947,.F.);
#60302=ADVANCED_FACE('',(#7202),#3948,.F.);
#60303=ADVANCED_FACE('',(#7203),#3949,.F.);
#60304=ADVANCED_FACE('',(#7204),#3950,.F.);
#60305=ADVANCED_FACE('',(#7205),#3951,.F.);
#60306=ADVANCED_FACE('',(#7206),#3952,.F.);
#60307=ADVANCED_FACE('',(#7207),#3953,.F.);
#60308=ADVANCED_FACE('',(#7208),#3954,.F.);
#60309=ADVANCED_FACE('',(#7209),#3955,.F.);
#60310=ADVANCED_FACE('',(#7210),#3956,.F.);
#60311=ADVANCED_FACE('',(#7211),#3957,.F.);
#60312=ADVANCED_FACE('',(#7212),#3958,.F.);
#60313=ADVANCED_FACE('',(#7213),#3959,.F.);
#60314=ADVANCED_FACE('',(#7214),#3960,.F.);
#60315=ADVANCED_FACE('',(#7215),#3961,.F.);
#60316=ADVANCED_FACE('',(#7216),#3962,.F.);
#60317=ADVANCED_FACE('',(#7217),#3963,.F.);
#60318=ADVANCED_FACE('',(#7218),#3964,.F.);
#60319=ADVANCED_FACE('',(#7219),#3965,.F.);
#60320=ADVANCED_FACE('',(#7220),#3966,.F.);
#60321=ADVANCED_FACE('',(#7221),#3967,.F.);
#60322=ADVANCED_FACE('',(#7222),#3968,.F.);
#60323=ADVANCED_FACE('',(#7223),#3969,.F.);
#60324=ADVANCED_FACE('',(#7224),#3970,.F.);
#60325=ADVANCED_FACE('',(#7225),#3971,.F.);
#60326=ADVANCED_FACE('',(#7226),#3972,.F.);
#60327=ADVANCED_FACE('',(#7227),#3973,.F.);
#60328=ADVANCED_FACE('',(#7228),#3974,.F.);
#60329=ADVANCED_FACE('',(#7229),#3975,.F.);
#60330=ADVANCED_FACE('',(#7230),#3976,.F.);
#60331=ADVANCED_FACE('',(#7231),#3977,.F.);
#60332=ADVANCED_FACE('',(#7232),#3978,.F.);
#60333=ADVANCED_FACE('',(#7233),#3979,.F.);
#60334=ADVANCED_FACE('',(#7234),#3980,.F.);
#60335=ADVANCED_FACE('',(#7235),#3981,.F.);
#60336=ADVANCED_FACE('',(#7236),#3982,.F.);
#60337=ADVANCED_FACE('',(#7237),#3983,.F.);
#60338=ADVANCED_FACE('',(#7238),#3984,.F.);
#60339=ADVANCED_FACE('',(#7239),#3985,.F.);
#60340=ADVANCED_FACE('',(#7240),#3986,.F.);
#60341=ADVANCED_FACE('',(#7241),#3987,.F.);
#60342=ADVANCED_FACE('',(#7242),#3988,.F.);
#60343=ADVANCED_FACE('',(#7243),#3989,.F.);
#60344=ADVANCED_FACE('',(#7244),#3990,.F.);
#60345=ADVANCED_FACE('',(#7245),#3991,.F.);
#60346=ADVANCED_FACE('',(#7246),#3992,.F.);
#60347=ADVANCED_FACE('',(#7247),#3993,.F.);
#60348=ADVANCED_FACE('',(#7248),#3994,.F.);
#60349=ADVANCED_FACE('',(#7249),#3995,.F.);
#60350=ADVANCED_FACE('',(#7250),#3996,.F.);
#60351=ADVANCED_FACE('',(#7251),#3997,.F.);
#60352=ADVANCED_FACE('',(#7252),#3998,.F.);
#60353=ADVANCED_FACE('',(#7253),#3999,.F.);
#60354=ADVANCED_FACE('',(#7254),#4000,.F.);
#60355=ADVANCED_FACE('',(#7255),#4001,.F.);
#60356=ADVANCED_FACE('',(#7256),#4002,.F.);
#60357=ADVANCED_FACE('',(#7257),#4003,.F.);
#60358=ADVANCED_FACE('',(#7258),#109,.T.);
#60359=ADVANCED_FACE('',(#7259),#952,.T.);
#60360=ADVANCED_FACE('',(#7260,#1858),#4004,.T.);
#60361=ADVANCED_FACE('',(#7261),#953,.F.);
#60362=ADVANCED_FACE('',(#7262),#868,.T.);
#60363=ADVANCED_FACE('',(#7263),#869,.T.);
#60364=ADVANCED_FACE('',(#7264),#870,.T.);
#60365=ADVANCED_FACE('',(#7265),#871,.T.);
#60366=ADVANCED_FACE('',(#7266),#872,.T.);
#60367=ADVANCED_FACE('',(#7267),#873,.T.);
#60368=ADVANCED_FACE('',(#7268),#4005,.F.);
#60369=ADVANCED_FACE('',(#7269),#4006,.F.);
#60370=ADVANCED_FACE('',(#7270),#4007,.F.);
#60371=ADVANCED_FACE('',(#7271),#4008,.T.);
#60372=ADVANCED_FACE('',(#7272),#4009,.T.);
#60373=ADVANCED_FACE('',(#7273),#4010,.T.);
#60374=ADVANCED_FACE('',(#7274),#4011,.T.);
#60375=ADVANCED_FACE('',(#7275),#4012,.T.);
#60376=ADVANCED_FACE('',(#7276),#4013,.T.);
#60377=ADVANCED_FACE('',(#7277),#4014,.F.);
#60378=ADVANCED_FACE('',(#7278),#4015,.F.);
#60379=ADVANCED_FACE('',(#7279),#4016,.F.);
#60380=ADVANCED_FACE('',(#7280),#4017,.F.);
#60381=ADVANCED_FACE('',(#7281),#4018,.F.);
#60382=ADVANCED_FACE('',(#7282),#4019,.F.);
#60383=ADVANCED_FACE('',(#7283),#954,.F.);
#60384=ADVANCED_FACE('',(#7284),#4020,.F.);
#60385=ADVANCED_FACE('',(#7285),#4021,.F.);
#60386=ADVANCED_FACE('',(#7286),#4022,.F.);
#60387=ADVANCED_FACE('',(#7287),#4023,.T.);
#60388=ADVANCED_FACE('',(#7288),#955,.T.);
#60389=ADVANCED_FACE('',(#7289),#874,.T.);
#60390=ADVANCED_FACE('',(#7290),#956,.T.);
#60391=ADVANCED_FACE('',(#7291),#4024,.T.);
#60392=CLOSED_SHELL('',(#57125,#57126,#57127,#57128,#57129,#57130,#57131,
#57132,#57133,#57134,#57135,#57136,#57137,#57138,#57139,#57140,#57141,#57142,
#57143,#57144,#57145,#57146,#57147,#57148,#57149,#57150,#57151,#57152,#57153,
#57154,#57155,#57156,#57157,#57158,#57159,#57160,#57161,#57162,#57163,#57164,
#57165,#57166,#57167,#57168,#57169,#57170,#57171,#57172,#57173,#57174,#57175,
#57176,#57177,#57178,#57179,#57180,#57181,#57182,#57183,#57184,#57185,#57186,
#57187,#57188,#57189,#57190,#57191,#57192,#57193,#57194,#57195,#57196,#57197,
#57198,#57199,#57200,#57201,#57202,#57203,#57204,#57205,#57206,#57207,#57208,
#57209,#57210,#57211,#57212,#57213,#57214,#57215,#57216,#57217,#57218,#57219,
#57220,#57221,#57222,#57223,#57224,#57225,#57226,#57227,#57228,#57229,#57230,
#57231,#57232,#57233,#57234,#57235,#57236,#57237,#57238,#57239,#57240,#57241,
#57242,#57243,#57244,#57245,#57246,#57247,#57248,#57249,#57250,#57251,#57252,
#57253,#57254,#57255,#57256,#57257,#57258,#57259,#57260,#57261,#57262,#57263,
#57264,#57265,#57266,#57267,#57268,#57269,#57270,#57271,#57272,#57273,#57274,
#57275,#57276,#57277,#57278,#57279,#57280,#57281,#57282,#57283,#57284,#57285,
#57286,#57287,#57288,#57289,#57290,#57291,#57292,#57293,#57294,#57295,#57296,
#57297,#57298,#57299,#57300,#57301,#57302,#57303,#57304,#57305,#57306,#57307,
#57308,#57309,#57310,#57311,#57312,#57313,#57314,#57315,#57316,#57317,#57318,
#57319,#57320,#57321,#57322,#57323,#57324,#57325,#57326,#57327,#57328,#57329,
#57330,#57331,#57332,#57333,#57334,#57335,#57336,#57337,#57338,#57339,#57340,
#57341,#57342,#57343,#57344,#57345,#57346,#57347,#57348,#57349,#57350,#57351,
#57352,#57353,#57354,#57355,#57356,#57357,#57358,#57359,#57360,#57361,#57362,
#57363,#57364,#57365,#57366,#57367,#57368,#57369,#57370,#57371,#57372,#57373,
#57374,#57375,#57376,#57377,#57378,#57379,#57380,#57381,#57382,#57383,#57384,
#57385,#57386,#57387,#57388,#57389,#57390,#57391,#57392,#57393,#57394,#57395,
#57396,#57397,#57398,#57399,#57400,#57401,#57402,#57403,#57404,#57405,#57406,
#57407,#57408,#57409,#57410,#57411,#57412,#57413,#57414,#57415,#57416,#57417,
#57418,#57419,#57420,#57421,#57422,#57423,#57424,#57425,#57426,#57427,#57428,
#57429,#57430,#57431,#57432,#57433,#57434,#57435,#57436,#57437,#57438,#57439,
#57440,#57441,#57442,#57443,#57444,#57445,#57446,#57447,#57448,#57449,#57450,
#57451,#57452,#57453,#57454,#57455,#57456,#57457,#57458,#57459,#57460,#57461,
#57462,#57463,#57464,#57465,#57466,#57467,#57468,#57469,#57470,#57471,#57472,
#57473,#57474,#57475,#57476,#57477,#57478,#57479,#57480,#57481,#57482,#57483,
#57484,#57485,#57486,#57487,#57488,#57489,#57490,#57491,#57492,#57493,#57494,
#57495,#57496,#57497,#57498,#57499,#57500,#57501,#57502,#57503,#57504,#57505,
#57506,#57507,#57508,#57509,#57510,#57511,#57512,#57513,#57514,#57515,#57516,
#57517,#57518,#57519,#57520,#57521,#57522,#57523,#57524,#57525,#57526,#57527,
#57528,#57529,#57530,#57531,#57532,#57533,#57534,#57535,#57536,#57537,#57538,
#57539,#57540,#57541,#57542,#57543,#57544,#57545,#57546,#57547,#57548,#57549,
#57550,#57551,#57552,#57553,#57554,#57555,#57556,#57557,#57558,#57559,#57560,
#57561,#57562,#57563,#57564,#57565,#57566,#57567,#57568,#57569,#57570,#57571,
#57572,#57573,#57574,#57575,#57576,#57577,#57578,#57579,#57580,#57581,#57582,
#57583,#57584,#57585,#57586,#57587,#57588,#57589,#57590,#57591,#57592,#57593,
#57594,#57595,#57596,#57597,#57598,#57599,#57600,#57601,#57602,#57603,#57604,
#57605,#57606,#57607,#57608,#57609,#57610,#57611,#57612,#57613,#57614,#57615,
#57616,#57617,#57618,#57619,#57620,#57621,#57622,#57623,#57624,#57625,#57626,
#57627,#57628,#57629,#57630,#57631,#57632,#57633,#57634,#57635,#57636,#57637,
#57638,#57639,#57640,#57641,#57642,#57643,#57644,#57645,#57646,#57647,#57648,
#57649,#57650,#57651,#57652,#57653,#57654,#57655,#57656,#57657,#57658,#57659,
#57660,#57661,#57662,#57663,#57664,#57665,#57666,#57667,#57668,#57669,#57670,
#57671,#57672,#57673,#57674,#57675,#57676,#57677,#57678,#57679,#57680,#57681,
#57682,#57683,#57684,#57685,#57686,#57687,#57688,#57689,#57690,#57691,#57692,
#57693,#57694,#57695,#57696,#57697,#57698,#57699,#57700,#57701,#57702,#57703,
#57704,#57705,#57706,#57707,#57708,#57709,#57710,#57711,#57712,#57713,#57714,
#57715,#57716,#57717,#57718,#57719,#57720,#57721,#57722,#57723,#57724,#57725,
#57726,#57727,#57728,#57729,#57730,#57731,#57732,#57733,#57734,#57735,#57736,
#57737,#57738,#57739,#57740,#57741,#57742,#57743,#57744,#57745,#57746,#57747,
#57748,#57749,#57750,#57751,#57752,#57753,#57754,#57755,#57756,#57757,#57758,
#57759,#57760,#57761,#57762,#57763,#57764,#57765,#57766,#57767,#57768,#57769,
#57770,#57771,#57772,#57773,#57774,#57775,#57776,#57777,#57778,#57779,#57780,
#57781,#57782,#57783,#57784,#57785,#57786,#57787,#57788,#57789,#57790,#57791,
#57792,#57793,#57794,#57795,#57796,#57797,#57798,#57799,#57800,#57801,#57802,
#57803,#57804,#57805,#57806,#57807,#57808,#57809,#57810,#57811,#57812,#57813,
#57814,#57815,#57816,#57817,#57818,#57819,#57820,#57821,#57822,#57823,#57824,
#57825,#57826,#57827,#57828,#57829,#57830,#57831,#57832,#57833,#57834,#57835,
#57836,#57837,#57838,#57839,#57840,#57841,#57842,#57843,#57844,#57845,#57846,
#57847,#57848,#57849,#57850,#57851,#57852,#57853,#57854,#57855,#57856,#57857,
#57858,#57859,#57860,#57861,#57862,#57863,#57864,#57865,#57866,#57867,#57868,
#57869,#57870,#57871,#57872,#57873,#57874,#57875,#57876,#57877,#57878,#57879,
#57880,#57881,#57882,#57883,#57884,#57885,#57886,#57887,#57888,#57889,#57890,
#57891,#57892,#57893,#57894,#57895,#57896,#57897,#57898,#57899,#57900,#57901,
#57902,#57903,#57904,#57905,#57906,#57907,#57908,#57909,#57910,#57911,#57912,
#57913,#57914,#57915,#57916,#57917,#57918,#57919,#57920,#57921,#57922,#57923,
#57924,#57925,#57926,#57927,#57928,#57929,#57930,#57931,#57932,#57933,#57934,
#57935,#57936,#57937,#57938,#57939,#57940,#57941,#57942,#57943,#57944,#57945,
#57946,#57947,#57948,#57949,#57950,#57951,#57952,#57953,#57954,#57955,#57956,
#57957,#57958,#57959,#57960,#57961,#57962,#57963,#57964,#57965,#57966,#57967,
#57968,#57969,#57970,#57971,#57972,#57973,#57974,#57975,#57976,#57977,#57978,
#57979,#57980,#57981,#57982,#57983,#57984,#57985,#57986,#57987,#57988,#57989,
#57990,#57991,#57992,#57993,#57994,#57995,#57996,#57997,#57998,#57999,#58000,
#58001,#58002,#58003,#58004,#58005,#58006,#58007,#58008,#58009,#58010,#58011,
#58012,#58013,#58014,#58015,#58016,#58017,#58018,#58019,#58020,#58021,#58022,
#58023,#58024,#58025,#58026,#58027,#58028,#58029,#58030,#58031,#58032,#58033,
#58034,#58035,#58036,#58037,#58038,#58039,#58040,#58041,#58042,#58043,#58044,
#58045,#58046,#58047,#58048,#58049,#58050,#58051,#58052,#58053,#58054,#58055,
#58056,#58057,#58058,#58059,#58060,#58061,#58062,#58063,#58064,#58065,#58066,
#58067,#58068,#58069,#58070,#58071,#58072,#58073,#58074,#58075,#58076,#58077,
#58078,#58079,#58080,#58081,#58082,#58083,#58084,#58085,#58086,#58087,#58088,
#58089,#58090,#58091,#58092,#58093,#58094,#58095,#58096,#58097,#58098,#58099,
#58100,#58101,#58102,#58103,#58104,#58105,#58106,#58107,#58108,#58109,#58110,
#58111,#58112,#58113,#58114,#58115,#58116,#58117,#58118,#58119,#58120,#58121,
#58122,#58123,#58124,#58125,#58126,#58127,#58128,#58129,#58130,#58131,#58132,
#58133,#58134,#58135,#58136,#58137,#58138,#58139,#58140,#58141,#58142,#58143,
#58144,#58145,#58146,#58147,#58148,#58149,#58150,#58151,#58152,#58153,#58154,
#58155,#58156,#58157,#58158,#58159,#58160,#58161,#58162,#58163,#58164,#58165,
#58166,#58167,#58168,#58169,#58170,#58171,#58172,#58173,#58174,#58175,#58176,
#58177,#58178,#58179,#58180,#58181,#58182,#58183,#58184,#58185,#58186,#58187,
#58188,#58189,#58190,#58191,#58192,#58193,#58194,#58195,#58196,#58197,#58198,
#58199,#58200,#58201,#58202,#58203,#58204,#58205,#58206,#58207,#58208,#58209,
#58210,#58211,#58212,#58213,#58214,#58215,#58216,#58217,#58218,#58219,#58220,
#58221,#58222,#58223,#58224,#58225,#58226,#58227,#58228,#58229,#58230,#58231,
#58232,#58233,#58234,#58235,#58236,#58237,#58238,#58239,#58240,#58241,#58242,
#58243,#58244,#58245,#58246,#58247,#58248,#58249,#58250,#58251,#58252,#58253,
#58254,#58255,#58256,#58257,#58258,#58259,#58260,#58261,#58262,#58263,#58264,
#58265,#58266,#58267,#58268,#58269,#58270,#58271,#58272,#58273,#58274,#58275,
#58276,#58277,#58278,#58279,#58280,#58281,#58282,#58283,#58284,#58285,#58286,
#58287,#58288,#58289,#58290,#58291,#58292,#58293,#58294,#58295,#58296,#58297,
#58298,#58299,#58300,#58301,#58302,#58303,#58304,#58305,#58306,#58307,#58308,
#58309,#58310,#58311,#58312,#58313,#58314,#58315,#58316,#58317,#58318,#58319,
#58320,#58321,#58322,#58323,#58324,#58325,#58326,#58327,#58328,#58329,#58330,
#58331,#58332,#58333,#58334,#58335,#58336,#58337,#58338,#58339,#58340,#58341,
#58342,#58343,#58344,#58345,#58346,#58347,#58348,#58349,#58350,#58351,#58352,
#58353,#58354,#58355,#58356,#58357,#58358,#58359,#58360,#58361,#58362,#58363,
#58364,#58365,#58366,#58367,#58368,#58369,#58370,#58371,#58372,#58373,#58374,
#58375,#58376,#58377,#58378,#58379,#58380,#58381,#58382,#58383,#58384,#58385,
#58386,#58387,#58388,#58389,#58390,#58391,#58392,#58393,#58394,#58395,#58396,
#58397,#58398,#58399,#58400,#58401,#58402,#58403,#58404,#58405,#58406,#58407,
#58408,#58409,#58410,#58411,#58412,#58413,#58414,#58415,#58416,#58417,#58418,
#58419,#58420,#58421,#58422,#58423,#58424,#58425,#58426,#58427,#58428,#58429,
#58430,#58431,#58432,#58433,#58434,#58435,#58436,#58437,#58438,#58439,#58440,
#58441,#58442,#58443,#58444,#58445,#58446,#58447,#58448,#58449,#58450,#58451,
#58452,#58453,#58454,#58455,#58456,#58457,#58458,#58459,#58460,#58461,#58462,
#58463,#58464,#58465,#58466,#58467,#58468,#58469,#58470,#58471,#58472,#58473,
#58474,#58475,#58476,#58477,#58478,#58479,#58480,#58481,#58482,#58483,#58484,
#58485,#58486,#58487,#58488,#58489,#58490,#58491,#58492,#58493,#58494,#58495,
#58496,#58497,#58498,#58499,#58500,#58501,#58502,#58503,#58504,#58505,#58506,
#58507,#58508,#58509,#58510,#58511,#58512,#58513,#58514,#58515,#58516,#58517,
#58518,#58519,#58520,#58521,#58522,#58523,#58524,#58525,#58526,#58527,#58528,
#58529,#58530,#58531,#58532,#58533,#58534,#58535,#58536,#58537,#58538,#58539,
#58540,#58541,#58542,#58543,#58544,#58545,#58546,#58547,#58548,#58549,#58550,
#58551,#58552,#58553,#58554,#58555,#58556,#58557,#58558,#58559,#58560,#58561,
#58562,#58563,#58564,#58565,#58566,#58567,#58568,#58569,#58570,#58571,#58572,
#58573,#58574,#58575,#58576,#58577,#58578,#58579,#58580,#58581,#58582,#58583,
#58584,#58585,#58586,#58587,#58588,#58589,#58590,#58591,#58592,#58593,#58594,
#58595,#58596,#58597,#58598,#58599,#58600,#58601,#58602,#58603,#58604,#58605,
#58606,#58607,#58608,#58609,#58610,#58611,#58612,#58613,#58614,#58615,#58616,
#58617,#58618,#58619,#58620,#58621,#58622,#58623,#58624,#58625,#58626,#58627,
#58628,#58629,#58630,#58631,#58632,#58633,#58634,#58635,#58636,#58637,#58638,
#58639,#58640,#58641,#58642,#58643,#58644,#58645,#58646,#58647,#58648,#58649,
#58650,#58651,#58652,#58653,#58654,#58655,#58656,#58657,#58658,#58659,#58660,
#58661,#58662,#58663,#58664,#58665,#58666,#58667,#58668,#58669,#58670,#58671,
#58672,#58673,#58674,#58675,#58676,#58677,#58678,#58679,#58680,#58681,#58682,
#58683,#58684,#58685,#58686,#58687,#58688,#58689,#58690,#58691,#58692,#58693,
#58694,#58695,#58696,#58697,#58698,#58699,#58700,#58701,#58702,#58703,#58704,
#58705,#58706,#58707,#58708,#58709,#58710,#58711,#58712,#58713,#58714,#58715,
#58716,#58717,#58718,#58719,#58720,#58721,#58722,#58723,#58724,#58725,#58726,
#58727,#58728,#58729,#58730,#58731,#58732,#58733,#58734,#58735,#58736,#58737,
#58738,#58739,#58740,#58741,#58742,#58743,#58744,#58745,#58746,#58747,#58748,
#58749,#58750,#58751,#58752,#58753,#58754,#58755,#58756,#58757,#58758,#58759,
#58760,#58761,#58762,#58763,#58764,#58765,#58766,#58767,#58768,#58769,#58770,
#58771,#58772,#58773,#58774,#58775,#58776,#58777,#58778,#58779,#58780,#58781,
#58782,#58783,#58784,#58785,#58786,#58787,#58788,#58789,#58790,#58791,#58792,
#58793,#58794,#58795,#58796,#58797,#58798,#58799,#58800,#58801,#58802,#58803,
#58804,#58805,#58806,#58807,#58808,#58809,#58810,#58811,#58812,#58813,#58814,
#58815,#58816,#58817,#58818,#58819,#58820,#58821,#58822,#58823,#58824,#58825,
#58826,#58827,#58828,#58829,#58830,#58831,#58832,#58833,#58834,#58835,#58836,
#58837,#58838,#58839,#58840,#58841,#58842,#58843,#58844,#58845,#58846,#58847,
#58848,#58849,#58850,#58851,#58852,#58853,#58854,#58855,#58856,#58857,#58858,
#58859,#58860,#58861,#58862,#58863,#58864,#58865,#58866,#58867,#58868,#58869,
#58870,#58871,#58872,#58873,#58874,#58875,#58876,#58877,#58878,#58879,#58880,
#58881,#58882,#58883,#58884,#58885,#58886,#58887,#58888,#58889,#58890,#58891,
#58892,#58893,#58894,#58895,#58896,#58897,#58898,#58899,#58900,#58901,#58902,
#58903,#58904,#58905,#58906,#58907,#58908,#58909,#58910,#58911,#58912,#58913,
#58914,#58915,#58916,#58917,#58918,#58919,#58920,#58921,#58922,#58923,#58924,
#58925,#58926,#58927,#58928,#58929,#58930,#58931,#58932,#58933,#58934,#58935,
#58936,#58937,#58938,#58939,#58940,#58941,#58942,#58943,#58944,#58945,#58946,
#58947,#58948,#58949,#58950,#58951,#58952,#58953,#58954,#58955,#58956,#58957,
#58958,#58959,#58960,#58961,#58962,#58963,#58964,#58965,#58966,#58967,#58968,
#58969,#58970,#58971));
#60393=CLOSED_SHELL('',(#58972,#58973,#58974,#58975,#58976,#58977,#58978,
#58979,#58980,#58981,#58982,#58983,#58984,#58985,#58986,#58987,#58988,#58989,
#58990,#58991,#58992,#58993,#58994,#58995,#58996,#58997,#58998,#58999,#59000,
#59001,#59002,#59003,#59004,#59005,#59006,#59007,#59008,#59009,#59010,#59011,
#59012,#59013,#59014,#59015,#59016,#59017,#59018,#59019,#59020,#59021,#59022,
#59023,#59024,#59025,#59026,#59027,#59028,#59029,#59030,#59031,#59032,#59033,
#59034,#59035,#59036,#59037,#59038,#59039,#59040,#59041,#59042,#59043,#59044,
#59045,#59046,#59047,#59048,#59049));
#60394=CLOSED_SHELL('',(#59050,#59051,#59052,#59053,#59054,#59055,#59056,
#59057,#59058,#59059,#59060,#59061,#59062,#59063,#59064,#59065,#59066));
#60395=CLOSED_SHELL('',(#59067,#59068,#59069,#59070,#59071,#59072,#59073,
#59074,#59075,#59076,#59077));
#60396=CLOSED_SHELL('',(#59078,#59079,#59080,#59081,#59082,#59083,#59084,
#59085,#59086,#59087,#59088,#59089,#59090,#59091,#59092,#59093,#59094,#59095,
#59096,#59097,#59098,#59099,#59100,#59101,#59102,#59103,#59104,#59105,#59106,
#59107,#59108,#59109,#59110,#59111,#59112,#59113,#59114,#59115,#59116,#59117,
#59118,#59119,#59120,#59121,#59122,#59123,#59124,#59125,#59126,#59127,#59128,
#59129,#59130,#59131,#59132,#59133,#59134,#59135,#59136,#59137,#59138,#59139,
#59140,#59141,#59142,#59143,#59144,#59145,#59146,#59147,#59148,#59149,#59150,
#59151,#59152,#59153,#59154,#59155,#59156,#59157,#59158,#59159,#59160,#59161,
#59162,#59163,#59164,#59165,#59166,#59167,#59168,#59169,#59170,#59171,#59172,
#59173,#59174,#59175,#59176,#59177,#59178,#59179,#59180,#59181,#59182,#59183));
#60397=CLOSED_SHELL('',(#59184,#59185,#59186,#59187,#59188,#59189,#59190,
#59191,#59192,#59193,#59194,#59195,#59196,#59197,#59198,#59199,#59200,#59201,
#59202,#59203,#59204,#59205,#59206,#59207,#59208,#59209,#59210,#59211,#59212,
#59213,#59214,#59215,#59216,#59217,#59218,#59219,#59220,#59221,#59222,#59223,
#59224,#59225,#59226,#59227,#59228,#59229,#59230,#59231,#59232,#59233,#59234,
#59235,#59236,#59237,#59238,#59239,#59240,#59241,#59242,#59243,#59244,#59245,
#59246,#59247,#59248,#59249,#59250,#59251,#59252,#59253,#59254,#59255,#59256,
#59257,#59258,#59259,#59260,#59261,#59262,#59263,#59264,#59265,#59266,#59267,
#59268,#59269,#59270,#59271,#59272,#59273,#59274,#59275,#59276,#59277,#59278,
#59279,#59280,#59281,#59282,#59283,#59284,#59285,#59286,#59287,#59288,#59289,
#59290,#59291,#59292,#59293,#59294,#59295,#59296,#59297,#59298,#59299,#59300,
#59301,#59302,#59303,#59304,#59305,#59306,#59307,#59308,#59309,#59310,#59311,
#59312,#59313,#59314,#59315,#59316,#59317,#59318,#59319,#59320,#59321,#59322));
#60398=CLOSED_SHELL('',(#59323,#59324,#59325,#59326,#59327,#59328,#59329,
#59330,#59331,#59332));
#60399=CLOSED_SHELL('',(#59333,#59334,#59335,#59336,#59337,#59338,#59339,
#59340,#59341,#59342,#59343,#59344,#59345,#59346,#59347,#59348,#59349,#59350,
#59351,#59352,#59353,#59354,#59355,#59356,#59357,#59358,#59359,#59360,#59361,
#59362,#59363,#59364,#59365,#59366,#59367,#59368,#59369,#59370,#59371,#59372,
#59373,#59374,#59375,#59376,#59377,#59378,#59379,#59380,#59381,#59382,#59383,
#59384,#59385,#59386,#59387,#59388,#59389,#59390,#59391,#59392,#59393,#59394,
#59395,#59396,#59397,#59398,#59399,#59400,#59401,#59402,#59403,#59404,#59405,
#59406,#59407,#59408,#59409,#59410,#59411,#59412,#59413,#59414,#59415,#59416,
#59417,#59418,#59419,#59420,#59421,#59422,#59423,#59424,#59425,#59426,#59427,
#59428,#59429,#59430,#59431,#59432,#59433,#59434,#59435,#59436,#59437,#59438,
#59439,#59440,#59441,#59442,#59443,#59444,#59445,#59446,#59447,#59448,#59449,
#59450,#59451,#59452,#59453,#59454,#59455,#59456,#59457,#59458,#59459,#59460,
#59461,#59462,#59463,#59464,#59465,#59466,#59467,#59468,#59469,#59470,#59471,
#59472,#59473,#59474,#59475,#59476,#59477,#59478,#59479,#59480,#59481,#59482,
#59483,#59484,#59485,#59486,#59487,#59488,#59489,#59490,#59491,#59492,#59493,
#59494,#59495,#59496,#59497,#59498,#59499,#59500,#59501,#59502,#59503,#59504,
#59505,#59506,#59507,#59508,#59509,#59510,#59511,#59512,#59513,#59514,#59515,
#59516,#59517,#59518,#59519,#59520,#59521,#59522,#59523,#59524,#59525,#59526,
#59527,#59528,#59529,#59530,#59531,#59532,#59533,#59534,#59535,#59536,#59537,
#59538,#59539,#59540,#59541,#59542,#59543,#59544,#59545,#59546,#59547,#59548,
#59549,#59550,#59551,#59552,#59553,#59554,#59555,#59556,#59557,#59558,#59559,
#59560,#59561,#59562,#59563,#59564,#59565,#59566,#59567,#59568,#59569,#59570,
#59571,#59572,#59573,#59574,#59575,#59576,#59577,#59578,#59579,#59580,#59581,
#59582,#59583,#59584,#59585,#59586,#59587,#59588,#59589,#59590,#59591,#59592,
#59593,#59594,#59595,#59596,#59597,#59598,#59599,#59600,#59601,#59602,#59603,
#59604,#59605,#59606,#59607,#59608,#59609,#59610,#59611,#59612,#59613,#59614,
#59615,#59616,#59617,#59618,#59619,#59620,#59621,#59622,#59623,#59624,#59625,
#59626,#59627,#59628,#59629,#59630,#59631,#59632,#59633,#59634,#59635,#59636,
#59637,#59638,#59639,#59640,#59641,#59642,#59643,#59644,#59645,#59646,#59647,
#59648,#59649,#59650,#59651,#59652,#59653,#59654,#59655,#59656,#59657,#59658,
#59659,#59660,#59661,#59662,#59663,#59664,#59665,#59666,#59667,#59668,#59669,
#59670,#59671,#59672,#59673,#59674,#59675,#59676,#59677,#59678,#59679,#59680,
#59681,#59682,#59683,#59684,#59685,#59686,#59687,#59688,#59689,#59690,#59691,
#59692,#59693,#59694,#59695,#59696,#59697,#59698,#59699,#59700,#59701,#59702,
#59703,#59704,#59705,#59706,#59707,#59708,#59709,#59710,#59711,#59712,#59713,
#59714,#59715,#59716,#59717,#59718,#59719,#59720,#59721,#59722,#59723,#59724,
#59725,#59726,#59727,#59728,#59729,#59730,#59731,#59732,#59733,#59734,#59735,
#59736,#59737,#59738,#59739,#59740,#59741,#59742,#59743,#59744,#59745,#59746,
#59747,#59748,#59749,#59750,#59751,#59752,#59753,#59754,#59755,#59756,#59757,
#59758,#59759,#59760,#59761,#59762,#59763,#59764,#59765,#59766,#59767,#59768,
#59769,#59770,#59771,#59772,#59773,#59774,#59775,#59776,#59777,#59778,#59779,
#59780,#59781,#59782,#59783,#59784,#59785,#59786,#59787,#59788,#59789,#59790,
#59791,#59792,#59793,#59794,#59795,#59796,#59797,#59798,#59799,#59800,#59801,
#59802,#59803,#59804,#59805,#59806,#59807,#59808,#59809,#59810,#59811,#59812,
#59813,#59814,#59815,#59816,#59817,#59818,#59819,#59820,#59821,#59822,#59823,
#59824,#59825,#59826,#59827,#59828,#59829,#59830,#59831,#59832,#59833,#59834,
#59835,#59836,#59837,#59838,#59839,#59840,#59841,#59842,#59843,#59844,#59845,
#59846,#59847,#59848));
#60400=CLOSED_SHELL('',(#59849,#59850,#59851,#59852,#59853,#59854,#59855,
#59856,#59857,#59858,#59859,#59860,#59861,#59862,#59863,#59864,#59865,#59866,
#59867));
#60401=CLOSED_SHELL('',(#59868,#59869,#59870,#59871,#59872,#59873,#59874,
#59875,#59876,#59877,#59878,#59879,#59880,#59881,#59882,#59883,#59884,#59885,
#59886,#59887,#59888,#59889,#59890,#59891,#59892,#59893,#59894,#59895,#59896,
#59897,#59898,#59899,#59900,#59901,#59902,#59903,#59904,#59905,#59906,#59907,
#59908,#59909,#59910,#59911,#59912,#59913,#59914,#59915,#59916,#59917,#59918,
#59919,#59920,#59921,#59922,#59923,#59924,#59925,#59926,#59927,#59928,#59929,
#59930,#59931,#59932,#59933,#59934,#59935,#59936,#59937,#59938,#59939,#59940,
#59941,#59942,#59943,#59944,#59945,#59946,#59947,#59948,#59949));
#60402=CLOSED_SHELL('',(#59950,#59951,#59952,#59953,#59954,#59955,#59956,
#59957,#59958,#59959,#59960,#59961,#59962,#59963,#59964,#59965,#59966,#59967,
#59968,#59969,#59970,#59971,#59972,#59973,#59974,#59975,#59976,#59977,#59978,
#59979,#59980,#59981,#59982,#59983,#59984,#59985,#59986,#59987,#59988));
#60403=CLOSED_SHELL('',(#59989,#59990,#59991,#59992,#59993,#59994,#59995,
#59996,#59997,#59998,#59999,#60000,#60001,#60002,#60003,#60004,#60005,#60006,
#60007,#60008,#60009,#60010,#60011,#60012,#60013,#60014,#60015,#60016,#60017,
#60018,#60019,#60020,#60021,#60022,#60023,#60024,#60025,#60026,#60027,#60028,
#60029,#60030,#60031,#60032,#60033));
#60404=CLOSED_SHELL('',(#60034,#60035,#60036,#60037,#60038,#60039,#60040,
#60041,#60042,#60043,#60044,#60045,#60046,#60047,#60048,#60049,#60050,#60051,
#60052,#60053,#60054,#60055,#60056,#60057,#60058,#60059,#60060,#60061,#60062,
#60063,#60064,#60065,#60066,#60067,#60068,#60069,#60070,#60071,#60072,#60073,
#60074,#60075,#60076));
#60405=CLOSED_SHELL('',(#60077,#60078,#60079,#60080,#60081,#60082,#60083,
#60084,#60085,#60086,#60087,#60088,#60089,#60090,#60091,#60092,#60093,#60094,
#60095,#60096,#60097,#60098,#60099,#60100,#60101,#60102,#60103,#60104,#60105,
#60106,#60107,#60108,#60109,#60110,#60111,#60112,#60113,#60114,#60115,#60116,
#60117,#60118,#60119,#60120,#60121,#60122,#60123,#60124,#60125,#60126,#60127,
#60128,#60129,#60130,#60131,#60132,#60133));
#60406=CLOSED_SHELL('',(#60134,#60135,#60136,#60137,#60138,#60139,#60140,
#60141,#60142,#60143,#60144,#60145,#60146,#60147,#60148,#60149,#60150,#60151,
#60152,#60153,#60154,#60155,#60156,#60157,#60158,#60159,#60160,#60161,#60162,
#60163,#60164,#60165,#60166,#60167,#60168,#60169,#60170,#60171,#60172,#60173,
#60174,#60175,#60176,#60177,#60178,#60179,#60180,#60181));
#60407=CLOSED_SHELL('',(#60182,#60183,#60184,#60185,#60186,#60187,#60188,
#60189,#60190,#60191,#60192,#60193,#60194,#60195,#60196,#60197,#60198,#60199,
#60200,#60201,#60202,#60203,#60204,#60205,#60206,#60207,#60208,#60209,#60210,
#60211,#60212,#60213));
#60408=CLOSED_SHELL('',(#60214,#60215,#60216,#60217,#60218,#60219,#60220,
#60221,#60222,#60223,#60224,#60225,#60226,#60227,#60228,#60229,#60230,#60231,
#60232,#60233,#60234,#60235,#60236,#60237,#60238,#60239,#60240,#60241,#60242,
#60243,#60244,#60245,#60246,#60247,#60248,#60249,#60250,#60251,#60252,#60253,
#60254,#60255,#60256,#60257,#60258,#60259,#60260,#60261,#60262,#60263,#60264,
#60265,#60266,#60267,#60268,#60269,#60270,#60271,#60272,#60273,#60274,#60275,
#60276,#60277,#60278,#60279,#60280,#60281,#60282,#60283,#60284,#60285,#60286,
#60287,#60288,#60289,#60290,#60291,#60292,#60293,#60294,#60295,#60296,#60297,
#60298,#60299,#60300,#60301,#60302,#60303,#60304,#60305,#60306,#60307,#60308,
#60309,#60310,#60311,#60312,#60313,#60314,#60315,#60316,#60317,#60318,#60319,
#60320,#60321,#60322,#60323,#60324,#60325,#60326,#60327,#60328,#60329,#60330,
#60331,#60332,#60333,#60334,#60335,#60336,#60337,#60338,#60339,#60340,#60341,
#60342,#60343,#60344,#60345,#60346,#60347,#60348,#60349,#60350,#60351,#60352,
#60353,#60354,#60355,#60356,#60357,#60358,#60359,#60360,#60361,#60362,#60363,
#60364,#60365,#60366,#60367,#60368,#60369,#60370,#60371,#60372,#60373,#60374,
#60375,#60376,#60377,#60378,#60379,#60380,#60381,#60382,#60383,#60384,#60385,
#60386));
#60409=CLOSED_SHELL('',(#60387,#60388,#60389,#60390,#60391));
#60410=DERIVED_UNIT_ELEMENT(#60446,1.);
#60411=DERIVED_UNIT_ELEMENT(#113986,-3.);
#60412=DERIVED_UNIT_ELEMENT(#60446,1.);
#60413=DERIVED_UNIT_ELEMENT(#113986,-3.);
#60414=DERIVED_UNIT_ELEMENT(#60446,1.);
#60415=DERIVED_UNIT_ELEMENT(#113986,-3.);
#60416=DERIVED_UNIT_ELEMENT(#60446,1.);
#60417=DERIVED_UNIT_ELEMENT(#113986,-3.);
#60418=DERIVED_UNIT_ELEMENT(#60446,1.);
#60419=DERIVED_UNIT_ELEMENT(#113986,-3.);
#60420=DERIVED_UNIT_ELEMENT(#60446,1.);
#60421=DERIVED_UNIT_ELEMENT(#113986,-3.);
#60422=DERIVED_UNIT_ELEMENT(#60446,1.);
#60423=DERIVED_UNIT_ELEMENT(#113986,-3.);
#60424=DERIVED_UNIT_ELEMENT(#60446,1.);
#60425=DERIVED_UNIT_ELEMENT(#113986,-3.);
#60426=DERIVED_UNIT_ELEMENT(#60446,1.);
#60427=DERIVED_UNIT_ELEMENT(#113986,-3.);
#60428=DERIVED_UNIT_ELEMENT(#60446,1.);
#60429=DERIVED_UNIT_ELEMENT(#113986,-3.);
#60430=DERIVED_UNIT_ELEMENT(#60446,1.);
#60431=DERIVED_UNIT_ELEMENT(#113986,-3.);
#60432=DERIVED_UNIT_ELEMENT(#60446,1.);
#60433=DERIVED_UNIT_ELEMENT(#113986,-3.);
#60434=DERIVED_UNIT_ELEMENT(#60446,1.);
#60435=DERIVED_UNIT_ELEMENT(#113986,-3.);
#60436=DERIVED_UNIT_ELEMENT(#60446,1.);
#60437=DERIVED_UNIT_ELEMENT(#113986,-3.);
#60438=DERIVED_UNIT_ELEMENT(#60446,1.);
#60439=DERIVED_UNIT_ELEMENT(#113986,-3.);
#60440=DERIVED_UNIT_ELEMENT(#60446,1.);
#60441=DERIVED_UNIT_ELEMENT(#113986,-3.);
#60442=DERIVED_UNIT_ELEMENT(#60446,1.);
#60443=DERIVED_UNIT_ELEMENT(#113986,-3.);
#60444=DERIVED_UNIT_ELEMENT(#60446,1.);
#60445=DERIVED_UNIT_ELEMENT(#113986,-3.);
#60446=(
MASS_UNIT()
NAMED_UNIT(*)
SI_UNIT(.KILO.,.GRAM.)
);
#60447=DERIVED_UNIT((#60410,#60411));
#60448=DERIVED_UNIT((#60412,#60413));
#60449=DERIVED_UNIT((#60414,#60415));
#60450=DERIVED_UNIT((#60416,#60417));
#60451=DERIVED_UNIT((#60418,#60419));
#60452=DERIVED_UNIT((#60420,#60421));
#60453=DERIVED_UNIT((#60422,#60423));
#60454=DERIVED_UNIT((#60424,#60425));
#60455=DERIVED_UNIT((#60426,#60427));
#60456=DERIVED_UNIT((#60428,#60429));
#60457=DERIVED_UNIT((#60430,#60431));
#60458=DERIVED_UNIT((#60432,#60433));
#60459=DERIVED_UNIT((#60434,#60435));
#60460=DERIVED_UNIT((#60436,#60437));
#60461=DERIVED_UNIT((#60438,#60439));
#60462=DERIVED_UNIT((#60440,#60441));
#60463=DERIVED_UNIT((#60442,#60443));
#60464=DERIVED_UNIT((#60444,#60445));
#60465=MEASURE_REPRESENTATION_ITEM('density measure',
POSITIVE_RATIO_MEASURE(7850.),#60447);
#60466=MEASURE_REPRESENTATION_ITEM('density measure',
POSITIVE_RATIO_MEASURE(7850.),#60448);
#60467=MEASURE_REPRESENTATION_ITEM('density measure',
POSITIVE_RATIO_MEASURE(7850.),#60449);
#60468=MEASURE_REPRESENTATION_ITEM('density measure',
POSITIVE_RATIO_MEASURE(7850.),#60450);
#60469=MEASURE_REPRESENTATION_ITEM('density measure',
POSITIVE_RATIO_MEASURE(7850.),#60451);
#60470=MEASURE_REPRESENTATION_ITEM('density measure',
POSITIVE_RATIO_MEASURE(7850.),#60452);
#60471=MEASURE_REPRESENTATION_ITEM('density measure',
POSITIVE_RATIO_MEASURE(7850.),#60453);
#60472=MEASURE_REPRESENTATION_ITEM('density measure',
POSITIVE_RATIO_MEASURE(7850.),#60454);
#60473=MEASURE_REPRESENTATION_ITEM('density measure',
POSITIVE_RATIO_MEASURE(7850.),#60455);
#60474=MEASURE_REPRESENTATION_ITEM('density measure',
POSITIVE_RATIO_MEASURE(7850.),#60456);
#60475=MEASURE_REPRESENTATION_ITEM('density measure',
POSITIVE_RATIO_MEASURE(7850.),#60457);
#60476=MEASURE_REPRESENTATION_ITEM('density measure',
POSITIVE_RATIO_MEASURE(7850.),#60458);
#60477=MEASURE_REPRESENTATION_ITEM('density measure',
POSITIVE_RATIO_MEASURE(7850.),#60459);
#60478=MEASURE_REPRESENTATION_ITEM('density measure',
POSITIVE_RATIO_MEASURE(7850.),#60460);
#60479=MEASURE_REPRESENTATION_ITEM('density measure',
POSITIVE_RATIO_MEASURE(7850.),#60461);
#60480=MEASURE_REPRESENTATION_ITEM('density measure',
POSITIVE_RATIO_MEASURE(7850.),#60462);
#60481=MEASURE_REPRESENTATION_ITEM('density measure',
POSITIVE_RATIO_MEASURE(7850.),#60463);
#60482=MEASURE_REPRESENTATION_ITEM('density measure',
POSITIVE_RATIO_MEASURE(7850.),#60464);
#60483=PROPERTY_DEFINITION_REPRESENTATION(#60573,#60519);
#60484=PROPERTY_DEFINITION_REPRESENTATION(#60574,#60520);
#60485=PROPERTY_DEFINITION_REPRESENTATION(#60575,#60521);
#60486=PROPERTY_DEFINITION_REPRESENTATION(#60576,#60522);
#60487=PROPERTY_DEFINITION_REPRESENTATION(#60577,#60523);
#60488=PROPERTY_DEFINITION_REPRESENTATION(#60578,#60524);
#60489=PROPERTY_DEFINITION_REPRESENTATION(#60579,#60525);
#60490=PROPERTY_DEFINITION_REPRESENTATION(#60580,#60526);
#60491=PROPERTY_DEFINITION_REPRESENTATION(#60581,#60527);
#60492=PROPERTY_DEFINITION_REPRESENTATION(#60582,#60528);
#60493=PROPERTY_DEFINITION_REPRESENTATION(#60583,#60529);
#60494=PROPERTY_DEFINITION_REPRESENTATION(#60584,#60530);
#60495=PROPERTY_DEFINITION_REPRESENTATION(#60585,#60531);
#60496=PROPERTY_DEFINITION_REPRESENTATION(#60586,#60532);
#60497=PROPERTY_DEFINITION_REPRESENTATION(#60587,#60533);
#60498=PROPERTY_DEFINITION_REPRESENTATION(#60588,#60534);
#60499=PROPERTY_DEFINITION_REPRESENTATION(#60589,#60535);
#60500=PROPERTY_DEFINITION_REPRESENTATION(#60590,#60536);
#60501=PROPERTY_DEFINITION_REPRESENTATION(#60591,#60537);
#60502=PROPERTY_DEFINITION_REPRESENTATION(#60592,#60538);
#60503=PROPERTY_DEFINITION_REPRESENTATION(#60593,#60539);
#60504=PROPERTY_DEFINITION_REPRESENTATION(#60594,#60540);
#60505=PROPERTY_DEFINITION_REPRESENTATION(#60595,#60541);
#60506=PROPERTY_DEFINITION_REPRESENTATION(#60596,#60542);
#60507=PROPERTY_DEFINITION_REPRESENTATION(#60597,#60543);
#60508=PROPERTY_DEFINITION_REPRESENTATION(#60598,#60544);
#60509=PROPERTY_DEFINITION_REPRESENTATION(#60599,#60545);
#60510=PROPERTY_DEFINITION_REPRESENTATION(#60600,#60546);
#60511=PROPERTY_DEFINITION_REPRESENTATION(#60601,#60547);
#60512=PROPERTY_DEFINITION_REPRESENTATION(#60602,#60548);
#60513=PROPERTY_DEFINITION_REPRESENTATION(#60603,#60549);
#60514=PROPERTY_DEFINITION_REPRESENTATION(#60604,#60550);
#60515=PROPERTY_DEFINITION_REPRESENTATION(#60605,#60551);
#60516=PROPERTY_DEFINITION_REPRESENTATION(#60606,#60552);
#60517=PROPERTY_DEFINITION_REPRESENTATION(#60607,#60553);
#60518=PROPERTY_DEFINITION_REPRESENTATION(#60608,#60554);
#60519=REPRESENTATION('material name',(#60555),#113966);
#60520=REPRESENTATION('density',(#60465),#113966);
#60521=REPRESENTATION('material name',(#60556),#113967);
#60522=REPRESENTATION('density',(#60466),#113967);
#60523=REPRESENTATION('material name',(#60557),#113968);
#60524=REPRESENTATION('density',(#60467),#113968);
#60525=REPRESENTATION('material name',(#60558),#113969);
#60526=REPRESENTATION('density',(#60468),#113969);
#60527=REPRESENTATION('material name',(#60559),#113970);
#60528=REPRESENTATION('density',(#60469),#113970);
#60529=REPRESENTATION('material name',(#60560),#113971);
#60530=REPRESENTATION('density',(#60470),#113971);
#60531=REPRESENTATION('material name',(#60561),#113972);
#60532=REPRESENTATION('density',(#60471),#113972);
#60533=REPRESENTATION('material name',(#60562),#113973);
#60534=REPRESENTATION('density',(#60472),#113973);
#60535=REPRESENTATION('material name',(#60563),#113974);
#60536=REPRESENTATION('density',(#60473),#113974);
#60537=REPRESENTATION('material name',(#60564),#113975);
#60538=REPRESENTATION('density',(#60474),#113975);
#60539=REPRESENTATION('material name',(#60565),#113976);
#60540=REPRESENTATION('density',(#60475),#113976);
#60541=REPRESENTATION('material name',(#60566),#113977);
#60542=REPRESENTATION('density',(#60476),#113977);
#60543=REPRESENTATION('material name',(#60567),#113978);
#60544=REPRESENTATION('density',(#60477),#113978);
#60545=REPRESENTATION('material name',(#60568),#113979);
#60546=REPRESENTATION('density',(#60478),#113979);
#60547=REPRESENTATION('material name',(#60569),#113980);
#60548=REPRESENTATION('density',(#60479),#113980);
#60549=REPRESENTATION('material name',(#60570),#113981);
#60550=REPRESENTATION('density',(#60480),#113981);
#60551=REPRESENTATION('material name',(#60571),#113982);
#60552=REPRESENTATION('density',(#60481),#113982);
#60553=REPRESENTATION('material name',(#60572),#113983);
#60554=REPRESENTATION('density',(#60482),#113983);
#60555=DESCRIPTIVE_REPRESENTATION_ITEM('Steel','Steel');
#60556=DESCRIPTIVE_REPRESENTATION_ITEM('Steel','Steel');
#60557=DESCRIPTIVE_REPRESENTATION_ITEM('Steel','Steel');
#60558=DESCRIPTIVE_REPRESENTATION_ITEM('Steel','Steel');
#60559=DESCRIPTIVE_REPRESENTATION_ITEM('Steel','Steel');
#60560=DESCRIPTIVE_REPRESENTATION_ITEM('Steel','Steel');
#60561=DESCRIPTIVE_REPRESENTATION_ITEM('Steel','Steel');
#60562=DESCRIPTIVE_REPRESENTATION_ITEM('Steel','Steel');
#60563=DESCRIPTIVE_REPRESENTATION_ITEM('Steel','Steel');
#60564=DESCRIPTIVE_REPRESENTATION_ITEM('Steel','Steel');
#60565=DESCRIPTIVE_REPRESENTATION_ITEM('Steel','Steel');
#60566=DESCRIPTIVE_REPRESENTATION_ITEM('Steel','Steel');
#60567=DESCRIPTIVE_REPRESENTATION_ITEM('Steel','Steel');
#60568=DESCRIPTIVE_REPRESENTATION_ITEM('Steel','Steel');
#60569=DESCRIPTIVE_REPRESENTATION_ITEM('Steel','Steel');
#60570=DESCRIPTIVE_REPRESENTATION_ITEM('Steel','Steel');
#60571=DESCRIPTIVE_REPRESENTATION_ITEM('Steel','Steel');
#60572=DESCRIPTIVE_REPRESENTATION_ITEM('Steel','Steel');
#60573=PROPERTY_DEFINITION('material property','material name',#114072);
#60574=PROPERTY_DEFINITION('material property','density of part',#114072);
#60575=PROPERTY_DEFINITION('material property','material name',#114073);
#60576=PROPERTY_DEFINITION('material property','density of part',#114073);
#60577=PROPERTY_DEFINITION('material property','material name',#114074);
#60578=PROPERTY_DEFINITION('material property','density of part',#114074);
#60579=PROPERTY_DEFINITION('material property','material name',#114075);
#60580=PROPERTY_DEFINITION('material property','density of part',#114075);
#60581=PROPERTY_DEFINITION('material property','material name',#114076);
#60582=PROPERTY_DEFINITION('material property','density of part',#114076);
#60583=PROPERTY_DEFINITION('material property','material name',#114077);
#60584=PROPERTY_DEFINITION('material property','density of part',#114077);
#60585=PROPERTY_DEFINITION('material property','material name',#114078);
#60586=PROPERTY_DEFINITION('material property','density of part',#114078);
#60587=PROPERTY_DEFINITION('material property','material name',#114079);
#60588=PROPERTY_DEFINITION('material property','density of part',#114079);
#60589=PROPERTY_DEFINITION('material property','material name',#114080);
#60590=PROPERTY_DEFINITION('material property','density of part',#114080);
#60591=PROPERTY_DEFINITION('material property','material name',#114081);
#60592=PROPERTY_DEFINITION('material property','density of part',#114081);
#60593=PROPERTY_DEFINITION('material property','material name',#114082);
#60594=PROPERTY_DEFINITION('material property','density of part',#114082);
#60595=PROPERTY_DEFINITION('material property','material name',#114083);
#60596=PROPERTY_DEFINITION('material property','density of part',#114083);
#60597=PROPERTY_DEFINITION('material property','material name',#114084);
#60598=PROPERTY_DEFINITION('material property','density of part',#114084);
#60599=PROPERTY_DEFINITION('material property','material name',#114085);
#60600=PROPERTY_DEFINITION('material property','density of part',#114085);
#60601=PROPERTY_DEFINITION('material property','material name',#114086);
#60602=PROPERTY_DEFINITION('material property','density of part',#114086);
#60603=PROPERTY_DEFINITION('material property','material name',#114087);
#60604=PROPERTY_DEFINITION('material property','density of part',#114087);
#60605=PROPERTY_DEFINITION('material property','material name',#114088);
#60606=PROPERTY_DEFINITION('material property','density of part',#114088);
#60607=PROPERTY_DEFINITION('material property','material name',#114089);
#60608=PROPERTY_DEFINITION('material property','density of part',#114089);
#60609=AXIS2_PLACEMENT_3D('',#76144,#63776,#63777);
#60610=AXIS2_PLACEMENT_3D('',#76145,#63778,#63779);
#60611=AXIS2_PLACEMENT_3D('',#76446,#63800,#63801);
#60612=AXIS2_PLACEMENT_3D('',#76870,#63831,#63832);
#60613=AXIS2_PLACEMENT_3D('',#76888,#63836,#63837);
#60614=AXIS2_PLACEMENT_3D('',#76889,#63838,#63839);
#60615=AXIS2_PLACEMENT_3D('',#76890,#63840,#63841);
#60616=AXIS2_PLACEMENT_3D('',#77191,#63862,#63863);
#60617=AXIS2_PLACEMENT_3D('',#77687,#63897,#63898);
#60618=AXIS2_PLACEMENT_3D('',#77688,#63899,#63900);
#60619=AXIS2_PLACEMENT_3D('',#77689,#63901,#63902);
#60620=AXIS2_PLACEMENT_3D('',#77690,#63903,#63904);
#60621=AXIS2_PLACEMENT_3D('',#77991,#63925,#63926);
#60622=AXIS2_PLACEMENT_3D('',#78040,#63931,#63932);
#60623=AXIS2_PLACEMENT_3D('',#78091,#63939,#63940);
#60624=AXIS2_PLACEMENT_3D('',#78097,#63944,#63945);
#60625=AXIS2_PLACEMENT_3D('',#78103,#63949,#63950);
#60626=AXIS2_PLACEMENT_3D('',#78109,#63954,#63955);
#60627=AXIS2_PLACEMENT_3D('',#78112,#63958,#63959);
#60628=AXIS2_PLACEMENT_3D('',#78113,#63960,#63961);
#60629=AXIS2_PLACEMENT_3D('',#78414,#63982,#63983);
#60630=AXIS2_PLACEMENT_3D('',#78808,#64011,#64012);
#60631=AXIS2_PLACEMENT_3D('',#78826,#64016,#64017);
#60632=AXIS2_PLACEMENT_3D('',#78827,#64018,#64019);
#60633=AXIS2_PLACEMENT_3D('',#78828,#64020,#64021);
#60634=AXIS2_PLACEMENT_3D('',#79129,#64042,#64043);
#60635=AXIS2_PLACEMENT_3D('',#79223,#64051,#64052);
#60636=AXIS2_PLACEMENT_3D('',#79229,#64056,#64057);
#60637=AXIS2_PLACEMENT_3D('',#79235,#64061,#64062);
#60638=AXIS2_PLACEMENT_3D('',#79241,#64066,#64067);
#60639=AXIS2_PLACEMENT_3D('',#79247,#64071,#64072);
#60640=AXIS2_PLACEMENT_3D('',#79253,#64076,#64077);
#60641=AXIS2_PLACEMENT_3D('',#79379,#64089,#64090);
#60642=AXIS2_PLACEMENT_3D('',#79397,#64094,#64095);
#60643=AXIS2_PLACEMENT_3D('',#79398,#64096,#64097);
#60644=AXIS2_PLACEMENT_3D('',#79699,#64118,#64119);
#60645=AXIS2_PLACEMENT_3D('',#79700,#64120,#64121);
#60646=AXIS2_PLACEMENT_3D('',#79709,#64126,#64127);
#60647=AXIS2_PLACEMENT_3D('',#79715,#64131,#64132);
#60648=AXIS2_PLACEMENT_3D('',#79718,#64135,#64136);
#60649=AXIS2_PLACEMENT_3D('',#79727,#64141,#64142);
#60650=AXIS2_PLACEMENT_3D('',#79733,#64146,#64147);
#60651=AXIS2_PLACEMENT_3D('',#79739,#64151,#64152);
#60652=AXIS2_PLACEMENT_3D('',#79745,#64156,#64157);
#60653=AXIS2_PLACEMENT_3D('',#79751,#64161,#64162);
#60654=AXIS2_PLACEMENT_3D('',#79757,#64166,#64167);
#60655=AXIS2_PLACEMENT_3D('',#79763,#64171,#64172);
#60656=AXIS2_PLACEMENT_3D('',#79769,#64176,#64177);
#60657=AXIS2_PLACEMENT_3D('',#79775,#64181,#64182);
#60658=AXIS2_PLACEMENT_3D('',#79781,#64186,#64187);
#60659=AXIS2_PLACEMENT_3D('',#79784,#64190,#64191);
#60660=AXIS2_PLACEMENT_3D('',#79785,#64192,#64193);
#60661=AXIS2_PLACEMENT_3D('',#79786,#64194,#64195);
#60662=AXIS2_PLACEMENT_3D('',#80087,#64216,#64217);
#60663=AXIS2_PLACEMENT_3D('',#80271,#64231,#64232);
#60664=AXIS2_PLACEMENT_3D('',#80382,#64243,#64244);
#60665=AXIS2_PLACEMENT_3D('',#80493,#64255,#64256);
#60666=AXIS2_PLACEMENT_3D('',#80511,#64260,#64261);
#60667=AXIS2_PLACEMENT_3D('',#80512,#64262,#64263);
#60668=AXIS2_PLACEMENT_3D('',#80813,#64284,#64285);
#60669=AXIS2_PLACEMENT_3D('',#80952,#64296,#64297);
#60670=AXIS2_PLACEMENT_3D('',#81093,#64310,#64311);
#60671=AXIS2_PLACEMENT_3D('',#81099,#64315,#64316);
#60672=AXIS2_PLACEMENT_3D('',#81105,#64320,#64321);
#60673=AXIS2_PLACEMENT_3D('',#81108,#64324,#64325);
#60674=AXIS2_PLACEMENT_3D('',#81109,#64326,#64327);
#60675=AXIS2_PLACEMENT_3D('',#81410,#64348,#64349);
#60676=AXIS2_PLACEMENT_3D('',#81411,#64350,#64351);
#60677=AXIS2_PLACEMENT_3D('',#81450,#64358,#64359);
#60678=AXIS2_PLACEMENT_3D('',#81486,#64365,#64366);
#60679=AXIS2_PLACEMENT_3D('',#81492,#64370,#64371);
#60680=AXIS2_PLACEMENT_3D('',#81498,#64375,#64376);
#60681=AXIS2_PLACEMENT_3D('',#81501,#64379,#64380);
#60682=AXIS2_PLACEMENT_3D('',#81502,#64381,#64382);
#60683=AXIS2_PLACEMENT_3D('',#81803,#64403,#64404);
#60684=AXIS2_PLACEMENT_3D('',#81804,#64405,#64406);
#60685=AXIS2_PLACEMENT_3D('',#82105,#64427,#64428);
#60686=AXIS2_PLACEMENT_3D('',#82106,#64429,#64430);
#60687=AXIS2_PLACEMENT_3D('',#82145,#64437,#64438);
#60688=AXIS2_PLACEMENT_3D('',#82181,#64444,#64445);
#60689=AXIS2_PLACEMENT_3D('',#82187,#64449,#64450);
#60690=AXIS2_PLACEMENT_3D('',#82193,#64454,#64455);
#60691=AXIS2_PLACEMENT_3D('',#82196,#64458,#64459);
#60692=AXIS2_PLACEMENT_3D('',#82197,#64460,#64461);
#60693=AXIS2_PLACEMENT_3D('',#82498,#64482,#64483);
#60694=AXIS2_PLACEMENT_3D('',#82637,#64494,#64495);
#60695=AXIS2_PLACEMENT_3D('',#82778,#64508,#64509);
#60696=AXIS2_PLACEMENT_3D('',#82784,#64513,#64514);
#60697=AXIS2_PLACEMENT_3D('',#82790,#64518,#64519);
#60698=AXIS2_PLACEMENT_3D('',#82793,#64522,#64523);
#60699=AXIS2_PLACEMENT_3D('',#82794,#64524,#64525);
#60700=AXIS2_PLACEMENT_3D('',#83095,#64546,#64547);
#60701=AXIS2_PLACEMENT_3D('',#83279,#64561,#64562);
#60702=AXIS2_PLACEMENT_3D('',#83390,#64573,#64574);
#60703=AXIS2_PLACEMENT_3D('',#83501,#64585,#64586);
#60704=AXIS2_PLACEMENT_3D('',#83519,#64590,#64591);
#60705=AXIS2_PLACEMENT_3D('',#83520,#64592,#64593);
#60706=AXIS2_PLACEMENT_3D('',#83821,#64614,#64615);
#60707=AXIS2_PLACEMENT_3D('',#83822,#64616,#64617);
#60708=AXIS2_PLACEMENT_3D('',#83831,#64622,#64623);
#60709=AXIS2_PLACEMENT_3D('',#83837,#64627,#64628);
#60710=AXIS2_PLACEMENT_3D('',#83840,#64631,#64632);
#60711=AXIS2_PLACEMENT_3D('',#83849,#64637,#64638);
#60712=AXIS2_PLACEMENT_3D('',#83855,#64642,#64643);
#60713=AXIS2_PLACEMENT_3D('',#83861,#64647,#64648);
#60714=AXIS2_PLACEMENT_3D('',#83867,#64652,#64653);
#60715=AXIS2_PLACEMENT_3D('',#83873,#64657,#64658);
#60716=AXIS2_PLACEMENT_3D('',#83879,#64662,#64663);
#60717=AXIS2_PLACEMENT_3D('',#83885,#64667,#64668);
#60718=AXIS2_PLACEMENT_3D('',#83891,#64672,#64673);
#60719=AXIS2_PLACEMENT_3D('',#83897,#64677,#64678);
#60720=AXIS2_PLACEMENT_3D('',#83903,#64682,#64683);
#60721=AXIS2_PLACEMENT_3D('',#83906,#64686,#64687);
#60722=AXIS2_PLACEMENT_3D('',#83907,#64688,#64689);
#60723=AXIS2_PLACEMENT_3D('',#83908,#64690,#64691);
#60724=AXIS2_PLACEMENT_3D('',#84209,#64712,#64713);
#60725=AXIS2_PLACEMENT_3D('',#84303,#64721,#64722);
#60726=AXIS2_PLACEMENT_3D('',#84309,#64726,#64727);
#60727=AXIS2_PLACEMENT_3D('',#84315,#64731,#64732);
#60728=AXIS2_PLACEMENT_3D('',#84321,#64736,#64737);
#60729=AXIS2_PLACEMENT_3D('',#84327,#64741,#64742);
#60730=AXIS2_PLACEMENT_3D('',#84333,#64746,#64747);
#60731=AXIS2_PLACEMENT_3D('',#84459,#64759,#64760);
#60732=AXIS2_PLACEMENT_3D('',#84477,#64764,#64765);
#60733=AXIS2_PLACEMENT_3D('',#84478,#64766,#64767);
#60734=AXIS2_PLACEMENT_3D('',#84779,#64788,#64789);
#60735=AXIS2_PLACEMENT_3D('',#85173,#64817,#64818);
#60736=AXIS2_PLACEMENT_3D('',#85191,#64822,#64823);
#60737=AXIS2_PLACEMENT_3D('',#85192,#64824,#64825);
#60738=AXIS2_PLACEMENT_3D('',#85193,#64826,#64827);
#60739=AXIS2_PLACEMENT_3D('',#85494,#64848,#64849);
#60740=AXIS2_PLACEMENT_3D('',#85543,#64854,#64855);
#60741=AXIS2_PLACEMENT_3D('',#85594,#64862,#64863);
#60742=AXIS2_PLACEMENT_3D('',#85600,#64867,#64868);
#60743=AXIS2_PLACEMENT_3D('',#85606,#64872,#64873);
#60744=AXIS2_PLACEMENT_3D('',#85612,#64877,#64878);
#60745=AXIS2_PLACEMENT_3D('',#85615,#64881,#64882);
#60746=AXIS2_PLACEMENT_3D('',#85616,#64883,#64884);
#60747=AXIS2_PLACEMENT_3D('',#85917,#64905,#64906);
#60748=AXIS2_PLACEMENT_3D('',#86413,#64940,#64941);
#60749=AXIS2_PLACEMENT_3D('',#86414,#64942,#64943);
#60750=AXIS2_PLACEMENT_3D('',#86415,#64944,#64945);
#60751=AXIS2_PLACEMENT_3D('',#86416,#64946,#64947);
#60752=AXIS2_PLACEMENT_3D('',#86717,#64968,#64969);
#60753=AXIS2_PLACEMENT_3D('',#87141,#64999,#65000);
#60754=AXIS2_PLACEMENT_3D('',#87159,#65004,#65005);
#60755=AXIS2_PLACEMENT_3D('',#87160,#65006,#65007);
#60756=AXIS2_PLACEMENT_3D('',#87161,#65008,#65009);
#60757=AXIS2_PLACEMENT_3D('',#87162,#65010,#65011);
#60758=AXIS2_PLACEMENT_3D('',#87171,#65016,#65017);
#60759=AXIS2_PLACEMENT_3D('',#87177,#65021,#65022);
#60760=AXIS2_PLACEMENT_3D('',#87183,#65026,#65027);
#60761=AXIS2_PLACEMENT_3D('',#87186,#65030,#65031);
#60762=AXIS2_PLACEMENT_3D('',#87187,#65032,#65033);
#60763=AXIS2_PLACEMENT_3D('',#87196,#65038,#65039);
#60764=AXIS2_PLACEMENT_3D('',#87202,#65043,#65044);
#60765=AXIS2_PLACEMENT_3D('',#87208,#65048,#65049);
#60766=AXIS2_PLACEMENT_3D('',#87211,#65052,#65053);
#60767=AXIS2_PLACEMENT_3D('',#87212,#65054,#65055);
#60768=AXIS2_PLACEMENT_3D('',#87221,#65060,#65061);
#60769=AXIS2_PLACEMENT_3D('',#87227,#65065,#65066);
#60770=AXIS2_PLACEMENT_3D('',#87233,#65070,#65071);
#60771=AXIS2_PLACEMENT_3D('',#87236,#65074,#65075);
#60772=AXIS2_PLACEMENT_3D('',#87237,#65076,#65077);
#60773=AXIS2_PLACEMENT_3D('',#87246,#65082,#65083);
#60774=AXIS2_PLACEMENT_3D('',#87252,#65087,#65088);
#60775=AXIS2_PLACEMENT_3D('',#87258,#65092,#65093);
#60776=AXIS2_PLACEMENT_3D('',#87261,#65096,#65097);
#60777=AXIS2_PLACEMENT_3D('',#87262,#65098,#65099);
#60778=AXIS2_PLACEMENT_3D('',#87271,#65104,#65105);
#60779=AXIS2_PLACEMENT_3D('',#87277,#65109,#65110);
#60780=AXIS2_PLACEMENT_3D('',#87283,#65114,#65115);
#60781=AXIS2_PLACEMENT_3D('',#87286,#65118,#65119);
#60782=AXIS2_PLACEMENT_3D('',#87287,#65120,#65121);
#60783=AXIS2_PLACEMENT_3D('',#87296,#65126,#65127);
#60784=AXIS2_PLACEMENT_3D('',#87302,#65131,#65132);
#60785=AXIS2_PLACEMENT_3D('',#87308,#65136,#65137);
#60786=AXIS2_PLACEMENT_3D('',#87311,#65140,#65141);
#60787=AXIS2_PLACEMENT_3D('',#87312,#65142,#65143);
#60788=AXIS2_PLACEMENT_3D('',#87321,#65148,#65149);
#60789=AXIS2_PLACEMENT_3D('',#87327,#65153,#65154);
#60790=AXIS2_PLACEMENT_3D('',#87333,#65158,#65159);
#60791=AXIS2_PLACEMENT_3D('',#87336,#65162,#65163);
#60792=AXIS2_PLACEMENT_3D('',#87337,#65164,#65165);
#60793=AXIS2_PLACEMENT_3D('',#87346,#65170,#65171);
#60794=AXIS2_PLACEMENT_3D('',#87352,#65175,#65176);
#60795=AXIS2_PLACEMENT_3D('',#87358,#65180,#65181);
#60796=AXIS2_PLACEMENT_3D('',#87361,#65184,#65185);
#60797=AXIS2_PLACEMENT_3D('',#87362,#65186,#65187);
#60798=AXIS2_PLACEMENT_3D('',#87371,#65192,#65193);
#60799=AXIS2_PLACEMENT_3D('',#87377,#65197,#65198);
#60800=AXIS2_PLACEMENT_3D('',#87383,#65202,#65203);
#60801=AXIS2_PLACEMENT_3D('',#87386,#65206,#65207);
#60802=AXIS2_PLACEMENT_3D('',#87387,#65208,#65209);
#60803=AXIS2_PLACEMENT_3D('',#87396,#65214,#65215);
#60804=AXIS2_PLACEMENT_3D('',#87402,#65219,#65220);
#60805=AXIS2_PLACEMENT_3D('',#87408,#65224,#65225);
#60806=AXIS2_PLACEMENT_3D('',#87411,#65228,#65229);
#60807=AXIS2_PLACEMENT_3D('',#87412,#65230,#65231);
#60808=AXIS2_PLACEMENT_3D('',#87421,#65236,#65237);
#60809=AXIS2_PLACEMENT_3D('',#87427,#65241,#65242);
#60810=AXIS2_PLACEMENT_3D('',#87433,#65246,#65247);
#60811=AXIS2_PLACEMENT_3D('',#87436,#65250,#65251);
#60812=AXIS2_PLACEMENT_3D('',#87437,#65252,#65253);
#60813=AXIS2_PLACEMENT_3D('',#87446,#65258,#65259);
#60814=AXIS2_PLACEMENT_3D('',#87452,#65263,#65264);
#60815=AXIS2_PLACEMENT_3D('',#87458,#65268,#65269);
#60816=AXIS2_PLACEMENT_3D('',#87461,#65272,#65273);
#60817=AXIS2_PLACEMENT_3D('',#87462,#65274,#65275);
#60818=AXIS2_PLACEMENT_3D('',#87471,#65280,#65281);
#60819=AXIS2_PLACEMENT_3D('',#87477,#65285,#65286);
#60820=AXIS2_PLACEMENT_3D('',#87483,#65290,#65291);
#60821=AXIS2_PLACEMENT_3D('',#87486,#65294,#65295);
#60822=AXIS2_PLACEMENT_3D('',#87487,#65296,#65297);
#60823=AXIS2_PLACEMENT_3D('',#87496,#65302,#65303);
#60824=AXIS2_PLACEMENT_3D('',#87502,#65307,#65308);
#60825=AXIS2_PLACEMENT_3D('',#87508,#65312,#65313);
#60826=AXIS2_PLACEMENT_3D('',#87511,#65316,#65317);
#60827=AXIS2_PLACEMENT_3D('',#87512,#65318,#65319);
#60828=AXIS2_PLACEMENT_3D('',#87521,#65324,#65325);
#60829=AXIS2_PLACEMENT_3D('',#87527,#65329,#65330);
#60830=AXIS2_PLACEMENT_3D('',#87533,#65334,#65335);
#60831=AXIS2_PLACEMENT_3D('',#87536,#65338,#65339);
#60832=AXIS2_PLACEMENT_3D('',#87537,#65340,#65341);
#60833=AXIS2_PLACEMENT_3D('',#87546,#65346,#65347);
#60834=AXIS2_PLACEMENT_3D('',#87552,#65351,#65352);
#60835=AXIS2_PLACEMENT_3D('',#87558,#65356,#65357);
#60836=AXIS2_PLACEMENT_3D('',#87561,#65360,#65361);
#60837=AXIS2_PLACEMENT_3D('',#87562,#65362,#65363);
#60838=AXIS2_PLACEMENT_3D('',#87571,#65368,#65369);
#60839=AXIS2_PLACEMENT_3D('',#87577,#65373,#65374);
#60840=AXIS2_PLACEMENT_3D('',#87583,#65378,#65379);
#60841=AXIS2_PLACEMENT_3D('',#87586,#65382,#65383);
#60842=AXIS2_PLACEMENT_3D('',#87587,#65384,#65385);
#60843=AXIS2_PLACEMENT_3D('',#87596,#65390,#65391);
#60844=AXIS2_PLACEMENT_3D('',#87602,#65395,#65396);
#60845=AXIS2_PLACEMENT_3D('',#87608,#65400,#65401);
#60846=AXIS2_PLACEMENT_3D('',#87611,#65404,#65405);
#60847=AXIS2_PLACEMENT_3D('',#87612,#65406,#65407);
#60848=AXIS2_PLACEMENT_3D('',#87621,#65412,#65413);
#60849=AXIS2_PLACEMENT_3D('',#87627,#65417,#65418);
#60850=AXIS2_PLACEMENT_3D('',#87633,#65422,#65423);
#60851=AXIS2_PLACEMENT_3D('',#87636,#65426,#65427);
#60852=AXIS2_PLACEMENT_3D('',#87637,#65428,#65429);
#60853=AXIS2_PLACEMENT_3D('',#87646,#65434,#65435);
#60854=AXIS2_PLACEMENT_3D('',#87652,#65439,#65440);
#60855=AXIS2_PLACEMENT_3D('',#87658,#65444,#65445);
#60856=AXIS2_PLACEMENT_3D('',#87661,#65448,#65449);
#60857=AXIS2_PLACEMENT_3D('',#87662,#65450,#65451);
#60858=AXIS2_PLACEMENT_3D('',#87671,#65456,#65457);
#60859=AXIS2_PLACEMENT_3D('',#87677,#65461,#65462);
#60860=AXIS2_PLACEMENT_3D('',#87683,#65466,#65467);
#60861=AXIS2_PLACEMENT_3D('',#87686,#65470,#65471);
#60862=AXIS2_PLACEMENT_3D('',#87687,#65472,#65473);
#60863=AXIS2_PLACEMENT_3D('',#87696,#65478,#65479);
#60864=AXIS2_PLACEMENT_3D('',#87702,#65483,#65484);
#60865=AXIS2_PLACEMENT_3D('',#87708,#65488,#65489);
#60866=AXIS2_PLACEMENT_3D('',#87711,#65492,#65493);
#60867=AXIS2_PLACEMENT_3D('',#87712,#65494,#65495);
#60868=AXIS2_PLACEMENT_3D('',#87721,#65500,#65501);
#60869=AXIS2_PLACEMENT_3D('',#87727,#65505,#65506);
#60870=AXIS2_PLACEMENT_3D('',#87733,#65510,#65511);
#60871=AXIS2_PLACEMENT_3D('',#87736,#65514,#65515);
#60872=AXIS2_PLACEMENT_3D('',#87737,#65516,#65517);
#60873=AXIS2_PLACEMENT_3D('',#87746,#65522,#65523);
#60874=AXIS2_PLACEMENT_3D('',#87752,#65527,#65528);
#60875=AXIS2_PLACEMENT_3D('',#87758,#65532,#65533);
#60876=AXIS2_PLACEMENT_3D('',#87761,#65536,#65537);
#60877=AXIS2_PLACEMENT_3D('',#87762,#65538,#65539);
#60878=AXIS2_PLACEMENT_3D('',#87771,#65544,#65545);
#60879=AXIS2_PLACEMENT_3D('',#87777,#65549,#65550);
#60880=AXIS2_PLACEMENT_3D('',#87783,#65554,#65555);
#60881=AXIS2_PLACEMENT_3D('',#87786,#65558,#65559);
#60882=AXIS2_PLACEMENT_3D('',#87787,#65560,#65561);
#60883=AXIS2_PLACEMENT_3D('',#87796,#65566,#65567);
#60884=AXIS2_PLACEMENT_3D('',#87802,#65571,#65572);
#60885=AXIS2_PLACEMENT_3D('',#87808,#65576,#65577);
#60886=AXIS2_PLACEMENT_3D('',#87811,#65580,#65581);
#60887=AXIS2_PLACEMENT_3D('',#87812,#65582,#65583);
#60888=AXIS2_PLACEMENT_3D('',#87821,#65588,#65589);
#60889=AXIS2_PLACEMENT_3D('',#87827,#65593,#65594);
#60890=AXIS2_PLACEMENT_3D('',#87833,#65598,#65599);
#60891=AXIS2_PLACEMENT_3D('',#87836,#65602,#65603);
#60892=AXIS2_PLACEMENT_3D('',#87837,#65604,#65605);
#60893=AXIS2_PLACEMENT_3D('',#87846,#65610,#65611);
#60894=AXIS2_PLACEMENT_3D('',#87852,#65615,#65616);
#60895=AXIS2_PLACEMENT_3D('',#87858,#65620,#65621);
#60896=AXIS2_PLACEMENT_3D('',#87861,#65624,#65625);
#60897=AXIS2_PLACEMENT_3D('',#87862,#65626,#65627);
#60898=AXIS2_PLACEMENT_3D('',#87871,#65632,#65633);
#60899=AXIS2_PLACEMENT_3D('',#87877,#65637,#65638);
#60900=AXIS2_PLACEMENT_3D('',#87883,#65642,#65643);
#60901=AXIS2_PLACEMENT_3D('',#87886,#65646,#65647);
#60902=AXIS2_PLACEMENT_3D('',#87887,#65648,#65649);
#60903=AXIS2_PLACEMENT_3D('',#87896,#65654,#65655);
#60904=AXIS2_PLACEMENT_3D('',#87902,#65659,#65660);
#60905=AXIS2_PLACEMENT_3D('',#87908,#65664,#65665);
#60906=AXIS2_PLACEMENT_3D('',#87911,#65668,#65669);
#60907=AXIS2_PLACEMENT_3D('',#87912,#65670,#65671);
#60908=AXIS2_PLACEMENT_3D('',#87921,#65676,#65677);
#60909=AXIS2_PLACEMENT_3D('',#87927,#65681,#65682);
#60910=AXIS2_PLACEMENT_3D('',#87933,#65686,#65687);
#60911=AXIS2_PLACEMENT_3D('',#87936,#65690,#65691);
#60912=AXIS2_PLACEMENT_3D('',#87937,#65692,#65693);
#60913=AXIS2_PLACEMENT_3D('',#87946,#65698,#65699);
#60914=AXIS2_PLACEMENT_3D('',#87952,#65703,#65704);
#60915=AXIS2_PLACEMENT_3D('',#87958,#65708,#65709);
#60916=AXIS2_PLACEMENT_3D('',#87961,#65712,#65713);
#60917=AXIS2_PLACEMENT_3D('',#87962,#65714,#65715);
#60918=AXIS2_PLACEMENT_3D('',#87971,#65720,#65721);
#60919=AXIS2_PLACEMENT_3D('',#87977,#65725,#65726);
#60920=AXIS2_PLACEMENT_3D('',#87983,#65730,#65731);
#60921=AXIS2_PLACEMENT_3D('',#87986,#65734,#65735);
#60922=AXIS2_PLACEMENT_3D('',#87987,#65736,#65737);
#60923=AXIS2_PLACEMENT_3D('',#87996,#65742,#65743);
#60924=AXIS2_PLACEMENT_3D('',#88002,#65747,#65748);
#60925=AXIS2_PLACEMENT_3D('',#88008,#65752,#65753);
#60926=AXIS2_PLACEMENT_3D('',#88011,#65756,#65757);
#60927=AXIS2_PLACEMENT_3D('',#88012,#65758,#65759);
#60928=AXIS2_PLACEMENT_3D('',#88021,#65764,#65765);
#60929=AXIS2_PLACEMENT_3D('',#88027,#65769,#65770);
#60930=AXIS2_PLACEMENT_3D('',#88033,#65774,#65775);
#60931=AXIS2_PLACEMENT_3D('',#88036,#65778,#65779);
#60932=AXIS2_PLACEMENT_3D('',#88037,#65780,#65781);
#60933=AXIS2_PLACEMENT_3D('',#88046,#65786,#65787);
#60934=AXIS2_PLACEMENT_3D('',#88052,#65791,#65792);
#60935=AXIS2_PLACEMENT_3D('',#88058,#65796,#65797);
#60936=AXIS2_PLACEMENT_3D('',#88061,#65800,#65801);
#60937=AXIS2_PLACEMENT_3D('',#88062,#65802,#65803);
#60938=AXIS2_PLACEMENT_3D('',#88071,#65808,#65809);
#60939=AXIS2_PLACEMENT_3D('',#88077,#65813,#65814);
#60940=AXIS2_PLACEMENT_3D('',#88083,#65818,#65819);
#60941=AXIS2_PLACEMENT_3D('',#88086,#65822,#65823);
#60942=AXIS2_PLACEMENT_3D('',#88087,#65824,#65825);
#60943=AXIS2_PLACEMENT_3D('',#88096,#65830,#65831);
#60944=AXIS2_PLACEMENT_3D('',#88102,#65835,#65836);
#60945=AXIS2_PLACEMENT_3D('',#88108,#65840,#65841);
#60946=AXIS2_PLACEMENT_3D('',#88111,#65844,#65845);
#60947=AXIS2_PLACEMENT_3D('',#88112,#65846,#65847);
#60948=AXIS2_PLACEMENT_3D('',#88121,#65852,#65853);
#60949=AXIS2_PLACEMENT_3D('',#88127,#65857,#65858);
#60950=AXIS2_PLACEMENT_3D('',#88133,#65862,#65863);
#60951=AXIS2_PLACEMENT_3D('',#88136,#65866,#65867);
#60952=AXIS2_PLACEMENT_3D('',#88137,#65868,#65869);
#60953=AXIS2_PLACEMENT_3D('',#88146,#65874,#65875);
#60954=AXIS2_PLACEMENT_3D('',#88152,#65879,#65880);
#60955=AXIS2_PLACEMENT_3D('',#88158,#65884,#65885);
#60956=AXIS2_PLACEMENT_3D('',#88161,#65888,#65889);
#60957=AXIS2_PLACEMENT_3D('',#88162,#65890,#65891);
#60958=AXIS2_PLACEMENT_3D('',#88171,#65896,#65897);
#60959=AXIS2_PLACEMENT_3D('',#88177,#65901,#65902);
#60960=AXIS2_PLACEMENT_3D('',#88183,#65906,#65907);
#60961=AXIS2_PLACEMENT_3D('',#88186,#65910,#65911);
#60962=AXIS2_PLACEMENT_3D('',#88187,#65912,#65913);
#60963=AXIS2_PLACEMENT_3D('',#88196,#65918,#65919);
#60964=AXIS2_PLACEMENT_3D('',#88202,#65923,#65924);
#60965=AXIS2_PLACEMENT_3D('',#88208,#65928,#65929);
#60966=AXIS2_PLACEMENT_3D('',#88211,#65932,#65933);
#60967=AXIS2_PLACEMENT_3D('',#88212,#65934,#65935);
#60968=AXIS2_PLACEMENT_3D('',#88221,#65940,#65941);
#60969=AXIS2_PLACEMENT_3D('',#88227,#65945,#65946);
#60970=AXIS2_PLACEMENT_3D('',#88233,#65950,#65951);
#60971=AXIS2_PLACEMENT_3D('',#88236,#65954,#65955);
#60972=AXIS2_PLACEMENT_3D('',#88237,#65956,#65957);
#60973=AXIS2_PLACEMENT_3D('',#88246,#65962,#65963);
#60974=AXIS2_PLACEMENT_3D('',#88252,#65967,#65968);
#60975=AXIS2_PLACEMENT_3D('',#88258,#65972,#65973);
#60976=AXIS2_PLACEMENT_3D('',#88261,#65976,#65977);
#60977=AXIS2_PLACEMENT_3D('',#88262,#65978,#65979);
#60978=AXIS2_PLACEMENT_3D('',#88271,#65984,#65985);
#60979=AXIS2_PLACEMENT_3D('',#88277,#65989,#65990);
#60980=AXIS2_PLACEMENT_3D('',#88283,#65994,#65995);
#60981=AXIS2_PLACEMENT_3D('',#88286,#65998,#65999);
#60982=AXIS2_PLACEMENT_3D('',#88287,#66000,#66001);
#60983=AXIS2_PLACEMENT_3D('',#88296,#66006,#66007);
#60984=AXIS2_PLACEMENT_3D('',#88302,#66011,#66012);
#60985=AXIS2_PLACEMENT_3D('',#88308,#66016,#66017);
#60986=AXIS2_PLACEMENT_3D('',#88311,#66020,#66021);
#60987=AXIS2_PLACEMENT_3D('',#88312,#66022,#66023);
#60988=AXIS2_PLACEMENT_3D('',#88321,#66028,#66029);
#60989=AXIS2_PLACEMENT_3D('',#88327,#66033,#66034);
#60990=AXIS2_PLACEMENT_3D('',#88333,#66038,#66039);
#60991=AXIS2_PLACEMENT_3D('',#88336,#66042,#66043);
#60992=AXIS2_PLACEMENT_3D('',#88337,#66044,#66045);
#60993=AXIS2_PLACEMENT_3D('',#88346,#66050,#66051);
#60994=AXIS2_PLACEMENT_3D('',#88352,#66055,#66056);
#60995=AXIS2_PLACEMENT_3D('',#88358,#66060,#66061);
#60996=AXIS2_PLACEMENT_3D('',#88361,#66064,#66065);
#60997=AXIS2_PLACEMENT_3D('',#88362,#66066,#66067);
#60998=AXIS2_PLACEMENT_3D('',#88371,#66072,#66073);
#60999=AXIS2_PLACEMENT_3D('',#88377,#66077,#66078);
#61000=AXIS2_PLACEMENT_3D('',#88383,#66082,#66083);
#61001=AXIS2_PLACEMENT_3D('',#88386,#66086,#66087);
#61002=AXIS2_PLACEMENT_3D('',#88387,#66088,#66089);
#61003=AXIS2_PLACEMENT_3D('',#88396,#66094,#66095);
#61004=AXIS2_PLACEMENT_3D('',#88402,#66099,#66100);
#61005=AXIS2_PLACEMENT_3D('',#88408,#66104,#66105);
#61006=AXIS2_PLACEMENT_3D('',#88411,#66108,#66109);
#61007=AXIS2_PLACEMENT_3D('',#88412,#66110,#66111);
#61008=AXIS2_PLACEMENT_3D('',#88421,#66116,#66117);
#61009=AXIS2_PLACEMENT_3D('',#88427,#66121,#66122);
#61010=AXIS2_PLACEMENT_3D('',#88433,#66126,#66127);
#61011=AXIS2_PLACEMENT_3D('',#88436,#66130,#66131);
#61012=AXIS2_PLACEMENT_3D('',#88437,#66132,#66133);
#61013=AXIS2_PLACEMENT_3D('',#88446,#66138,#66139);
#61014=AXIS2_PLACEMENT_3D('',#88452,#66143,#66144);
#61015=AXIS2_PLACEMENT_3D('',#88458,#66148,#66149);
#61016=AXIS2_PLACEMENT_3D('',#88461,#66152,#66153);
#61017=AXIS2_PLACEMENT_3D('',#88462,#66154,#66155);
#61018=AXIS2_PLACEMENT_3D('',#88471,#66160,#66161);
#61019=AXIS2_PLACEMENT_3D('',#88477,#66165,#66166);
#61020=AXIS2_PLACEMENT_3D('',#88483,#66170,#66171);
#61021=AXIS2_PLACEMENT_3D('',#88486,#66174,#66175);
#61022=AXIS2_PLACEMENT_3D('',#88487,#66176,#66177);
#61023=AXIS2_PLACEMENT_3D('',#88496,#66182,#66183);
#61024=AXIS2_PLACEMENT_3D('',#88502,#66187,#66188);
#61025=AXIS2_PLACEMENT_3D('',#88508,#66192,#66193);
#61026=AXIS2_PLACEMENT_3D('',#88511,#66196,#66197);
#61027=AXIS2_PLACEMENT_3D('',#88512,#66198,#66199);
#61028=AXIS2_PLACEMENT_3D('',#88521,#66204,#66205);
#61029=AXIS2_PLACEMENT_3D('',#88527,#66209,#66210);
#61030=AXIS2_PLACEMENT_3D('',#88533,#66214,#66215);
#61031=AXIS2_PLACEMENT_3D('',#88536,#66218,#66219);
#61032=AXIS2_PLACEMENT_3D('',#88537,#66220,#66221);
#61033=AXIS2_PLACEMENT_3D('',#88546,#66226,#66227);
#61034=AXIS2_PLACEMENT_3D('',#88552,#66231,#66232);
#61035=AXIS2_PLACEMENT_3D('',#88558,#66236,#66237);
#61036=AXIS2_PLACEMENT_3D('',#88561,#66240,#66241);
#61037=AXIS2_PLACEMENT_3D('',#88562,#66242,#66243);
#61038=AXIS2_PLACEMENT_3D('',#88571,#66248,#66249);
#61039=AXIS2_PLACEMENT_3D('',#88577,#66253,#66254);
#61040=AXIS2_PLACEMENT_3D('',#88583,#66258,#66259);
#61041=AXIS2_PLACEMENT_3D('',#88586,#66262,#66263);
#61042=AXIS2_PLACEMENT_3D('',#88587,#66264,#66265);
#61043=AXIS2_PLACEMENT_3D('',#88596,#66270,#66271);
#61044=AXIS2_PLACEMENT_3D('',#88602,#66275,#66276);
#61045=AXIS2_PLACEMENT_3D('',#88608,#66280,#66281);
#61046=AXIS2_PLACEMENT_3D('',#88611,#66284,#66285);
#61047=AXIS2_PLACEMENT_3D('',#88612,#66286,#66287);
#61048=AXIS2_PLACEMENT_3D('',#88621,#66292,#66293);
#61049=AXIS2_PLACEMENT_3D('',#88627,#66297,#66298);
#61050=AXIS2_PLACEMENT_3D('',#88633,#66302,#66303);
#61051=AXIS2_PLACEMENT_3D('',#88636,#66306,#66307);
#61052=AXIS2_PLACEMENT_3D('',#88637,#66308,#66309);
#61053=AXIS2_PLACEMENT_3D('',#88646,#66314,#66315);
#61054=AXIS2_PLACEMENT_3D('',#88652,#66319,#66320);
#61055=AXIS2_PLACEMENT_3D('',#88658,#66324,#66325);
#61056=AXIS2_PLACEMENT_3D('',#88661,#66328,#66329);
#61057=AXIS2_PLACEMENT_3D('',#88662,#66330,#66331);
#61058=AXIS2_PLACEMENT_3D('',#88671,#66336,#66337);
#61059=AXIS2_PLACEMENT_3D('',#88677,#66341,#66342);
#61060=AXIS2_PLACEMENT_3D('',#88683,#66346,#66347);
#61061=AXIS2_PLACEMENT_3D('',#88686,#66350,#66351);
#61062=AXIS2_PLACEMENT_3D('',#88687,#66352,#66353);
#61063=AXIS2_PLACEMENT_3D('',#88696,#66358,#66359);
#61064=AXIS2_PLACEMENT_3D('',#88702,#66363,#66364);
#61065=AXIS2_PLACEMENT_3D('',#88708,#66368,#66369);
#61066=AXIS2_PLACEMENT_3D('',#88711,#66372,#66373);
#61067=AXIS2_PLACEMENT_3D('',#88712,#66374,#66375);
#61068=AXIS2_PLACEMENT_3D('',#88721,#66380,#66381);
#61069=AXIS2_PLACEMENT_3D('',#88727,#66385,#66386);
#61070=AXIS2_PLACEMENT_3D('',#88733,#66390,#66391);
#61071=AXIS2_PLACEMENT_3D('',#88736,#66394,#66395);
#61072=AXIS2_PLACEMENT_3D('',#88737,#66396,#66397);
#61073=AXIS2_PLACEMENT_3D('',#88746,#66402,#66403);
#61074=AXIS2_PLACEMENT_3D('',#88752,#66407,#66408);
#61075=AXIS2_PLACEMENT_3D('',#88758,#66412,#66413);
#61076=AXIS2_PLACEMENT_3D('',#88761,#66416,#66417);
#61077=AXIS2_PLACEMENT_3D('',#88762,#66418,#66419);
#61078=AXIS2_PLACEMENT_3D('',#88771,#66424,#66425);
#61079=AXIS2_PLACEMENT_3D('',#88777,#66429,#66430);
#61080=AXIS2_PLACEMENT_3D('',#88783,#66434,#66435);
#61081=AXIS2_PLACEMENT_3D('',#88786,#66438,#66439);
#61082=AXIS2_PLACEMENT_3D('',#88787,#66440,#66441);
#61083=AXIS2_PLACEMENT_3D('',#88796,#66446,#66447);
#61084=AXIS2_PLACEMENT_3D('',#88802,#66451,#66452);
#61085=AXIS2_PLACEMENT_3D('',#88808,#66456,#66457);
#61086=AXIS2_PLACEMENT_3D('',#88811,#66460,#66461);
#61087=AXIS2_PLACEMENT_3D('',#88812,#66462,#66463);
#61088=AXIS2_PLACEMENT_3D('',#88821,#66468,#66469);
#61089=AXIS2_PLACEMENT_3D('',#88827,#66473,#66474);
#61090=AXIS2_PLACEMENT_3D('',#88833,#66478,#66479);
#61091=AXIS2_PLACEMENT_3D('',#88836,#66482,#66483);
#61092=AXIS2_PLACEMENT_3D('',#88837,#66484,#66485);
#61093=AXIS2_PLACEMENT_3D('',#88846,#66490,#66491);
#61094=AXIS2_PLACEMENT_3D('',#88852,#66495,#66496);
#61095=AXIS2_PLACEMENT_3D('',#88858,#66500,#66501);
#61096=AXIS2_PLACEMENT_3D('',#88861,#66504,#66505);
#61097=AXIS2_PLACEMENT_3D('',#88862,#66506,#66507);
#61098=AXIS2_PLACEMENT_3D('',#88871,#66512,#66513);
#61099=AXIS2_PLACEMENT_3D('',#88877,#66517,#66518);
#61100=AXIS2_PLACEMENT_3D('',#88883,#66522,#66523);
#61101=AXIS2_PLACEMENT_3D('',#88886,#66526,#66527);
#61102=AXIS2_PLACEMENT_3D('',#88887,#66528,#66529);
#61103=AXIS2_PLACEMENT_3D('',#88896,#66534,#66535);
#61104=AXIS2_PLACEMENT_3D('',#88902,#66539,#66540);
#61105=AXIS2_PLACEMENT_3D('',#88908,#66544,#66545);
#61106=AXIS2_PLACEMENT_3D('',#88911,#66548,#66549);
#61107=AXIS2_PLACEMENT_3D('',#88912,#66550,#66551);
#61108=AXIS2_PLACEMENT_3D('',#88921,#66556,#66557);
#61109=AXIS2_PLACEMENT_3D('',#88927,#66561,#66562);
#61110=AXIS2_PLACEMENT_3D('',#88933,#66566,#66567);
#61111=AXIS2_PLACEMENT_3D('',#88936,#66570,#66571);
#61112=AXIS2_PLACEMENT_3D('',#88937,#66572,#66573);
#61113=AXIS2_PLACEMENT_3D('',#88946,#66578,#66579);
#61114=AXIS2_PLACEMENT_3D('',#88952,#66583,#66584);
#61115=AXIS2_PLACEMENT_3D('',#88958,#66588,#66589);
#61116=AXIS2_PLACEMENT_3D('',#88961,#66592,#66593);
#61117=AXIS2_PLACEMENT_3D('',#88962,#66594,#66595);
#61118=AXIS2_PLACEMENT_3D('',#88971,#66600,#66601);
#61119=AXIS2_PLACEMENT_3D('',#88977,#66605,#66606);
#61120=AXIS2_PLACEMENT_3D('',#88983,#66610,#66611);
#61121=AXIS2_PLACEMENT_3D('',#88986,#66614,#66615);
#61122=AXIS2_PLACEMENT_3D('',#88987,#66616,#66617);
#61123=AXIS2_PLACEMENT_3D('',#88996,#66622,#66623);
#61124=AXIS2_PLACEMENT_3D('',#89002,#66627,#66628);
#61125=AXIS2_PLACEMENT_3D('',#89008,#66632,#66633);
#61126=AXIS2_PLACEMENT_3D('',#89011,#66636,#66637);
#61127=AXIS2_PLACEMENT_3D('',#89012,#66638,#66639);
#61128=AXIS2_PLACEMENT_3D('',#89021,#66644,#66645);
#61129=AXIS2_PLACEMENT_3D('',#89027,#66649,#66650);
#61130=AXIS2_PLACEMENT_3D('',#89033,#66654,#66655);
#61131=AXIS2_PLACEMENT_3D('',#89036,#66658,#66659);
#61132=AXIS2_PLACEMENT_3D('',#89037,#66660,#66661);
#61133=AXIS2_PLACEMENT_3D('',#89046,#66666,#66667);
#61134=AXIS2_PLACEMENT_3D('',#89052,#66671,#66672);
#61135=AXIS2_PLACEMENT_3D('',#89058,#66676,#66677);
#61136=AXIS2_PLACEMENT_3D('',#89061,#66680,#66681);
#61137=AXIS2_PLACEMENT_3D('',#89062,#66682,#66683);
#61138=AXIS2_PLACEMENT_3D('',#89071,#66688,#66689);
#61139=AXIS2_PLACEMENT_3D('',#89077,#66693,#66694);
#61140=AXIS2_PLACEMENT_3D('',#89083,#66698,#66699);
#61141=AXIS2_PLACEMENT_3D('',#89086,#66702,#66703);
#61142=AXIS2_PLACEMENT_3D('',#89087,#66704,#66705);
#61143=AXIS2_PLACEMENT_3D('',#89096,#66710,#66711);
#61144=AXIS2_PLACEMENT_3D('',#89102,#66715,#66716);
#61145=AXIS2_PLACEMENT_3D('',#89108,#66720,#66721);
#61146=AXIS2_PLACEMENT_3D('',#89111,#66724,#66725);
#61147=AXIS2_PLACEMENT_3D('',#89112,#66726,#66727);
#61148=AXIS2_PLACEMENT_3D('',#89121,#66732,#66733);
#61149=AXIS2_PLACEMENT_3D('',#89127,#66737,#66738);
#61150=AXIS2_PLACEMENT_3D('',#89133,#66742,#66743);
#61151=AXIS2_PLACEMENT_3D('',#89136,#66746,#66747);
#61152=AXIS2_PLACEMENT_3D('',#89137,#66748,#66749);
#61153=AXIS2_PLACEMENT_3D('',#89146,#66754,#66755);
#61154=AXIS2_PLACEMENT_3D('',#89152,#66759,#66760);
#61155=AXIS2_PLACEMENT_3D('',#89158,#66764,#66765);
#61156=AXIS2_PLACEMENT_3D('',#89161,#66768,#66769);
#61157=AXIS2_PLACEMENT_3D('',#89162,#66770,#66771);
#61158=AXIS2_PLACEMENT_3D('',#89171,#66776,#66777);
#61159=AXIS2_PLACEMENT_3D('',#89177,#66781,#66782);
#61160=AXIS2_PLACEMENT_3D('',#89183,#66786,#66787);
#61161=AXIS2_PLACEMENT_3D('',#89186,#66790,#66791);
#61162=AXIS2_PLACEMENT_3D('',#89187,#66792,#66793);
#61163=AXIS2_PLACEMENT_3D('',#89196,#66798,#66799);
#61164=AXIS2_PLACEMENT_3D('',#89202,#66803,#66804);
#61165=AXIS2_PLACEMENT_3D('',#89208,#66808,#66809);
#61166=AXIS2_PLACEMENT_3D('',#89211,#66812,#66813);
#61167=AXIS2_PLACEMENT_3D('',#89212,#66814,#66815);
#61168=AXIS2_PLACEMENT_3D('',#89221,#66820,#66821);
#61169=AXIS2_PLACEMENT_3D('',#89227,#66825,#66826);
#61170=AXIS2_PLACEMENT_3D('',#89233,#66830,#66831);
#61171=AXIS2_PLACEMENT_3D('',#89236,#66834,#66835);
#61172=AXIS2_PLACEMENT_3D('',#89237,#66836,#66837);
#61173=AXIS2_PLACEMENT_3D('',#89246,#66842,#66843);
#61174=AXIS2_PLACEMENT_3D('',#89252,#66847,#66848);
#61175=AXIS2_PLACEMENT_3D('',#89258,#66852,#66853);
#61176=AXIS2_PLACEMENT_3D('',#89261,#66856,#66857);
#61177=AXIS2_PLACEMENT_3D('',#89262,#66858,#66859);
#61178=AXIS2_PLACEMENT_3D('',#89271,#66864,#66865);
#61179=AXIS2_PLACEMENT_3D('',#89277,#66869,#66870);
#61180=AXIS2_PLACEMENT_3D('',#89283,#66874,#66875);
#61181=AXIS2_PLACEMENT_3D('',#89286,#66878,#66879);
#61182=AXIS2_PLACEMENT_3D('',#89287,#66880,#66881);
#61183=AXIS2_PLACEMENT_3D('',#89296,#66886,#66887);
#61184=AXIS2_PLACEMENT_3D('',#89302,#66891,#66892);
#61185=AXIS2_PLACEMENT_3D('',#89308,#66896,#66897);
#61186=AXIS2_PLACEMENT_3D('',#89311,#66900,#66901);
#61187=AXIS2_PLACEMENT_3D('',#89312,#66902,#66903);
#61188=AXIS2_PLACEMENT_3D('',#89321,#66908,#66909);
#61189=AXIS2_PLACEMENT_3D('',#89327,#66913,#66914);
#61190=AXIS2_PLACEMENT_3D('',#89333,#66918,#66919);
#61191=AXIS2_PLACEMENT_3D('',#89336,#66922,#66923);
#61192=AXIS2_PLACEMENT_3D('',#89337,#66924,#66925);
#61193=AXIS2_PLACEMENT_3D('',#89346,#66930,#66931);
#61194=AXIS2_PLACEMENT_3D('',#89352,#66935,#66936);
#61195=AXIS2_PLACEMENT_3D('',#89358,#66940,#66941);
#61196=AXIS2_PLACEMENT_3D('',#89361,#66944,#66945);
#61197=AXIS2_PLACEMENT_3D('',#89362,#66946,#66947);
#61198=AXIS2_PLACEMENT_3D('',#89371,#66952,#66953);
#61199=AXIS2_PLACEMENT_3D('',#89377,#66957,#66958);
#61200=AXIS2_PLACEMENT_3D('',#89383,#66962,#66963);
#61201=AXIS2_PLACEMENT_3D('',#89386,#66966,#66967);
#61202=AXIS2_PLACEMENT_3D('',#89387,#66968,#66969);
#61203=AXIS2_PLACEMENT_3D('',#89396,#66974,#66975);
#61204=AXIS2_PLACEMENT_3D('',#89402,#66979,#66980);
#61205=AXIS2_PLACEMENT_3D('',#89408,#66984,#66985);
#61206=AXIS2_PLACEMENT_3D('',#89411,#66988,#66989);
#61207=AXIS2_PLACEMENT_3D('',#89412,#66990,#66991);
#61208=AXIS2_PLACEMENT_3D('',#89421,#66996,#66997);
#61209=AXIS2_PLACEMENT_3D('',#89427,#67001,#67002);
#61210=AXIS2_PLACEMENT_3D('',#89433,#67006,#67007);
#61211=AXIS2_PLACEMENT_3D('',#89436,#67010,#67011);
#61212=AXIS2_PLACEMENT_3D('',#89437,#67012,#67013);
#61213=AXIS2_PLACEMENT_3D('',#89446,#67018,#67019);
#61214=AXIS2_PLACEMENT_3D('',#89452,#67023,#67024);
#61215=AXIS2_PLACEMENT_3D('',#89458,#67028,#67029);
#61216=AXIS2_PLACEMENT_3D('',#89461,#67032,#67033);
#61217=AXIS2_PLACEMENT_3D('',#89462,#67034,#67035);
#61218=AXIS2_PLACEMENT_3D('',#89471,#67040,#67041);
#61219=AXIS2_PLACEMENT_3D('',#89477,#67045,#67046);
#61220=AXIS2_PLACEMENT_3D('',#89483,#67050,#67051);
#61221=AXIS2_PLACEMENT_3D('',#89486,#67054,#67055);
#61222=AXIS2_PLACEMENT_3D('',#89487,#67056,#67057);
#61223=AXIS2_PLACEMENT_3D('',#89496,#67062,#67063);
#61224=AXIS2_PLACEMENT_3D('',#89502,#67067,#67068);
#61225=AXIS2_PLACEMENT_3D('',#89508,#67072,#67073);
#61226=AXIS2_PLACEMENT_3D('',#89511,#67076,#67077);
#61227=AXIS2_PLACEMENT_3D('',#89512,#67078,#67079);
#61228=AXIS2_PLACEMENT_3D('',#89521,#67084,#67085);
#61229=AXIS2_PLACEMENT_3D('',#89527,#67089,#67090);
#61230=AXIS2_PLACEMENT_3D('',#89533,#67094,#67095);
#61231=AXIS2_PLACEMENT_3D('',#89536,#67098,#67099);
#61232=AXIS2_PLACEMENT_3D('',#89537,#67100,#67101);
#61233=AXIS2_PLACEMENT_3D('',#89546,#67106,#67107);
#61234=AXIS2_PLACEMENT_3D('',#89552,#67111,#67112);
#61235=AXIS2_PLACEMENT_3D('',#89558,#67116,#67117);
#61236=AXIS2_PLACEMENT_3D('',#89561,#67120,#67121);
#61237=AXIS2_PLACEMENT_3D('',#89562,#67122,#67123);
#61238=AXIS2_PLACEMENT_3D('',#89571,#67128,#67129);
#61239=AXIS2_PLACEMENT_3D('',#89577,#67133,#67134);
#61240=AXIS2_PLACEMENT_3D('',#89583,#67138,#67139);
#61241=AXIS2_PLACEMENT_3D('',#89586,#67142,#67143);
#61242=AXIS2_PLACEMENT_3D('',#89587,#67144,#67145);
#61243=AXIS2_PLACEMENT_3D('',#89596,#67150,#67151);
#61244=AXIS2_PLACEMENT_3D('',#89602,#67155,#67156);
#61245=AXIS2_PLACEMENT_3D('',#89608,#67160,#67161);
#61246=AXIS2_PLACEMENT_3D('',#89611,#67164,#67165);
#61247=AXIS2_PLACEMENT_3D('',#89612,#67166,#67167);
#61248=AXIS2_PLACEMENT_3D('',#89621,#67172,#67173);
#61249=AXIS2_PLACEMENT_3D('',#89627,#67177,#67178);
#61250=AXIS2_PLACEMENT_3D('',#89633,#67182,#67183);
#61251=AXIS2_PLACEMENT_3D('',#89636,#67186,#67187);
#61252=AXIS2_PLACEMENT_3D('',#89637,#67188,#67189);
#61253=AXIS2_PLACEMENT_3D('',#89646,#67194,#67195);
#61254=AXIS2_PLACEMENT_3D('',#89652,#67199,#67200);
#61255=AXIS2_PLACEMENT_3D('',#89658,#67204,#67205);
#61256=AXIS2_PLACEMENT_3D('',#89661,#67208,#67209);
#61257=AXIS2_PLACEMENT_3D('',#89662,#67210,#67211);
#61258=AXIS2_PLACEMENT_3D('',#89671,#67216,#67217);
#61259=AXIS2_PLACEMENT_3D('',#89677,#67221,#67222);
#61260=AXIS2_PLACEMENT_3D('',#89683,#67226,#67227);
#61261=AXIS2_PLACEMENT_3D('',#89686,#67230,#67231);
#61262=AXIS2_PLACEMENT_3D('',#89687,#67232,#67233);
#61263=AXIS2_PLACEMENT_3D('',#89696,#67238,#67239);
#61264=AXIS2_PLACEMENT_3D('',#89702,#67243,#67244);
#61265=AXIS2_PLACEMENT_3D('',#89708,#67248,#67249);
#61266=AXIS2_PLACEMENT_3D('',#89711,#67252,#67253);
#61267=AXIS2_PLACEMENT_3D('',#89712,#67254,#67255);
#61268=AXIS2_PLACEMENT_3D('',#89721,#67260,#67261);
#61269=AXIS2_PLACEMENT_3D('',#89727,#67265,#67266);
#61270=AXIS2_PLACEMENT_3D('',#89733,#67270,#67271);
#61271=AXIS2_PLACEMENT_3D('',#89736,#67274,#67275);
#61272=AXIS2_PLACEMENT_3D('',#89737,#67276,#67277);
#61273=AXIS2_PLACEMENT_3D('',#89746,#67282,#67283);
#61274=AXIS2_PLACEMENT_3D('',#89752,#67287,#67288);
#61275=AXIS2_PLACEMENT_3D('',#89758,#67292,#67293);
#61276=AXIS2_PLACEMENT_3D('',#89761,#67296,#67297);
#61277=AXIS2_PLACEMENT_3D('',#89762,#67298,#67299);
#61278=AXIS2_PLACEMENT_3D('',#89771,#67304,#67305);
#61279=AXIS2_PLACEMENT_3D('',#89777,#67309,#67310);
#61280=AXIS2_PLACEMENT_3D('',#89783,#67314,#67315);
#61281=AXIS2_PLACEMENT_3D('',#89786,#67318,#67319);
#61282=AXIS2_PLACEMENT_3D('',#89787,#67320,#67321);
#61283=AXIS2_PLACEMENT_3D('',#89796,#67326,#67327);
#61284=AXIS2_PLACEMENT_3D('',#89802,#67331,#67332);
#61285=AXIS2_PLACEMENT_3D('',#89808,#67336,#67337);
#61286=AXIS2_PLACEMENT_3D('',#89811,#67340,#67341);
#61287=AXIS2_PLACEMENT_3D('',#89812,#67342,#67343);
#61288=AXIS2_PLACEMENT_3D('',#89821,#67348,#67349);
#61289=AXIS2_PLACEMENT_3D('',#89827,#67353,#67354);
#61290=AXIS2_PLACEMENT_3D('',#89833,#67358,#67359);
#61291=AXIS2_PLACEMENT_3D('',#89836,#67362,#67363);
#61292=AXIS2_PLACEMENT_3D('',#89837,#67364,#67365);
#61293=AXIS2_PLACEMENT_3D('',#89846,#67370,#67371);
#61294=AXIS2_PLACEMENT_3D('',#89852,#67375,#67376);
#61295=AXIS2_PLACEMENT_3D('',#89858,#67380,#67381);
#61296=AXIS2_PLACEMENT_3D('',#89861,#67384,#67385);
#61297=AXIS2_PLACEMENT_3D('',#89862,#67386,#67387);
#61298=AXIS2_PLACEMENT_3D('',#89871,#67392,#67393);
#61299=AXIS2_PLACEMENT_3D('',#89877,#67397,#67398);
#61300=AXIS2_PLACEMENT_3D('',#89883,#67402,#67403);
#61301=AXIS2_PLACEMENT_3D('',#89886,#67406,#67407);
#61302=AXIS2_PLACEMENT_3D('',#89887,#67408,#67409);
#61303=AXIS2_PLACEMENT_3D('',#89896,#67414,#67415);
#61304=AXIS2_PLACEMENT_3D('',#89902,#67419,#67420);
#61305=AXIS2_PLACEMENT_3D('',#89908,#67424,#67425);
#61306=AXIS2_PLACEMENT_3D('',#89911,#67428,#67429);
#61307=AXIS2_PLACEMENT_3D('',#89912,#67430,#67431);
#61308=AXIS2_PLACEMENT_3D('',#89921,#67436,#67437);
#61309=AXIS2_PLACEMENT_3D('',#89927,#67441,#67442);
#61310=AXIS2_PLACEMENT_3D('',#89933,#67446,#67447);
#61311=AXIS2_PLACEMENT_3D('',#89936,#67450,#67451);
#61312=AXIS2_PLACEMENT_3D('',#89937,#67452,#67453);
#61313=AXIS2_PLACEMENT_3D('',#89946,#67458,#67459);
#61314=AXIS2_PLACEMENT_3D('',#89952,#67463,#67464);
#61315=AXIS2_PLACEMENT_3D('',#89958,#67468,#67469);
#61316=AXIS2_PLACEMENT_3D('',#89961,#67472,#67473);
#61317=AXIS2_PLACEMENT_3D('',#89962,#67474,#67475);
#61318=AXIS2_PLACEMENT_3D('',#89971,#67480,#67481);
#61319=AXIS2_PLACEMENT_3D('',#89977,#67485,#67486);
#61320=AXIS2_PLACEMENT_3D('',#89983,#67490,#67491);
#61321=AXIS2_PLACEMENT_3D('',#89986,#67494,#67495);
#61322=AXIS2_PLACEMENT_3D('',#89987,#67496,#67497);
#61323=AXIS2_PLACEMENT_3D('',#89996,#67502,#67503);
#61324=AXIS2_PLACEMENT_3D('',#90002,#67507,#67508);
#61325=AXIS2_PLACEMENT_3D('',#90008,#67512,#67513);
#61326=AXIS2_PLACEMENT_3D('',#90011,#67516,#67517);
#61327=AXIS2_PLACEMENT_3D('',#90012,#67518,#67519);
#61328=AXIS2_PLACEMENT_3D('',#90021,#67524,#67525);
#61329=AXIS2_PLACEMENT_3D('',#90027,#67529,#67530);
#61330=AXIS2_PLACEMENT_3D('',#90033,#67534,#67535);
#61331=AXIS2_PLACEMENT_3D('',#90036,#67538,#67539);
#61332=AXIS2_PLACEMENT_3D('',#90037,#67540,#67541);
#61333=AXIS2_PLACEMENT_3D('',#90046,#67546,#67547);
#61334=AXIS2_PLACEMENT_3D('',#90052,#67551,#67552);
#61335=AXIS2_PLACEMENT_3D('',#90058,#67556,#67557);
#61336=AXIS2_PLACEMENT_3D('',#90061,#67560,#67561);
#61337=AXIS2_PLACEMENT_3D('',#90062,#67562,#67563);
#61338=AXIS2_PLACEMENT_3D('',#90071,#67568,#67569);
#61339=AXIS2_PLACEMENT_3D('',#90077,#67573,#67574);
#61340=AXIS2_PLACEMENT_3D('',#90083,#67578,#67579);
#61341=AXIS2_PLACEMENT_3D('',#90086,#67582,#67583);
#61342=AXIS2_PLACEMENT_3D('',#90087,#67584,#67585);
#61343=AXIS2_PLACEMENT_3D('',#90096,#67590,#67591);
#61344=AXIS2_PLACEMENT_3D('',#90102,#67595,#67596);
#61345=AXIS2_PLACEMENT_3D('',#90108,#67600,#67601);
#61346=AXIS2_PLACEMENT_3D('',#90111,#67604,#67605);
#61347=AXIS2_PLACEMENT_3D('',#90112,#67606,#67607);
#61348=AXIS2_PLACEMENT_3D('',#90121,#67612,#67613);
#61349=AXIS2_PLACEMENT_3D('',#90127,#67617,#67618);
#61350=AXIS2_PLACEMENT_3D('',#90133,#67622,#67623);
#61351=AXIS2_PLACEMENT_3D('',#90136,#67626,#67627);
#61352=AXIS2_PLACEMENT_3D('',#90137,#67628,#67629);
#61353=AXIS2_PLACEMENT_3D('',#90146,#67634,#67635);
#61354=AXIS2_PLACEMENT_3D('',#90152,#67639,#67640);
#61355=AXIS2_PLACEMENT_3D('',#90158,#67644,#67645);
#61356=AXIS2_PLACEMENT_3D('',#90161,#67648,#67649);
#61357=AXIS2_PLACEMENT_3D('',#90162,#67650,#67651);
#61358=AXIS2_PLACEMENT_3D('',#90171,#67656,#67657);
#61359=AXIS2_PLACEMENT_3D('',#90177,#67661,#67662);
#61360=AXIS2_PLACEMENT_3D('',#90183,#67666,#67667);
#61361=AXIS2_PLACEMENT_3D('',#90186,#67670,#67671);
#61362=AXIS2_PLACEMENT_3D('',#90187,#67672,#67673);
#61363=AXIS2_PLACEMENT_3D('',#90196,#67678,#67679);
#61364=AXIS2_PLACEMENT_3D('',#90202,#67683,#67684);
#61365=AXIS2_PLACEMENT_3D('',#90208,#67688,#67689);
#61366=AXIS2_PLACEMENT_3D('',#90211,#67692,#67693);
#61367=AXIS2_PLACEMENT_3D('',#90212,#67694,#67695);
#61368=AXIS2_PLACEMENT_3D('',#90221,#67700,#67701);
#61369=AXIS2_PLACEMENT_3D('',#90227,#67705,#67706);
#61370=AXIS2_PLACEMENT_3D('',#90233,#67710,#67711);
#61371=AXIS2_PLACEMENT_3D('',#90236,#67714,#67715);
#61372=AXIS2_PLACEMENT_3D('',#90237,#67716,#67717);
#61373=AXIS2_PLACEMENT_3D('',#90246,#67722,#67723);
#61374=AXIS2_PLACEMENT_3D('',#90252,#67727,#67728);
#61375=AXIS2_PLACEMENT_3D('',#90258,#67732,#67733);
#61376=AXIS2_PLACEMENT_3D('',#90261,#67736,#67737);
#61377=AXIS2_PLACEMENT_3D('',#90262,#67738,#67739);
#61378=AXIS2_PLACEMENT_3D('',#90271,#67744,#67745);
#61379=AXIS2_PLACEMENT_3D('',#90277,#67749,#67750);
#61380=AXIS2_PLACEMENT_3D('',#90283,#67754,#67755);
#61381=AXIS2_PLACEMENT_3D('',#90286,#67758,#67759);
#61382=AXIS2_PLACEMENT_3D('',#90287,#67760,#67761);
#61383=AXIS2_PLACEMENT_3D('',#90296,#67766,#67767);
#61384=AXIS2_PLACEMENT_3D('',#90302,#67771,#67772);
#61385=AXIS2_PLACEMENT_3D('',#90308,#67776,#67777);
#61386=AXIS2_PLACEMENT_3D('',#90311,#67780,#67781);
#61387=AXIS2_PLACEMENT_3D('',#90312,#67782,#67783);
#61388=AXIS2_PLACEMENT_3D('',#90321,#67788,#67789);
#61389=AXIS2_PLACEMENT_3D('',#90327,#67793,#67794);
#61390=AXIS2_PLACEMENT_3D('',#90333,#67798,#67799);
#61391=AXIS2_PLACEMENT_3D('',#90336,#67802,#67803);
#61392=AXIS2_PLACEMENT_3D('',#90337,#67804,#67805);
#61393=AXIS2_PLACEMENT_3D('',#90346,#67810,#67811);
#61394=AXIS2_PLACEMENT_3D('',#90352,#67815,#67816);
#61395=AXIS2_PLACEMENT_3D('',#90358,#67820,#67821);
#61396=AXIS2_PLACEMENT_3D('',#90361,#67824,#67825);
#61397=AXIS2_PLACEMENT_3D('',#90362,#67826,#67827);
#61398=AXIS2_PLACEMENT_3D('',#90371,#67832,#67833);
#61399=AXIS2_PLACEMENT_3D('',#90377,#67837,#67838);
#61400=AXIS2_PLACEMENT_3D('',#90383,#67842,#67843);
#61401=AXIS2_PLACEMENT_3D('',#90386,#67846,#67847);
#61402=AXIS2_PLACEMENT_3D('',#90387,#67848,#67849);
#61403=AXIS2_PLACEMENT_3D('',#90396,#67854,#67855);
#61404=AXIS2_PLACEMENT_3D('',#90402,#67859,#67860);
#61405=AXIS2_PLACEMENT_3D('',#90408,#67864,#67865);
#61406=AXIS2_PLACEMENT_3D('',#90411,#67868,#67869);
#61407=AXIS2_PLACEMENT_3D('',#90412,#67870,#67871);
#61408=AXIS2_PLACEMENT_3D('',#90421,#67876,#67877);
#61409=AXIS2_PLACEMENT_3D('',#90427,#67881,#67882);
#61410=AXIS2_PLACEMENT_3D('',#90433,#67886,#67887);
#61411=AXIS2_PLACEMENT_3D('',#90436,#67890,#67891);
#61412=AXIS2_PLACEMENT_3D('',#90437,#67892,#67893);
#61413=AXIS2_PLACEMENT_3D('',#90446,#67898,#67899);
#61414=AXIS2_PLACEMENT_3D('',#90452,#67903,#67904);
#61415=AXIS2_PLACEMENT_3D('',#90458,#67908,#67909);
#61416=AXIS2_PLACEMENT_3D('',#90461,#67912,#67913);
#61417=AXIS2_PLACEMENT_3D('',#90462,#67914,#67915);
#61418=AXIS2_PLACEMENT_3D('',#90471,#67920,#67921);
#61419=AXIS2_PLACEMENT_3D('',#90477,#67925,#67926);
#61420=AXIS2_PLACEMENT_3D('',#90483,#67930,#67931);
#61421=AXIS2_PLACEMENT_3D('',#90486,#67934,#67935);
#61422=AXIS2_PLACEMENT_3D('',#90487,#67936,#67937);
#61423=AXIS2_PLACEMENT_3D('',#90496,#67942,#67943);
#61424=AXIS2_PLACEMENT_3D('',#90502,#67947,#67948);
#61425=AXIS2_PLACEMENT_3D('',#90508,#67952,#67953);
#61426=AXIS2_PLACEMENT_3D('',#90511,#67956,#67957);
#61427=AXIS2_PLACEMENT_3D('',#90512,#67958,#67959);
#61428=AXIS2_PLACEMENT_3D('',#90521,#67964,#67965);
#61429=AXIS2_PLACEMENT_3D('',#90527,#67969,#67970);
#61430=AXIS2_PLACEMENT_3D('',#90533,#67974,#67975);
#61431=AXIS2_PLACEMENT_3D('',#90536,#67978,#67979);
#61432=AXIS2_PLACEMENT_3D('',#90537,#67980,#67981);
#61433=AXIS2_PLACEMENT_3D('',#90546,#67986,#67987);
#61434=AXIS2_PLACEMENT_3D('',#90552,#67991,#67992);
#61435=AXIS2_PLACEMENT_3D('',#90558,#67996,#67997);
#61436=AXIS2_PLACEMENT_3D('',#90561,#68000,#68001);
#61437=AXIS2_PLACEMENT_3D('',#90562,#68002,#68003);
#61438=AXIS2_PLACEMENT_3D('',#90571,#68008,#68009);
#61439=AXIS2_PLACEMENT_3D('',#90577,#68013,#68014);
#61440=AXIS2_PLACEMENT_3D('',#90583,#68018,#68019);
#61441=AXIS2_PLACEMENT_3D('',#90586,#68022,#68023);
#61442=AXIS2_PLACEMENT_3D('',#90587,#68024,#68025);
#61443=AXIS2_PLACEMENT_3D('',#90596,#68030,#68031);
#61444=AXIS2_PLACEMENT_3D('',#90602,#68035,#68036);
#61445=AXIS2_PLACEMENT_3D('',#90608,#68040,#68041);
#61446=AXIS2_PLACEMENT_3D('',#90611,#68044,#68045);
#61447=AXIS2_PLACEMENT_3D('',#90612,#68046,#68047);
#61448=AXIS2_PLACEMENT_3D('',#90621,#68052,#68053);
#61449=AXIS2_PLACEMENT_3D('',#90627,#68057,#68058);
#61450=AXIS2_PLACEMENT_3D('',#90633,#68062,#68063);
#61451=AXIS2_PLACEMENT_3D('',#90636,#68066,#68067);
#61452=AXIS2_PLACEMENT_3D('',#90637,#68068,#68069);
#61453=AXIS2_PLACEMENT_3D('',#90646,#68074,#68075);
#61454=AXIS2_PLACEMENT_3D('',#90652,#68079,#68080);
#61455=AXIS2_PLACEMENT_3D('',#90658,#68084,#68085);
#61456=AXIS2_PLACEMENT_3D('',#90661,#68088,#68089);
#61457=AXIS2_PLACEMENT_3D('',#90662,#68090,#68091);
#61458=AXIS2_PLACEMENT_3D('',#90671,#68096,#68097);
#61459=AXIS2_PLACEMENT_3D('',#90677,#68101,#68102);
#61460=AXIS2_PLACEMENT_3D('',#90683,#68106,#68107);
#61461=AXIS2_PLACEMENT_3D('',#90686,#68110,#68111);
#61462=AXIS2_PLACEMENT_3D('',#90687,#68112,#68113);
#61463=AXIS2_PLACEMENT_3D('',#90696,#68118,#68119);
#61464=AXIS2_PLACEMENT_3D('',#90702,#68123,#68124);
#61465=AXIS2_PLACEMENT_3D('',#90708,#68128,#68129);
#61466=AXIS2_PLACEMENT_3D('',#90711,#68132,#68133);
#61467=AXIS2_PLACEMENT_3D('',#90712,#68134,#68135);
#61468=AXIS2_PLACEMENT_3D('',#90721,#68140,#68141);
#61469=AXIS2_PLACEMENT_3D('',#90727,#68145,#68146);
#61470=AXIS2_PLACEMENT_3D('',#90733,#68150,#68151);
#61471=AXIS2_PLACEMENT_3D('',#90736,#68154,#68155);
#61472=AXIS2_PLACEMENT_3D('',#90737,#68156,#68157);
#61473=AXIS2_PLACEMENT_3D('',#90746,#68162,#68163);
#61474=AXIS2_PLACEMENT_3D('',#90752,#68167,#68168);
#61475=AXIS2_PLACEMENT_3D('',#90758,#68172,#68173);
#61476=AXIS2_PLACEMENT_3D('',#90761,#68176,#68177);
#61477=AXIS2_PLACEMENT_3D('',#90762,#68178,#68179);
#61478=AXIS2_PLACEMENT_3D('',#90771,#68184,#68185);
#61479=AXIS2_PLACEMENT_3D('',#90777,#68189,#68190);
#61480=AXIS2_PLACEMENT_3D('',#90783,#68194,#68195);
#61481=AXIS2_PLACEMENT_3D('',#90786,#68198,#68199);
#61482=AXIS2_PLACEMENT_3D('',#90787,#68200,#68201);
#61483=AXIS2_PLACEMENT_3D('',#90796,#68206,#68207);
#61484=AXIS2_PLACEMENT_3D('',#90802,#68211,#68212);
#61485=AXIS2_PLACEMENT_3D('',#90808,#68216,#68217);
#61486=AXIS2_PLACEMENT_3D('',#90811,#68220,#68221);
#61487=AXIS2_PLACEMENT_3D('',#90812,#68222,#68223);
#61488=AXIS2_PLACEMENT_3D('',#90821,#68228,#68229);
#61489=AXIS2_PLACEMENT_3D('',#90827,#68233,#68234);
#61490=AXIS2_PLACEMENT_3D('',#90833,#68238,#68239);
#61491=AXIS2_PLACEMENT_3D('',#90836,#68242,#68243);
#61492=AXIS2_PLACEMENT_3D('',#90837,#68244,#68245);
#61493=AXIS2_PLACEMENT_3D('',#90846,#68250,#68251);
#61494=AXIS2_PLACEMENT_3D('',#90852,#68255,#68256);
#61495=AXIS2_PLACEMENT_3D('',#90858,#68260,#68261);
#61496=AXIS2_PLACEMENT_3D('',#90861,#68264,#68265);
#61497=AXIS2_PLACEMENT_3D('',#90862,#68266,#68267);
#61498=AXIS2_PLACEMENT_3D('',#90871,#68272,#68273);
#61499=AXIS2_PLACEMENT_3D('',#90877,#68277,#68278);
#61500=AXIS2_PLACEMENT_3D('',#90883,#68282,#68283);
#61501=AXIS2_PLACEMENT_3D('',#90886,#68286,#68287);
#61502=AXIS2_PLACEMENT_3D('',#90887,#68288,#68289);
#61503=AXIS2_PLACEMENT_3D('',#90896,#68294,#68295);
#61504=AXIS2_PLACEMENT_3D('',#90902,#68299,#68300);
#61505=AXIS2_PLACEMENT_3D('',#90908,#68304,#68305);
#61506=AXIS2_PLACEMENT_3D('',#90911,#68308,#68309);
#61507=AXIS2_PLACEMENT_3D('',#90912,#68310,#68311);
#61508=AXIS2_PLACEMENT_3D('',#90921,#68316,#68317);
#61509=AXIS2_PLACEMENT_3D('',#90927,#68321,#68322);
#61510=AXIS2_PLACEMENT_3D('',#90933,#68326,#68327);
#61511=AXIS2_PLACEMENT_3D('',#90936,#68330,#68331);
#61512=AXIS2_PLACEMENT_3D('',#90937,#68332,#68333);
#61513=AXIS2_PLACEMENT_3D('',#90946,#68338,#68339);
#61514=AXIS2_PLACEMENT_3D('',#90952,#68343,#68344);
#61515=AXIS2_PLACEMENT_3D('',#90958,#68348,#68349);
#61516=AXIS2_PLACEMENT_3D('',#90961,#68352,#68353);
#61517=AXIS2_PLACEMENT_3D('',#90962,#68354,#68355);
#61518=AXIS2_PLACEMENT_3D('',#90971,#68360,#68361);
#61519=AXIS2_PLACEMENT_3D('',#90977,#68365,#68366);
#61520=AXIS2_PLACEMENT_3D('',#90983,#68370,#68371);
#61521=AXIS2_PLACEMENT_3D('',#90986,#68374,#68375);
#61522=AXIS2_PLACEMENT_3D('',#90987,#68376,#68377);
#61523=AXIS2_PLACEMENT_3D('',#90996,#68382,#68383);
#61524=AXIS2_PLACEMENT_3D('',#91002,#68387,#68388);
#61525=AXIS2_PLACEMENT_3D('',#91008,#68392,#68393);
#61526=AXIS2_PLACEMENT_3D('',#91011,#68396,#68397);
#61527=AXIS2_PLACEMENT_3D('',#91012,#68398,#68399);
#61528=AXIS2_PLACEMENT_3D('',#91021,#68404,#68405);
#61529=AXIS2_PLACEMENT_3D('',#91027,#68409,#68410);
#61530=AXIS2_PLACEMENT_3D('',#91033,#68414,#68415);
#61531=AXIS2_PLACEMENT_3D('',#91036,#68418,#68419);
#61532=AXIS2_PLACEMENT_3D('',#91037,#68420,#68421);
#61533=AXIS2_PLACEMENT_3D('',#91046,#68426,#68427);
#61534=AXIS2_PLACEMENT_3D('',#91052,#68431,#68432);
#61535=AXIS2_PLACEMENT_3D('',#91058,#68436,#68437);
#61536=AXIS2_PLACEMENT_3D('',#91061,#68440,#68441);
#61537=AXIS2_PLACEMENT_3D('',#91062,#68442,#68443);
#61538=AXIS2_PLACEMENT_3D('',#91071,#68448,#68449);
#61539=AXIS2_PLACEMENT_3D('',#91077,#68453,#68454);
#61540=AXIS2_PLACEMENT_3D('',#91083,#68458,#68459);
#61541=AXIS2_PLACEMENT_3D('',#91086,#68462,#68463);
#61542=AXIS2_PLACEMENT_3D('',#91087,#68464,#68465);
#61543=AXIS2_PLACEMENT_3D('',#91096,#68470,#68471);
#61544=AXIS2_PLACEMENT_3D('',#91102,#68475,#68476);
#61545=AXIS2_PLACEMENT_3D('',#91108,#68480,#68481);
#61546=AXIS2_PLACEMENT_3D('',#91111,#68484,#68485);
#61547=AXIS2_PLACEMENT_3D('',#91112,#68486,#68487);
#61548=AXIS2_PLACEMENT_3D('',#91121,#68492,#68493);
#61549=AXIS2_PLACEMENT_3D('',#91127,#68497,#68498);
#61550=AXIS2_PLACEMENT_3D('',#91133,#68502,#68503);
#61551=AXIS2_PLACEMENT_3D('',#91136,#68506,#68507);
#61552=AXIS2_PLACEMENT_3D('',#91137,#68508,#68509);
#61553=AXIS2_PLACEMENT_3D('',#91146,#68514,#68515);
#61554=AXIS2_PLACEMENT_3D('',#91152,#68519,#68520);
#61555=AXIS2_PLACEMENT_3D('',#91158,#68524,#68525);
#61556=AXIS2_PLACEMENT_3D('',#91161,#68528,#68529);
#61557=AXIS2_PLACEMENT_3D('',#91162,#68530,#68531);
#61558=AXIS2_PLACEMENT_3D('',#91171,#68536,#68537);
#61559=AXIS2_PLACEMENT_3D('',#91177,#68541,#68542);
#61560=AXIS2_PLACEMENT_3D('',#91183,#68546,#68547);
#61561=AXIS2_PLACEMENT_3D('',#91186,#68550,#68551);
#61562=AXIS2_PLACEMENT_3D('',#91187,#68552,#68553);
#61563=AXIS2_PLACEMENT_3D('',#91196,#68558,#68559);
#61564=AXIS2_PLACEMENT_3D('',#91202,#68563,#68564);
#61565=AXIS2_PLACEMENT_3D('',#91208,#68568,#68569);
#61566=AXIS2_PLACEMENT_3D('',#91211,#68572,#68573);
#61567=AXIS2_PLACEMENT_3D('',#91212,#68574,#68575);
#61568=AXIS2_PLACEMENT_3D('',#91221,#68580,#68581);
#61569=AXIS2_PLACEMENT_3D('',#91227,#68585,#68586);
#61570=AXIS2_PLACEMENT_3D('',#91233,#68590,#68591);
#61571=AXIS2_PLACEMENT_3D('',#91236,#68594,#68595);
#61572=AXIS2_PLACEMENT_3D('',#91237,#68596,#68597);
#61573=AXIS2_PLACEMENT_3D('',#91246,#68602,#68603);
#61574=AXIS2_PLACEMENT_3D('',#91252,#68607,#68608);
#61575=AXIS2_PLACEMENT_3D('',#91258,#68612,#68613);
#61576=AXIS2_PLACEMENT_3D('',#91261,#68616,#68617);
#61577=AXIS2_PLACEMENT_3D('',#91262,#68618,#68619);
#61578=AXIS2_PLACEMENT_3D('',#91271,#68624,#68625);
#61579=AXIS2_PLACEMENT_3D('',#91277,#68629,#68630);
#61580=AXIS2_PLACEMENT_3D('',#91283,#68634,#68635);
#61581=AXIS2_PLACEMENT_3D('',#91286,#68638,#68639);
#61582=AXIS2_PLACEMENT_3D('',#91287,#68640,#68641);
#61583=AXIS2_PLACEMENT_3D('',#91296,#68646,#68647);
#61584=AXIS2_PLACEMENT_3D('',#91302,#68651,#68652);
#61585=AXIS2_PLACEMENT_3D('',#91308,#68656,#68657);
#61586=AXIS2_PLACEMENT_3D('',#91311,#68660,#68661);
#61587=AXIS2_PLACEMENT_3D('',#91312,#68662,#68663);
#61588=AXIS2_PLACEMENT_3D('',#91321,#68668,#68669);
#61589=AXIS2_PLACEMENT_3D('',#91327,#68673,#68674);
#61590=AXIS2_PLACEMENT_3D('',#91333,#68678,#68679);
#61591=AXIS2_PLACEMENT_3D('',#91336,#68682,#68683);
#61592=AXIS2_PLACEMENT_3D('',#91337,#68684,#68685);
#61593=AXIS2_PLACEMENT_3D('',#91346,#68690,#68691);
#61594=AXIS2_PLACEMENT_3D('',#91352,#68695,#68696);
#61595=AXIS2_PLACEMENT_3D('',#91358,#68700,#68701);
#61596=AXIS2_PLACEMENT_3D('',#91361,#68704,#68705);
#61597=AXIS2_PLACEMENT_3D('',#91362,#68706,#68707);
#61598=AXIS2_PLACEMENT_3D('',#91371,#68712,#68713);
#61599=AXIS2_PLACEMENT_3D('',#91377,#68717,#68718);
#61600=AXIS2_PLACEMENT_3D('',#91383,#68722,#68723);
#61601=AXIS2_PLACEMENT_3D('',#91386,#68726,#68727);
#61602=AXIS2_PLACEMENT_3D('',#91387,#68728,#68729);
#61603=AXIS2_PLACEMENT_3D('',#91396,#68734,#68735);
#61604=AXIS2_PLACEMENT_3D('',#91402,#68739,#68740);
#61605=AXIS2_PLACEMENT_3D('',#91408,#68744,#68745);
#61606=AXIS2_PLACEMENT_3D('',#91411,#68748,#68749);
#61607=AXIS2_PLACEMENT_3D('',#91412,#68750,#68751);
#61608=AXIS2_PLACEMENT_3D('',#91421,#68756,#68757);
#61609=AXIS2_PLACEMENT_3D('',#91427,#68761,#68762);
#61610=AXIS2_PLACEMENT_3D('',#91433,#68766,#68767);
#61611=AXIS2_PLACEMENT_3D('',#91436,#68770,#68771);
#61612=AXIS2_PLACEMENT_3D('',#91437,#68772,#68773);
#61613=AXIS2_PLACEMENT_3D('',#91446,#68778,#68779);
#61614=AXIS2_PLACEMENT_3D('',#91452,#68783,#68784);
#61615=AXIS2_PLACEMENT_3D('',#91458,#68788,#68789);
#61616=AXIS2_PLACEMENT_3D('',#91461,#68792,#68793);
#61617=AXIS2_PLACEMENT_3D('',#91462,#68794,#68795);
#61618=AXIS2_PLACEMENT_3D('',#91471,#68800,#68801);
#61619=AXIS2_PLACEMENT_3D('',#91477,#68805,#68806);
#61620=AXIS2_PLACEMENT_3D('',#91483,#68810,#68811);
#61621=AXIS2_PLACEMENT_3D('',#91486,#68814,#68815);
#61622=AXIS2_PLACEMENT_3D('',#91487,#68816,#68817);
#61623=AXIS2_PLACEMENT_3D('',#91496,#68822,#68823);
#61624=AXIS2_PLACEMENT_3D('',#91502,#68827,#68828);
#61625=AXIS2_PLACEMENT_3D('',#91508,#68832,#68833);
#61626=AXIS2_PLACEMENT_3D('',#91511,#68836,#68837);
#61627=AXIS2_PLACEMENT_3D('',#91512,#68838,#68839);
#61628=AXIS2_PLACEMENT_3D('',#91521,#68844,#68845);
#61629=AXIS2_PLACEMENT_3D('',#91527,#68849,#68850);
#61630=AXIS2_PLACEMENT_3D('',#91533,#68854,#68855);
#61631=AXIS2_PLACEMENT_3D('',#91536,#68858,#68859);
#61632=AXIS2_PLACEMENT_3D('',#91537,#68860,#68861);
#61633=AXIS2_PLACEMENT_3D('',#91546,#68866,#68867);
#61634=AXIS2_PLACEMENT_3D('',#91552,#68871,#68872);
#61635=AXIS2_PLACEMENT_3D('',#91558,#68876,#68877);
#61636=AXIS2_PLACEMENT_3D('',#91561,#68880,#68881);
#61637=AXIS2_PLACEMENT_3D('',#91562,#68882,#68883);
#61638=AXIS2_PLACEMENT_3D('',#91571,#68888,#68889);
#61639=AXIS2_PLACEMENT_3D('',#91577,#68893,#68894);
#61640=AXIS2_PLACEMENT_3D('',#91583,#68898,#68899);
#61641=AXIS2_PLACEMENT_3D('',#91586,#68902,#68903);
#61642=AXIS2_PLACEMENT_3D('',#91587,#68904,#68905);
#61643=AXIS2_PLACEMENT_3D('',#91596,#68910,#68911);
#61644=AXIS2_PLACEMENT_3D('',#91602,#68915,#68916);
#61645=AXIS2_PLACEMENT_3D('',#91608,#68920,#68921);
#61646=AXIS2_PLACEMENT_3D('',#91611,#68924,#68925);
#61647=AXIS2_PLACEMENT_3D('',#91612,#68926,#68927);
#61648=AXIS2_PLACEMENT_3D('',#91621,#68932,#68933);
#61649=AXIS2_PLACEMENT_3D('',#91627,#68937,#68938);
#61650=AXIS2_PLACEMENT_3D('',#91633,#68942,#68943);
#61651=AXIS2_PLACEMENT_3D('',#91636,#68946,#68947);
#61652=AXIS2_PLACEMENT_3D('',#91637,#68948,#68949);
#61653=AXIS2_PLACEMENT_3D('',#91646,#68954,#68955);
#61654=AXIS2_PLACEMENT_3D('',#91652,#68959,#68960);
#61655=AXIS2_PLACEMENT_3D('',#91658,#68964,#68965);
#61656=AXIS2_PLACEMENT_3D('',#91661,#68968,#68969);
#61657=AXIS2_PLACEMENT_3D('',#91662,#68970,#68971);
#61658=AXIS2_PLACEMENT_3D('',#91671,#68976,#68977);
#61659=AXIS2_PLACEMENT_3D('',#91677,#68981,#68982);
#61660=AXIS2_PLACEMENT_3D('',#91683,#68986,#68987);
#61661=AXIS2_PLACEMENT_3D('',#91686,#68990,#68991);
#61662=AXIS2_PLACEMENT_3D('',#91687,#68992,#68993);
#61663=AXIS2_PLACEMENT_3D('',#91700,#69000,#69001);
#61664=AXIS2_PLACEMENT_3D('',#91713,#69008,#69009);
#61665=AXIS2_PLACEMENT_3D('',#91716,#69012,#69013);
#61666=AXIS2_PLACEMENT_3D('',#91728,#69019,#69020);
#61667=AXIS2_PLACEMENT_3D('',#91748,#69030,#69031);
#61668=AXIS2_PLACEMENT_3D('',#91758,#69037,#69038);
#61669=AXIS2_PLACEMENT_3D('',#91764,#69042,#69043);
#61670=AXIS2_PLACEMENT_3D('',#91770,#69047,#69048);
#61671=AXIS2_PLACEMENT_3D('',#91774,#69051,#69052);
#61672=AXIS2_PLACEMENT_3D('',#91777,#69054,#69055);
#61673=AXIS2_PLACEMENT_3D('',#91779,#69056,#69057);
#61674=AXIS2_PLACEMENT_3D('',#91781,#69058,#69059);
#61675=AXIS2_PLACEMENT_3D('',#91782,#69060,#69061);
#61676=AXIS2_PLACEMENT_3D('',#91784,#69062,#69063);
#61677=AXIS2_PLACEMENT_3D('',#91787,#69065,#69066);
#61678=AXIS2_PLACEMENT_3D('',#91789,#69067,#69068);
#61679=AXIS2_PLACEMENT_3D('',#91792,#69070,#69071);
#61680=AXIS2_PLACEMENT_3D('',#91794,#69072,#69073);
#61681=AXIS2_PLACEMENT_3D('',#91796,#69075,#69076);
#61682=AXIS2_PLACEMENT_3D('',#91798,#69077,#69078);
#61683=AXIS2_PLACEMENT_3D('',#91800,#69080,#69081);
#61684=AXIS2_PLACEMENT_3D('',#91802,#69082,#69083);
#61685=AXIS2_PLACEMENT_3D('',#91805,#69085,#69086);
#61686=AXIS2_PLACEMENT_3D('',#91806,#69087,#69088);
#61687=AXIS2_PLACEMENT_3D('',#91809,#69090,#69091);
#61688=AXIS2_PLACEMENT_3D('',#91810,#69092,#69093);
#61689=AXIS2_PLACEMENT_3D('',#91820,#69098,#69099);
#61690=AXIS2_PLACEMENT_3D('',#91821,#69100,#69101);
#61691=AXIS2_PLACEMENT_3D('',#91824,#69103,#69104);
#61692=AXIS2_PLACEMENT_3D('',#91827,#69106,#69107);
#61693=AXIS2_PLACEMENT_3D('',#91828,#69108,#69109);
#61694=AXIS2_PLACEMENT_3D('',#91831,#69111,#69112);
#61695=AXIS2_PLACEMENT_3D('',#91832,#69113,#69114);
#61696=AXIS2_PLACEMENT_3D('',#91835,#69116,#69117);
#61697=AXIS2_PLACEMENT_3D('',#91837,#69118,#69119);
#61698=AXIS2_PLACEMENT_3D('',#91840,#69121,#69122);
#61699=AXIS2_PLACEMENT_3D('',#91841,#69123,#69124);
#61700=AXIS2_PLACEMENT_3D('',#91843,#69125,#69126);
#61701=AXIS2_PLACEMENT_3D('',#91844,#69127,#69128);
#61702=AXIS2_PLACEMENT_3D('',#91846,#69129,#69130);
#61703=AXIS2_PLACEMENT_3D('',#91849,#69132,#69133);
#61704=AXIS2_PLACEMENT_3D('',#91850,#69134,#69135);
#61705=AXIS2_PLACEMENT_3D('',#91852,#69136,#69137);
#61706=AXIS2_PLACEMENT_3D('',#91853,#69138,#69139);
#61707=AXIS2_PLACEMENT_3D('',#91855,#69140,#69141);
#61708=AXIS2_PLACEMENT_3D('',#91858,#69143,#69144);
#61709=AXIS2_PLACEMENT_3D('',#91859,#69145,#69146);
#61710=AXIS2_PLACEMENT_3D('',#91861,#69147,#69148);
#61711=AXIS2_PLACEMENT_3D('',#91862,#69149,#69150);
#61712=AXIS2_PLACEMENT_3D('',#91864,#69151,#69152);
#61713=AXIS2_PLACEMENT_3D('',#91867,#69154,#69155);
#61714=AXIS2_PLACEMENT_3D('',#91868,#69156,#69157);
#61715=AXIS2_PLACEMENT_3D('',#91870,#69158,#69159);
#61716=AXIS2_PLACEMENT_3D('',#91871,#69160,#69161);
#61717=AXIS2_PLACEMENT_3D('',#91873,#69162,#69163);
#61718=AXIS2_PLACEMENT_3D('',#91876,#69165,#69166);
#61719=AXIS2_PLACEMENT_3D('',#91877,#69167,#69168);
#61720=AXIS2_PLACEMENT_3D('',#91879,#69169,#69170);
#61721=AXIS2_PLACEMENT_3D('',#91880,#69171,#69172);
#61722=AXIS2_PLACEMENT_3D('',#91882,#69173,#69174);
#61723=AXIS2_PLACEMENT_3D('',#91885,#69176,#69177);
#61724=AXIS2_PLACEMENT_3D('',#91886,#69178,#69179);
#61725=AXIS2_PLACEMENT_3D('',#91888,#69180,#69181);
#61726=AXIS2_PLACEMENT_3D('',#91889,#69182,#69183);
#61727=AXIS2_PLACEMENT_3D('',#91892,#69185,#69186);
#61728=AXIS2_PLACEMENT_3D('',#91893,#69187,#69188);
#61729=AXIS2_PLACEMENT_3D('',#91898,#69191,#69192);
#61730=AXIS2_PLACEMENT_3D('',#91900,#69193,#69194);
#61731=AXIS2_PLACEMENT_3D('',#91902,#69195,#69196);
#61732=AXIS2_PLACEMENT_3D('',#91903,#69197,#69198);
#61733=AXIS2_PLACEMENT_3D('',#91905,#69200,#69201);
#61734=AXIS2_PLACEMENT_3D('',#91908,#69203,#69204);
#61735=AXIS2_PLACEMENT_3D('',#91909,#69205,#69206);
#61736=AXIS2_PLACEMENT_3D('',#91911,#69208,#69209);
#61737=AXIS2_PLACEMENT_3D('',#91914,#69211,#69212);
#61738=AXIS2_PLACEMENT_3D('',#91915,#69213,#69214);
#61739=AXIS2_PLACEMENT_3D('',#91917,#69216,#69217);
#61740=AXIS2_PLACEMENT_3D('',#91920,#69219,#69220);
#61741=AXIS2_PLACEMENT_3D('',#91921,#69221,#69222);
#61742=AXIS2_PLACEMENT_3D('',#91923,#69224,#69225);
#61743=AXIS2_PLACEMENT_3D('',#91926,#69227,#69228);
#61744=AXIS2_PLACEMENT_3D('',#91927,#69229,#69230);
#61745=AXIS2_PLACEMENT_3D('',#91929,#69232,#69233);
#61746=AXIS2_PLACEMENT_3D('',#91932,#69235,#69236);
#61747=AXIS2_PLACEMENT_3D('',#91933,#69237,#69238);
#61748=AXIS2_PLACEMENT_3D('',#91935,#69240,#69241);
#61749=AXIS2_PLACEMENT_3D('',#91940,#69243,#69244);
#61750=AXIS2_PLACEMENT_3D('',#91944,#69247,#69248);
#61751=AXIS2_PLACEMENT_3D('',#91950,#69252,#69253);
#61752=AXIS2_PLACEMENT_3D('',#91956,#69257,#69258);
#61753=AXIS2_PLACEMENT_3D('',#91964,#69263,#69264);
#61754=AXIS2_PLACEMENT_3D('',#91970,#69268,#69269);
#61755=AXIS2_PLACEMENT_3D('',#91976,#69273,#69274);
#61756=AXIS2_PLACEMENT_3D('',#91980,#69276,#69277);
#61757=AXIS2_PLACEMENT_3D('',#91982,#69279,#69280);
#61758=AXIS2_PLACEMENT_3D('',#91986,#69283,#69284);
#61759=AXIS2_PLACEMENT_3D('',#91989,#69287,#69288);
#61760=AXIS2_PLACEMENT_3D('',#91992,#69290,#69291);
#61761=AXIS2_PLACEMENT_3D('',#91994,#69292,#69293);
#61762=AXIS2_PLACEMENT_3D('',#91998,#69295,#69296);
#61763=AXIS2_PLACEMENT_3D('',#91999,#69297,#69298);
#61764=AXIS2_PLACEMENT_3D('',#92000,#69299,#69300);
#61765=AXIS2_PLACEMENT_3D('',#92004,#69303,#69304);
#61766=AXIS2_PLACEMENT_3D('',#92008,#69307,#69308);
#61767=AXIS2_PLACEMENT_3D('',#92012,#69311,#69312);
#61768=AXIS2_PLACEMENT_3D('',#92014,#69314,#69315);
#61769=AXIS2_PLACEMENT_3D('',#92018,#69318,#69319);
#61770=AXIS2_PLACEMENT_3D('',#92023,#69321,#69322);
#61771=AXIS2_PLACEMENT_3D('',#92027,#69325,#69326);
#61772=AXIS2_PLACEMENT_3D('',#92033,#69330,#69331);
#61773=AXIS2_PLACEMENT_3D('',#92039,#69335,#69336);
#61774=AXIS2_PLACEMENT_3D('',#92042,#69339,#69340);
#61775=AXIS2_PLACEMENT_3D('',#92048,#69344,#69345);
#61776=AXIS2_PLACEMENT_3D('',#92054,#69349,#69350);
#61777=AXIS2_PLACEMENT_3D('',#92060,#69354,#69355);
#61778=AXIS2_PLACEMENT_3D('',#92063,#69358,#69359);
#61779=AXIS2_PLACEMENT_3D('',#92069,#69363,#69364);
#61780=AXIS2_PLACEMENT_3D('',#92073,#69367,#69368);
#61781=AXIS2_PLACEMENT_3D('',#92077,#69371,#69372);
#61782=AXIS2_PLACEMENT_3D('',#92079,#69374,#69375);
#61783=AXIS2_PLACEMENT_3D('',#92083,#69378,#69379);
#61784=AXIS2_PLACEMENT_3D('',#92087,#69382,#69383);
#61785=AXIS2_PLACEMENT_3D('',#92091,#69386,#69387);
#61786=AXIS2_PLACEMENT_3D('',#92093,#69389,#69390);
#61787=AXIS2_PLACEMENT_3D('',#92097,#69392,#69393);
#61788=AXIS2_PLACEMENT_3D('',#92099,#69395,#69396);
#61789=AXIS2_PLACEMENT_3D('',#92103,#69399,#69400);
#61790=AXIS2_PLACEMENT_3D('',#92106,#69403,#69404);
#61791=AXIS2_PLACEMENT_3D('',#92108,#69406,#69407);
#61792=AXIS2_PLACEMENT_3D('',#92110,#69409,#69410);
#61793=AXIS2_PLACEMENT_3D('',#92112,#69412,#69413);
#61794=AXIS2_PLACEMENT_3D('',#92114,#69415,#69416);
#61795=AXIS2_PLACEMENT_3D('',#92116,#69418,#69419);
#61796=AXIS2_PLACEMENT_3D('',#92117,#69420,#69421);
#61797=AXIS2_PLACEMENT_3D('',#92119,#69423,#69424);
#61798=AXIS2_PLACEMENT_3D('',#92121,#69426,#69427);
#61799=AXIS2_PLACEMENT_3D('',#92123,#69429,#69430);
#61800=AXIS2_PLACEMENT_3D('',#92124,#69431,#69432);
#61801=AXIS2_PLACEMENT_3D('',#92126,#69434,#69435);
#61802=AXIS2_PLACEMENT_3D('',#92128,#69437,#69438);
#61803=AXIS2_PLACEMENT_3D('',#92130,#69440,#69441);
#61804=AXIS2_PLACEMENT_3D('',#92132,#69443,#69444);
#61805=AXIS2_PLACEMENT_3D('',#92133,#69445,#69446);
#61806=AXIS2_PLACEMENT_3D('',#92134,#69447,#69448);
#61807=AXIS2_PLACEMENT_3D('',#92135,#69449,#69450);
#61808=AXIS2_PLACEMENT_3D('',#92136,#69451,#69452);
#61809=AXIS2_PLACEMENT_3D('',#92138,#69454,#69455);
#61810=AXIS2_PLACEMENT_3D('',#92140,#69457,#69458);
#61811=AXIS2_PLACEMENT_3D('',#92142,#69460,#69461);
#61812=AXIS2_PLACEMENT_3D('',#92143,#69462,#69463);
#61813=AXIS2_PLACEMENT_3D('',#92144,#69464,#69465);
#61814=AXIS2_PLACEMENT_3D('',#92149,#69467,#69468);
#61815=AXIS2_PLACEMENT_3D('',#92154,#69469,#69470);
#61816=AXIS2_PLACEMENT_3D('',#92155,#69471,#69472);
#61817=AXIS2_PLACEMENT_3D('',#92158,#69473,#69474);
#61818=AXIS2_PLACEMENT_3D('',#92161,#69476,#69477);
#61819=AXIS2_PLACEMENT_3D('',#92162,#69478,#69479);
#61820=AXIS2_PLACEMENT_3D('',#92163,#69480,#69481);
#61821=AXIS2_PLACEMENT_3D('',#92170,#69484,#69485);
#61822=AXIS2_PLACEMENT_3D('',#92171,#69486,#69487);
#61823=AXIS2_PLACEMENT_3D('',#92179,#69492,#69493);
#61824=AXIS2_PLACEMENT_3D('',#92180,#69494,#69495);
#61825=AXIS2_PLACEMENT_3D('',#92183,#69497,#69498);
#61826=AXIS2_PLACEMENT_3D('',#92184,#69499,#69500);
#61827=AXIS2_PLACEMENT_3D('',#92187,#69502,#69503);
#61828=AXIS2_PLACEMENT_3D('',#92188,#69504,#69505);
#61829=AXIS2_PLACEMENT_3D('',#92191,#69507,#69508);
#61830=AXIS2_PLACEMENT_3D('',#92192,#69509,#69510);
#61831=AXIS2_PLACEMENT_3D('',#92195,#69512,#69513);
#61832=AXIS2_PLACEMENT_3D('',#92198,#69515,#69516);
#61833=AXIS2_PLACEMENT_3D('',#92205,#69517,#69518);
#61834=AXIS2_PLACEMENT_3D('',#92208,#69520,#69521);
#61835=AXIS2_PLACEMENT_3D('',#92209,#69522,#69523);
#61836=AXIS2_PLACEMENT_3D('',#92210,#69524,#69525);
#61837=AXIS2_PLACEMENT_3D('',#92231,#69533,#69534);
#61838=AXIS2_PLACEMENT_3D('',#92234,#69536,#69537);
#61839=AXIS2_PLACEMENT_3D('',#92235,#69538,#69539);
#61840=AXIS2_PLACEMENT_3D('',#92237,#69540,#69541);
#61841=AXIS2_PLACEMENT_3D('',#92240,#69543,#69544);
#61842=AXIS2_PLACEMENT_3D('',#92241,#69545,#69546);
#61843=AXIS2_PLACEMENT_3D('',#92242,#69547,#69548);
#61844=AXIS2_PLACEMENT_3D('',#92245,#69550,#69551);
#61845=AXIS2_PLACEMENT_3D('',#92246,#69552,#69553);
#61846=AXIS2_PLACEMENT_3D('',#92247,#69554,#69555);
#61847=AXIS2_PLACEMENT_3D('',#92248,#69556,#69557);
#61848=AXIS2_PLACEMENT_3D('',#92249,#69558,#69559);
#61849=AXIS2_PLACEMENT_3D('',#92252,#69561,#69562);
#61850=AXIS2_PLACEMENT_3D('',#92253,#69563,#69564);
#61851=AXIS2_PLACEMENT_3D('',#92259,#69568,#69569);
#61852=AXIS2_PLACEMENT_3D('',#92266,#69570,#69571);
#61853=AXIS2_PLACEMENT_3D('',#92269,#69573,#69574);
#61854=AXIS2_PLACEMENT_3D('',#92270,#69575,#69576);
#61855=AXIS2_PLACEMENT_3D('',#92271,#69577,#69578);
#61856=AXIS2_PLACEMENT_3D('',#92278,#69583,#69584);
#61857=AXIS2_PLACEMENT_3D('',#92282,#69586,#69587);
#61858=AXIS2_PLACEMENT_3D('',#92284,#69588,#69589);
#61859=AXIS2_PLACEMENT_3D('',#92285,#69590,#69591);
#61860=AXIS2_PLACEMENT_3D('',#92286,#69592,#69593);
#61861=AXIS2_PLACEMENT_3D('',#92288,#69594,#69595);
#61862=AXIS2_PLACEMENT_3D('',#92291,#69597,#69598);
#61863=AXIS2_PLACEMENT_3D('',#92292,#69599,#69600);
#61864=AXIS2_PLACEMENT_3D('',#92299,#69604,#69605);
#61865=AXIS2_PLACEMENT_3D('',#92301,#69606,#69607);
#61866=AXIS2_PLACEMENT_3D('',#92303,#69608,#69609);
#61867=AXIS2_PLACEMENT_3D('',#92305,#69610,#69611);
#61868=AXIS2_PLACEMENT_3D('',#92307,#69612,#69613);
#61869=AXIS2_PLACEMENT_3D('',#92308,#69614,#69615);
#61870=AXIS2_PLACEMENT_3D('',#92312,#69617,#69618);
#61871=AXIS2_PLACEMENT_3D('',#92314,#69619,#69620);
#61872=AXIS2_PLACEMENT_3D('',#92315,#69621,#69622);
#61873=AXIS2_PLACEMENT_3D('',#92316,#69623,#69624);
#61874=AXIS2_PLACEMENT_3D('',#92319,#69626,#69627);
#61875=AXIS2_PLACEMENT_3D('',#92320,#69628,#69629);
#61876=AXIS2_PLACEMENT_3D('',#92324,#69631,#69632);
#61877=AXIS2_PLACEMENT_3D('',#92326,#69633,#69634);
#61878=AXIS2_PLACEMENT_3D('',#92327,#69635,#69636);
#61879=AXIS2_PLACEMENT_3D('',#92328,#69637,#69638);
#61880=AXIS2_PLACEMENT_3D('',#92330,#69640,#69641);
#61881=AXIS2_PLACEMENT_3D('',#92332,#69643,#69644);
#61882=AXIS2_PLACEMENT_3D('',#92334,#69646,#69647);
#61883=AXIS2_PLACEMENT_3D('',#92336,#69649,#69650);
#61884=AXIS2_PLACEMENT_3D('',#92338,#69652,#69653);
#61885=AXIS2_PLACEMENT_3D('',#92340,#69655,#69656);
#61886=AXIS2_PLACEMENT_3D('',#92343,#69658,#69659);
#61887=AXIS2_PLACEMENT_3D('',#92344,#69660,#69661);
#61888=AXIS2_PLACEMENT_3D('',#92347,#69663,#69664);
#61889=AXIS2_PLACEMENT_3D('',#92348,#69665,#69666);
#61890=AXIS2_PLACEMENT_3D('',#92351,#69668,#69669);
#61891=AXIS2_PLACEMENT_3D('',#92352,#69670,#69671);
#61892=AXIS2_PLACEMENT_3D('',#92355,#69673,#69674);
#61893=AXIS2_PLACEMENT_3D('',#92356,#69675,#69676);
#61894=AXIS2_PLACEMENT_3D('',#92359,#69678,#69679);
#61895=AXIS2_PLACEMENT_3D('',#92360,#69680,#69681);
#61896=AXIS2_PLACEMENT_3D('',#92363,#69683,#69684);
#61897=AXIS2_PLACEMENT_3D('',#92364,#69685,#69686);
#61898=AXIS2_PLACEMENT_3D('',#92367,#69688,#69689);
#61899=AXIS2_PLACEMENT_3D('',#92368,#69690,#69691);
#61900=AXIS2_PLACEMENT_3D('',#92371,#69693,#69694);
#61901=AXIS2_PLACEMENT_3D('',#92372,#69695,#69696);
#61902=AXIS2_PLACEMENT_3D('',#92375,#69698,#69699);
#61903=AXIS2_PLACEMENT_3D('',#92378,#69701,#69702);
#61904=AXIS2_PLACEMENT_3D('',#92381,#69704,#69705);
#61905=AXIS2_PLACEMENT_3D('',#92384,#69707,#69708);
#61906=AXIS2_PLACEMENT_3D('',#92388,#69710,#69711);
#61907=AXIS2_PLACEMENT_3D('',#92389,#69712,#69713);
#61908=AXIS2_PLACEMENT_3D('',#92390,#69714,#69715);
#61909=AXIS2_PLACEMENT_3D('',#92397,#69720,#69721);
#61910=AXIS2_PLACEMENT_3D('',#92401,#69723,#69724);
#61911=AXIS2_PLACEMENT_3D('',#92404,#69726,#69727);
#61912=AXIS2_PLACEMENT_3D('',#92405,#69728,#69729);
#61913=AXIS2_PLACEMENT_3D('',#92409,#69731,#69732);
#61914=AXIS2_PLACEMENT_3D('',#92410,#69733,#69734);
#61915=AXIS2_PLACEMENT_3D('',#92412,#69735,#69736);
#61916=AXIS2_PLACEMENT_3D('',#92414,#69738,#69739);
#61917=AXIS2_PLACEMENT_3D('',#92416,#69741,#69742);
#61918=AXIS2_PLACEMENT_3D('',#92426,#69748,#69749);
#61919=AXIS2_PLACEMENT_3D('',#92432,#69753,#69754);
#61920=AXIS2_PLACEMENT_3D('',#92438,#69758,#69759);
#61921=AXIS2_PLACEMENT_3D('',#92456,#69769,#69770);
#61922=AXIS2_PLACEMENT_3D('',#92460,#69773,#69774);
#61923=AXIS2_PLACEMENT_3D('',#92468,#69779,#69780);
#61924=AXIS2_PLACEMENT_3D('',#92478,#69786,#69787);
#61925=AXIS2_PLACEMENT_3D('',#92480,#69789,#69790);
#61926=AXIS2_PLACEMENT_3D('',#92484,#69793,#69794);
#61927=AXIS2_PLACEMENT_3D('',#92487,#69797,#69798);
#61928=AXIS2_PLACEMENT_3D('',#92491,#69801,#69802);
#61929=AXIS2_PLACEMENT_3D('',#92495,#69805,#69806);
#61930=AXIS2_PLACEMENT_3D('',#92498,#69809,#69810);
#61931=AXIS2_PLACEMENT_3D('',#92502,#69813,#69814);
#61932=AXIS2_PLACEMENT_3D('',#92505,#69817,#69818);
#61933=AXIS2_PLACEMENT_3D('',#92509,#69821,#69822);
#61934=AXIS2_PLACEMENT_3D('',#92512,#69825,#69826);
#61935=AXIS2_PLACEMENT_3D('',#92517,#69830,#69831);
#61936=AXIS2_PLACEMENT_3D('',#92519,#69833,#69834);
#61937=AXIS2_PLACEMENT_3D('',#92523,#69838,#69839);
#61938=AXIS2_PLACEMENT_3D('',#92524,#69840,#69841);
#61939=AXIS2_PLACEMENT_3D('',#92525,#69842,#69843);
#61940=AXIS2_PLACEMENT_3D('',#92526,#69844,#69845);
#61941=AXIS2_PLACEMENT_3D('',#92528,#69847,#69848);
#61942=AXIS2_PLACEMENT_3D('',#92530,#69850,#69851);
#61943=AXIS2_PLACEMENT_3D('',#92531,#69852,#69853);
#61944=AXIS2_PLACEMENT_3D('',#92534,#69856,#69857);
#61945=AXIS2_PLACEMENT_3D('',#92535,#69858,#69859);
#61946=AXIS2_PLACEMENT_3D('',#92537,#69861,#69862);
#61947=AXIS2_PLACEMENT_3D('',#92538,#69863,#69864);
#61948=AXIS2_PLACEMENT_3D('',#92539,#69865,#69866);
#61949=AXIS2_PLACEMENT_3D('',#92540,#69867,#69868);
#61950=AXIS2_PLACEMENT_3D('',#92542,#69869,#69870);
#61951=AXIS2_PLACEMENT_3D('',#92545,#69872,#69873);
#61952=AXIS2_PLACEMENT_3D('',#92547,#69874,#69875);
#61953=AXIS2_PLACEMENT_3D('',#92550,#69877,#69878);
#61954=AXIS2_PLACEMENT_3D('',#92552,#69879,#69880);
#61955=AXIS2_PLACEMENT_3D('',#92555,#69882,#69883);
#61956=AXIS2_PLACEMENT_3D('',#92564,#69888,#69889);
#61957=AXIS2_PLACEMENT_3D('',#92570,#69893,#69894);
#61958=AXIS2_PLACEMENT_3D('',#92576,#69898,#69899);
#61959=AXIS2_PLACEMENT_3D('',#92579,#69902,#69903);
#61960=AXIS2_PLACEMENT_3D('',#92585,#69907,#69908);
#61961=AXIS2_PLACEMENT_3D('',#92589,#69911,#69912);
#61962=AXIS2_PLACEMENT_3D('',#92590,#69913,#69914);
#61963=AXIS2_PLACEMENT_3D('',#92596,#69918,#69919);
#61964=AXIS2_PLACEMENT_3D('',#92600,#69922,#69923);
#61965=AXIS2_PLACEMENT_3D('',#92606,#69927,#69928);
#61966=AXIS2_PLACEMENT_3D('',#92609,#69931,#69932);
#61967=AXIS2_PLACEMENT_3D('',#92611,#69934,#69935);
#61968=AXIS2_PLACEMENT_3D('',#92612,#69936,#69937);
#61969=AXIS2_PLACEMENT_3D('',#92613,#69938,#69939);
#61970=AXIS2_PLACEMENT_3D('',#92614,#69940,#69941);
#61971=AXIS2_PLACEMENT_3D('',#92617,#69942,#69943);
#61972=AXIS2_PLACEMENT_3D('',#92619,#69945,#69946);
#61973=AXIS2_PLACEMENT_3D('',#92622,#69947,#69948);
#61974=AXIS2_PLACEMENT_3D('',#92624,#69950,#69951);
#61975=AXIS2_PLACEMENT_3D('',#92627,#69954,#69955);
#61976=AXIS2_PLACEMENT_3D('',#92630,#69956,#69957);
#61977=AXIS2_PLACEMENT_3D('',#92632,#69959,#69960);
#61978=AXIS2_PLACEMENT_3D('',#92635,#69961,#69962);
#61979=AXIS2_PLACEMENT_3D('',#92637,#69964,#69965);
#61980=AXIS2_PLACEMENT_3D('',#92640,#69968,#69969);
#61981=AXIS2_PLACEMENT_3D('',#92642,#69970,#69971);
#61982=AXIS2_PLACEMENT_3D('',#92643,#69972,#69973);
#61983=AXIS2_PLACEMENT_3D('',#92645,#69974,#69975);
#61984=AXIS2_PLACEMENT_3D('',#92647,#69977,#69978);
#61985=AXIS2_PLACEMENT_3D('',#92649,#69979,#69980);
#61986=AXIS2_PLACEMENT_3D('',#92651,#69982,#69983);
#61987=AXIS2_PLACEMENT_3D('',#92653,#69984,#69985);
#61988=AXIS2_PLACEMENT_3D('',#92655,#69987,#69988);
#61989=AXIS2_PLACEMENT_3D('',#92656,#69989,#69990);
#61990=AXIS2_PLACEMENT_3D('',#92657,#69991,#69992);
#61991=AXIS2_PLACEMENT_3D('',#92661,#69994,#69995);
#61992=AXIS2_PLACEMENT_3D('',#92662,#69996,#69997);
#61993=AXIS2_PLACEMENT_3D('',#92708,#69999,#70000);
#61994=AXIS2_PLACEMENT_3D('',#92730,#70001,#70002);
#61995=AXIS2_PLACEMENT_3D('',#92731,#70003,#70004);
#61996=AXIS2_PLACEMENT_3D('',#92733,#70006,#70007);
#61997=AXIS2_PLACEMENT_3D('',#92742,#70012,#70013);
#61998=AXIS2_PLACEMENT_3D('',#92894,#70019,#70020);
#61999=AXIS2_PLACEMENT_3D('',#92896,#70021,#70022);
#62000=AXIS2_PLACEMENT_3D('',#92898,#70023,#70024);
#62001=AXIS2_PLACEMENT_3D('',#93040,#70026,#70027);
#62002=AXIS2_PLACEMENT_3D('',#93041,#70028,#70029);
#62003=AXIS2_PLACEMENT_3D('',#93042,#70030,#70031);
#62004=AXIS2_PLACEMENT_3D('',#93044,#70032,#70033);
#62005=AXIS2_PLACEMENT_3D('',#93048,#70035,#70036);
#62006=AXIS2_PLACEMENT_3D('',#93052,#70038,#70039);
#62007=AXIS2_PLACEMENT_3D('',#93056,#70041,#70042);
#62008=AXIS2_PLACEMENT_3D('',#93060,#70044,#70045);
#62009=AXIS2_PLACEMENT_3D('',#93064,#70047,#70048);
#62010=AXIS2_PLACEMENT_3D('',#93067,#70050,#70051);
#62011=AXIS2_PLACEMENT_3D('',#93069,#70052,#70053);
#62012=AXIS2_PLACEMENT_3D('',#93073,#70055,#70056);
#62013=AXIS2_PLACEMENT_3D('',#93077,#70058,#70059);
#62014=AXIS2_PLACEMENT_3D('',#93081,#70061,#70062);
#62015=AXIS2_PLACEMENT_3D('',#93085,#70064,#70065);
#62016=AXIS2_PLACEMENT_3D('',#93089,#70067,#70068);
#62017=AXIS2_PLACEMENT_3D('',#93093,#70070,#70071);
#62018=AXIS2_PLACEMENT_3D('',#93097,#70073,#70074);
#62019=AXIS2_PLACEMENT_3D('',#93101,#70076,#70077);
#62020=AXIS2_PLACEMENT_3D('',#93105,#70079,#70080);
#62021=AXIS2_PLACEMENT_3D('',#93109,#70082,#70083);
#62022=AXIS2_PLACEMENT_3D('',#93113,#70085,#70086);
#62023=AXIS2_PLACEMENT_3D('',#93117,#70088,#70089);
#62024=AXIS2_PLACEMENT_3D('',#93121,#70091,#70092);
#62025=AXIS2_PLACEMENT_3D('',#93125,#70094,#70095);
#62026=AXIS2_PLACEMENT_3D('',#93129,#70097,#70098);
#62027=AXIS2_PLACEMENT_3D('',#93133,#70100,#70101);
#62028=AXIS2_PLACEMENT_3D('',#93137,#70103,#70104);
#62029=AXIS2_PLACEMENT_3D('',#93141,#70106,#70107);
#62030=AXIS2_PLACEMENT_3D('',#93145,#70109,#70110);
#62031=AXIS2_PLACEMENT_3D('',#93149,#70112,#70113);
#62032=AXIS2_PLACEMENT_3D('',#93153,#70115,#70116);
#62033=AXIS2_PLACEMENT_3D('',#93157,#70118,#70119);
#62034=AXIS2_PLACEMENT_3D('',#93161,#70121,#70122);
#62035=AXIS2_PLACEMENT_3D('',#93165,#70124,#70125);
#62036=AXIS2_PLACEMENT_3D('',#93168,#70127,#70128);
#62037=AXIS2_PLACEMENT_3D('',#93169,#70129,#70130);
#62038=AXIS2_PLACEMENT_3D('',#93175,#70134,#70135);
#62039=AXIS2_PLACEMENT_3D('',#93324,#70140,#70141);
#62040=AXIS2_PLACEMENT_3D('',#93326,#70142,#70143);
#62041=AXIS2_PLACEMENT_3D('',#93328,#70144,#70145);
#62042=AXIS2_PLACEMENT_3D('',#93470,#70147,#70148);
#62043=AXIS2_PLACEMENT_3D('',#93471,#70149,#70150);
#62044=AXIS2_PLACEMENT_3D('',#93477,#70154,#70155);
#62045=AXIS2_PLACEMENT_3D('',#93626,#70160,#70161);
#62046=AXIS2_PLACEMENT_3D('',#93628,#70162,#70163);
#62047=AXIS2_PLACEMENT_3D('',#93630,#70164,#70165);
#62048=AXIS2_PLACEMENT_3D('',#93772,#70167,#70168);
#62049=AXIS2_PLACEMENT_3D('',#93773,#70169,#70170);
#62050=AXIS2_PLACEMENT_3D('',#93779,#70174,#70175);
#62051=AXIS2_PLACEMENT_3D('',#93928,#70180,#70181);
#62052=AXIS2_PLACEMENT_3D('',#93930,#70182,#70183);
#62053=AXIS2_PLACEMENT_3D('',#93932,#70184,#70185);
#62054=AXIS2_PLACEMENT_3D('',#94074,#70187,#70188);
#62055=AXIS2_PLACEMENT_3D('',#94075,#70189,#70190);
#62056=AXIS2_PLACEMENT_3D('',#94081,#70194,#70195);
#62057=AXIS2_PLACEMENT_3D('',#94230,#70200,#70201);
#62058=AXIS2_PLACEMENT_3D('',#94232,#70202,#70203);
#62059=AXIS2_PLACEMENT_3D('',#94234,#70204,#70205);
#62060=AXIS2_PLACEMENT_3D('',#94376,#70207,#70208);
#62061=AXIS2_PLACEMENT_3D('',#94377,#70209,#70210);
#62062=AXIS2_PLACEMENT_3D('',#94383,#70214,#70215);
#62063=AXIS2_PLACEMENT_3D('',#94532,#70220,#70221);
#62064=AXIS2_PLACEMENT_3D('',#94534,#70222,#70223);
#62065=AXIS2_PLACEMENT_3D('',#94536,#70224,#70225);
#62066=AXIS2_PLACEMENT_3D('',#94678,#70227,#70228);
#62067=AXIS2_PLACEMENT_3D('',#94679,#70229,#70230);
#62068=AXIS2_PLACEMENT_3D('',#94685,#70234,#70235);
#62069=AXIS2_PLACEMENT_3D('',#94834,#70240,#70241);
#62070=AXIS2_PLACEMENT_3D('',#94836,#70242,#70243);
#62071=AXIS2_PLACEMENT_3D('',#94838,#70244,#70245);
#62072=AXIS2_PLACEMENT_3D('',#94980,#70247,#70248);
#62073=AXIS2_PLACEMENT_3D('',#94981,#70249,#70250);
#62074=AXIS2_PLACEMENT_3D('',#94987,#70254,#70255);
#62075=AXIS2_PLACEMENT_3D('',#95136,#70260,#70261);
#62076=AXIS2_PLACEMENT_3D('',#95138,#70262,#70263);
#62077=AXIS2_PLACEMENT_3D('',#95140,#70264,#70265);
#62078=AXIS2_PLACEMENT_3D('',#95282,#70267,#70268);
#62079=AXIS2_PLACEMENT_3D('',#95283,#70269,#70270);
#62080=AXIS2_PLACEMENT_3D('',#95289,#70274,#70275);
#62081=AXIS2_PLACEMENT_3D('',#95438,#70280,#70281);
#62082=AXIS2_PLACEMENT_3D('',#95440,#70282,#70283);
#62083=AXIS2_PLACEMENT_3D('',#95442,#70284,#70285);
#62084=AXIS2_PLACEMENT_3D('',#95584,#70287,#70288);
#62085=AXIS2_PLACEMENT_3D('',#95585,#70289,#70290);
#62086=AXIS2_PLACEMENT_3D('',#95591,#70294,#70295);
#62087=AXIS2_PLACEMENT_3D('',#95740,#70300,#70301);
#62088=AXIS2_PLACEMENT_3D('',#95742,#70302,#70303);
#62089=AXIS2_PLACEMENT_3D('',#95744,#70304,#70305);
#62090=AXIS2_PLACEMENT_3D('',#95886,#70307,#70308);
#62091=AXIS2_PLACEMENT_3D('',#95887,#70309,#70310);
#62092=AXIS2_PLACEMENT_3D('',#95893,#70314,#70315);
#62093=AXIS2_PLACEMENT_3D('',#96042,#70320,#70321);
#62094=AXIS2_PLACEMENT_3D('',#96044,#70322,#70323);
#62095=AXIS2_PLACEMENT_3D('',#96046,#70324,#70325);
#62096=AXIS2_PLACEMENT_3D('',#96188,#70327,#70328);
#62097=AXIS2_PLACEMENT_3D('',#96189,#70329,#70330);
#62098=AXIS2_PLACEMENT_3D('',#96195,#70334,#70335);
#62099=AXIS2_PLACEMENT_3D('',#96344,#70340,#70341);
#62100=AXIS2_PLACEMENT_3D('',#96346,#70342,#70343);
#62101=AXIS2_PLACEMENT_3D('',#96348,#70344,#70345);
#62102=AXIS2_PLACEMENT_3D('',#96490,#70347,#70348);
#62103=AXIS2_PLACEMENT_3D('',#96491,#70349,#70350);
#62104=AXIS2_PLACEMENT_3D('',#96497,#70354,#70355);
#62105=AXIS2_PLACEMENT_3D('',#96646,#70360,#70361);
#62106=AXIS2_PLACEMENT_3D('',#96648,#70362,#70363);
#62107=AXIS2_PLACEMENT_3D('',#96650,#70364,#70365);
#62108=AXIS2_PLACEMENT_3D('',#96792,#70367,#70368);
#62109=AXIS2_PLACEMENT_3D('',#96793,#70369,#70370);
#62110=AXIS2_PLACEMENT_3D('',#96799,#70374,#70375);
#62111=AXIS2_PLACEMENT_3D('',#96948,#70380,#70381);
#62112=AXIS2_PLACEMENT_3D('',#96950,#70382,#70383);
#62113=AXIS2_PLACEMENT_3D('',#96952,#70384,#70385);
#62114=AXIS2_PLACEMENT_3D('',#97094,#70387,#70388);
#62115=AXIS2_PLACEMENT_3D('',#97095,#70389,#70390);
#62116=AXIS2_PLACEMENT_3D('',#97101,#70394,#70395);
#62117=AXIS2_PLACEMENT_3D('',#97250,#70400,#70401);
#62118=AXIS2_PLACEMENT_3D('',#97252,#70402,#70403);
#62119=AXIS2_PLACEMENT_3D('',#97254,#70404,#70405);
#62120=AXIS2_PLACEMENT_3D('',#97396,#70407,#70408);
#62121=AXIS2_PLACEMENT_3D('',#97397,#70409,#70410);
#62122=AXIS2_PLACEMENT_3D('',#97546,#70415,#70416);
#62123=AXIS2_PLACEMENT_3D('',#97548,#70417,#70418);
#62124=AXIS2_PLACEMENT_3D('',#97550,#70419,#70420);
#62125=AXIS2_PLACEMENT_3D('',#97695,#70423,#70424);
#62126=AXIS2_PLACEMENT_3D('',#97698,#70427,#70428);
#62127=AXIS2_PLACEMENT_3D('',#97699,#70429,#70430);
#62128=AXIS2_PLACEMENT_3D('',#97701,#70431,#70432);
#62129=AXIS2_PLACEMENT_3D('',#97704,#70434,#70435);
#62130=AXIS2_PLACEMENT_3D('',#97705,#70436,#70437);
#62131=AXIS2_PLACEMENT_3D('',#97706,#70438,#70439);
#62132=AXIS2_PLACEMENT_3D('',#97708,#70440,#70441);
#62133=AXIS2_PLACEMENT_3D('',#97709,#70442,#70443);
#62134=AXIS2_PLACEMENT_3D('',#97711,#70444,#70445);
#62135=AXIS2_PLACEMENT_3D('',#97713,#70447,#70448);
#62136=AXIS2_PLACEMENT_3D('',#97715,#70449,#70450);
#62137=AXIS2_PLACEMENT_3D('',#97717,#70452,#70453);
#62138=AXIS2_PLACEMENT_3D('',#97718,#70454,#70455);
#62139=AXIS2_PLACEMENT_3D('',#97719,#70456,#70457);
#62140=AXIS2_PLACEMENT_3D('',#97724,#70459,#70460);
#62141=AXIS2_PLACEMENT_3D('',#97725,#70461,#70462);
#62142=AXIS2_PLACEMENT_3D('',#97726,#70463,#70464);
#62143=AXIS2_PLACEMENT_3D('',#97790,#70466,#70467);
#62144=AXIS2_PLACEMENT_3D('',#97809,#70468,#70469);
#62145=AXIS2_PLACEMENT_3D('',#97811,#70471,#70472);
#62146=AXIS2_PLACEMENT_3D('',#97824,#70475,#70476);
#62147=AXIS2_PLACEMENT_3D('',#97834,#70478,#70479);
#62148=AXIS2_PLACEMENT_3D('',#97836,#70480,#70481);
#62149=AXIS2_PLACEMENT_3D('',#97846,#70482,#70483);
#62150=AXIS2_PLACEMENT_3D('',#97856,#70484,#70485);
#62151=AXIS2_PLACEMENT_3D('',#97866,#70486,#70487);
#62152=AXIS2_PLACEMENT_3D('',#97876,#70488,#70489);
#62153=AXIS2_PLACEMENT_3D('',#97886,#70490,#70491);
#62154=AXIS2_PLACEMENT_3D('',#97896,#70492,#70493);
#62155=AXIS2_PLACEMENT_3D('',#97906,#70494,#70495);
#62156=AXIS2_PLACEMENT_3D('',#97916,#70496,#70497);
#62157=AXIS2_PLACEMENT_3D('',#97926,#70498,#70499);
#62158=AXIS2_PLACEMENT_3D('',#97936,#70500,#70501);
#62159=AXIS2_PLACEMENT_3D('',#97946,#70502,#70503);
#62160=AXIS2_PLACEMENT_3D('',#97956,#70504,#70505);
#62161=AXIS2_PLACEMENT_3D('',#97966,#70506,#70507);
#62162=AXIS2_PLACEMENT_3D('',#97976,#70508,#70509);
#62163=AXIS2_PLACEMENT_3D('',#97986,#70510,#70511);
#62164=AXIS2_PLACEMENT_3D('',#97996,#70512,#70513);
#62165=AXIS2_PLACEMENT_3D('',#98006,#70514,#70515);
#62166=AXIS2_PLACEMENT_3D('',#98016,#70516,#70517);
#62167=AXIS2_PLACEMENT_3D('',#98023,#70519,#70520);
#62168=AXIS2_PLACEMENT_3D('',#98029,#70521,#70522);
#62169=AXIS2_PLACEMENT_3D('',#98039,#70523,#70524);
#62170=AXIS2_PLACEMENT_3D('',#98049,#70525,#70526);
#62171=AXIS2_PLACEMENT_3D('',#98059,#70527,#70528);
#62172=AXIS2_PLACEMENT_3D('',#98069,#70529,#70530);
#62173=AXIS2_PLACEMENT_3D('',#98079,#70531,#70532);
#62174=AXIS2_PLACEMENT_3D('',#98089,#70533,#70534);
#62175=AXIS2_PLACEMENT_3D('',#98099,#70535,#70536);
#62176=AXIS2_PLACEMENT_3D('',#98109,#70537,#70538);
#62177=AXIS2_PLACEMENT_3D('',#98119,#70539,#70540);
#62178=AXIS2_PLACEMENT_3D('',#98129,#70541,#70542);
#62179=AXIS2_PLACEMENT_3D('',#98139,#70543,#70544);
#62180=AXIS2_PLACEMENT_3D('',#98149,#70545,#70546);
#62181=AXIS2_PLACEMENT_3D('',#98159,#70547,#70548);
#62182=AXIS2_PLACEMENT_3D('',#98169,#70549,#70550);
#62183=AXIS2_PLACEMENT_3D('',#98179,#70551,#70552);
#62184=AXIS2_PLACEMENT_3D('',#98189,#70553,#70554);
#62185=AXIS2_PLACEMENT_3D('',#98199,#70555,#70556);
#62186=AXIS2_PLACEMENT_3D('',#98209,#70557,#70558);
#62187=AXIS2_PLACEMENT_3D('',#98219,#70559,#70560);
#62188=AXIS2_PLACEMENT_3D('',#98228,#70561,#70562);
#62189=AXIS2_PLACEMENT_3D('',#98229,#70563,#70564);
#62190=AXIS2_PLACEMENT_3D('',#98231,#70565,#70566);
#62191=AXIS2_PLACEMENT_3D('',#98233,#70568,#70569);
#62192=AXIS2_PLACEMENT_3D('',#98236,#70571,#70572);
#62193=AXIS2_PLACEMENT_3D('',#98237,#70573,#70574);
#62194=AXIS2_PLACEMENT_3D('',#98245,#70577,#70578);
#62195=AXIS2_PLACEMENT_3D('',#98249,#70579,#70580);
#62196=AXIS2_PLACEMENT_3D('',#98251,#70581,#70582);
#62197=AXIS2_PLACEMENT_3D('',#98253,#70584,#70585);
#62198=AXIS2_PLACEMENT_3D('',#98255,#70586,#70587);
#62199=AXIS2_PLACEMENT_3D('',#98263,#70589,#70590);
#62200=AXIS2_PLACEMENT_3D('',#98273,#70591,#70592);
#62201=AXIS2_PLACEMENT_3D('',#98283,#70593,#70594);
#62202=AXIS2_PLACEMENT_3D('',#98293,#70595,#70596);
#62203=AXIS2_PLACEMENT_3D('',#98303,#70597,#70598);
#62204=AXIS2_PLACEMENT_3D('',#98313,#70599,#70600);
#62205=AXIS2_PLACEMENT_3D('',#98323,#70601,#70602);
#62206=AXIS2_PLACEMENT_3D('',#98333,#70603,#70604);
#62207=AXIS2_PLACEMENT_3D('',#98343,#70605,#70606);
#62208=AXIS2_PLACEMENT_3D('',#98353,#70607,#70608);
#62209=AXIS2_PLACEMENT_3D('',#98363,#70609,#70610);
#62210=AXIS2_PLACEMENT_3D('',#98373,#70611,#70612);
#62211=AXIS2_PLACEMENT_3D('',#98383,#70613,#70614);
#62212=AXIS2_PLACEMENT_3D('',#98393,#70615,#70616);
#62213=AXIS2_PLACEMENT_3D('',#98403,#70617,#70618);
#62214=AXIS2_PLACEMENT_3D('',#98413,#70619,#70620);
#62215=AXIS2_PLACEMENT_3D('',#98423,#70621,#70622);
#62216=AXIS2_PLACEMENT_3D('',#98440,#70623,#70624);
#62217=AXIS2_PLACEMENT_3D('',#98450,#70625,#70626);
#62218=AXIS2_PLACEMENT_3D('',#98460,#70627,#70628);
#62219=AXIS2_PLACEMENT_3D('',#98470,#70629,#70630);
#62220=AXIS2_PLACEMENT_3D('',#98480,#70631,#70632);
#62221=AXIS2_PLACEMENT_3D('',#98490,#70633,#70634);
#62222=AXIS2_PLACEMENT_3D('',#98500,#70635,#70636);
#62223=AXIS2_PLACEMENT_3D('',#98510,#70637,#70638);
#62224=AXIS2_PLACEMENT_3D('',#98520,#70639,#70640);
#62225=AXIS2_PLACEMENT_3D('',#98530,#70641,#70642);
#62226=AXIS2_PLACEMENT_3D('',#98540,#70643,#70644);
#62227=AXIS2_PLACEMENT_3D('',#98550,#70645,#70646);
#62228=AXIS2_PLACEMENT_3D('',#98560,#70647,#70648);
#62229=AXIS2_PLACEMENT_3D('',#98570,#70649,#70650);
#62230=AXIS2_PLACEMENT_3D('',#98580,#70651,#70652);
#62231=AXIS2_PLACEMENT_3D('',#98590,#70653,#70654);
#62232=AXIS2_PLACEMENT_3D('',#98600,#70655,#70656);
#62233=AXIS2_PLACEMENT_3D('',#98610,#70657,#70658);
#62234=AXIS2_PLACEMENT_3D('',#98620,#70659,#70660);
#62235=AXIS2_PLACEMENT_3D('',#98630,#70661,#70662);
#62236=AXIS2_PLACEMENT_3D('',#98634,#70663,#70664);
#62237=AXIS2_PLACEMENT_3D('',#98636,#70666,#70667);
#62238=AXIS2_PLACEMENT_3D('',#98638,#70669,#70670);
#62239=AXIS2_PLACEMENT_3D('',#98641,#70673,#70674);
#62240=AXIS2_PLACEMENT_3D('',#98643,#70676,#70677);
#62241=AXIS2_PLACEMENT_3D('',#98645,#70679,#70680);
#62242=AXIS2_PLACEMENT_3D('',#98646,#70681,#70682);
#62243=AXIS2_PLACEMENT_3D('',#98649,#70685,#70686);
#62244=AXIS2_PLACEMENT_3D('',#98650,#70687,#70688);
#62245=AXIS2_PLACEMENT_3D('',#98652,#70690,#70691);
#62246=AXIS2_PLACEMENT_3D('',#98654,#70693,#70694);
#62247=AXIS2_PLACEMENT_3D('',#98656,#70696,#70697);
#62248=AXIS2_PLACEMENT_3D('',#98659,#70700,#70701);
#62249=AXIS2_PLACEMENT_3D('',#98661,#70703,#70704);
#62250=AXIS2_PLACEMENT_3D('',#98663,#70706,#70707);
#62251=AXIS2_PLACEMENT_3D('',#98664,#70708,#70709);
#62252=AXIS2_PLACEMENT_3D('',#98667,#70712,#70713);
#62253=AXIS2_PLACEMENT_3D('',#98668,#70714,#70715);
#62254=AXIS2_PLACEMENT_3D('',#98670,#70717,#70718);
#62255=AXIS2_PLACEMENT_3D('',#98672,#70720,#70721);
#62256=AXIS2_PLACEMENT_3D('',#98674,#70723,#70724);
#62257=AXIS2_PLACEMENT_3D('',#98677,#70727,#70728);
#62258=AXIS2_PLACEMENT_3D('',#98679,#70730,#70731);
#62259=AXIS2_PLACEMENT_3D('',#98681,#70733,#70734);
#62260=AXIS2_PLACEMENT_3D('',#98682,#70735,#70736);
#62261=AXIS2_PLACEMENT_3D('',#98685,#70739,#70740);
#62262=AXIS2_PLACEMENT_3D('',#98686,#70741,#70742);
#62263=AXIS2_PLACEMENT_3D('',#98688,#70744,#70745);
#62264=AXIS2_PLACEMENT_3D('',#98690,#70747,#70748);
#62265=AXIS2_PLACEMENT_3D('',#98692,#70750,#70751);
#62266=AXIS2_PLACEMENT_3D('',#98695,#70754,#70755);
#62267=AXIS2_PLACEMENT_3D('',#98697,#70757,#70758);
#62268=AXIS2_PLACEMENT_3D('',#98699,#70760,#70761);
#62269=AXIS2_PLACEMENT_3D('',#98700,#70762,#70763);
#62270=AXIS2_PLACEMENT_3D('',#98703,#70766,#70767);
#62271=AXIS2_PLACEMENT_3D('',#98704,#70768,#70769);
#62272=AXIS2_PLACEMENT_3D('',#98706,#70771,#70772);
#62273=AXIS2_PLACEMENT_3D('',#98708,#70774,#70775);
#62274=AXIS2_PLACEMENT_3D('',#98710,#70777,#70778);
#62275=AXIS2_PLACEMENT_3D('',#98713,#70781,#70782);
#62276=AXIS2_PLACEMENT_3D('',#98715,#70784,#70785);
#62277=AXIS2_PLACEMENT_3D('',#98717,#70787,#70788);
#62278=AXIS2_PLACEMENT_3D('',#98718,#70789,#70790);
#62279=AXIS2_PLACEMENT_3D('',#98721,#70793,#70794);
#62280=AXIS2_PLACEMENT_3D('',#98722,#70795,#70796);
#62281=AXIS2_PLACEMENT_3D('',#98724,#70798,#70799);
#62282=AXIS2_PLACEMENT_3D('',#98726,#70801,#70802);
#62283=AXIS2_PLACEMENT_3D('',#98728,#70804,#70805);
#62284=AXIS2_PLACEMENT_3D('',#98731,#70808,#70809);
#62285=AXIS2_PLACEMENT_3D('',#98733,#70811,#70812);
#62286=AXIS2_PLACEMENT_3D('',#98735,#70814,#70815);
#62287=AXIS2_PLACEMENT_3D('',#98736,#70816,#70817);
#62288=AXIS2_PLACEMENT_3D('',#98739,#70820,#70821);
#62289=AXIS2_PLACEMENT_3D('',#98740,#70822,#70823);
#62290=AXIS2_PLACEMENT_3D('',#98742,#70825,#70826);
#62291=AXIS2_PLACEMENT_3D('',#98744,#70828,#70829);
#62292=AXIS2_PLACEMENT_3D('',#98746,#70831,#70832);
#62293=AXIS2_PLACEMENT_3D('',#98749,#70835,#70836);
#62294=AXIS2_PLACEMENT_3D('',#98751,#70838,#70839);
#62295=AXIS2_PLACEMENT_3D('',#98753,#70841,#70842);
#62296=AXIS2_PLACEMENT_3D('',#98754,#70843,#70844);
#62297=AXIS2_PLACEMENT_3D('',#98757,#70847,#70848);
#62298=AXIS2_PLACEMENT_3D('',#98758,#70849,#70850);
#62299=AXIS2_PLACEMENT_3D('',#98760,#70852,#70853);
#62300=AXIS2_PLACEMENT_3D('',#98762,#70855,#70856);
#62301=AXIS2_PLACEMENT_3D('',#98764,#70858,#70859);
#62302=AXIS2_PLACEMENT_3D('',#98767,#70862,#70863);
#62303=AXIS2_PLACEMENT_3D('',#98769,#70865,#70866);
#62304=AXIS2_PLACEMENT_3D('',#98771,#70868,#70869);
#62305=AXIS2_PLACEMENT_3D('',#98772,#70870,#70871);
#62306=AXIS2_PLACEMENT_3D('',#98775,#70874,#70875);
#62307=AXIS2_PLACEMENT_3D('',#98776,#70876,#70877);
#62308=AXIS2_PLACEMENT_3D('',#98778,#70879,#70880);
#62309=AXIS2_PLACEMENT_3D('',#98780,#70882,#70883);
#62310=AXIS2_PLACEMENT_3D('',#98782,#70885,#70886);
#62311=AXIS2_PLACEMENT_3D('',#98785,#70889,#70890);
#62312=AXIS2_PLACEMENT_3D('',#98787,#70892,#70893);
#62313=AXIS2_PLACEMENT_3D('',#98789,#70895,#70896);
#62314=AXIS2_PLACEMENT_3D('',#98790,#70897,#70898);
#62315=AXIS2_PLACEMENT_3D('',#98793,#70901,#70902);
#62316=AXIS2_PLACEMENT_3D('',#98794,#70903,#70904);
#62317=AXIS2_PLACEMENT_3D('',#98796,#70906,#70907);
#62318=AXIS2_PLACEMENT_3D('',#98798,#70909,#70910);
#62319=AXIS2_PLACEMENT_3D('',#98800,#70912,#70913);
#62320=AXIS2_PLACEMENT_3D('',#98803,#70916,#70917);
#62321=AXIS2_PLACEMENT_3D('',#98805,#70919,#70920);
#62322=AXIS2_PLACEMENT_3D('',#98807,#70922,#70923);
#62323=AXIS2_PLACEMENT_3D('',#98808,#70924,#70925);
#62324=AXIS2_PLACEMENT_3D('',#98811,#70928,#70929);
#62325=AXIS2_PLACEMENT_3D('',#98812,#70930,#70931);
#62326=AXIS2_PLACEMENT_3D('',#98814,#70933,#70934);
#62327=AXIS2_PLACEMENT_3D('',#98816,#70936,#70937);
#62328=AXIS2_PLACEMENT_3D('',#98818,#70939,#70940);
#62329=AXIS2_PLACEMENT_3D('',#98821,#70943,#70944);
#62330=AXIS2_PLACEMENT_3D('',#98823,#70946,#70947);
#62331=AXIS2_PLACEMENT_3D('',#98825,#70949,#70950);
#62332=AXIS2_PLACEMENT_3D('',#98826,#70951,#70952);
#62333=AXIS2_PLACEMENT_3D('',#98829,#70955,#70956);
#62334=AXIS2_PLACEMENT_3D('',#98830,#70957,#70958);
#62335=AXIS2_PLACEMENT_3D('',#98832,#70960,#70961);
#62336=AXIS2_PLACEMENT_3D('',#98834,#70963,#70964);
#62337=AXIS2_PLACEMENT_3D('',#98836,#70966,#70967);
#62338=AXIS2_PLACEMENT_3D('',#98839,#70970,#70971);
#62339=AXIS2_PLACEMENT_3D('',#98841,#70973,#70974);
#62340=AXIS2_PLACEMENT_3D('',#98843,#70976,#70977);
#62341=AXIS2_PLACEMENT_3D('',#98844,#70978,#70979);
#62342=AXIS2_PLACEMENT_3D('',#98847,#70982,#70983);
#62343=AXIS2_PLACEMENT_3D('',#98848,#70984,#70985);
#62344=AXIS2_PLACEMENT_3D('',#98850,#70987,#70988);
#62345=AXIS2_PLACEMENT_3D('',#98852,#70990,#70991);
#62346=AXIS2_PLACEMENT_3D('',#98854,#70993,#70994);
#62347=AXIS2_PLACEMENT_3D('',#98857,#70997,#70998);
#62348=AXIS2_PLACEMENT_3D('',#98858,#70999,#71000);
#62349=AXIS2_PLACEMENT_3D('',#98860,#71001,#71002);
#62350=AXIS2_PLACEMENT_3D('',#98863,#71004,#71005);
#62351=AXIS2_PLACEMENT_3D('',#98864,#71006,#71007);
#62352=AXIS2_PLACEMENT_3D('',#98866,#71008,#71009);
#62353=AXIS2_PLACEMENT_3D('',#98867,#71010,#71011);
#62354=AXIS2_PLACEMENT_3D('',#98869,#71012,#71013);
#62355=AXIS2_PLACEMENT_3D('',#98871,#71015,#71016);
#62356=AXIS2_PLACEMENT_3D('',#98873,#71017,#71018);
#62357=AXIS2_PLACEMENT_3D('',#98875,#71020,#71021);
#62358=AXIS2_PLACEMENT_3D('',#98877,#71022,#71023);
#62359=AXIS2_PLACEMENT_3D('',#98879,#71025,#71026);
#62360=AXIS2_PLACEMENT_3D('',#98881,#71027,#71028);
#62361=AXIS2_PLACEMENT_3D('',#98882,#71029,#71030);
#62362=AXIS2_PLACEMENT_3D('',#98884,#71031,#71032);
#62363=AXIS2_PLACEMENT_3D('',#98886,#71034,#71035);
#62364=AXIS2_PLACEMENT_3D('',#98888,#71036,#71037);
#62365=AXIS2_PLACEMENT_3D('',#98890,#71039,#71040);
#62366=AXIS2_PLACEMENT_3D('',#98891,#71041,#71042);
#62367=AXIS2_PLACEMENT_3D('',#98892,#71043,#71044);
#62368=AXIS2_PLACEMENT_3D('',#98894,#71045,#71046);
#62369=AXIS2_PLACEMENT_3D('',#98895,#71047,#71048);
#62370=AXIS2_PLACEMENT_3D('',#98898,#71050,#71051);
#62371=AXIS2_PLACEMENT_3D('',#98899,#71052,#71053);
#62372=AXIS2_PLACEMENT_3D('',#98900,#71054,#71055);
#62373=AXIS2_PLACEMENT_3D('',#98904,#71057,#71058);
#62374=AXIS2_PLACEMENT_3D('',#98905,#71059,#71060);
#62375=AXIS2_PLACEMENT_3D('',#98907,#71062,#71063);
#62376=AXIS2_PLACEMENT_3D('',#98908,#71064,#71065);
#62377=AXIS2_PLACEMENT_3D('',#98910,#71066,#71067);
#62378=AXIS2_PLACEMENT_3D('',#98913,#71069,#71070);
#62379=AXIS2_PLACEMENT_3D('',#98914,#71071,#71072);
#62380=AXIS2_PLACEMENT_3D('',#98916,#71073,#71074);
#62381=AXIS2_PLACEMENT_3D('',#98917,#71075,#71076);
#62382=AXIS2_PLACEMENT_3D('',#98919,#71077,#71078);
#62383=AXIS2_PLACEMENT_3D('',#98921,#71080,#71081);
#62384=AXIS2_PLACEMENT_3D('',#98923,#71082,#71083);
#62385=AXIS2_PLACEMENT_3D('',#98925,#71085,#71086);
#62386=AXIS2_PLACEMENT_3D('',#98927,#71087,#71088);
#62387=AXIS2_PLACEMENT_3D('',#98928,#71089,#71090);
#62388=AXIS2_PLACEMENT_3D('',#98930,#71091,#71092);
#62389=AXIS2_PLACEMENT_3D('',#98932,#71094,#71095);
#62390=AXIS2_PLACEMENT_3D('',#98934,#71096,#71097);
#62391=AXIS2_PLACEMENT_3D('',#98936,#71099,#71100);
#62392=AXIS2_PLACEMENT_3D('',#98938,#71101,#71102);
#62393=AXIS2_PLACEMENT_3D('',#98939,#71103,#71104);
#62394=AXIS2_PLACEMENT_3D('',#98942,#71106,#71107);
#62395=AXIS2_PLACEMENT_3D('',#98943,#71108,#71109);
#62396=AXIS2_PLACEMENT_3D('',#98945,#71111,#71112);
#62397=AXIS2_PLACEMENT_3D('',#98946,#71113,#71114);
#62398=AXIS2_PLACEMENT_3D('',#98948,#71115,#71116);
#62399=AXIS2_PLACEMENT_3D('',#98951,#71118,#71119);
#62400=AXIS2_PLACEMENT_3D('',#98952,#71120,#71121);
#62401=AXIS2_PLACEMENT_3D('',#98955,#71123,#71124);
#62402=AXIS2_PLACEMENT_3D('',#98956,#71125,#71126);
#62403=AXIS2_PLACEMENT_3D('',#98965,#71131,#71132);
#62404=AXIS2_PLACEMENT_3D('',#98967,#71133,#71134);
#62405=AXIS2_PLACEMENT_3D('',#98970,#71136,#71137);
#62406=AXIS2_PLACEMENT_3D('',#98971,#71138,#71139);
#62407=AXIS2_PLACEMENT_3D('',#98974,#71141,#71142);
#62408=AXIS2_PLACEMENT_3D('',#98975,#71143,#71144);
#62409=AXIS2_PLACEMENT_3D('',#98984,#71149,#71150);
#62410=AXIS2_PLACEMENT_3D('',#98986,#71151,#71152);
#62411=AXIS2_PLACEMENT_3D('',#98987,#71153,#71154);
#62412=AXIS2_PLACEMENT_3D('',#98989,#71155,#71156);
#62413=AXIS2_PLACEMENT_3D('',#98990,#71157,#71158);
#62414=AXIS2_PLACEMENT_3D('',#98993,#71160,#71161);
#62415=AXIS2_PLACEMENT_3D('',#98994,#71162,#71163);
#62416=AXIS2_PLACEMENT_3D('',#98997,#71165,#71166);
#62417=AXIS2_PLACEMENT_3D('',#98998,#71167,#71168);
#62418=AXIS2_PLACEMENT_3D('',#99007,#71173,#71174);
#62419=AXIS2_PLACEMENT_3D('',#99014,#71179,#71180);
#62420=AXIS2_PLACEMENT_3D('',#99018,#71183,#71184);
#62421=AXIS2_PLACEMENT_3D('',#99022,#71187,#71188);
#62422=AXIS2_PLACEMENT_3D('',#99028,#71192,#71193);
#62423=AXIS2_PLACEMENT_3D('',#99034,#71197,#71198);
#62424=AXIS2_PLACEMENT_3D('',#99040,#71202,#71203);
#62425=AXIS2_PLACEMENT_3D('',#99046,#71207,#71208);
#62426=AXIS2_PLACEMENT_3D('',#99052,#71212,#71213);
#62427=AXIS2_PLACEMENT_3D('',#99058,#71217,#71218);
#62428=AXIS2_PLACEMENT_3D('',#99064,#71222,#71223);
#62429=AXIS2_PLACEMENT_3D('',#99070,#71227,#71228);
#62430=AXIS2_PLACEMENT_3D('',#99076,#71232,#71233);
#62431=AXIS2_PLACEMENT_3D('',#99082,#71237,#71238);
#62432=AXIS2_PLACEMENT_3D('',#99088,#71242,#71243);
#62433=AXIS2_PLACEMENT_3D('',#99094,#71247,#71248);
#62434=AXIS2_PLACEMENT_3D('',#99100,#71252,#71253);
#62435=AXIS2_PLACEMENT_3D('',#99106,#71257,#71258);
#62436=AXIS2_PLACEMENT_3D('',#99112,#71262,#71263);
#62437=AXIS2_PLACEMENT_3D('',#99118,#71267,#71268);
#62438=AXIS2_PLACEMENT_3D('',#99124,#71272,#71273);
#62439=AXIS2_PLACEMENT_3D('',#99130,#71277,#71278);
#62440=AXIS2_PLACEMENT_3D('',#99136,#71282,#71283);
#62441=AXIS2_PLACEMENT_3D('',#99142,#71287,#71288);
#62442=AXIS2_PLACEMENT_3D('',#99148,#71292,#71293);
#62443=AXIS2_PLACEMENT_3D('',#99154,#71297,#71298);
#62444=AXIS2_PLACEMENT_3D('',#99160,#71302,#71303);
#62445=AXIS2_PLACEMENT_3D('',#99166,#71307,#71308);
#62446=AXIS2_PLACEMENT_3D('',#99172,#71312,#71313);
#62447=AXIS2_PLACEMENT_3D('',#99178,#71317,#71318);
#62448=AXIS2_PLACEMENT_3D('',#99184,#71322,#71323);
#62449=AXIS2_PLACEMENT_3D('',#99190,#71327,#71328);
#62450=AXIS2_PLACEMENT_3D('',#99196,#71332,#71333);
#62451=AXIS2_PLACEMENT_3D('',#99202,#71337,#71338);
#62452=AXIS2_PLACEMENT_3D('',#99208,#71342,#71343);
#62453=AXIS2_PLACEMENT_3D('',#99214,#71347,#71348);
#62454=AXIS2_PLACEMENT_3D('',#99220,#71352,#71353);
#62455=AXIS2_PLACEMENT_3D('',#99226,#71357,#71358);
#62456=AXIS2_PLACEMENT_3D('',#99232,#71362,#71363);
#62457=AXIS2_PLACEMENT_3D('',#99238,#71367,#71368);
#62458=AXIS2_PLACEMENT_3D('',#99244,#71372,#71373);
#62459=AXIS2_PLACEMENT_3D('',#99250,#71377,#71378);
#62460=AXIS2_PLACEMENT_3D('',#99256,#71382,#71383);
#62461=AXIS2_PLACEMENT_3D('',#99262,#71387,#71388);
#62462=AXIS2_PLACEMENT_3D('',#99268,#71392,#71393);
#62463=AXIS2_PLACEMENT_3D('',#99274,#71397,#71398);
#62464=AXIS2_PLACEMENT_3D('',#99280,#71402,#71403);
#62465=AXIS2_PLACEMENT_3D('',#99286,#71407,#71408);
#62466=AXIS2_PLACEMENT_3D('',#99292,#71412,#71413);
#62467=AXIS2_PLACEMENT_3D('',#99298,#71417,#71418);
#62468=AXIS2_PLACEMENT_3D('',#99304,#71422,#71423);
#62469=AXIS2_PLACEMENT_3D('',#99310,#71427,#71428);
#62470=AXIS2_PLACEMENT_3D('',#99316,#71432,#71433);
#62471=AXIS2_PLACEMENT_3D('',#99322,#71437,#71438);
#62472=AXIS2_PLACEMENT_3D('',#99328,#71442,#71443);
#62473=AXIS2_PLACEMENT_3D('',#99334,#71447,#71448);
#62474=AXIS2_PLACEMENT_3D('',#99340,#71452,#71453);
#62475=AXIS2_PLACEMENT_3D('',#99346,#71457,#71458);
#62476=AXIS2_PLACEMENT_3D('',#99352,#71462,#71463);
#62477=AXIS2_PLACEMENT_3D('',#99358,#71467,#71468);
#62478=AXIS2_PLACEMENT_3D('',#99364,#71472,#71473);
#62479=AXIS2_PLACEMENT_3D('',#99370,#71477,#71478);
#62480=AXIS2_PLACEMENT_3D('',#99376,#71482,#71483);
#62481=AXIS2_PLACEMENT_3D('',#99382,#71487,#71488);
#62482=AXIS2_PLACEMENT_3D('',#99388,#71492,#71493);
#62483=AXIS2_PLACEMENT_3D('',#99394,#71497,#71498);
#62484=AXIS2_PLACEMENT_3D('',#99400,#71502,#71503);
#62485=AXIS2_PLACEMENT_3D('',#99406,#71507,#71508);
#62486=AXIS2_PLACEMENT_3D('',#99412,#71512,#71513);
#62487=AXIS2_PLACEMENT_3D('',#99418,#71517,#71518);
#62488=AXIS2_PLACEMENT_3D('',#99424,#71522,#71523);
#62489=AXIS2_PLACEMENT_3D('',#99430,#71527,#71528);
#62490=AXIS2_PLACEMENT_3D('',#99436,#71532,#71533);
#62491=AXIS2_PLACEMENT_3D('',#99442,#71537,#71538);
#62492=AXIS2_PLACEMENT_3D('',#99448,#71542,#71543);
#62493=AXIS2_PLACEMENT_3D('',#99454,#71547,#71548);
#62494=AXIS2_PLACEMENT_3D('',#99460,#71552,#71553);
#62495=AXIS2_PLACEMENT_3D('',#99466,#71557,#71558);
#62496=AXIS2_PLACEMENT_3D('',#99472,#71562,#71563);
#62497=AXIS2_PLACEMENT_3D('',#99478,#71567,#71568);
#62498=AXIS2_PLACEMENT_3D('',#99484,#71572,#71573);
#62499=AXIS2_PLACEMENT_3D('',#99490,#71577,#71578);
#62500=AXIS2_PLACEMENT_3D('',#99496,#71582,#71583);
#62501=AXIS2_PLACEMENT_3D('',#99502,#71587,#71588);
#62502=AXIS2_PLACEMENT_3D('',#99508,#71592,#71593);
#62503=AXIS2_PLACEMENT_3D('',#99514,#71597,#71598);
#62504=AXIS2_PLACEMENT_3D('',#99520,#71602,#71603);
#62505=AXIS2_PLACEMENT_3D('',#99526,#71607,#71608);
#62506=AXIS2_PLACEMENT_3D('',#99532,#71612,#71613);
#62507=AXIS2_PLACEMENT_3D('',#99538,#71617,#71618);
#62508=AXIS2_PLACEMENT_3D('',#99544,#71622,#71623);
#62509=AXIS2_PLACEMENT_3D('',#99550,#71627,#71628);
#62510=AXIS2_PLACEMENT_3D('',#99556,#71632,#71633);
#62511=AXIS2_PLACEMENT_3D('',#99562,#71637,#71638);
#62512=AXIS2_PLACEMENT_3D('',#99568,#71642,#71643);
#62513=AXIS2_PLACEMENT_3D('',#99574,#71647,#71648);
#62514=AXIS2_PLACEMENT_3D('',#99580,#71652,#71653);
#62515=AXIS2_PLACEMENT_3D('',#99586,#71657,#71658);
#62516=AXIS2_PLACEMENT_3D('',#99592,#71662,#71663);
#62517=AXIS2_PLACEMENT_3D('',#99598,#71667,#71668);
#62518=AXIS2_PLACEMENT_3D('',#99604,#71672,#71673);
#62519=AXIS2_PLACEMENT_3D('',#99610,#71677,#71678);
#62520=AXIS2_PLACEMENT_3D('',#99616,#71682,#71683);
#62521=AXIS2_PLACEMENT_3D('',#99622,#71687,#71688);
#62522=AXIS2_PLACEMENT_3D('',#99628,#71692,#71693);
#62523=AXIS2_PLACEMENT_3D('',#99634,#71697,#71698);
#62524=AXIS2_PLACEMENT_3D('',#99640,#71702,#71703);
#62525=AXIS2_PLACEMENT_3D('',#99646,#71707,#71708);
#62526=AXIS2_PLACEMENT_3D('',#99652,#71712,#71713);
#62527=AXIS2_PLACEMENT_3D('',#99658,#71717,#71718);
#62528=AXIS2_PLACEMENT_3D('',#99664,#71722,#71723);
#62529=AXIS2_PLACEMENT_3D('',#99670,#71727,#71728);
#62530=AXIS2_PLACEMENT_3D('',#99676,#71732,#71733);
#62531=AXIS2_PLACEMENT_3D('',#99682,#71737,#71738);
#62532=AXIS2_PLACEMENT_3D('',#99688,#71742,#71743);
#62533=AXIS2_PLACEMENT_3D('',#99694,#71747,#71748);
#62534=AXIS2_PLACEMENT_3D('',#99700,#71752,#71753);
#62535=AXIS2_PLACEMENT_3D('',#99706,#71757,#71758);
#62536=AXIS2_PLACEMENT_3D('',#99712,#71762,#71763);
#62537=AXIS2_PLACEMENT_3D('',#99718,#71767,#71768);
#62538=AXIS2_PLACEMENT_3D('',#99724,#71772,#71773);
#62539=AXIS2_PLACEMENT_3D('',#99730,#71777,#71778);
#62540=AXIS2_PLACEMENT_3D('',#99736,#71782,#71783);
#62541=AXIS2_PLACEMENT_3D('',#99742,#71787,#71788);
#62542=AXIS2_PLACEMENT_3D('',#99748,#71792,#71793);
#62543=AXIS2_PLACEMENT_3D('',#99754,#71797,#71798);
#62544=AXIS2_PLACEMENT_3D('',#99760,#71802,#71803);
#62545=AXIS2_PLACEMENT_3D('',#99766,#71807,#71808);
#62546=AXIS2_PLACEMENT_3D('',#99772,#71812,#71813);
#62547=AXIS2_PLACEMENT_3D('',#99778,#71817,#71818);
#62548=AXIS2_PLACEMENT_3D('',#99784,#71822,#71823);
#62549=AXIS2_PLACEMENT_3D('',#99790,#71827,#71828);
#62550=AXIS2_PLACEMENT_3D('',#99796,#71832,#71833);
#62551=AXIS2_PLACEMENT_3D('',#99802,#71837,#71838);
#62552=AXIS2_PLACEMENT_3D('',#99808,#71842,#71843);
#62553=AXIS2_PLACEMENT_3D('',#99814,#71847,#71848);
#62554=AXIS2_PLACEMENT_3D('',#99820,#71852,#71853);
#62555=AXIS2_PLACEMENT_3D('',#99826,#71857,#71858);
#62556=AXIS2_PLACEMENT_3D('',#99832,#71862,#71863);
#62557=AXIS2_PLACEMENT_3D('',#99838,#71867,#71868);
#62558=AXIS2_PLACEMENT_3D('',#99844,#71872,#71873);
#62559=AXIS2_PLACEMENT_3D('',#99850,#71877,#71878);
#62560=AXIS2_PLACEMENT_3D('',#99856,#71882,#71883);
#62561=AXIS2_PLACEMENT_3D('',#99862,#71887,#71888);
#62562=AXIS2_PLACEMENT_3D('',#99868,#71892,#71893);
#62563=AXIS2_PLACEMENT_3D('',#99874,#71897,#71898);
#62564=AXIS2_PLACEMENT_3D('',#99880,#71902,#71903);
#62565=AXIS2_PLACEMENT_3D('',#99886,#71907,#71908);
#62566=AXIS2_PLACEMENT_3D('',#99892,#71912,#71913);
#62567=AXIS2_PLACEMENT_3D('',#99898,#71917,#71918);
#62568=AXIS2_PLACEMENT_3D('',#99904,#71922,#71923);
#62569=AXIS2_PLACEMENT_3D('',#99910,#71927,#71928);
#62570=AXIS2_PLACEMENT_3D('',#99916,#71932,#71933);
#62571=AXIS2_PLACEMENT_3D('',#99922,#71937,#71938);
#62572=AXIS2_PLACEMENT_3D('',#99928,#71942,#71943);
#62573=AXIS2_PLACEMENT_3D('',#99934,#71947,#71948);
#62574=AXIS2_PLACEMENT_3D('',#99940,#71952,#71953);
#62575=AXIS2_PLACEMENT_3D('',#99946,#71957,#71958);
#62576=AXIS2_PLACEMENT_3D('',#99952,#71962,#71963);
#62577=AXIS2_PLACEMENT_3D('',#99958,#71967,#71968);
#62578=AXIS2_PLACEMENT_3D('',#99964,#71972,#71973);
#62579=AXIS2_PLACEMENT_3D('',#99970,#71977,#71978);
#62580=AXIS2_PLACEMENT_3D('',#99976,#71982,#71983);
#62581=AXIS2_PLACEMENT_3D('',#99982,#71987,#71988);
#62582=AXIS2_PLACEMENT_3D('',#99988,#71992,#71993);
#62583=AXIS2_PLACEMENT_3D('',#99994,#71997,#71998);
#62584=AXIS2_PLACEMENT_3D('',#100000,#72002,#72003);
#62585=AXIS2_PLACEMENT_3D('',#100006,#72007,#72008);
#62586=AXIS2_PLACEMENT_3D('',#100012,#72012,#72013);
#62587=AXIS2_PLACEMENT_3D('',#100018,#72017,#72018);
#62588=AXIS2_PLACEMENT_3D('',#100024,#72022,#72023);
#62589=AXIS2_PLACEMENT_3D('',#100030,#72027,#72028);
#62590=AXIS2_PLACEMENT_3D('',#100036,#72032,#72033);
#62591=AXIS2_PLACEMENT_3D('',#100042,#72037,#72038);
#62592=AXIS2_PLACEMENT_3D('',#100048,#72042,#72043);
#62593=AXIS2_PLACEMENT_3D('',#100054,#72047,#72048);
#62594=AXIS2_PLACEMENT_3D('',#100060,#72052,#72053);
#62595=AXIS2_PLACEMENT_3D('',#100066,#72057,#72058);
#62596=AXIS2_PLACEMENT_3D('',#100072,#72062,#72063);
#62597=AXIS2_PLACEMENT_3D('',#100078,#72067,#72068);
#62598=AXIS2_PLACEMENT_3D('',#100084,#72072,#72073);
#62599=AXIS2_PLACEMENT_3D('',#100090,#72077,#72078);
#62600=AXIS2_PLACEMENT_3D('',#100096,#72082,#72083);
#62601=AXIS2_PLACEMENT_3D('',#100102,#72087,#72088);
#62602=AXIS2_PLACEMENT_3D('',#100108,#72092,#72093);
#62603=AXIS2_PLACEMENT_3D('',#100114,#72097,#72098);
#62604=AXIS2_PLACEMENT_3D('',#100120,#72102,#72103);
#62605=AXIS2_PLACEMENT_3D('',#100126,#72107,#72108);
#62606=AXIS2_PLACEMENT_3D('',#100132,#72112,#72113);
#62607=AXIS2_PLACEMENT_3D('',#100138,#72117,#72118);
#62608=AXIS2_PLACEMENT_3D('',#100144,#72122,#72123);
#62609=AXIS2_PLACEMENT_3D('',#100150,#72127,#72128);
#62610=AXIS2_PLACEMENT_3D('',#100156,#72132,#72133);
#62611=AXIS2_PLACEMENT_3D('',#100162,#72137,#72138);
#62612=AXIS2_PLACEMENT_3D('',#100168,#72142,#72143);
#62613=AXIS2_PLACEMENT_3D('',#100174,#72147,#72148);
#62614=AXIS2_PLACEMENT_3D('',#100180,#72152,#72153);
#62615=AXIS2_PLACEMENT_3D('',#100186,#72157,#72158);
#62616=AXIS2_PLACEMENT_3D('',#100192,#72162,#72163);
#62617=AXIS2_PLACEMENT_3D('',#100198,#72167,#72168);
#62618=AXIS2_PLACEMENT_3D('',#100204,#72172,#72173);
#62619=AXIS2_PLACEMENT_3D('',#100210,#72177,#72178);
#62620=AXIS2_PLACEMENT_3D('',#100216,#72182,#72183);
#62621=AXIS2_PLACEMENT_3D('',#100222,#72187,#72188);
#62622=AXIS2_PLACEMENT_3D('',#100228,#72192,#72193);
#62623=AXIS2_PLACEMENT_3D('',#100234,#72197,#72198);
#62624=AXIS2_PLACEMENT_3D('',#100240,#72202,#72203);
#62625=AXIS2_PLACEMENT_3D('',#100246,#72207,#72208);
#62626=AXIS2_PLACEMENT_3D('',#100252,#72212,#72213);
#62627=AXIS2_PLACEMENT_3D('',#100258,#72217,#72218);
#62628=AXIS2_PLACEMENT_3D('',#100264,#72222,#72223);
#62629=AXIS2_PLACEMENT_3D('',#100270,#72227,#72228);
#62630=AXIS2_PLACEMENT_3D('',#100276,#72232,#72233);
#62631=AXIS2_PLACEMENT_3D('',#100282,#72237,#72238);
#62632=AXIS2_PLACEMENT_3D('',#100288,#72242,#72243);
#62633=AXIS2_PLACEMENT_3D('',#100294,#72247,#72248);
#62634=AXIS2_PLACEMENT_3D('',#100300,#72252,#72253);
#62635=AXIS2_PLACEMENT_3D('',#100306,#72257,#72258);
#62636=AXIS2_PLACEMENT_3D('',#100312,#72262,#72263);
#62637=AXIS2_PLACEMENT_3D('',#100318,#72267,#72268);
#62638=AXIS2_PLACEMENT_3D('',#100324,#72272,#72273);
#62639=AXIS2_PLACEMENT_3D('',#100330,#72277,#72278);
#62640=AXIS2_PLACEMENT_3D('',#100336,#72282,#72283);
#62641=AXIS2_PLACEMENT_3D('',#100342,#72287,#72288);
#62642=AXIS2_PLACEMENT_3D('',#100348,#72292,#72293);
#62643=AXIS2_PLACEMENT_3D('',#100354,#72297,#72298);
#62644=AXIS2_PLACEMENT_3D('',#100360,#72302,#72303);
#62645=AXIS2_PLACEMENT_3D('',#100366,#72307,#72308);
#62646=AXIS2_PLACEMENT_3D('',#100372,#72312,#72313);
#62647=AXIS2_PLACEMENT_3D('',#100378,#72317,#72318);
#62648=AXIS2_PLACEMENT_3D('',#100384,#72322,#72323);
#62649=AXIS2_PLACEMENT_3D('',#100390,#72327,#72328);
#62650=AXIS2_PLACEMENT_3D('',#100396,#72332,#72333);
#62651=AXIS2_PLACEMENT_3D('',#100402,#72337,#72338);
#62652=AXIS2_PLACEMENT_3D('',#100408,#72342,#72343);
#62653=AXIS2_PLACEMENT_3D('',#100414,#72347,#72348);
#62654=AXIS2_PLACEMENT_3D('',#100420,#72352,#72353);
#62655=AXIS2_PLACEMENT_3D('',#100426,#72357,#72358);
#62656=AXIS2_PLACEMENT_3D('',#100432,#72362,#72363);
#62657=AXIS2_PLACEMENT_3D('',#100438,#72367,#72368);
#62658=AXIS2_PLACEMENT_3D('',#100444,#72372,#72373);
#62659=AXIS2_PLACEMENT_3D('',#100450,#72377,#72378);
#62660=AXIS2_PLACEMENT_3D('',#100456,#72382,#72383);
#62661=AXIS2_PLACEMENT_3D('',#100462,#72387,#72388);
#62662=AXIS2_PLACEMENT_3D('',#100468,#72392,#72393);
#62663=AXIS2_PLACEMENT_3D('',#100474,#72397,#72398);
#62664=AXIS2_PLACEMENT_3D('',#100480,#72402,#72403);
#62665=AXIS2_PLACEMENT_3D('',#100486,#72407,#72408);
#62666=AXIS2_PLACEMENT_3D('',#100492,#72412,#72413);
#62667=AXIS2_PLACEMENT_3D('',#100498,#72417,#72418);
#62668=AXIS2_PLACEMENT_3D('',#100504,#72422,#72423);
#62669=AXIS2_PLACEMENT_3D('',#100510,#72427,#72428);
#62670=AXIS2_PLACEMENT_3D('',#100516,#72432,#72433);
#62671=AXIS2_PLACEMENT_3D('',#100522,#72437,#72438);
#62672=AXIS2_PLACEMENT_3D('',#100528,#72442,#72443);
#62673=AXIS2_PLACEMENT_3D('',#100534,#72447,#72448);
#62674=AXIS2_PLACEMENT_3D('',#100540,#72452,#72453);
#62675=AXIS2_PLACEMENT_3D('',#100546,#72457,#72458);
#62676=AXIS2_PLACEMENT_3D('',#100552,#72462,#72463);
#62677=AXIS2_PLACEMENT_3D('',#100558,#72467,#72468);
#62678=AXIS2_PLACEMENT_3D('',#100564,#72472,#72473);
#62679=AXIS2_PLACEMENT_3D('',#100570,#72477,#72478);
#62680=AXIS2_PLACEMENT_3D('',#100576,#72482,#72483);
#62681=AXIS2_PLACEMENT_3D('',#100582,#72487,#72488);
#62682=AXIS2_PLACEMENT_3D('',#100588,#72492,#72493);
#62683=AXIS2_PLACEMENT_3D('',#100594,#72497,#72498);
#62684=AXIS2_PLACEMENT_3D('',#100600,#72502,#72503);
#62685=AXIS2_PLACEMENT_3D('',#100606,#72507,#72508);
#62686=AXIS2_PLACEMENT_3D('',#100612,#72512,#72513);
#62687=AXIS2_PLACEMENT_3D('',#100618,#72517,#72518);
#62688=AXIS2_PLACEMENT_3D('',#100624,#72522,#72523);
#62689=AXIS2_PLACEMENT_3D('',#100630,#72527,#72528);
#62690=AXIS2_PLACEMENT_3D('',#100636,#72532,#72533);
#62691=AXIS2_PLACEMENT_3D('',#100642,#72537,#72538);
#62692=AXIS2_PLACEMENT_3D('',#100648,#72542,#72543);
#62693=AXIS2_PLACEMENT_3D('',#100654,#72547,#72548);
#62694=AXIS2_PLACEMENT_3D('',#100660,#72552,#72553);
#62695=AXIS2_PLACEMENT_3D('',#100666,#72557,#72558);
#62696=AXIS2_PLACEMENT_3D('',#100672,#72562,#72563);
#62697=AXIS2_PLACEMENT_3D('',#100678,#72567,#72568);
#62698=AXIS2_PLACEMENT_3D('',#100684,#72572,#72573);
#62699=AXIS2_PLACEMENT_3D('',#100690,#72577,#72578);
#62700=AXIS2_PLACEMENT_3D('',#100696,#72582,#72583);
#62701=AXIS2_PLACEMENT_3D('',#100702,#72587,#72588);
#62702=AXIS2_PLACEMENT_3D('',#100708,#72592,#72593);
#62703=AXIS2_PLACEMENT_3D('',#100714,#72597,#72598);
#62704=AXIS2_PLACEMENT_3D('',#100720,#72602,#72603);
#62705=AXIS2_PLACEMENT_3D('',#100726,#72607,#72608);
#62706=AXIS2_PLACEMENT_3D('',#100732,#72612,#72613);
#62707=AXIS2_PLACEMENT_3D('',#100738,#72617,#72618);
#62708=AXIS2_PLACEMENT_3D('',#100744,#72622,#72623);
#62709=AXIS2_PLACEMENT_3D('',#100750,#72627,#72628);
#62710=AXIS2_PLACEMENT_3D('',#100756,#72632,#72633);
#62711=AXIS2_PLACEMENT_3D('',#100762,#72637,#72638);
#62712=AXIS2_PLACEMENT_3D('',#100768,#72642,#72643);
#62713=AXIS2_PLACEMENT_3D('',#100774,#72647,#72648);
#62714=AXIS2_PLACEMENT_3D('',#100780,#72652,#72653);
#62715=AXIS2_PLACEMENT_3D('',#100786,#72657,#72658);
#62716=AXIS2_PLACEMENT_3D('',#100792,#72662,#72663);
#62717=AXIS2_PLACEMENT_3D('',#100798,#72667,#72668);
#62718=AXIS2_PLACEMENT_3D('',#100804,#72672,#72673);
#62719=AXIS2_PLACEMENT_3D('',#100810,#72677,#72678);
#62720=AXIS2_PLACEMENT_3D('',#100816,#72682,#72683);
#62721=AXIS2_PLACEMENT_3D('',#100822,#72687,#72688);
#62722=AXIS2_PLACEMENT_3D('',#100828,#72692,#72693);
#62723=AXIS2_PLACEMENT_3D('',#100834,#72697,#72698);
#62724=AXIS2_PLACEMENT_3D('',#100840,#72702,#72703);
#62725=AXIS2_PLACEMENT_3D('',#100846,#72707,#72708);
#62726=AXIS2_PLACEMENT_3D('',#100852,#72712,#72713);
#62727=AXIS2_PLACEMENT_3D('',#100858,#72717,#72718);
#62728=AXIS2_PLACEMENT_3D('',#100864,#72722,#72723);
#62729=AXIS2_PLACEMENT_3D('',#100870,#72727,#72728);
#62730=AXIS2_PLACEMENT_3D('',#100876,#72732,#72733);
#62731=AXIS2_PLACEMENT_3D('',#100882,#72737,#72738);
#62732=AXIS2_PLACEMENT_3D('',#100888,#72742,#72743);
#62733=AXIS2_PLACEMENT_3D('',#100894,#72747,#72748);
#62734=AXIS2_PLACEMENT_3D('',#100900,#72752,#72753);
#62735=AXIS2_PLACEMENT_3D('',#100906,#72757,#72758);
#62736=AXIS2_PLACEMENT_3D('',#100912,#72762,#72763);
#62737=AXIS2_PLACEMENT_3D('',#100918,#72767,#72768);
#62738=AXIS2_PLACEMENT_3D('',#100924,#72772,#72773);
#62739=AXIS2_PLACEMENT_3D('',#100930,#72777,#72778);
#62740=AXIS2_PLACEMENT_3D('',#100936,#72782,#72783);
#62741=AXIS2_PLACEMENT_3D('',#100942,#72787,#72788);
#62742=AXIS2_PLACEMENT_3D('',#100948,#72792,#72793);
#62743=AXIS2_PLACEMENT_3D('',#100954,#72797,#72798);
#62744=AXIS2_PLACEMENT_3D('',#100960,#72802,#72803);
#62745=AXIS2_PLACEMENT_3D('',#100966,#72807,#72808);
#62746=AXIS2_PLACEMENT_3D('',#100972,#72812,#72813);
#62747=AXIS2_PLACEMENT_3D('',#100978,#72817,#72818);
#62748=AXIS2_PLACEMENT_3D('',#100984,#72822,#72823);
#62749=AXIS2_PLACEMENT_3D('',#100990,#72827,#72828);
#62750=AXIS2_PLACEMENT_3D('',#100996,#72832,#72833);
#62751=AXIS2_PLACEMENT_3D('',#101002,#72837,#72838);
#62752=AXIS2_PLACEMENT_3D('',#101008,#72842,#72843);
#62753=AXIS2_PLACEMENT_3D('',#101014,#72847,#72848);
#62754=AXIS2_PLACEMENT_3D('',#101020,#72852,#72853);
#62755=AXIS2_PLACEMENT_3D('',#101026,#72857,#72858);
#62756=AXIS2_PLACEMENT_3D('',#101032,#72862,#72863);
#62757=AXIS2_PLACEMENT_3D('',#101038,#72867,#72868);
#62758=AXIS2_PLACEMENT_3D('',#101044,#72872,#72873);
#62759=AXIS2_PLACEMENT_3D('',#101050,#72877,#72878);
#62760=AXIS2_PLACEMENT_3D('',#101056,#72882,#72883);
#62761=AXIS2_PLACEMENT_3D('',#101062,#72887,#72888);
#62762=AXIS2_PLACEMENT_3D('',#101068,#72892,#72893);
#62763=AXIS2_PLACEMENT_3D('',#101074,#72897,#72898);
#62764=AXIS2_PLACEMENT_3D('',#101080,#72902,#72903);
#62765=AXIS2_PLACEMENT_3D('',#101086,#72907,#72908);
#62766=AXIS2_PLACEMENT_3D('',#101092,#72912,#72913);
#62767=AXIS2_PLACEMENT_3D('',#101098,#72917,#72918);
#62768=AXIS2_PLACEMENT_3D('',#101104,#72922,#72923);
#62769=AXIS2_PLACEMENT_3D('',#101110,#72927,#72928);
#62770=AXIS2_PLACEMENT_3D('',#101116,#72932,#72933);
#62771=AXIS2_PLACEMENT_3D('',#101122,#72937,#72938);
#62772=AXIS2_PLACEMENT_3D('',#101128,#72942,#72943);
#62773=AXIS2_PLACEMENT_3D('',#101134,#72947,#72948);
#62774=AXIS2_PLACEMENT_3D('',#101140,#72952,#72953);
#62775=AXIS2_PLACEMENT_3D('',#101146,#72957,#72958);
#62776=AXIS2_PLACEMENT_3D('',#101152,#72962,#72963);
#62777=AXIS2_PLACEMENT_3D('',#101158,#72967,#72968);
#62778=AXIS2_PLACEMENT_3D('',#101164,#72972,#72973);
#62779=AXIS2_PLACEMENT_3D('',#101170,#72977,#72978);
#62780=AXIS2_PLACEMENT_3D('',#101176,#72982,#72983);
#62781=AXIS2_PLACEMENT_3D('',#101182,#72987,#72988);
#62782=AXIS2_PLACEMENT_3D('',#101188,#72992,#72993);
#62783=AXIS2_PLACEMENT_3D('',#101194,#72997,#72998);
#62784=AXIS2_PLACEMENT_3D('',#101200,#73002,#73003);
#62785=AXIS2_PLACEMENT_3D('',#101206,#73007,#73008);
#62786=AXIS2_PLACEMENT_3D('',#101212,#73012,#73013);
#62787=AXIS2_PLACEMENT_3D('',#101218,#73017,#73018);
#62788=AXIS2_PLACEMENT_3D('',#101224,#73022,#73023);
#62789=AXIS2_PLACEMENT_3D('',#101230,#73027,#73028);
#62790=AXIS2_PLACEMENT_3D('',#101236,#73032,#73033);
#62791=AXIS2_PLACEMENT_3D('',#101242,#73037,#73038);
#62792=AXIS2_PLACEMENT_3D('',#101248,#73042,#73043);
#62793=AXIS2_PLACEMENT_3D('',#101254,#73047,#73048);
#62794=AXIS2_PLACEMENT_3D('',#101260,#73052,#73053);
#62795=AXIS2_PLACEMENT_3D('',#101266,#73057,#73058);
#62796=AXIS2_PLACEMENT_3D('',#101272,#73062,#73063);
#62797=AXIS2_PLACEMENT_3D('',#101278,#73067,#73068);
#62798=AXIS2_PLACEMENT_3D('',#101284,#73072,#73073);
#62799=AXIS2_PLACEMENT_3D('',#101290,#73077,#73078);
#62800=AXIS2_PLACEMENT_3D('',#101296,#73082,#73083);
#62801=AXIS2_PLACEMENT_3D('',#101302,#73087,#73088);
#62802=AXIS2_PLACEMENT_3D('',#101308,#73092,#73093);
#62803=AXIS2_PLACEMENT_3D('',#101314,#73097,#73098);
#62804=AXIS2_PLACEMENT_3D('',#101320,#73102,#73103);
#62805=AXIS2_PLACEMENT_3D('',#101326,#73107,#73108);
#62806=AXIS2_PLACEMENT_3D('',#101332,#73112,#73113);
#62807=AXIS2_PLACEMENT_3D('',#101338,#73117,#73118);
#62808=AXIS2_PLACEMENT_3D('',#101344,#73122,#73123);
#62809=AXIS2_PLACEMENT_3D('',#101350,#73127,#73128);
#62810=AXIS2_PLACEMENT_3D('',#101356,#73132,#73133);
#62811=AXIS2_PLACEMENT_3D('',#101362,#73137,#73138);
#62812=AXIS2_PLACEMENT_3D('',#101368,#73142,#73143);
#62813=AXIS2_PLACEMENT_3D('',#101374,#73147,#73148);
#62814=AXIS2_PLACEMENT_3D('',#101380,#73152,#73153);
#62815=AXIS2_PLACEMENT_3D('',#101386,#73157,#73158);
#62816=AXIS2_PLACEMENT_3D('',#101392,#73162,#73163);
#62817=AXIS2_PLACEMENT_3D('',#101398,#73167,#73168);
#62818=AXIS2_PLACEMENT_3D('',#101404,#73172,#73173);
#62819=AXIS2_PLACEMENT_3D('',#101410,#73177,#73178);
#62820=AXIS2_PLACEMENT_3D('',#101416,#73182,#73183);
#62821=AXIS2_PLACEMENT_3D('',#101422,#73187,#73188);
#62822=AXIS2_PLACEMENT_3D('',#101428,#73192,#73193);
#62823=AXIS2_PLACEMENT_3D('',#101434,#73197,#73198);
#62824=AXIS2_PLACEMENT_3D('',#101440,#73202,#73203);
#62825=AXIS2_PLACEMENT_3D('',#101446,#73207,#73208);
#62826=AXIS2_PLACEMENT_3D('',#101452,#73212,#73213);
#62827=AXIS2_PLACEMENT_3D('',#101458,#73217,#73218);
#62828=AXIS2_PLACEMENT_3D('',#101464,#73222,#73223);
#62829=AXIS2_PLACEMENT_3D('',#101470,#73227,#73228);
#62830=AXIS2_PLACEMENT_3D('',#101476,#73232,#73233);
#62831=AXIS2_PLACEMENT_3D('',#101482,#73237,#73238);
#62832=AXIS2_PLACEMENT_3D('',#101488,#73242,#73243);
#62833=AXIS2_PLACEMENT_3D('',#101494,#73247,#73248);
#62834=AXIS2_PLACEMENT_3D('',#101500,#73252,#73253);
#62835=AXIS2_PLACEMENT_3D('',#101506,#73257,#73258);
#62836=AXIS2_PLACEMENT_3D('',#101512,#73262,#73263);
#62837=AXIS2_PLACEMENT_3D('',#101518,#73267,#73268);
#62838=AXIS2_PLACEMENT_3D('',#101524,#73272,#73273);
#62839=AXIS2_PLACEMENT_3D('',#101530,#73277,#73278);
#62840=AXIS2_PLACEMENT_3D('',#101536,#73282,#73283);
#62841=AXIS2_PLACEMENT_3D('',#101542,#73287,#73288);
#62842=AXIS2_PLACEMENT_3D('',#101548,#73292,#73293);
#62843=AXIS2_PLACEMENT_3D('',#101554,#73297,#73298);
#62844=AXIS2_PLACEMENT_3D('',#101560,#73302,#73303);
#62845=AXIS2_PLACEMENT_3D('',#101566,#73307,#73308);
#62846=AXIS2_PLACEMENT_3D('',#101572,#73312,#73313);
#62847=AXIS2_PLACEMENT_3D('',#101578,#73317,#73318);
#62848=AXIS2_PLACEMENT_3D('',#101584,#73322,#73323);
#62849=AXIS2_PLACEMENT_3D('',#101590,#73327,#73328);
#62850=AXIS2_PLACEMENT_3D('',#101596,#73332,#73333);
#62851=AXIS2_PLACEMENT_3D('',#101602,#73337,#73338);
#62852=AXIS2_PLACEMENT_3D('',#101608,#73342,#73343);
#62853=AXIS2_PLACEMENT_3D('',#101614,#73347,#73348);
#62854=AXIS2_PLACEMENT_3D('',#101620,#73352,#73353);
#62855=AXIS2_PLACEMENT_3D('',#101626,#73357,#73358);
#62856=AXIS2_PLACEMENT_3D('',#101632,#73362,#73363);
#62857=AXIS2_PLACEMENT_3D('',#101638,#73367,#73368);
#62858=AXIS2_PLACEMENT_3D('',#101644,#73372,#73373);
#62859=AXIS2_PLACEMENT_3D('',#101650,#73377,#73378);
#62860=AXIS2_PLACEMENT_3D('',#101656,#73382,#73383);
#62861=AXIS2_PLACEMENT_3D('',#101662,#73387,#73388);
#62862=AXIS2_PLACEMENT_3D('',#101668,#73392,#73393);
#62863=AXIS2_PLACEMENT_3D('',#101674,#73397,#73398);
#62864=AXIS2_PLACEMENT_3D('',#101680,#73402,#73403);
#62865=AXIS2_PLACEMENT_3D('',#101686,#73407,#73408);
#62866=AXIS2_PLACEMENT_3D('',#101692,#73412,#73413);
#62867=AXIS2_PLACEMENT_3D('',#101698,#73417,#73418);
#62868=AXIS2_PLACEMENT_3D('',#101704,#73422,#73423);
#62869=AXIS2_PLACEMENT_3D('',#101710,#73427,#73428);
#62870=AXIS2_PLACEMENT_3D('',#101716,#73432,#73433);
#62871=AXIS2_PLACEMENT_3D('',#101722,#73437,#73438);
#62872=AXIS2_PLACEMENT_3D('',#101728,#73442,#73443);
#62873=AXIS2_PLACEMENT_3D('',#101734,#73447,#73448);
#62874=AXIS2_PLACEMENT_3D('',#101740,#73452,#73453);
#62875=AXIS2_PLACEMENT_3D('',#101746,#73457,#73458);
#62876=AXIS2_PLACEMENT_3D('',#101752,#73462,#73463);
#62877=AXIS2_PLACEMENT_3D('',#101758,#73467,#73468);
#62878=AXIS2_PLACEMENT_3D('',#101764,#73472,#73473);
#62879=AXIS2_PLACEMENT_3D('',#101770,#73477,#73478);
#62880=AXIS2_PLACEMENT_3D('',#101776,#73482,#73483);
#62881=AXIS2_PLACEMENT_3D('',#101782,#73487,#73488);
#62882=AXIS2_PLACEMENT_3D('',#101788,#73492,#73493);
#62883=AXIS2_PLACEMENT_3D('',#101794,#73497,#73498);
#62884=AXIS2_PLACEMENT_3D('',#101800,#73502,#73503);
#62885=AXIS2_PLACEMENT_3D('',#101806,#73507,#73508);
#62886=AXIS2_PLACEMENT_3D('',#101812,#73512,#73513);
#62887=AXIS2_PLACEMENT_3D('',#101818,#73517,#73518);
#62888=AXIS2_PLACEMENT_3D('',#101824,#73522,#73523);
#62889=AXIS2_PLACEMENT_3D('',#101830,#73527,#73528);
#62890=AXIS2_PLACEMENT_3D('',#101836,#73532,#73533);
#62891=AXIS2_PLACEMENT_3D('',#101842,#73537,#73538);
#62892=AXIS2_PLACEMENT_3D('',#101848,#73542,#73543);
#62893=AXIS2_PLACEMENT_3D('',#101854,#73547,#73548);
#62894=AXIS2_PLACEMENT_3D('',#101860,#73552,#73553);
#62895=AXIS2_PLACEMENT_3D('',#101866,#73557,#73558);
#62896=AXIS2_PLACEMENT_3D('',#101872,#73562,#73563);
#62897=AXIS2_PLACEMENT_3D('',#101878,#73567,#73568);
#62898=AXIS2_PLACEMENT_3D('',#101884,#73572,#73573);
#62899=AXIS2_PLACEMENT_3D('',#101890,#73577,#73578);
#62900=AXIS2_PLACEMENT_3D('',#101896,#73582,#73583);
#62901=AXIS2_PLACEMENT_3D('',#101902,#73587,#73588);
#62902=AXIS2_PLACEMENT_3D('',#101908,#73592,#73593);
#62903=AXIS2_PLACEMENT_3D('',#101914,#73597,#73598);
#62904=AXIS2_PLACEMENT_3D('',#101920,#73602,#73603);
#62905=AXIS2_PLACEMENT_3D('',#101926,#73607,#73608);
#62906=AXIS2_PLACEMENT_3D('',#101932,#73612,#73613);
#62907=AXIS2_PLACEMENT_3D('',#101938,#73617,#73618);
#62908=AXIS2_PLACEMENT_3D('',#101944,#73622,#73623);
#62909=AXIS2_PLACEMENT_3D('',#101950,#73627,#73628);
#62910=AXIS2_PLACEMENT_3D('',#101956,#73632,#73633);
#62911=AXIS2_PLACEMENT_3D('',#101962,#73637,#73638);
#62912=AXIS2_PLACEMENT_3D('',#101968,#73642,#73643);
#62913=AXIS2_PLACEMENT_3D('',#101974,#73647,#73648);
#62914=AXIS2_PLACEMENT_3D('',#101980,#73652,#73653);
#62915=AXIS2_PLACEMENT_3D('',#101986,#73657,#73658);
#62916=AXIS2_PLACEMENT_3D('',#101992,#73662,#73663);
#62917=AXIS2_PLACEMENT_3D('',#101998,#73667,#73668);
#62918=AXIS2_PLACEMENT_3D('',#102004,#73672,#73673);
#62919=AXIS2_PLACEMENT_3D('',#102010,#73677,#73678);
#62920=AXIS2_PLACEMENT_3D('',#102013,#73681,#73682);
#62921=AXIS2_PLACEMENT_3D('',#102016,#73685,#73686);
#62922=AXIS2_PLACEMENT_3D('',#102017,#73687,#73688);
#62923=AXIS2_PLACEMENT_3D('',#102018,#73689,#73690);
#62924=AXIS2_PLACEMENT_3D('',#102019,#73691,#73692);
#62925=AXIS2_PLACEMENT_3D('',#102022,#73693,#73694);
#62926=AXIS2_PLACEMENT_3D('',#102026,#73696,#73697);
#62927=AXIS2_PLACEMENT_3D('',#102028,#73699,#73700);
#62928=AXIS2_PLACEMENT_3D('',#102030,#73701,#73702);
#62929=AXIS2_PLACEMENT_3D('',#102033,#73704,#73705);
#62930=AXIS2_PLACEMENT_3D('',#102034,#73706,#73707);
#62931=AXIS2_PLACEMENT_3D('',#102036,#73708,#73709);
#62932=AXIS2_PLACEMENT_3D('',#102039,#73711,#73712);
#62933=AXIS2_PLACEMENT_3D('',#102040,#73713,#73714);
#62934=AXIS2_PLACEMENT_3D('',#102050,#73720,#73721);
#62935=AXIS2_PLACEMENT_3D('',#102052,#73722,#73723);
#62936=AXIS2_PLACEMENT_3D('',#102054,#73724,#73725);
#62937=AXIS2_PLACEMENT_3D('',#102056,#73727,#73728);
#62938=AXIS2_PLACEMENT_3D('',#102062,#73732,#73733);
#62939=AXIS2_PLACEMENT_3D('',#102074,#73740,#73741);
#62940=AXIS2_PLACEMENT_3D('',#102076,#73742,#73743);
#62941=AXIS2_PLACEMENT_3D('',#102078,#73744,#73745);
#62942=AXIS2_PLACEMENT_3D('',#102080,#73747,#73748);
#62943=AXIS2_PLACEMENT_3D('',#102085,#73751,#73752);
#62944=AXIS2_PLACEMENT_3D('',#102088,#73754,#73755);
#62945=AXIS2_PLACEMENT_3D('',#102089,#73756,#73757);
#62946=AXIS2_PLACEMENT_3D('',#102091,#73758,#73759);
#62947=AXIS2_PLACEMENT_3D('',#102093,#73761,#73762);
#62948=AXIS2_PLACEMENT_3D('',#102101,#73767,#73768);
#62949=AXIS2_PLACEMENT_3D('',#102105,#73771,#73772);
#62950=AXIS2_PLACEMENT_3D('',#102111,#73776,#73777);
#62951=AXIS2_PLACEMENT_3D('',#102114,#73780,#73781);
#62952=AXIS2_PLACEMENT_3D('',#102115,#73782,#73783);
#62953=AXIS2_PLACEMENT_3D('',#102116,#73784,#73785);
#62954=AXIS2_PLACEMENT_3D('',#102119,#73787,#73788);
#62955=AXIS2_PLACEMENT_3D('',#102120,#73789,#73790);
#62956=AXIS2_PLACEMENT_3D('',#102122,#73792,#73793);
#62957=AXIS2_PLACEMENT_3D('',#102123,#73794,#73795);
#62958=AXIS2_PLACEMENT_3D('',#102124,#73796,#73797);
#62959=AXIS2_PLACEMENT_3D('',#102133,#73802,#73803);
#62960=AXIS2_PLACEMENT_3D('',#102139,#73807,#73808);
#62961=AXIS2_PLACEMENT_3D('',#102143,#73811,#73812);
#62962=AXIS2_PLACEMENT_3D('',#102147,#73815,#73816);
#62963=AXIS2_PLACEMENT_3D('',#102156,#73821,#73822);
#62964=AXIS2_PLACEMENT_3D('',#102162,#73826,#73827);
#62965=AXIS2_PLACEMENT_3D('',#102166,#73830,#73831);
#62966=AXIS2_PLACEMENT_3D('',#102170,#73834,#73835);
#62967=AXIS2_PLACEMENT_3D('',#102179,#73840,#73841);
#62968=AXIS2_PLACEMENT_3D('',#102185,#73845,#73846);
#62969=AXIS2_PLACEMENT_3D('',#102189,#73849,#73850);
#62970=AXIS2_PLACEMENT_3D('',#102193,#73853,#73854);
#62971=AXIS2_PLACEMENT_3D('',#102202,#73859,#73860);
#62972=AXIS2_PLACEMENT_3D('',#102208,#73864,#73865);
#62973=AXIS2_PLACEMENT_3D('',#102212,#73868,#73869);
#62974=AXIS2_PLACEMENT_3D('',#102216,#73872,#73873);
#62975=AXIS2_PLACEMENT_3D('',#102225,#73878,#73879);
#62976=AXIS2_PLACEMENT_3D('',#102231,#73883,#73884);
#62977=AXIS2_PLACEMENT_3D('',#102235,#73887,#73888);
#62978=AXIS2_PLACEMENT_3D('',#102239,#73891,#73892);
#62979=AXIS2_PLACEMENT_3D('',#102248,#73897,#73898);
#62980=AXIS2_PLACEMENT_3D('',#102254,#73902,#73903);
#62981=AXIS2_PLACEMENT_3D('',#102258,#73906,#73907);
#62982=AXIS2_PLACEMENT_3D('',#102262,#73910,#73911);
#62983=AXIS2_PLACEMENT_3D('',#102271,#73916,#73917);
#62984=AXIS2_PLACEMENT_3D('',#102277,#73921,#73922);
#62985=AXIS2_PLACEMENT_3D('',#102281,#73925,#73926);
#62986=AXIS2_PLACEMENT_3D('',#102285,#73929,#73930);
#62987=AXIS2_PLACEMENT_3D('',#102294,#73935,#73936);
#62988=AXIS2_PLACEMENT_3D('',#102300,#73940,#73941);
#62989=AXIS2_PLACEMENT_3D('',#102304,#73944,#73945);
#62990=AXIS2_PLACEMENT_3D('',#102308,#73948,#73949);
#62991=AXIS2_PLACEMENT_3D('',#102319,#73953,#73954);
#62992=AXIS2_PLACEMENT_3D('',#102330,#73958,#73959);
#62993=AXIS2_PLACEMENT_3D('',#102331,#73960,#73961);
#62994=AXIS2_PLACEMENT_3D('',#102333,#73963,#73964);
#62995=AXIS2_PLACEMENT_3D('',#102342,#73969,#73970);
#62996=AXIS2_PLACEMENT_3D('',#102348,#73974,#73975);
#62997=AXIS2_PLACEMENT_3D('',#102352,#73978,#73979);
#62998=AXIS2_PLACEMENT_3D('',#102356,#73982,#73983);
#62999=AXIS2_PLACEMENT_3D('',#102365,#73988,#73989);
#63000=AXIS2_PLACEMENT_3D('',#102371,#73993,#73994);
#63001=AXIS2_PLACEMENT_3D('',#102375,#73997,#73998);
#63002=AXIS2_PLACEMENT_3D('',#102379,#74001,#74002);
#63003=AXIS2_PLACEMENT_3D('',#102388,#74007,#74008);
#63004=AXIS2_PLACEMENT_3D('',#102394,#74012,#74013);
#63005=AXIS2_PLACEMENT_3D('',#102398,#74016,#74017);
#63006=AXIS2_PLACEMENT_3D('',#102402,#74020,#74021);
#63007=AXIS2_PLACEMENT_3D('',#102411,#74026,#74027);
#63008=AXIS2_PLACEMENT_3D('',#102417,#74031,#74032);
#63009=AXIS2_PLACEMENT_3D('',#102421,#74035,#74036);
#63010=AXIS2_PLACEMENT_3D('',#102425,#74039,#74040);
#63011=AXIS2_PLACEMENT_3D('',#102434,#74045,#74046);
#63012=AXIS2_PLACEMENT_3D('',#102440,#74050,#74051);
#63013=AXIS2_PLACEMENT_3D('',#102444,#74054,#74055);
#63014=AXIS2_PLACEMENT_3D('',#102448,#74058,#74059);
#63015=AXIS2_PLACEMENT_3D('',#102457,#74064,#74065);
#63016=AXIS2_PLACEMENT_3D('',#102463,#74069,#74070);
#63017=AXIS2_PLACEMENT_3D('',#102467,#74073,#74074);
#63018=AXIS2_PLACEMENT_3D('',#102471,#74077,#74078);
#63019=AXIS2_PLACEMENT_3D('',#102480,#74083,#74084);
#63020=AXIS2_PLACEMENT_3D('',#102486,#74088,#74089);
#63021=AXIS2_PLACEMENT_3D('',#102490,#74092,#74093);
#63022=AXIS2_PLACEMENT_3D('',#102494,#74096,#74097);
#63023=AXIS2_PLACEMENT_3D('',#102505,#74101,#74102);
#63024=AXIS2_PLACEMENT_3D('',#102516,#74106,#74107);
#63025=AXIS2_PLACEMENT_3D('',#102517,#74108,#74109);
#63026=AXIS2_PLACEMENT_3D('',#102519,#74111,#74112);
#63027=AXIS2_PLACEMENT_3D('',#102522,#74114,#74115);
#63028=AXIS2_PLACEMENT_3D('',#102523,#74116,#74117);
#63029=AXIS2_PLACEMENT_3D('',#102525,#74118,#74119);
#63030=AXIS2_PLACEMENT_3D('',#102527,#74121,#74122);
#63031=AXIS2_PLACEMENT_3D('',#102561,#74144,#74145);
#63032=AXIS2_PLACEMENT_3D('',#102563,#74146,#74147);
#63033=AXIS2_PLACEMENT_3D('',#102566,#74149,#74150);
#63034=AXIS2_PLACEMENT_3D('',#102567,#74151,#74152);
#63035=AXIS2_PLACEMENT_3D('',#102570,#74154,#74155);
#63036=AXIS2_PLACEMENT_3D('',#102572,#74156,#74157);
#63037=AXIS2_PLACEMENT_3D('',#102577,#74158,#74159);
#63038=AXIS2_PLACEMENT_3D('',#102578,#74160,#74161);
#63039=AXIS2_PLACEMENT_3D('',#102581,#74163,#74164);
#63040=AXIS2_PLACEMENT_3D('',#102582,#74165,#74166);
#63041=AXIS2_PLACEMENT_3D('',#102586,#74168,#74169);
#63042=AXIS2_PLACEMENT_3D('',#102588,#74171,#74172);
#63043=AXIS2_PLACEMENT_3D('',#102590,#74173,#74174);
#63044=AXIS2_PLACEMENT_3D('',#102593,#74176,#74177);
#63045=AXIS2_PLACEMENT_3D('',#102594,#74178,#74179);
#63046=AXIS2_PLACEMENT_3D('',#102597,#74181,#74182);
#63047=AXIS2_PLACEMENT_3D('',#102602,#74183,#74184);
#63048=AXIS2_PLACEMENT_3D('',#102603,#74185,#74186);
#63049=AXIS2_PLACEMENT_3D('',#102607,#74188,#74189);
#63050=AXIS2_PLACEMENT_3D('',#102609,#74191,#74192);
#63051=AXIS2_PLACEMENT_3D('',#102612,#74193,#74194);
#63052=AXIS2_PLACEMENT_3D('',#102615,#74197,#74198);
#63053=AXIS2_PLACEMENT_3D('',#102619,#74201,#74202);
#63054=AXIS2_PLACEMENT_3D('',#102621,#74203,#74204);
#63055=AXIS2_PLACEMENT_3D('',#102623,#74206,#74207);
#63056=AXIS2_PLACEMENT_3D('',#102625,#74209,#74210);
#63057=AXIS2_PLACEMENT_3D('',#102627,#74212,#74213);
#63058=AXIS2_PLACEMENT_3D('',#102628,#74214,#74215);
#63059=AXIS2_PLACEMENT_3D('',#102629,#74216,#74217);
#63060=AXIS2_PLACEMENT_3D('',#102645,#74219,#74220);
#63061=AXIS2_PLACEMENT_3D('',#102653,#74221,#74222);
#63062=AXIS2_PLACEMENT_3D('',#102701,#74224,#74225);
#63063=AXIS2_PLACEMENT_3D('',#102749,#74227,#74228);
#63064=AXIS2_PLACEMENT_3D('',#102803,#74230,#74231);
#63065=AXIS2_PLACEMENT_3D('',#102851,#74233,#74234);
#63066=AXIS2_PLACEMENT_3D('',#102905,#74236,#74237);
#63067=AXIS2_PLACEMENT_3D('',#102953,#74239,#74240);
#63068=AXIS2_PLACEMENT_3D('',#103001,#74242,#74243);
#63069=AXIS2_PLACEMENT_3D('',#103055,#74245,#74246);
#63070=AXIS2_PLACEMENT_3D('',#103103,#74248,#74249);
#63071=AXIS2_PLACEMENT_3D('',#103151,#74251,#74252);
#63072=AXIS2_PLACEMENT_3D('',#103166,#74254,#74255);
#63073=AXIS2_PLACEMENT_3D('',#103175,#74256,#74257);
#63074=AXIS2_PLACEMENT_3D('',#103199,#74259,#74260);
#63075=AXIS2_PLACEMENT_3D('',#103224,#74262,#74263);
#63076=AXIS2_PLACEMENT_3D('',#103249,#74265,#74266);
#63077=AXIS2_PLACEMENT_3D('',#103273,#74268,#74269);
#63078=AXIS2_PLACEMENT_3D('',#103298,#74271,#74272);
#63079=AXIS2_PLACEMENT_3D('',#103323,#74274,#74275);
#63080=AXIS2_PLACEMENT_3D('',#103348,#74277,#74278);
#63081=AXIS2_PLACEMENT_3D('',#103373,#74280,#74281);
#63082=AXIS2_PLACEMENT_3D('',#103397,#74283,#74284);
#63083=AXIS2_PLACEMENT_3D('',#103485,#74285,#74286);
#63084=AXIS2_PLACEMENT_3D('',#103487,#74287,#74288);
#63085=AXIS2_PLACEMENT_3D('',#103966,#74289,#74290);
#63086=AXIS2_PLACEMENT_3D('',#103968,#74291,#74292);
#63087=AXIS2_PLACEMENT_3D('',#104055,#74293,#74294);
#63088=AXIS2_PLACEMENT_3D('',#104056,#74295,#74296);
#63089=AXIS2_PLACEMENT_3D('',#104057,#74297,#74298);
#63090=AXIS2_PLACEMENT_3D('',#104361,#74299,#74300);
#63091=AXIS2_PLACEMENT_3D('',#104363,#74301,#74302);
#63092=AXIS2_PLACEMENT_3D('',#104364,#74303,#74304);
#63093=AXIS2_PLACEMENT_3D('',#104365,#74305,#74306);
#63094=AXIS2_PLACEMENT_3D('',#104367,#74307,#74308);
#63095=AXIS2_PLACEMENT_3D('',#104368,#74309,#74310);
#63096=AXIS2_PLACEMENT_3D('',#104369,#74311,#74312);
#63097=AXIS2_PLACEMENT_3D('',#104370,#74313,#74314);
#63098=AXIS2_PLACEMENT_3D('',#104387,#74319,#74320);
#63099=AXIS2_PLACEMENT_3D('',#104404,#74325,#74326);
#63100=AXIS2_PLACEMENT_3D('',#104405,#74327,#74328);
#63101=AXIS2_PLACEMENT_3D('',#104407,#74329,#74330);
#63102=AXIS2_PLACEMENT_3D('',#104408,#74331,#74332);
#63103=AXIS2_PLACEMENT_3D('',#104409,#74333,#74334);
#63104=AXIS2_PLACEMENT_3D('',#104410,#74335,#74336);
#63105=AXIS2_PLACEMENT_3D('',#104411,#74337,#74338);
#63106=AXIS2_PLACEMENT_3D('',#104412,#74339,#74340);
#63107=AXIS2_PLACEMENT_3D('',#104413,#74341,#74342);
#63108=AXIS2_PLACEMENT_3D('',#104414,#74343,#74344);
#63109=AXIS2_PLACEMENT_3D('',#104415,#74345,#74346);
#63110=AXIS2_PLACEMENT_3D('',#104416,#74347,#74348);
#63111=AXIS2_PLACEMENT_3D('',#104417,#74349,#74350);
#63112=AXIS2_PLACEMENT_3D('',#104419,#74352,#74353);
#63113=AXIS2_PLACEMENT_3D('',#104421,#74354,#74355);
#63114=AXIS2_PLACEMENT_3D('',#104423,#74357,#74358);
#63115=AXIS2_PLACEMENT_3D('',#104424,#74359,#74360);
#63116=AXIS2_PLACEMENT_3D('',#104425,#74361,#74362);
#63117=AXIS2_PLACEMENT_3D('',#104441,#74364,#74365);
#63118=AXIS2_PLACEMENT_3D('',#104449,#74366,#74367);
#63119=AXIS2_PLACEMENT_3D('',#104497,#74369,#74370);
#63120=AXIS2_PLACEMENT_3D('',#104545,#74372,#74373);
#63121=AXIS2_PLACEMENT_3D('',#104599,#74375,#74376);
#63122=AXIS2_PLACEMENT_3D('',#104647,#74378,#74379);
#63123=AXIS2_PLACEMENT_3D('',#104662,#74381,#74382);
#63124=AXIS2_PLACEMENT_3D('',#104671,#74383,#74384);
#63125=AXIS2_PLACEMENT_3D('',#104696,#74386,#74387);
#63126=AXIS2_PLACEMENT_3D('',#104721,#74389,#74390);
#63127=AXIS2_PLACEMENT_3D('',#104745,#74392,#74393);
#63128=AXIS2_PLACEMENT_3D('',#104833,#74394,#74395);
#63129=AXIS2_PLACEMENT_3D('',#104835,#74396,#74397);
#63130=AXIS2_PLACEMENT_3D('',#105159,#74398,#74399);
#63131=AXIS2_PLACEMENT_3D('',#105161,#74400,#74401);
#63132=AXIS2_PLACEMENT_3D('',#105162,#74402,#74403);
#63133=AXIS2_PLACEMENT_3D('',#105246,#74404,#74405);
#63134=AXIS2_PLACEMENT_3D('',#105247,#74406,#74407);
#63135=AXIS2_PLACEMENT_3D('',#105399,#74408,#74409);
#63136=AXIS2_PLACEMENT_3D('',#105401,#74410,#74411);
#63137=AXIS2_PLACEMENT_3D('',#105409,#74413,#74414);
#63138=AXIS2_PLACEMENT_3D('',#105419,#74415,#74416);
#63139=AXIS2_PLACEMENT_3D('',#105429,#74417,#74418);
#63140=AXIS2_PLACEMENT_3D('',#105439,#74419,#74420);
#63141=AXIS2_PLACEMENT_3D('',#105449,#74421,#74422);
#63142=AXIS2_PLACEMENT_3D('',#105459,#74423,#74424);
#63143=AXIS2_PLACEMENT_3D('',#105463,#74425,#74426);
#63144=AXIS2_PLACEMENT_3D('',#105468,#74429,#74430);
#63145=AXIS2_PLACEMENT_3D('',#105469,#74431,#74432);
#63146=AXIS2_PLACEMENT_3D('',#105474,#74435,#74436);
#63147=AXIS2_PLACEMENT_3D('',#105475,#74437,#74438);
#63148=AXIS2_PLACEMENT_3D('',#105479,#74440,#74441);
#63149=AXIS2_PLACEMENT_3D('',#105481,#74443,#74444);
#63150=AXIS2_PLACEMENT_3D('',#105486,#74447,#74448);
#63151=AXIS2_PLACEMENT_3D('',#105487,#74449,#74450);
#63152=AXIS2_PLACEMENT_3D('',#105491,#74452,#74453);
#63153=AXIS2_PLACEMENT_3D('',#105493,#74455,#74456);
#63154=AXIS2_PLACEMENT_3D('',#105497,#74458,#74459);
#63155=AXIS2_PLACEMENT_3D('',#105499,#74461,#74462);
#63156=AXIS2_PLACEMENT_3D('',#105506,#74467,#74468);
#63157=AXIS2_PLACEMENT_3D('',#105511,#74472,#74473);
#63158=AXIS2_PLACEMENT_3D('',#105516,#74477,#74478);
#63159=AXIS2_PLACEMENT_3D('',#105517,#74479,#74480);
#63160=AXIS2_PLACEMENT_3D('',#105518,#74481,#74482);
#63161=AXIS2_PLACEMENT_3D('',#105520,#74484,#74485);
#63162=AXIS2_PLACEMENT_3D('',#105521,#74486,#74487);
#63163=AXIS2_PLACEMENT_3D('',#105523,#74489,#74490);
#63164=AXIS2_PLACEMENT_3D('',#105525,#74492,#74493);
#63165=AXIS2_PLACEMENT_3D('',#105528,#74495,#74496);
#63166=AXIS2_PLACEMENT_3D('',#105529,#74497,#74498);
#63167=AXIS2_PLACEMENT_3D('',#105530,#74499,#74500);
#63168=AXIS2_PLACEMENT_3D('',#105531,#74501,#74502);
#63169=AXIS2_PLACEMENT_3D('',#105532,#74503,#74504);
#63170=AXIS2_PLACEMENT_3D('',#105533,#74505,#74506);
#63171=AXIS2_PLACEMENT_3D('',#105534,#74507,#74508);
#63172=AXIS2_PLACEMENT_3D('',#105535,#74509,#74510);
#63173=AXIS2_PLACEMENT_3D('',#105538,#74512,#74513);
#63174=AXIS2_PLACEMENT_3D('',#105539,#74514,#74515);
#63175=AXIS2_PLACEMENT_3D('',#105541,#74517,#74518);
#63176=AXIS2_PLACEMENT_3D('',#105542,#74519,#74520);
#63177=AXIS2_PLACEMENT_3D('',#105545,#74522,#74523);
#63178=AXIS2_PLACEMENT_3D('',#105547,#74525,#74526);
#63179=AXIS2_PLACEMENT_3D('',#105549,#74528,#74529);
#63180=AXIS2_PLACEMENT_3D('',#105550,#74530,#74531);
#63181=AXIS2_PLACEMENT_3D('',#105552,#74532,#74533);
#63182=AXIS2_PLACEMENT_3D('',#105553,#74534,#74535);
#63183=AXIS2_PLACEMENT_3D('',#105555,#74537,#74538);
#63184=AXIS2_PLACEMENT_3D('',#105556,#74539,#74540);
#63185=AXIS2_PLACEMENT_3D('',#105557,#74541,#74542);
#63186=AXIS2_PLACEMENT_3D('',#105559,#74543,#74544);
#63187=AXIS2_PLACEMENT_3D('',#105561,#74546,#74547);
#63188=AXIS2_PLACEMENT_3D('',#105562,#74548,#74549);
#63189=AXIS2_PLACEMENT_3D('',#105563,#74550,#74551);
#63190=AXIS2_PLACEMENT_3D('',#105579,#74553,#74554);
#63191=AXIS2_PLACEMENT_3D('',#105587,#74555,#74556);
#63192=AXIS2_PLACEMENT_3D('',#105635,#74558,#74559);
#63193=AXIS2_PLACEMENT_3D('',#105683,#74561,#74562);
#63194=AXIS2_PLACEMENT_3D('',#105688,#74564,#74565);
#63195=AXIS2_PLACEMENT_3D('',#105736,#74566,#74567);
#63196=AXIS2_PLACEMENT_3D('',#105750,#74569,#74570);
#63197=AXIS2_PLACEMENT_3D('',#105757,#74571,#74572);
#63198=AXIS2_PLACEMENT_3D('',#105782,#74574,#74575);
#63199=AXIS2_PLACEMENT_3D('',#105806,#74577,#74578);
#63200=AXIS2_PLACEMENT_3D('',#105881,#74579,#74580);
#63201=AXIS2_PLACEMENT_3D('',#106149,#74581,#74582);
#63202=AXIS2_PLACEMENT_3D('',#106151,#74583,#74584);
#63203=AXIS2_PLACEMENT_3D('',#106152,#74585,#74586);
#63204=AXIS2_PLACEMENT_3D('',#106230,#74587,#74588);
#63205=AXIS2_PLACEMENT_3D('',#106231,#74589,#74590);
#63206=AXIS2_PLACEMENT_3D('',#106344,#74591,#74592);
#63207=AXIS2_PLACEMENT_3D('',#106346,#74593,#74594);
#63208=AXIS2_PLACEMENT_3D('',#106354,#74596,#74597);
#63209=AXIS2_PLACEMENT_3D('',#106364,#74598,#74599);
#63210=AXIS2_PLACEMENT_3D('',#106374,#74600,#74601);
#63211=AXIS2_PLACEMENT_3D('',#106384,#74602,#74603);
#63212=AXIS2_PLACEMENT_3D('',#106394,#74604,#74605);
#63213=AXIS2_PLACEMENT_3D('',#106404,#74606,#74607);
#63214=AXIS2_PLACEMENT_3D('',#106408,#74608,#74609);
#63215=AXIS2_PLACEMENT_3D('',#106413,#74612,#74613);
#63216=AXIS2_PLACEMENT_3D('',#106414,#74614,#74615);
#63217=AXIS2_PLACEMENT_3D('',#106419,#74618,#74619);
#63218=AXIS2_PLACEMENT_3D('',#106420,#74620,#74621);
#63219=AXIS2_PLACEMENT_3D('',#106424,#74623,#74624);
#63220=AXIS2_PLACEMENT_3D('',#106426,#74626,#74627);
#63221=AXIS2_PLACEMENT_3D('',#106431,#74630,#74631);
#63222=AXIS2_PLACEMENT_3D('',#106432,#74632,#74633);
#63223=AXIS2_PLACEMENT_3D('',#106436,#74635,#74636);
#63224=AXIS2_PLACEMENT_3D('',#106438,#74638,#74639);
#63225=AXIS2_PLACEMENT_3D('',#106442,#74641,#74642);
#63226=AXIS2_PLACEMENT_3D('',#106444,#74644,#74645);
#63227=AXIS2_PLACEMENT_3D('',#106451,#74650,#74651);
#63228=AXIS2_PLACEMENT_3D('',#106456,#74655,#74656);
#63229=AXIS2_PLACEMENT_3D('',#106461,#74660,#74661);
#63230=AXIS2_PLACEMENT_3D('',#106462,#74662,#74663);
#63231=AXIS2_PLACEMENT_3D('',#106463,#74664,#74665);
#63232=AXIS2_PLACEMENT_3D('',#106465,#74667,#74668);
#63233=AXIS2_PLACEMENT_3D('',#106466,#74669,#74670);
#63234=AXIS2_PLACEMENT_3D('',#106468,#74672,#74673);
#63235=AXIS2_PLACEMENT_3D('',#106470,#74675,#74676);
#63236=AXIS2_PLACEMENT_3D('',#106473,#74678,#74679);
#63237=AXIS2_PLACEMENT_3D('',#106474,#74680,#74681);
#63238=AXIS2_PLACEMENT_3D('',#106475,#74682,#74683);
#63239=AXIS2_PLACEMENT_3D('',#106476,#74684,#74685);
#63240=AXIS2_PLACEMENT_3D('',#106477,#74686,#74687);
#63241=AXIS2_PLACEMENT_3D('',#106478,#74688,#74689);
#63242=AXIS2_PLACEMENT_3D('',#106479,#74690,#74691);
#63243=AXIS2_PLACEMENT_3D('',#106480,#74692,#74693);
#63244=AXIS2_PLACEMENT_3D('',#106483,#74695,#74696);
#63245=AXIS2_PLACEMENT_3D('',#106484,#74697,#74698);
#63246=AXIS2_PLACEMENT_3D('',#106486,#74700,#74701);
#63247=AXIS2_PLACEMENT_3D('',#106487,#74702,#74703);
#63248=AXIS2_PLACEMENT_3D('',#106490,#74705,#74706);
#63249=AXIS2_PLACEMENT_3D('',#106492,#74708,#74709);
#63250=AXIS2_PLACEMENT_3D('',#106494,#74711,#74712);
#63251=AXIS2_PLACEMENT_3D('',#106495,#74713,#74714);
#63252=AXIS2_PLACEMENT_3D('',#106497,#74715,#74716);
#63253=AXIS2_PLACEMENT_3D('',#106498,#74717,#74718);
#63254=AXIS2_PLACEMENT_3D('',#106500,#74720,#74721);
#63255=AXIS2_PLACEMENT_3D('',#106501,#74722,#74723);
#63256=AXIS2_PLACEMENT_3D('',#106502,#74724,#74725);
#63257=AXIS2_PLACEMENT_3D('',#106504,#74726,#74727);
#63258=AXIS2_PLACEMENT_3D('',#106506,#74729,#74730);
#63259=AXIS2_PLACEMENT_3D('',#106507,#74731,#74732);
#63260=AXIS2_PLACEMENT_3D('',#106508,#74733,#74734);
#63261=AXIS2_PLACEMENT_3D('',#106524,#74736,#74737);
#63262=AXIS2_PLACEMENT_3D('',#106532,#74738,#74739);
#63263=AXIS2_PLACEMENT_3D('',#106580,#74741,#74742);
#63264=AXIS2_PLACEMENT_3D('',#106628,#74744,#74745);
#63265=AXIS2_PLACEMENT_3D('',#106682,#74747,#74748);
#63266=AXIS2_PLACEMENT_3D('',#106730,#74750,#74751);
#63267=AXIS2_PLACEMENT_3D('',#106778,#74753,#74754);
#63268=AXIS2_PLACEMENT_3D('',#106832,#74756,#74757);
#63269=AXIS2_PLACEMENT_3D('',#106880,#74759,#74760);
#63270=AXIS2_PLACEMENT_3D('',#106928,#74762,#74763);
#63271=AXIS2_PLACEMENT_3D('',#106982,#74765,#74766);
#63272=AXIS2_PLACEMENT_3D('',#107030,#74768,#74769);
#63273=AXIS2_PLACEMENT_3D('',#107045,#74771,#74772);
#63274=AXIS2_PLACEMENT_3D('',#107054,#74773,#74774);
#63275=AXIS2_PLACEMENT_3D('',#107079,#74776,#74777);
#63276=AXIS2_PLACEMENT_3D('',#107104,#74779,#74780);
#63277=AXIS2_PLACEMENT_3D('',#107128,#74782,#74783);
#63278=AXIS2_PLACEMENT_3D('',#107153,#74785,#74786);
#63279=AXIS2_PLACEMENT_3D('',#107178,#74788,#74789);
#63280=AXIS2_PLACEMENT_3D('',#107202,#74791,#74792);
#63281=AXIS2_PLACEMENT_3D('',#107227,#74794,#74795);
#63282=AXIS2_PLACEMENT_3D('',#107252,#74797,#74798);
#63283=AXIS2_PLACEMENT_3D('',#107276,#74800,#74801);
#63284=AXIS2_PLACEMENT_3D('',#107364,#74802,#74803);
#63285=AXIS2_PLACEMENT_3D('',#107366,#74804,#74805);
#63286=AXIS2_PLACEMENT_3D('',#107842,#74806,#74807);
#63287=AXIS2_PLACEMENT_3D('',#107844,#74808,#74809);
#63288=AXIS2_PLACEMENT_3D('',#107845,#74810,#74811);
#63289=AXIS2_PLACEMENT_3D('',#107929,#74812,#74813);
#63290=AXIS2_PLACEMENT_3D('',#107930,#74814,#74815);
#63291=AXIS2_PLACEMENT_3D('',#108234,#74816,#74817);
#63292=AXIS2_PLACEMENT_3D('',#108236,#74818,#74819);
#63293=AXIS2_PLACEMENT_3D('',#108244,#74821,#74822);
#63294=AXIS2_PLACEMENT_3D('',#108254,#74823,#74824);
#63295=AXIS2_PLACEMENT_3D('',#108264,#74825,#74826);
#63296=AXIS2_PLACEMENT_3D('',#108274,#74827,#74828);
#63297=AXIS2_PLACEMENT_3D('',#108284,#74829,#74830);
#63298=AXIS2_PLACEMENT_3D('',#108294,#74831,#74832);
#63299=AXIS2_PLACEMENT_3D('',#108298,#74833,#74834);
#63300=AXIS2_PLACEMENT_3D('',#108303,#74837,#74838);
#63301=AXIS2_PLACEMENT_3D('',#108304,#74839,#74840);
#63302=AXIS2_PLACEMENT_3D('',#108309,#74843,#74844);
#63303=AXIS2_PLACEMENT_3D('',#108310,#74845,#74846);
#63304=AXIS2_PLACEMENT_3D('',#108314,#74848,#74849);
#63305=AXIS2_PLACEMENT_3D('',#108316,#74851,#74852);
#63306=AXIS2_PLACEMENT_3D('',#108321,#74855,#74856);
#63307=AXIS2_PLACEMENT_3D('',#108322,#74857,#74858);
#63308=AXIS2_PLACEMENT_3D('',#108326,#74860,#74861);
#63309=AXIS2_PLACEMENT_3D('',#108328,#74863,#74864);
#63310=AXIS2_PLACEMENT_3D('',#108332,#74866,#74867);
#63311=AXIS2_PLACEMENT_3D('',#108334,#74869,#74870);
#63312=AXIS2_PLACEMENT_3D('',#108341,#74875,#74876);
#63313=AXIS2_PLACEMENT_3D('',#108346,#74880,#74881);
#63314=AXIS2_PLACEMENT_3D('',#108351,#74885,#74886);
#63315=AXIS2_PLACEMENT_3D('',#108352,#74887,#74888);
#63316=AXIS2_PLACEMENT_3D('',#108353,#74889,#74890);
#63317=AXIS2_PLACEMENT_3D('',#108355,#74892,#74893);
#63318=AXIS2_PLACEMENT_3D('',#108356,#74894,#74895);
#63319=AXIS2_PLACEMENT_3D('',#108358,#74897,#74898);
#63320=AXIS2_PLACEMENT_3D('',#108360,#74900,#74901);
#63321=AXIS2_PLACEMENT_3D('',#108363,#74903,#74904);
#63322=AXIS2_PLACEMENT_3D('',#108364,#74905,#74906);
#63323=AXIS2_PLACEMENT_3D('',#108365,#74907,#74908);
#63324=AXIS2_PLACEMENT_3D('',#108366,#74909,#74910);
#63325=AXIS2_PLACEMENT_3D('',#108367,#74911,#74912);
#63326=AXIS2_PLACEMENT_3D('',#108368,#74913,#74914);
#63327=AXIS2_PLACEMENT_3D('',#108369,#74915,#74916);
#63328=AXIS2_PLACEMENT_3D('',#108370,#74917,#74918);
#63329=AXIS2_PLACEMENT_3D('',#108373,#74920,#74921);
#63330=AXIS2_PLACEMENT_3D('',#108374,#74922,#74923);
#63331=AXIS2_PLACEMENT_3D('',#108376,#74925,#74926);
#63332=AXIS2_PLACEMENT_3D('',#108377,#74927,#74928);
#63333=AXIS2_PLACEMENT_3D('',#108380,#74930,#74931);
#63334=AXIS2_PLACEMENT_3D('',#108382,#74933,#74934);
#63335=AXIS2_PLACEMENT_3D('',#108384,#74936,#74937);
#63336=AXIS2_PLACEMENT_3D('',#108385,#74938,#74939);
#63337=AXIS2_PLACEMENT_3D('',#108387,#74940,#74941);
#63338=AXIS2_PLACEMENT_3D('',#108388,#74942,#74943);
#63339=AXIS2_PLACEMENT_3D('',#108390,#74945,#74946);
#63340=AXIS2_PLACEMENT_3D('',#108391,#74947,#74948);
#63341=AXIS2_PLACEMENT_3D('',#108392,#74949,#74950);
#63342=AXIS2_PLACEMENT_3D('',#108394,#74951,#74952);
#63343=AXIS2_PLACEMENT_3D('',#108396,#74954,#74955);
#63344=AXIS2_PLACEMENT_3D('',#108397,#74956,#74957);
#63345=AXIS2_PLACEMENT_3D('',#108398,#74958,#74959);
#63346=AXIS2_PLACEMENT_3D('',#108414,#74961,#74962);
#63347=AXIS2_PLACEMENT_3D('',#108422,#74963,#74964);
#63348=AXIS2_PLACEMENT_3D('',#108470,#74966,#74967);
#63349=AXIS2_PLACEMENT_3D('',#108518,#74969,#74970);
#63350=AXIS2_PLACEMENT_3D('',#108572,#74972,#74973);
#63351=AXIS2_PLACEMENT_3D('',#108620,#74975,#74976);
#63352=AXIS2_PLACEMENT_3D('',#108668,#74978,#74979);
#63353=AXIS2_PLACEMENT_3D('',#108678,#74981,#74982);
#63354=AXIS2_PLACEMENT_3D('',#108679,#74983,#74984);
#63355=AXIS2_PLACEMENT_3D('',#108694,#74986,#74987);
#63356=AXIS2_PLACEMENT_3D('',#108705,#74988,#74989);
#63357=AXIS2_PLACEMENT_3D('',#108729,#74991,#74992);
#63358=AXIS2_PLACEMENT_3D('',#108754,#74994,#74995);
#63359=AXIS2_PLACEMENT_3D('',#108779,#74997,#74998);
#63360=AXIS2_PLACEMENT_3D('',#108803,#75000,#75001);
#63361=AXIS2_PLACEMENT_3D('',#108879,#75002,#75003);
#63362=AXIS2_PLACEMENT_3D('',#108881,#75004,#75005);
#63363=AXIS2_PLACEMENT_3D('',#109225,#75006,#75007);
#63364=AXIS2_PLACEMENT_3D('',#109227,#75008,#75009);
#63365=AXIS2_PLACEMENT_3D('',#109228,#75010,#75011);
#63366=AXIS2_PLACEMENT_3D('',#109306,#75012,#75013);
#63367=AXIS2_PLACEMENT_3D('',#109307,#75014,#75015);
#63368=AXIS2_PLACEMENT_3D('',#109497,#75016,#75017);
#63369=AXIS2_PLACEMENT_3D('',#109499,#75018,#75019);
#63370=AXIS2_PLACEMENT_3D('',#109507,#75021,#75022);
#63371=AXIS2_PLACEMENT_3D('',#109517,#75023,#75024);
#63372=AXIS2_PLACEMENT_3D('',#109527,#75025,#75026);
#63373=AXIS2_PLACEMENT_3D('',#109537,#75027,#75028);
#63374=AXIS2_PLACEMENT_3D('',#109547,#75029,#75030);
#63375=AXIS2_PLACEMENT_3D('',#109557,#75031,#75032);
#63376=AXIS2_PLACEMENT_3D('',#109561,#75033,#75034);
#63377=AXIS2_PLACEMENT_3D('',#109566,#75037,#75038);
#63378=AXIS2_PLACEMENT_3D('',#109567,#75039,#75040);
#63379=AXIS2_PLACEMENT_3D('',#109572,#75043,#75044);
#63380=AXIS2_PLACEMENT_3D('',#109573,#75045,#75046);
#63381=AXIS2_PLACEMENT_3D('',#109577,#75048,#75049);
#63382=AXIS2_PLACEMENT_3D('',#109579,#75051,#75052);
#63383=AXIS2_PLACEMENT_3D('',#109584,#75055,#75056);
#63384=AXIS2_PLACEMENT_3D('',#109585,#75057,#75058);
#63385=AXIS2_PLACEMENT_3D('',#109589,#75060,#75061);
#63386=AXIS2_PLACEMENT_3D('',#109591,#75063,#75064);
#63387=AXIS2_PLACEMENT_3D('',#109595,#75066,#75067);
#63388=AXIS2_PLACEMENT_3D('',#109597,#75069,#75070);
#63389=AXIS2_PLACEMENT_3D('',#109604,#75075,#75076);
#63390=AXIS2_PLACEMENT_3D('',#109609,#75080,#75081);
#63391=AXIS2_PLACEMENT_3D('',#109614,#75085,#75086);
#63392=AXIS2_PLACEMENT_3D('',#109615,#75087,#75088);
#63393=AXIS2_PLACEMENT_3D('',#109616,#75089,#75090);
#63394=AXIS2_PLACEMENT_3D('',#109618,#75092,#75093);
#63395=AXIS2_PLACEMENT_3D('',#109619,#75094,#75095);
#63396=AXIS2_PLACEMENT_3D('',#109621,#75097,#75098);
#63397=AXIS2_PLACEMENT_3D('',#109623,#75100,#75101);
#63398=AXIS2_PLACEMENT_3D('',#109626,#75103,#75104);
#63399=AXIS2_PLACEMENT_3D('',#109627,#75105,#75106);
#63400=AXIS2_PLACEMENT_3D('',#109628,#75107,#75108);
#63401=AXIS2_PLACEMENT_3D('',#109629,#75109,#75110);
#63402=AXIS2_PLACEMENT_3D('',#109630,#75111,#75112);
#63403=AXIS2_PLACEMENT_3D('',#109631,#75113,#75114);
#63404=AXIS2_PLACEMENT_3D('',#109632,#75115,#75116);
#63405=AXIS2_PLACEMENT_3D('',#109633,#75117,#75118);
#63406=AXIS2_PLACEMENT_3D('',#109636,#75120,#75121);
#63407=AXIS2_PLACEMENT_3D('',#109637,#75122,#75123);
#63408=AXIS2_PLACEMENT_3D('',#109639,#75125,#75126);
#63409=AXIS2_PLACEMENT_3D('',#109640,#75127,#75128);
#63410=AXIS2_PLACEMENT_3D('',#109643,#75130,#75131);
#63411=AXIS2_PLACEMENT_3D('',#109645,#75133,#75134);
#63412=AXIS2_PLACEMENT_3D('',#109647,#75136,#75137);
#63413=AXIS2_PLACEMENT_3D('',#109648,#75138,#75139);
#63414=AXIS2_PLACEMENT_3D('',#109650,#75140,#75141);
#63415=AXIS2_PLACEMENT_3D('',#109651,#75142,#75143);
#63416=AXIS2_PLACEMENT_3D('',#109653,#75145,#75146);
#63417=AXIS2_PLACEMENT_3D('',#109654,#75147,#75148);
#63418=AXIS2_PLACEMENT_3D('',#109655,#75149,#75150);
#63419=AXIS2_PLACEMENT_3D('',#109657,#75151,#75152);
#63420=AXIS2_PLACEMENT_3D('',#109659,#75154,#75155);
#63421=AXIS2_PLACEMENT_3D('',#109660,#75156,#75157);
#63422=AXIS2_PLACEMENT_3D('',#109661,#75158,#75159);
#63423=AXIS2_PLACEMENT_3D('',#109677,#75161,#75162);
#63424=AXIS2_PLACEMENT_3D('',#109685,#75163,#75164);
#63425=AXIS2_PLACEMENT_3D('',#109733,#75166,#75167);
#63426=AXIS2_PLACEMENT_3D('',#109781,#75169,#75170);
#63427=AXIS2_PLACEMENT_3D('',#109835,#75172,#75173);
#63428=AXIS2_PLACEMENT_3D('',#109883,#75175,#75176);
#63429=AXIS2_PLACEMENT_3D('',#109931,#75178,#75179);
#63430=AXIS2_PLACEMENT_3D('',#109985,#75181,#75182);
#63431=AXIS2_PLACEMENT_3D('',#109990,#75184,#75185);
#63432=AXIS2_PLACEMENT_3D('',#110032,#75186,#75187);
#63433=AXIS2_PLACEMENT_3D('',#110045,#75189,#75190);
#63434=AXIS2_PLACEMENT_3D('',#110052,#75191,#75192);
#63435=AXIS2_PLACEMENT_3D('',#110077,#75194,#75195);
#63436=AXIS2_PLACEMENT_3D('',#110102,#75197,#75198);
#63437=AXIS2_PLACEMENT_3D('',#110126,#75200,#75201);
#63438=AXIS2_PLACEMENT_3D('',#110151,#75203,#75204);
#63439=AXIS2_PLACEMENT_3D('',#110176,#75206,#75207);
#63440=AXIS2_PLACEMENT_3D('',#110200,#75209,#75210);
#63441=AXIS2_PLACEMENT_3D('',#110275,#75211,#75212);
#63442=AXIS2_PLACEMENT_3D('',#110643,#75213,#75214);
#63443=AXIS2_PLACEMENT_3D('',#110645,#75215,#75216);
#63444=AXIS2_PLACEMENT_3D('',#110646,#75217,#75218);
#63445=AXIS2_PLACEMENT_3D('',#110724,#75219,#75220);
#63446=AXIS2_PLACEMENT_3D('',#110725,#75221,#75222);
#63447=AXIS2_PLACEMENT_3D('',#110938,#75223,#75224);
#63448=AXIS2_PLACEMENT_3D('',#110947,#75229,#75230);
#63449=AXIS2_PLACEMENT_3D('',#110953,#75234,#75235);
#63450=AXIS2_PLACEMENT_3D('',#110959,#75239,#75240);
#63451=AXIS2_PLACEMENT_3D('',#110965,#75244,#75245);
#63452=AXIS2_PLACEMENT_3D('',#110971,#75249,#75250);
#63453=AXIS2_PLACEMENT_3D('',#110974,#75253,#75254);
#63454=AXIS2_PLACEMENT_3D('',#110975,#75255,#75256);
#63455=AXIS2_PLACEMENT_3D('',#110977,#75257,#75258);
#63456=AXIS2_PLACEMENT_3D('',#110978,#75259,#75260);
#63457=AXIS2_PLACEMENT_3D('',#110980,#75262,#75263);
#63458=AXIS2_PLACEMENT_3D('',#110981,#75264,#75265);
#63459=AXIS2_PLACEMENT_3D('',#110982,#75266,#75267);
#63460=AXIS2_PLACEMENT_3D('',#110984,#75268,#75269);
#63461=AXIS2_PLACEMENT_3D('',#110986,#75271,#75272);
#63462=AXIS2_PLACEMENT_3D('',#110987,#75273,#75274);
#63463=AXIS2_PLACEMENT_3D('',#110988,#75275,#75276);
#63464=AXIS2_PLACEMENT_3D('',#111004,#75278,#75279);
#63465=AXIS2_PLACEMENT_3D('',#111012,#75280,#75281);
#63466=AXIS2_PLACEMENT_3D('',#111060,#75283,#75284);
#63467=AXIS2_PLACEMENT_3D('',#111108,#75286,#75287);
#63468=AXIS2_PLACEMENT_3D('',#111162,#75289,#75290);
#63469=AXIS2_PLACEMENT_3D('',#111210,#75292,#75293);
#63470=AXIS2_PLACEMENT_3D('',#111258,#75295,#75296);
#63471=AXIS2_PLACEMENT_3D('',#111312,#75298,#75299);
#63472=AXIS2_PLACEMENT_3D('',#111360,#75301,#75302);
#63473=AXIS2_PLACEMENT_3D('',#111408,#75304,#75305);
#63474=AXIS2_PLACEMENT_3D('',#111456,#75307,#75308);
#63475=AXIS2_PLACEMENT_3D('',#111510,#75310,#75311);
#63476=AXIS2_PLACEMENT_3D('',#111558,#75313,#75314);
#63477=AXIS2_PLACEMENT_3D('',#111606,#75316,#75317);
#63478=AXIS2_PLACEMENT_3D('',#111620,#75319,#75320);
#63479=AXIS2_PLACEMENT_3D('',#111628,#75321,#75322);
#63480=AXIS2_PLACEMENT_3D('',#111652,#75324,#75325);
#63481=AXIS2_PLACEMENT_3D('',#111677,#75327,#75328);
#63482=AXIS2_PLACEMENT_3D('',#111702,#75330,#75331);
#63483=AXIS2_PLACEMENT_3D('',#111726,#75333,#75334);
#63484=AXIS2_PLACEMENT_3D('',#111750,#75336,#75337);
#63485=AXIS2_PLACEMENT_3D('',#111775,#75339,#75340);
#63486=AXIS2_PLACEMENT_3D('',#111800,#75342,#75343);
#63487=AXIS2_PLACEMENT_3D('',#111824,#75345,#75346);
#63488=AXIS2_PLACEMENT_3D('',#111849,#75348,#75349);
#63489=AXIS2_PLACEMENT_3D('',#111874,#75351,#75352);
#63490=AXIS2_PLACEMENT_3D('',#111898,#75354,#75355);
#63491=AXIS2_PLACEMENT_3D('',#111983,#75356,#75357);
#63492=AXIS2_PLACEMENT_3D('',#111985,#75358,#75359);
#63493=AXIS2_PLACEMENT_3D('',#112499,#75360,#75361);
#63494=AXIS2_PLACEMENT_3D('',#112501,#75362,#75363);
#63495=AXIS2_PLACEMENT_3D('',#112585,#75364,#75365);
#63496=AXIS2_PLACEMENT_3D('',#112586,#75366,#75367);
#63497=AXIS2_PLACEMENT_3D('',#112587,#75368,#75369);
#63498=AXIS2_PLACEMENT_3D('',#112932,#75370,#75371);
#63499=AXIS2_PLACEMENT_3D('',#112934,#75372,#75373);
#63500=AXIS2_PLACEMENT_3D('',#112935,#75374,#75375);
#63501=AXIS2_PLACEMENT_3D('',#112936,#75376,#75377);
#63502=AXIS2_PLACEMENT_3D('',#112937,#75378,#75379);
#63503=AXIS2_PLACEMENT_3D('',#112938,#75380,#75381);
#63504=AXIS2_PLACEMENT_3D('',#112940,#75382,#75383);
#63505=AXIS2_PLACEMENT_3D('',#112941,#75384,#75385);
#63506=AXIS2_PLACEMENT_3D('',#112944,#75387,#75388);
#63507=AXIS2_PLACEMENT_3D('',#112945,#75389,#75390);
#63508=AXIS2_PLACEMENT_3D('',#112946,#75391,#75392);
#63509=AXIS2_PLACEMENT_3D('',#112957,#75396,#75397);
#63510=AXIS2_PLACEMENT_3D('',#112959,#75398,#75399);
#63511=AXIS2_PLACEMENT_3D('',#112961,#75401,#75402);
#63512=AXIS2_PLACEMENT_3D('',#112967,#75404,#75405);
#63513=AXIS2_PLACEMENT_3D('',#112969,#75406,#75407);
#63514=AXIS2_PLACEMENT_3D('',#112973,#75409,#75410);
#63515=AXIS2_PLACEMENT_3D('',#112977,#75412,#75413);
#63516=AXIS2_PLACEMENT_3D('',#112981,#75415,#75416);
#63517=AXIS2_PLACEMENT_3D('',#112985,#75418,#75419);
#63518=AXIS2_PLACEMENT_3D('',#112989,#75421,#75422);
#63519=AXIS2_PLACEMENT_3D('',#112993,#75424,#75425);
#63520=AXIS2_PLACEMENT_3D('',#112997,#75427,#75428);
#63521=AXIS2_PLACEMENT_3D('',#113001,#75430,#75431);
#63522=AXIS2_PLACEMENT_3D('',#113005,#75433,#75434);
#63523=AXIS2_PLACEMENT_3D('',#113009,#75436,#75437);
#63524=AXIS2_PLACEMENT_3D('',#113013,#75439,#75440);
#63525=AXIS2_PLACEMENT_3D('',#113017,#75442,#75443);
#63526=AXIS2_PLACEMENT_3D('',#113021,#75445,#75446);
#63527=AXIS2_PLACEMENT_3D('',#113025,#75448,#75449);
#63528=AXIS2_PLACEMENT_3D('',#113029,#75451,#75452);
#63529=AXIS2_PLACEMENT_3D('',#113033,#75454,#75455);
#63530=AXIS2_PLACEMENT_3D('',#113037,#75457,#75458);
#63531=AXIS2_PLACEMENT_3D('',#113041,#75460,#75461);
#63532=AXIS2_PLACEMENT_3D('',#113045,#75463,#75464);
#63533=AXIS2_PLACEMENT_3D('',#113049,#75466,#75467);
#63534=AXIS2_PLACEMENT_3D('',#113053,#75469,#75470);
#63535=AXIS2_PLACEMENT_3D('',#113057,#75472,#75473);
#63536=AXIS2_PLACEMENT_3D('',#113061,#75475,#75476);
#63537=AXIS2_PLACEMENT_3D('',#113065,#75478,#75479);
#63538=AXIS2_PLACEMENT_3D('',#113069,#75481,#75482);
#63539=AXIS2_PLACEMENT_3D('',#113073,#75484,#75485);
#63540=AXIS2_PLACEMENT_3D('',#113077,#75487,#75488);
#63541=AXIS2_PLACEMENT_3D('',#113081,#75490,#75491);
#63542=AXIS2_PLACEMENT_3D('',#113085,#75493,#75494);
#63543=AXIS2_PLACEMENT_3D('',#113089,#75496,#75497);
#63544=AXIS2_PLACEMENT_3D('',#113093,#75499,#75500);
#63545=AXIS2_PLACEMENT_3D('',#113097,#75502,#75503);
#63546=AXIS2_PLACEMENT_3D('',#113101,#75505,#75506);
#63547=AXIS2_PLACEMENT_3D('',#113105,#75508,#75509);
#63548=AXIS2_PLACEMENT_3D('',#113109,#75511,#75512);
#63549=AXIS2_PLACEMENT_3D('',#113113,#75514,#75515);
#63550=AXIS2_PLACEMENT_3D('',#113117,#75517,#75518);
#63551=AXIS2_PLACEMENT_3D('',#113121,#75520,#75521);
#63552=AXIS2_PLACEMENT_3D('',#113122,#75522,#75523);
#63553=AXIS2_PLACEMENT_3D('',#113124,#75524,#75525);
#63554=AXIS2_PLACEMENT_3D('',#113128,#75527,#75528);
#63555=AXIS2_PLACEMENT_3D('',#113132,#75530,#75531);
#63556=AXIS2_PLACEMENT_3D('',#113136,#75533,#75534);
#63557=AXIS2_PLACEMENT_3D('',#113140,#75536,#75537);
#63558=AXIS2_PLACEMENT_3D('',#113144,#75539,#75540);
#63559=AXIS2_PLACEMENT_3D('',#113148,#75542,#75543);
#63560=AXIS2_PLACEMENT_3D('',#113152,#75545,#75546);
#63561=AXIS2_PLACEMENT_3D('',#113156,#75548,#75549);
#63562=AXIS2_PLACEMENT_3D('',#113160,#75551,#75552);
#63563=AXIS2_PLACEMENT_3D('',#113164,#75554,#75555);
#63564=AXIS2_PLACEMENT_3D('',#113168,#75557,#75558);
#63565=AXIS2_PLACEMENT_3D('',#113172,#75560,#75561);
#63566=AXIS2_PLACEMENT_3D('',#113176,#75563,#75564);
#63567=AXIS2_PLACEMENT_3D('',#113180,#75566,#75567);
#63568=AXIS2_PLACEMENT_3D('',#113184,#75569,#75570);
#63569=AXIS2_PLACEMENT_3D('',#113188,#75572,#75573);
#63570=AXIS2_PLACEMENT_3D('',#113192,#75575,#75576);
#63571=AXIS2_PLACEMENT_3D('',#113196,#75578,#75579);
#63572=AXIS2_PLACEMENT_3D('',#113200,#75581,#75582);
#63573=AXIS2_PLACEMENT_3D('',#113204,#75584,#75585);
#63574=AXIS2_PLACEMENT_3D('',#113208,#75587,#75588);
#63575=AXIS2_PLACEMENT_3D('',#113212,#75590,#75591);
#63576=AXIS2_PLACEMENT_3D('',#113216,#75593,#75594);
#63577=AXIS2_PLACEMENT_3D('',#113220,#75596,#75597);
#63578=AXIS2_PLACEMENT_3D('',#113224,#75599,#75600);
#63579=AXIS2_PLACEMENT_3D('',#113228,#75602,#75603);
#63580=AXIS2_PLACEMENT_3D('',#113232,#75605,#75606);
#63581=AXIS2_PLACEMENT_3D('',#113236,#75608,#75609);
#63582=AXIS2_PLACEMENT_3D('',#113240,#75611,#75612);
#63583=AXIS2_PLACEMENT_3D('',#113244,#75614,#75615);
#63584=AXIS2_PLACEMENT_3D('',#113248,#75617,#75618);
#63585=AXIS2_PLACEMENT_3D('',#113252,#75620,#75621);
#63586=AXIS2_PLACEMENT_3D('',#113255,#75623,#75624);
#63587=AXIS2_PLACEMENT_3D('',#113256,#75625,#75626);
#63588=AXIS2_PLACEMENT_3D('',#113264,#75629,#75630);
#63589=AXIS2_PLACEMENT_3D('',#113266,#75632,#75633);
#63590=AXIS2_PLACEMENT_3D('',#113270,#75634,#75635);
#63591=AXIS2_PLACEMENT_3D('',#113278,#75638,#75639);
#63592=AXIS2_PLACEMENT_3D('',#113280,#75641,#75642);
#63593=AXIS2_PLACEMENT_3D('',#113284,#75643,#75644);
#63594=AXIS2_PLACEMENT_3D('',#113292,#75647,#75648);
#63595=AXIS2_PLACEMENT_3D('',#113294,#75650,#75651);
#63596=AXIS2_PLACEMENT_3D('',#113298,#75652,#75653);
#63597=AXIS2_PLACEMENT_3D('',#113306,#75656,#75657);
#63598=AXIS2_PLACEMENT_3D('',#113308,#75659,#75660);
#63599=AXIS2_PLACEMENT_3D('',#113312,#75661,#75662);
#63600=AXIS2_PLACEMENT_3D('',#113320,#75665,#75666);
#63601=AXIS2_PLACEMENT_3D('',#113322,#75668,#75669);
#63602=AXIS2_PLACEMENT_3D('',#113326,#75670,#75671);
#63603=AXIS2_PLACEMENT_3D('',#113334,#75674,#75675);
#63604=AXIS2_PLACEMENT_3D('',#113336,#75677,#75678);
#63605=AXIS2_PLACEMENT_3D('',#113340,#75679,#75680);
#63606=AXIS2_PLACEMENT_3D('',#113348,#75683,#75684);
#63607=AXIS2_PLACEMENT_3D('',#113350,#75686,#75687);
#63608=AXIS2_PLACEMENT_3D('',#113354,#75688,#75689);
#63609=AXIS2_PLACEMENT_3D('',#113362,#75692,#75693);
#63610=AXIS2_PLACEMENT_3D('',#113364,#75695,#75696);
#63611=AXIS2_PLACEMENT_3D('',#113368,#75697,#75698);
#63612=AXIS2_PLACEMENT_3D('',#113376,#75701,#75702);
#63613=AXIS2_PLACEMENT_3D('',#113378,#75704,#75705);
#63614=AXIS2_PLACEMENT_3D('',#113382,#75706,#75707);
#63615=AXIS2_PLACEMENT_3D('',#113390,#75710,#75711);
#63616=AXIS2_PLACEMENT_3D('',#113392,#75713,#75714);
#63617=AXIS2_PLACEMENT_3D('',#113396,#75715,#75716);
#63618=AXIS2_PLACEMENT_3D('',#113404,#75719,#75720);
#63619=AXIS2_PLACEMENT_3D('',#113406,#75722,#75723);
#63620=AXIS2_PLACEMENT_3D('',#113410,#75724,#75725);
#63621=AXIS2_PLACEMENT_3D('',#113418,#75728,#75729);
#63622=AXIS2_PLACEMENT_3D('',#113420,#75731,#75732);
#63623=AXIS2_PLACEMENT_3D('',#113424,#75733,#75734);
#63624=AXIS2_PLACEMENT_3D('',#113432,#75737,#75738);
#63625=AXIS2_PLACEMENT_3D('',#113434,#75740,#75741);
#63626=AXIS2_PLACEMENT_3D('',#113438,#75742,#75743);
#63627=AXIS2_PLACEMENT_3D('',#113446,#75746,#75747);
#63628=AXIS2_PLACEMENT_3D('',#113448,#75749,#75750);
#63629=AXIS2_PLACEMENT_3D('',#113452,#75751,#75752);
#63630=AXIS2_PLACEMENT_3D('',#113460,#75755,#75756);
#63631=AXIS2_PLACEMENT_3D('',#113462,#75758,#75759);
#63632=AXIS2_PLACEMENT_3D('',#113466,#75760,#75761);
#63633=AXIS2_PLACEMENT_3D('',#113474,#75764,#75765);
#63634=AXIS2_PLACEMENT_3D('',#113476,#75767,#75768);
#63635=AXIS2_PLACEMENT_3D('',#113480,#75769,#75770);
#63636=AXIS2_PLACEMENT_3D('',#113488,#75773,#75774);
#63637=AXIS2_PLACEMENT_3D('',#113490,#75776,#75777);
#63638=AXIS2_PLACEMENT_3D('',#113494,#75778,#75779);
#63639=AXIS2_PLACEMENT_3D('',#113502,#75782,#75783);
#63640=AXIS2_PLACEMENT_3D('',#113504,#75785,#75786);
#63641=AXIS2_PLACEMENT_3D('',#113508,#75787,#75788);
#63642=AXIS2_PLACEMENT_3D('',#113516,#75791,#75792);
#63643=AXIS2_PLACEMENT_3D('',#113518,#75794,#75795);
#63644=AXIS2_PLACEMENT_3D('',#113522,#75796,#75797);
#63645=AXIS2_PLACEMENT_3D('',#113530,#75800,#75801);
#63646=AXIS2_PLACEMENT_3D('',#113532,#75803,#75804);
#63647=AXIS2_PLACEMENT_3D('',#113536,#75805,#75806);
#63648=AXIS2_PLACEMENT_3D('',#113544,#75809,#75810);
#63649=AXIS2_PLACEMENT_3D('',#113546,#75812,#75813);
#63650=AXIS2_PLACEMENT_3D('',#113550,#75814,#75815);
#63651=AXIS2_PLACEMENT_3D('',#113558,#75818,#75819);
#63652=AXIS2_PLACEMENT_3D('',#113560,#75821,#75822);
#63653=AXIS2_PLACEMENT_3D('',#113564,#75823,#75824);
#63654=AXIS2_PLACEMENT_3D('',#113572,#75827,#75828);
#63655=AXIS2_PLACEMENT_3D('',#113574,#75830,#75831);
#63656=AXIS2_PLACEMENT_3D('',#113578,#75832,#75833);
#63657=AXIS2_PLACEMENT_3D('',#113586,#75836,#75837);
#63658=AXIS2_PLACEMENT_3D('',#113588,#75839,#75840);
#63659=AXIS2_PLACEMENT_3D('',#113592,#75841,#75842);
#63660=AXIS2_PLACEMENT_3D('',#113600,#75845,#75846);
#63661=AXIS2_PLACEMENT_3D('',#113602,#75848,#75849);
#63662=AXIS2_PLACEMENT_3D('',#113606,#75850,#75851);
#63663=AXIS2_PLACEMENT_3D('',#113614,#75854,#75855);
#63664=AXIS2_PLACEMENT_3D('',#113616,#75857,#75858);
#63665=AXIS2_PLACEMENT_3D('',#113620,#75859,#75860);
#63666=AXIS2_PLACEMENT_3D('',#113628,#75863,#75864);
#63667=AXIS2_PLACEMENT_3D('',#113630,#75866,#75867);
#63668=AXIS2_PLACEMENT_3D('',#113634,#75868,#75869);
#63669=AXIS2_PLACEMENT_3D('',#113642,#75872,#75873);
#63670=AXIS2_PLACEMENT_3D('',#113644,#75875,#75876);
#63671=AXIS2_PLACEMENT_3D('',#113648,#75877,#75878);
#63672=AXIS2_PLACEMENT_3D('',#113656,#75881,#75882);
#63673=AXIS2_PLACEMENT_3D('',#113658,#75884,#75885);
#63674=AXIS2_PLACEMENT_3D('',#113662,#75886,#75887);
#63675=AXIS2_PLACEMENT_3D('',#113670,#75890,#75891);
#63676=AXIS2_PLACEMENT_3D('',#113672,#75893,#75894);
#63677=AXIS2_PLACEMENT_3D('',#113676,#75895,#75896);
#63678=AXIS2_PLACEMENT_3D('',#113684,#75899,#75900);
#63679=AXIS2_PLACEMENT_3D('',#113686,#75902,#75903);
#63680=AXIS2_PLACEMENT_3D('',#113690,#75904,#75905);
#63681=AXIS2_PLACEMENT_3D('',#113698,#75908,#75909);
#63682=AXIS2_PLACEMENT_3D('',#113700,#75911,#75912);
#63683=AXIS2_PLACEMENT_3D('',#113704,#75913,#75914);
#63684=AXIS2_PLACEMENT_3D('',#113712,#75917,#75918);
#63685=AXIS2_PLACEMENT_3D('',#113714,#75920,#75921);
#63686=AXIS2_PLACEMENT_3D('',#113718,#75922,#75923);
#63687=AXIS2_PLACEMENT_3D('',#113726,#75926,#75927);
#63688=AXIS2_PLACEMENT_3D('',#113728,#75929,#75930);
#63689=AXIS2_PLACEMENT_3D('',#113732,#75931,#75932);
#63690=AXIS2_PLACEMENT_3D('',#113740,#75935,#75936);
#63691=AXIS2_PLACEMENT_3D('',#113742,#75938,#75939);
#63692=AXIS2_PLACEMENT_3D('',#113746,#75940,#75941);
#63693=AXIS2_PLACEMENT_3D('',#113747,#75942,#75943);
#63694=AXIS2_PLACEMENT_3D('',#113748,#75944,#75945);
#63695=AXIS2_PLACEMENT_3D('',#113750,#75946,#75947);
#63696=AXIS2_PLACEMENT_3D('',#113752,#75949,#75950);
#63697=AXIS2_PLACEMENT_3D('',#113754,#75951,#75952);
#63698=AXIS2_PLACEMENT_3D('',#113755,#75953,#75954);
#63699=AXIS2_PLACEMENT_3D('',#113763,#75956,#75957);
#63700=AXIS2_PLACEMENT_3D('',#113773,#75958,#75959);
#63701=AXIS2_PLACEMENT_3D('',#113783,#75960,#75961);
#63702=AXIS2_PLACEMENT_3D('',#113793,#75962,#75963);
#63703=AXIS2_PLACEMENT_3D('',#113803,#75964,#75965);
#63704=AXIS2_PLACEMENT_3D('',#113813,#75966,#75967);
#63705=AXIS2_PLACEMENT_3D('',#113817,#75968,#75969);
#63706=AXIS2_PLACEMENT_3D('',#113822,#75972,#75973);
#63707=AXIS2_PLACEMENT_3D('',#113823,#75974,#75975);
#63708=AXIS2_PLACEMENT_3D('',#113828,#75978,#75979);
#63709=AXIS2_PLACEMENT_3D('',#113829,#75980,#75981);
#63710=AXIS2_PLACEMENT_3D('',#113833,#75983,#75984);
#63711=AXIS2_PLACEMENT_3D('',#113835,#75986,#75987);
#63712=AXIS2_PLACEMENT_3D('',#113840,#75990,#75991);
#63713=AXIS2_PLACEMENT_3D('',#113841,#75992,#75993);
#63714=AXIS2_PLACEMENT_3D('',#113845,#75995,#75996);
#63715=AXIS2_PLACEMENT_3D('',#113847,#75998,#75999);
#63716=AXIS2_PLACEMENT_3D('',#113851,#76001,#76002);
#63717=AXIS2_PLACEMENT_3D('',#113853,#76004,#76005);
#63718=AXIS2_PLACEMENT_3D('',#113860,#76010,#76011);
#63719=AXIS2_PLACEMENT_3D('',#113865,#76015,#76016);
#63720=AXIS2_PLACEMENT_3D('',#113870,#76020,#76021);
#63721=AXIS2_PLACEMENT_3D('',#113871,#76022,#76023);
#63722=AXIS2_PLACEMENT_3D('',#113872,#76024,#76025);
#63723=AXIS2_PLACEMENT_3D('',#113874,#76027,#76028);
#63724=AXIS2_PLACEMENT_3D('',#113875,#76029,#76030);
#63725=AXIS2_PLACEMENT_3D('',#113877,#76032,#76033);
#63726=AXIS2_PLACEMENT_3D('',#113879,#76035,#76036);
#63727=AXIS2_PLACEMENT_3D('',#113882,#76038,#76039);
#63728=AXIS2_PLACEMENT_3D('',#113883,#76040,#76041);
#63729=AXIS2_PLACEMENT_3D('',#113884,#76042,#76043);
#63730=AXIS2_PLACEMENT_3D('',#113885,#76044,#76045);
#63731=AXIS2_PLACEMENT_3D('',#113886,#76046,#76047);
#63732=AXIS2_PLACEMENT_3D('',#113887,#76048,#76049);
#63733=AXIS2_PLACEMENT_3D('',#113888,#76050,#76051);
#63734=AXIS2_PLACEMENT_3D('',#113889,#76052,#76053);
#63735=AXIS2_PLACEMENT_3D('',#113892,#76055,#76056);
#63736=AXIS2_PLACEMENT_3D('',#113893,#76057,#76058);
#63737=AXIS2_PLACEMENT_3D('',#113895,#76060,#76061);
#63738=AXIS2_PLACEMENT_3D('',#113896,#76062,#76063);
#63739=AXIS2_PLACEMENT_3D('',#113899,#76065,#76066);
#63740=AXIS2_PLACEMENT_3D('',#113901,#76068,#76069);
#63741=AXIS2_PLACEMENT_3D('',#113903,#76071,#76072);
#63742=AXIS2_PLACEMENT_3D('',#113904,#76073,#76074);
#63743=AXIS2_PLACEMENT_3D('',#113905,#76075,#76076);
#63744=AXIS2_PLACEMENT_3D('',#113907,#76077,#76078);
#63745=AXIS2_PLACEMENT_3D('',#113908,#76079,#76080);
#63746=AXIS2_PLACEMENT_3D('',#113910,#76081,#76082);
#63747=AXIS2_PLACEMENT_3D('',#113912,#76084,#76085);
#63748=AXIS2_PLACEMENT_3D('',#113914,#76086,#76087);
#63749=AXIS2_PLACEMENT_3D('',#113916,#76089,#76090);
#63750=AXIS2_PLACEMENT_3D('',#113918,#76091,#76092);
#63751=AXIS2_PLACEMENT_3D('',#113920,#76094,#76095);
#63752=AXIS2_PLACEMENT_3D('',#113921,#76096,#76097);
#63753=AXIS2_PLACEMENT_3D('',#113922,#76098,#76099);
#63754=AXIS2_PLACEMENT_3D('',#113923,#76100,#76101);
#63755=AXIS2_PLACEMENT_3D('',#113924,#76102,#76103);
#63756=AXIS2_PLACEMENT_3D('',#113925,#76104,#76105);
#63757=AXIS2_PLACEMENT_3D('',#113926,#76106,#76107);
#63758=AXIS2_PLACEMENT_3D('',#113927,#76108,#76109);
#63759=AXIS2_PLACEMENT_3D('',#113928,#76110,#76111);
#63760=AXIS2_PLACEMENT_3D('',#113929,#76112,#76113);
#63761=AXIS2_PLACEMENT_3D('',#113930,#76114,#76115);
#63762=AXIS2_PLACEMENT_3D('',#113931,#76116,#76117);
#63763=AXIS2_PLACEMENT_3D('',#113932,#76118,#76119);
#63764=AXIS2_PLACEMENT_3D('',#113933,#76120,#76121);
#63765=AXIS2_PLACEMENT_3D('',#113934,#76122,#76123);
#63766=AXIS2_PLACEMENT_3D('',#113935,#76124,#76125);
#63767=AXIS2_PLACEMENT_3D('',#113936,#76126,#76127);
#63768=AXIS2_PLACEMENT_3D('',#113937,#76128,#76129);
#63769=AXIS2_PLACEMENT_3D('',#113938,#76130,#76131);
#63770=AXIS2_PLACEMENT_3D('',#113939,#76132,#76133);
#63771=AXIS2_PLACEMENT_3D('',#113940,#76134,#76135);
#63772=AXIS2_PLACEMENT_3D('',#113941,#76136,#76137);
#63773=AXIS2_PLACEMENT_3D('',#113942,#76138,#76139);
#63774=AXIS2_PLACEMENT_3D('',#113943,#76140,#76141);
#63775=AXIS2_PLACEMENT_3D('',#113944,#76142,#76143);
#63776=DIRECTION('axis',(0.,0.,1.));
#63777=DIRECTION('refdir',(1.,0.,0.));
#63778=DIRECTION('axis',(0.,0.,1.));
#63779=DIRECTION('refdir',(1.,0.,0.));
#63780=DIRECTION('',(0.,0.,-1.));
#63781=DIRECTION('',(0.,0.,-1.));
#63782=DIRECTION('',(0.,0.,-1.));
#63783=DIRECTION('',(0.,0.,-1.));
#63784=DIRECTION('',(0.,0.,-1.));
#63785=DIRECTION('',(0.,0.,-1.));
#63786=DIRECTION('',(0.,0.,-1.));
#63787=DIRECTION('',(0.,0.,-1.));
#63788=DIRECTION('',(0.,0.,-1.));
#63789=DIRECTION('',(0.,0.,-1.));
#63790=DIRECTION('',(0.,0.,-1.));
#63791=DIRECTION('',(0.,0.,-1.));
#63792=DIRECTION('',(0.,0.,-1.));
#63793=DIRECTION('',(0.,0.,-1.));
#63794=DIRECTION('',(0.,0.,-1.));
#63795=DIRECTION('',(0.,0.,-1.));
#63796=DIRECTION('',(0.,0.,-1.));
#63797=DIRECTION('',(0.,0.,-1.));
#63798=DIRECTION('',(0.,0.,-1.));
#63799=DIRECTION('',(0.,0.,-1.));
#63800=DIRECTION('center_axis',(0.,0.,1.));
#63801=DIRECTION('ref_axis',(1.,0.,0.));
#63802=DIRECTION('',(0.,0.,-1.));
#63803=DIRECTION('',(0.,0.,-1.));
#63804=DIRECTION('',(0.,0.,-1.));
#63805=DIRECTION('',(0.,0.,-1.));
#63806=DIRECTION('',(0.,0.,-1.));
#63807=DIRECTION('',(0.,0.,-1.));
#63808=DIRECTION('',(0.,0.,-1.));
#63809=DIRECTION('',(0.,0.,-1.));
#63810=DIRECTION('',(0.,0.,-1.));
#63811=DIRECTION('',(0.,0.,-1.));
#63812=DIRECTION('',(0.,0.,-1.));
#63813=DIRECTION('',(0.,0.,-1.));
#63814=DIRECTION('',(0.,0.,-1.));
#63815=DIRECTION('',(0.,0.,-1.));
#63816=DIRECTION('',(0.,0.,-1.));
#63817=DIRECTION('',(0.,0.,-1.));
#63818=DIRECTION('',(0.,0.,-1.));
#63819=DIRECTION('',(0.,0.,-1.));
#63820=DIRECTION('',(0.,0.,-1.));
#63821=DIRECTION('',(0.,0.,-1.));
#63822=DIRECTION('',(0.,0.,-1.));
#63823=DIRECTION('',(0.,0.,-1.));
#63824=DIRECTION('',(0.,0.,-1.));
#63825=DIRECTION('',(0.,0.,-1.));
#63826=DIRECTION('',(0.,0.,-1.));
#63827=DIRECTION('',(0.,0.,-1.));
#63828=DIRECTION('',(0.,0.,-1.));
#63829=DIRECTION('',(0.,0.,-1.));
#63830=DIRECTION('',(0.,0.,-1.));
#63831=DIRECTION('center_axis',(-0.0920922327212455,0.995750481130899,0.));
#63832=DIRECTION('ref_axis',(0.995750481130899,0.0920922327212455,0.));
#63833=DIRECTION('',(0.995750481130899,0.0920922327212455,0.));
#63834=DIRECTION('',(0.,0.,-1.));
#63835=DIRECTION('',(0.995750481130898,0.0920922327212455,0.));
#63836=DIRECTION('center_axis',(0.,0.,1.));
#63837=DIRECTION('ref_axis',(1.,0.,0.));
#63838=DIRECTION('center_axis',(0.,0.,1.));
#63839=DIRECTION('ref_axis',(0.,-1.,0.));
#63840=DIRECTION('center_axis',(0.,0.,1.));
#63841=DIRECTION('ref_axis',(0.,-1.,0.));
#63842=DIRECTION('',(0.,0.,-1.));
#63843=DIRECTION('',(0.,0.,-1.));
#63844=DIRECTION('',(0.,0.,-1.));
#63845=DIRECTION('',(0.,0.,-1.));
#63846=DIRECTION('',(0.,0.,-1.));
#63847=DIRECTION('',(0.,0.,-1.));
#63848=DIRECTION('',(0.,0.,-1.));
#63849=DIRECTION('',(0.,0.,-1.));
#63850=DIRECTION('',(0.,0.,-1.));
#63851=DIRECTION('',(0.,0.,-1.));
#63852=DIRECTION('',(0.,0.,-1.));
#63853=DIRECTION('',(0.,0.,-1.));
#63854=DIRECTION('',(0.,0.,-1.));
#63855=DIRECTION('',(0.,0.,-1.));
#63856=DIRECTION('',(0.,0.,-1.));
#63857=DIRECTION('',(0.,0.,-1.));
#63858=DIRECTION('',(0.,0.,-1.));
#63859=DIRECTION('',(0.,0.,-1.));
#63860=DIRECTION('',(0.,0.,-1.));
#63861=DIRECTION('',(0.,0.,-1.));
#63862=DIRECTION('center_axis',(0.,0.,1.));
#63863=DIRECTION('ref_axis',(1.,0.,0.));
#63864=DIRECTION('',(0.,0.,-1.));
#63865=DIRECTION('',(0.,0.,-1.));
#63866=DIRECTION('',(0.,0.,-1.));
#63867=DIRECTION('',(0.,0.,-1.));
#63868=DIRECTION('',(0.,0.,-1.));
#63869=DIRECTION('',(0.,0.,-1.));
#63870=DIRECTION('',(0.,0.,-1.));
#63871=DIRECTION('',(0.,0.,-1.));
#63872=DIRECTION('',(0.,0.,-1.));
#63873=DIRECTION('',(0.,0.,-1.));
#63874=DIRECTION('',(0.,0.,-1.));
#63875=DIRECTION('',(0.,0.,-1.));
#63876=DIRECTION('',(0.,0.,-1.));
#63877=DIRECTION('',(0.,0.,-1.));
#63878=DIRECTION('',(0.,0.,-1.));
#63879=DIRECTION('',(0.,0.,-1.));
#63880=DIRECTION('',(0.,0.,-1.));
#63881=DIRECTION('',(0.,0.,-1.));
#63882=DIRECTION('',(0.,0.,-1.));
#63883=DIRECTION('',(0.,0.,-1.));
#63884=DIRECTION('',(0.,0.,-1.));
#63885=DIRECTION('',(0.,0.,-1.));
#63886=DIRECTION('',(0.,0.,-1.));
#63887=DIRECTION('',(0.,0.,-1.));
#63888=DIRECTION('',(0.,0.,-1.));
#63889=DIRECTION('',(0.,0.,-1.));
#63890=DIRECTION('',(0.,0.,-1.));
#63891=DIRECTION('',(0.,0.,-1.));
#63892=DIRECTION('',(0.,0.,-1.));
#63893=DIRECTION('',(0.,0.,-1.));
#63894=DIRECTION('',(0.,0.,-1.));
#63895=DIRECTION('',(0.,0.,-1.));
#63896=DIRECTION('',(0.,0.,-1.));
#63897=DIRECTION('center_axis',(0.,0.,1.));
#63898=DIRECTION('ref_axis',(1.,0.,0.));
#63899=DIRECTION('center_axis',(0.,0.,1.));
#63900=DIRECTION('ref_axis',(0.,-1.,0.));
#63901=DIRECTION('center_axis',(0.,0.,1.));
#63902=DIRECTION('ref_axis',(0.,-1.,0.));
#63903=DIRECTION('center_axis',(0.,0.,1.));
#63904=DIRECTION('ref_axis',(0.,-1.,0.));
#63905=DIRECTION('',(0.,0.,-1.));
#63906=DIRECTION('',(0.,0.,-1.));
#63907=DIRECTION('',(0.,0.,-1.));
#63908=DIRECTION('',(0.,0.,-1.));
#63909=DIRECTION('',(0.,0.,-1.));
#63910=DIRECTION('',(0.,0.,-1.));
#63911=DIRECTION('',(0.,0.,-1.));
#63912=DIRECTION('',(0.,0.,-1.));
#63913=DIRECTION('',(0.,0.,-1.));
#63914=DIRECTION('',(0.,0.,-1.));
#63915=DIRECTION('',(0.,0.,-1.));
#63916=DIRECTION('',(0.,0.,-1.));
#63917=DIRECTION('',(0.,0.,-1.));
#63918=DIRECTION('',(0.,0.,-1.));
#63919=DIRECTION('',(0.,0.,-1.));
#63920=DIRECTION('',(0.,0.,-1.));
#63921=DIRECTION('',(0.,0.,-1.));
#63922=DIRECTION('',(0.,0.,-1.));
#63923=DIRECTION('',(0.,0.,-1.));
#63924=DIRECTION('',(0.,0.,-1.));
#63925=DIRECTION('center_axis',(0.,0.,1.));
#63926=DIRECTION('ref_axis',(1.,0.,0.));
#63927=DIRECTION('',(0.,0.,-1.));
#63928=DIRECTION('',(0.,0.,-1.));
#63929=DIRECTION('',(0.,0.,-1.));
#63930=DIRECTION('',(0.,0.,-1.));
#63931=DIRECTION('center_axis',(0.,-1.,0.));
#63932=DIRECTION('ref_axis',(-1.,0.,0.));
#63933=DIRECTION('',(-1.,0.,0.));
#63934=DIRECTION('',(0.,0.,-1.));
#63935=DIRECTION('',(-1.,0.,0.));
#63936=DIRECTION('',(0.,0.,-1.));
#63937=DIRECTION('',(0.,0.,-1.));
#63938=DIRECTION('',(0.,0.,-1.));
#63939=DIRECTION('center_axis',(1.,0.,0.));
#63940=DIRECTION('ref_axis',(0.,-1.,0.));
#63941=DIRECTION('',(0.,-1.,0.));
#63942=DIRECTION('',(0.,0.,-1.));
#63943=DIRECTION('',(0.,-1.,0.));
#63944=DIRECTION('center_axis',(0.,1.,0.));
#63945=DIRECTION('ref_axis',(1.,0.,0.));
#63946=DIRECTION('',(1.,0.,0.));
#63947=DIRECTION('',(0.,0.,-1.));
#63948=DIRECTION('',(1.,0.,0.));
#63949=DIRECTION('center_axis',(-1.,0.,0.));
#63950=DIRECTION('ref_axis',(0.,1.,0.));
#63951=DIRECTION('',(0.,1.,0.));
#63952=DIRECTION('',(0.,0.,-1.));
#63953=DIRECTION('',(0.,1.,0.));
#63954=DIRECTION('center_axis',(0.,-1.,0.));
#63955=DIRECTION('ref_axis',(-1.,0.,0.));
#63956=DIRECTION('',(-1.,0.,0.));
#63957=DIRECTION('',(-1.,0.,0.));
#63958=DIRECTION('center_axis',(0.,0.,1.));
#63959=DIRECTION('ref_axis',(1.,0.,0.));
#63960=DIRECTION('center_axis',(0.,0.,1.));
#63961=DIRECTION('ref_axis',(0.,-1.,0.));
#63962=DIRECTION('',(0.,0.,-1.));
#63963=DIRECTION('',(0.,0.,-1.));
#63964=DIRECTION('',(0.,0.,-1.));
#63965=DIRECTION('',(0.,0.,-1.));
#63966=DIRECTION('',(0.,0.,-1.));
#63967=DIRECTION('',(0.,0.,-1.));
#63968=DIRECTION('',(0.,0.,-1.));
#63969=DIRECTION('',(0.,0.,-1.));
#63970=DIRECTION('',(0.,0.,-1.));
#63971=DIRECTION('',(0.,0.,-1.));
#63972=DIRECTION('',(0.,0.,-1.));
#63973=DIRECTION('',(0.,0.,-1.));
#63974=DIRECTION('',(0.,0.,-1.));
#63975=DIRECTION('',(0.,0.,-1.));
#63976=DIRECTION('',(0.,0.,-1.));
#63977=DIRECTION('',(0.,0.,-1.));
#63978=DIRECTION('',(0.,0.,-1.));
#63979=DIRECTION('',(0.,0.,-1.));
#63980=DIRECTION('',(0.,0.,-1.));
#63981=DIRECTION('',(0.,0.,-1.));
#63982=DIRECTION('center_axis',(0.,0.,1.));
#63983=DIRECTION('ref_axis',(1.,0.,0.));
#63984=DIRECTION('',(0.,0.,-1.));
#63985=DIRECTION('',(0.,0.,-1.));
#63986=DIRECTION('',(0.,0.,-1.));
#63987=DIRECTION('',(0.,0.,-1.));
#63988=DIRECTION('',(0.,0.,-1.));
#63989=DIRECTION('',(0.,0.,-1.));
#63990=DIRECTION('',(0.,0.,-1.));
#63991=DIRECTION('',(0.,0.,-1.));
#63992=DIRECTION('',(0.,0.,-1.));
#63993=DIRECTION('',(0.,0.,-1.));
#63994=DIRECTION('',(0.,0.,-1.));
#63995=DIRECTION('',(0.,0.,-1.));
#63996=DIRECTION('',(0.,0.,-1.));
#63997=DIRECTION('',(0.,0.,-1.));
#63998=DIRECTION('',(0.,0.,-1.));
#63999=DIRECTION('',(0.,0.,-1.));
#64000=DIRECTION('',(0.,0.,-1.));
#64001=DIRECTION('',(0.,0.,-1.));
#64002=DIRECTION('',(0.,0.,-1.));
#64003=DIRECTION('',(0.,0.,-1.));
#64004=DIRECTION('',(0.,0.,-1.));
#64005=DIRECTION('',(0.,0.,-1.));
#64006=DIRECTION('',(0.,0.,-1.));
#64007=DIRECTION('',(0.,0.,-1.));
#64008=DIRECTION('',(0.,0.,-1.));
#64009=DIRECTION('',(0.,0.,-1.));
#64010=DIRECTION('',(0.,0.,-1.));
#64011=DIRECTION('center_axis',(0.0779743449792121,-0.99695536586402,0.));
#64012=DIRECTION('ref_axis',(-0.99695536586402,-0.0779743449792121,0.));
#64013=DIRECTION('',(-0.99695536586402,-0.0779743449792121,0.));
#64014=DIRECTION('',(0.,0.,-1.));
#64015=DIRECTION('',(-0.99695536586402,-0.0779743449792121,0.));
#64016=DIRECTION('center_axis',(0.,0.,1.));
#64017=DIRECTION('ref_axis',(1.,0.,0.));
#64018=DIRECTION('center_axis',(0.,0.,1.));
#64019=DIRECTION('ref_axis',(0.,-1.,0.));
#64020=DIRECTION('center_axis',(0.,0.,1.));
#64021=DIRECTION('ref_axis',(0.,-1.,0.));
#64022=DIRECTION('',(0.,0.,-1.));
#64023=DIRECTION('',(0.,0.,-1.));
#64024=DIRECTION('',(0.,0.,-1.));
#64025=DIRECTION('',(0.,0.,-1.));
#64026=DIRECTION('',(0.,0.,-1.));
#64027=DIRECTION('',(0.,0.,-1.));
#64028=DIRECTION('',(0.,0.,-1.));
#64029=DIRECTION('',(0.,0.,-1.));
#64030=DIRECTION('',(0.,0.,-1.));
#64031=DIRECTION('',(0.,0.,-1.));
#64032=DIRECTION('',(0.,0.,-1.));
#64033=DIRECTION('',(0.,0.,-1.));
#64034=DIRECTION('',(0.,0.,-1.));
#64035=DIRECTION('',(0.,0.,-1.));
#64036=DIRECTION('',(0.,0.,-1.));
#64037=DIRECTION('',(0.,0.,-1.));
#64038=DIRECTION('',(0.,0.,-1.));
#64039=DIRECTION('',(0.,0.,-1.));
#64040=DIRECTION('',(0.,0.,-1.));
#64041=DIRECTION('',(0.,0.,-1.));
#64042=DIRECTION('center_axis',(0.,0.,1.));
#64043=DIRECTION('ref_axis',(1.,0.,0.));
#64044=DIRECTION('',(0.,0.,-1.));
#64045=DIRECTION('',(0.,0.,-1.));
#64046=DIRECTION('',(0.,0.,-1.));
#64047=DIRECTION('',(0.,0.,-1.));
#64048=DIRECTION('',(0.,0.,-1.));
#64049=DIRECTION('',(0.,0.,-1.));
#64050=DIRECTION('',(0.,0.,-1.));
#64051=DIRECTION('center_axis',(0.980484873509324,-0.196594539139329,0.));
#64052=DIRECTION('ref_axis',(-0.196594539139329,-0.980484873509324,0.));
#64053=DIRECTION('',(-0.196594539139329,-0.980484873509324,0.));
#64054=DIRECTION('',(0.,0.,-1.));
#64055=DIRECTION('',(-0.196594539139329,-0.980484873509324,0.));
#64056=DIRECTION('center_axis',(0.,-1.,0.));
#64057=DIRECTION('ref_axis',(-1.,0.,0.));
#64058=DIRECTION('',(-1.,0.,0.));
#64059=DIRECTION('',(0.,0.,-1.));
#64060=DIRECTION('',(-1.,0.,0.));
#64061=DIRECTION('center_axis',(1.,0.,0.));
#64062=DIRECTION('ref_axis',(0.,-1.,0.));
#64063=DIRECTION('',(0.,-1.,0.));
#64064=DIRECTION('',(0.,0.,-1.));
#64065=DIRECTION('',(0.,-1.,0.));
#64066=DIRECTION('center_axis',(0.,1.,0.));
#64067=DIRECTION('ref_axis',(1.,0.,0.));
#64068=DIRECTION('',(1.,0.,0.));
#64069=DIRECTION('',(0.,0.,-1.));
#64070=DIRECTION('',(1.,0.,0.));
#64071=DIRECTION('center_axis',(-0.982679588991295,0.185312777163097,0.));
#64072=DIRECTION('ref_axis',(0.185312777163097,0.982679588991295,0.));
#64073=DIRECTION('',(0.185312777163097,0.982679588991295,0.));
#64074=DIRECTION('',(0.,0.,-1.));
#64075=DIRECTION('',(0.185312777163097,0.982679588991295,0.));
#64076=DIRECTION('center_axis',(-0.129088379836863,-0.991633092525201,0.));
#64077=DIRECTION('ref_axis',(-0.991633092525201,0.129088379836863,0.));
#64078=DIRECTION('',(-0.991633092525201,0.129088379836863,0.));
#64079=DIRECTION('',(0.,0.,-1.));
#64080=DIRECTION('',(-0.991633092525201,0.129088379836863,0.));
#64081=DIRECTION('',(0.,0.,-1.));
#64082=DIRECTION('',(0.,0.,-1.));
#64083=DIRECTION('',(0.,0.,-1.));
#64084=DIRECTION('',(0.,0.,-1.));
#64085=DIRECTION('',(0.,0.,-1.));
#64086=DIRECTION('',(0.,0.,-1.));
#64087=DIRECTION('',(0.,0.,-1.));
#64088=DIRECTION('',(0.,0.,-1.));
#64089=DIRECTION('center_axis',(-0.0843540635911639,0.99643584437517,0.));
#64090=DIRECTION('ref_axis',(0.99643584437517,0.0843540635911639,0.));
#64091=DIRECTION('',(0.99643584437517,0.0843540635911639,0.));
#64092=DIRECTION('',(0.,0.,-1.));
#64093=DIRECTION('',(0.99643584437517,0.0843540635911639,0.));
#64094=DIRECTION('center_axis',(0.,0.,1.));
#64095=DIRECTION('ref_axis',(1.,0.,0.));
#64096=DIRECTION('center_axis',(0.,0.,1.));
#64097=DIRECTION('ref_axis',(0.,-1.,0.));
#64098=DIRECTION('',(0.,0.,-1.));
#64099=DIRECTION('',(0.,0.,-1.));
#64100=DIRECTION('',(0.,0.,-1.));
#64101=DIRECTION('',(0.,0.,-1.));
#64102=DIRECTION('',(0.,0.,-1.));
#64103=DIRECTION('',(0.,0.,-1.));
#64104=DIRECTION('',(0.,0.,-1.));
#64105=DIRECTION('',(0.,0.,-1.));
#64106=DIRECTION('',(0.,0.,-1.));
#64107=DIRECTION('',(0.,0.,-1.));
#64108=DIRECTION('',(0.,0.,-1.));
#64109=DIRECTION('',(0.,0.,-1.));
#64110=DIRECTION('',(0.,0.,-1.));
#64111=DIRECTION('',(0.,0.,-1.));
#64112=DIRECTION('',(0.,0.,-1.));
#64113=DIRECTION('',(0.,0.,-1.));
#64114=DIRECTION('',(0.,0.,-1.));
#64115=DIRECTION('',(0.,0.,-1.));
#64116=DIRECTION('',(0.,0.,-1.));
#64117=DIRECTION('',(0.,0.,-1.));
#64118=DIRECTION('center_axis',(0.,0.,1.));
#64119=DIRECTION('ref_axis',(1.,0.,0.));
#64120=DIRECTION('center_axis',(0.821386116423605,-0.570372551712079,0.));
#64121=DIRECTION('ref_axis',(-0.570372551712079,-0.821386116423605,0.));
#64122=DIRECTION('',(-0.570372551712079,-0.821386116423605,0.));
#64123=DIRECTION('',(0.,0.,-1.));
#64124=DIRECTION('',(-0.570372551712079,-0.821386116423605,0.));
#64125=DIRECTION('',(0.,0.,-1.));
#64126=DIRECTION('center_axis',(-1.,0.,0.));
#64127=DIRECTION('ref_axis',(0.,1.,0.));
#64128=DIRECTION('',(0.,1.,0.));
#64129=DIRECTION('',(0.,0.,-1.));
#64130=DIRECTION('',(0.,1.,0.));
#64131=DIRECTION('center_axis',(0.,1.,0.));
#64132=DIRECTION('ref_axis',(1.,0.,0.));
#64133=DIRECTION('',(1.,0.,0.));
#64134=DIRECTION('',(1.,0.,0.));
#64135=DIRECTION('center_axis',(1.,0.,0.));
#64136=DIRECTION('ref_axis',(0.,-1.,0.));
#64137=DIRECTION('',(0.,-1.,0.));
#64138=DIRECTION('',(0.,0.,-1.));
#64139=DIRECTION('',(0.,-1.,0.));
#64140=DIRECTION('',(0.,0.,-1.));
#64141=DIRECTION('center_axis',(0.,-1.,0.));
#64142=DIRECTION('ref_axis',(-1.,0.,0.));
#64143=DIRECTION('',(-1.,0.,0.));
#64144=DIRECTION('',(0.,0.,-1.));
#64145=DIRECTION('',(-1.,0.,0.));
#64146=DIRECTION('center_axis',(1.,0.,0.));
#64147=DIRECTION('ref_axis',(0.,-1.,0.));
#64148=DIRECTION('',(0.,-1.,0.));
#64149=DIRECTION('',(0.,0.,-1.));
#64150=DIRECTION('',(0.,-1.,0.));
#64151=DIRECTION('center_axis',(0.,1.,0.));
#64152=DIRECTION('ref_axis',(1.,0.,0.));
#64153=DIRECTION('',(1.,0.,0.));
#64154=DIRECTION('',(0.,0.,-1.));
#64155=DIRECTION('',(1.,0.,0.));
#64156=DIRECTION('center_axis',(1.,0.,0.));
#64157=DIRECTION('ref_axis',(0.,-1.,0.));
#64158=DIRECTION('',(0.,-1.,0.));
#64159=DIRECTION('',(0.,0.,-1.));
#64160=DIRECTION('',(0.,-1.,0.));
#64161=DIRECTION('center_axis',(0.,1.,0.));
#64162=DIRECTION('ref_axis',(1.,0.,0.));
#64163=DIRECTION('',(1.,0.,0.));
#64164=DIRECTION('',(0.,0.,-1.));
#64165=DIRECTION('',(1.,0.,0.));
#64166=DIRECTION('center_axis',(-0.817611346967032,0.575770514450641,0.));
#64167=DIRECTION('ref_axis',(0.575770514450641,0.817611346967032,0.));
#64168=DIRECTION('',(0.575770514450641,0.817611346967032,0.));
#64169=DIRECTION('',(0.,0.,-1.));
#64170=DIRECTION('',(0.575770514450641,0.817611346967032,0.));
#64171=DIRECTION('center_axis',(-1.,0.,0.));
#64172=DIRECTION('ref_axis',(0.,1.,0.));
#64173=DIRECTION('',(0.,1.,0.));
#64174=DIRECTION('',(0.,0.,-1.));
#64175=DIRECTION('',(0.,1.,0.));
#64176=DIRECTION('center_axis',(0.,-1.,0.));
#64177=DIRECTION('ref_axis',(-1.,0.,0.));
#64178=DIRECTION('',(-1.,0.,0.));
#64179=DIRECTION('',(0.,0.,-1.));
#64180=DIRECTION('',(-1.,0.,0.));
#64181=DIRECTION('center_axis',(-1.,0.,0.));
#64182=DIRECTION('ref_axis',(0.,1.,0.));
#64183=DIRECTION('',(0.,1.,0.));
#64184=DIRECTION('',(0.,0.,-1.));
#64185=DIRECTION('',(0.,1.,0.));
#64186=DIRECTION('center_axis',(0.,-1.,0.));
#64187=DIRECTION('ref_axis',(-1.,0.,0.));
#64188=DIRECTION('',(-1.,0.,0.));
#64189=DIRECTION('',(-1.,0.,0.));
#64190=DIRECTION('center_axis',(0.,0.,-1.));
#64191=DIRECTION('ref_axis',(-1.,0.,0.));
#64192=DIRECTION('center_axis',(0.,0.,1.));
#64193=DIRECTION('ref_axis',(0.,-1.,0.));
#64194=DIRECTION('center_axis',(0.,0.,1.));
#64195=DIRECTION('ref_axis',(0.,-1.,0.));
#64196=DIRECTION('',(0.,0.,-1.));
#64197=DIRECTION('',(0.,0.,-1.));
#64198=DIRECTION('',(0.,0.,-1.));
#64199=DIRECTION('',(0.,0.,-1.));
#64200=DIRECTION('',(0.,0.,-1.));
#64201=DIRECTION('',(0.,0.,-1.));
#64202=DIRECTION('',(0.,0.,-1.));
#64203=DIRECTION('',(0.,0.,-1.));
#64204=DIRECTION('',(0.,0.,-1.));
#64205=DIRECTION('',(0.,0.,-1.));
#64206=DIRECTION('',(0.,0.,-1.));
#64207=DIRECTION('',(0.,0.,-1.));
#64208=DIRECTION('',(0.,0.,-1.));
#64209=DIRECTION('',(0.,0.,-1.));
#64210=DIRECTION('',(0.,0.,-1.));
#64211=DIRECTION('',(0.,0.,-1.));
#64212=DIRECTION('',(0.,0.,-1.));
#64213=DIRECTION('',(0.,0.,-1.));
#64214=DIRECTION('',(0.,0.,-1.));
#64215=DIRECTION('',(0.,0.,-1.));
#64216=DIRECTION('center_axis',(0.,0.,1.));
#64217=DIRECTION('ref_axis',(1.,0.,0.));
#64218=DIRECTION('',(0.,0.,-1.));
#64219=DIRECTION('',(0.,0.,-1.));
#64220=DIRECTION('',(0.,0.,-1.));
#64221=DIRECTION('',(0.,0.,-1.));
#64222=DIRECTION('',(0.,0.,-1.));
#64223=DIRECTION('',(0.,0.,-1.));
#64224=DIRECTION('',(0.,0.,-1.));
#64225=DIRECTION('',(0.,0.,-1.));
#64226=DIRECTION('',(0.,0.,-1.));
#64227=DIRECTION('',(0.,0.,-1.));
#64228=DIRECTION('',(0.,0.,-1.));
#64229=DIRECTION('',(0.,0.,-1.));
#64230=DIRECTION('',(0.,0.,-1.));
#64231=DIRECTION('center_axis',(-0.175033346417238,-0.984562505705952,0.));
#64232=DIRECTION('ref_axis',(-0.984562505705952,0.175033346417238,0.));
#64233=DIRECTION('',(-0.984562505705952,0.175033346417238,0.));
#64234=DIRECTION('',(0.,0.,-1.));
#64235=DIRECTION('',(-0.984562505705952,0.175033346417238,0.));
#64236=DIRECTION('',(0.,0.,-1.));
#64237=DIRECTION('',(0.,0.,-1.));
#64238=DIRECTION('',(0.,0.,-1.));
#64239=DIRECTION('',(0.,0.,-1.));
#64240=DIRECTION('',(0.,0.,-1.));
#64241=DIRECTION('',(0.,0.,-1.));
#64242=DIRECTION('',(0.,0.,-1.));
#64243=DIRECTION('center_axis',(-0.992083480553514,0.125580124274607,0.));
#64244=DIRECTION('ref_axis',(0.125580124274607,0.992083480553514,0.));
#64245=DIRECTION('',(0.125580124274607,0.992083480553514,0.));
#64246=DIRECTION('',(0.,0.,-1.));
#64247=DIRECTION('',(0.125580124274607,0.992083480553514,0.));
#64248=DIRECTION('',(0.,0.,-1.));
#64249=DIRECTION('',(0.,0.,-1.));
#64250=DIRECTION('',(0.,0.,-1.));
#64251=DIRECTION('',(0.,0.,-1.));
#64252=DIRECTION('',(0.,0.,-1.));
#64253=DIRECTION('',(0.,0.,-1.));
#64254=DIRECTION('',(0.,0.,-1.));
#64255=DIRECTION('center_axis',(-0.132163863358704,0.991227881580266,0.));
#64256=DIRECTION('ref_axis',(0.991227881580266,0.132163863358704,0.));
#64257=DIRECTION('',(0.991227881580266,0.132163863358704,0.));
#64258=DIRECTION('',(0.,0.,-1.));
#64259=DIRECTION('',(0.991227881580266,0.132163863358704,0.));
#64260=DIRECTION('center_axis',(0.,0.,1.));
#64261=DIRECTION('ref_axis',(1.,0.,0.));
#64262=DIRECTION('center_axis',(0.,0.,1.));
#64263=DIRECTION('ref_axis',(0.,-1.,0.));
#64264=DIRECTION('',(0.,0.,-1.));
#64265=DIRECTION('',(0.,0.,-1.));
#64266=DIRECTION('',(0.,0.,-1.));
#64267=DIRECTION('',(0.,0.,-1.));
#64268=DIRECTION('',(0.,0.,-1.));
#64269=DIRECTION('',(0.,0.,-1.));
#64270=DIRECTION('',(0.,0.,-1.));
#64271=DIRECTION('',(0.,0.,-1.));
#64272=DIRECTION('',(0.,0.,-1.));
#64273=DIRECTION('',(0.,0.,-1.));
#64274=DIRECTION('',(0.,0.,-1.));
#64275=DIRECTION('',(0.,0.,-1.));
#64276=DIRECTION('',(0.,0.,-1.));
#64277=DIRECTION('',(0.,0.,-1.));
#64278=DIRECTION('',(0.,0.,-1.));
#64279=DIRECTION('',(0.,0.,-1.));
#64280=DIRECTION('',(0.,0.,-1.));
#64281=DIRECTION('',(0.,0.,-1.));
#64282=DIRECTION('',(0.,0.,-1.));
#64283=DIRECTION('',(0.,0.,-1.));
#64284=DIRECTION('center_axis',(0.,0.,1.));
#64285=DIRECTION('ref_axis',(1.,0.,0.));
#64286=DIRECTION('',(0.,0.,-1.));
#64287=DIRECTION('',(0.,0.,-1.));
#64288=DIRECTION('',(0.,0.,-1.));
#64289=DIRECTION('',(0.,0.,-1.));
#64290=DIRECTION('',(0.,0.,-1.));
#64291=DIRECTION('',(0.,0.,-1.));
#64292=DIRECTION('',(0.,0.,-1.));
#64293=DIRECTION('',(0.,0.,-1.));
#64294=DIRECTION('',(0.,0.,-1.));
#64295=DIRECTION('',(0.,0.,-1.));
#64296=DIRECTION('center_axis',(-0.102165169950561,-0.99476744923071,0.));
#64297=DIRECTION('ref_axis',(-0.99476744923071,0.102165169950561,0.));
#64298=DIRECTION('',(-0.99476744923071,0.102165169950561,0.));
#64299=DIRECTION('',(0.,0.,-1.));
#64300=DIRECTION('',(-0.99476744923071,0.102165169950561,0.));
#64301=DIRECTION('',(0.,0.,-1.));
#64302=DIRECTION('',(0.,0.,-1.));
#64303=DIRECTION('',(0.,0.,-1.));
#64304=DIRECTION('',(0.,0.,-1.));
#64305=DIRECTION('',(0.,0.,-1.));
#64306=DIRECTION('',(0.,0.,-1.));
#64307=DIRECTION('',(0.,0.,-1.));
#64308=DIRECTION('',(0.,0.,-1.));
#64309=DIRECTION('',(0.,0.,-1.));
#64310=DIRECTION('center_axis',(0.,-1.,0.));
#64311=DIRECTION('ref_axis',(-1.,0.,0.));
#64312=DIRECTION('',(-1.,0.,0.));
#64313=DIRECTION('',(0.,0.,-1.));
#64314=DIRECTION('',(-1.,0.,0.));
#64315=DIRECTION('center_axis',(1.,0.,0.));
#64316=DIRECTION('ref_axis',(0.,-1.,0.));
#64317=DIRECTION('',(0.,-1.,0.));
#64318=DIRECTION('',(0.,0.,-1.));
#64319=DIRECTION('',(0.,-1.,0.));
#64320=DIRECTION('center_axis',(0.,1.,0.));
#64321=DIRECTION('ref_axis',(1.,0.,0.));
#64322=DIRECTION('',(1.,0.,0.));
#64323=DIRECTION('',(1.,0.,0.));
#64324=DIRECTION('center_axis',(0.,0.,1.));
#64325=DIRECTION('ref_axis',(1.,0.,0.));
#64326=DIRECTION('center_axis',(0.,0.,1.));
#64327=DIRECTION('ref_axis',(0.,-1.,0.));
#64328=DIRECTION('',(0.,0.,-1.));
#64329=DIRECTION('',(0.,0.,-1.));
#64330=DIRECTION('',(0.,0.,-1.));
#64331=DIRECTION('',(0.,0.,-1.));
#64332=DIRECTION('',(0.,0.,-1.));
#64333=DIRECTION('',(0.,0.,-1.));
#64334=DIRECTION('',(0.,0.,-1.));
#64335=DIRECTION('',(0.,0.,-1.));
#64336=DIRECTION('',(0.,0.,-1.));
#64337=DIRECTION('',(0.,0.,-1.));
#64338=DIRECTION('',(0.,0.,-1.));
#64339=DIRECTION('',(0.,0.,-1.));
#64340=DIRECTION('',(0.,0.,-1.));
#64341=DIRECTION('',(0.,0.,-1.));
#64342=DIRECTION('',(0.,0.,-1.));
#64343=DIRECTION('',(0.,0.,-1.));
#64344=DIRECTION('',(0.,0.,-1.));
#64345=DIRECTION('',(0.,0.,-1.));
#64346=DIRECTION('',(0.,0.,-1.));
#64347=DIRECTION('',(0.,0.,-1.));
#64348=DIRECTION('center_axis',(0.,0.,1.));
#64349=DIRECTION('ref_axis',(1.,0.,0.));
#64350=DIRECTION('center_axis',(0.,1.,0.));
#64351=DIRECTION('ref_axis',(1.,0.,0.));
#64352=DIRECTION('',(1.,0.,0.));
#64353=DIRECTION('',(0.,0.,-1.));
#64354=DIRECTION('',(1.,0.,0.));
#64355=DIRECTION('',(0.,0.,-1.));
#64356=DIRECTION('',(0.,0.,-1.));
#64357=DIRECTION('',(0.,0.,-1.));
#64358=DIRECTION('center_axis',(-1.,0.,0.));
#64359=DIRECTION('ref_axis',(0.,1.,0.));
#64360=DIRECTION('',(0.,1.,0.));
#64361=DIRECTION('',(0.,0.,-1.));
#64362=DIRECTION('',(0.,1.,0.));
#64363=DIRECTION('',(0.,0.,-1.));
#64364=DIRECTION('',(0.,0.,-1.));
#64365=DIRECTION('center_axis',(-1.,0.,0.));
#64366=DIRECTION('ref_axis',(0.,1.,0.));
#64367=DIRECTION('',(0.,1.,0.));
#64368=DIRECTION('',(0.,0.,-1.));
#64369=DIRECTION('',(0.,1.,0.));
#64370=DIRECTION('center_axis',(0.,-1.,0.));
#64371=DIRECTION('ref_axis',(-1.,0.,0.));
#64372=DIRECTION('',(-1.,0.,0.));
#64373=DIRECTION('',(0.,0.,-1.));
#64374=DIRECTION('',(-1.,0.,0.));
#64375=DIRECTION('center_axis',(1.,0.,0.));
#64376=DIRECTION('ref_axis',(0.,-1.,0.));
#64377=DIRECTION('',(0.,-1.,0.));
#64378=DIRECTION('',(0.,-1.,0.));
#64379=DIRECTION('center_axis',(0.,0.,1.));
#64380=DIRECTION('ref_axis',(1.,0.,0.));
#64381=DIRECTION('center_axis',(0.,0.,1.));
#64382=DIRECTION('ref_axis',(0.,-1.,0.));
#64383=DIRECTION('',(0.,0.,-1.));
#64384=DIRECTION('',(0.,0.,-1.));
#64385=DIRECTION('',(0.,0.,-1.));
#64386=DIRECTION('',(0.,0.,-1.));
#64387=DIRECTION('',(0.,0.,-1.));
#64388=DIRECTION('',(0.,0.,-1.));
#64389=DIRECTION('',(0.,0.,-1.));
#64390=DIRECTION('',(0.,0.,-1.));
#64391=DIRECTION('',(0.,0.,-1.));
#64392=DIRECTION('',(0.,0.,-1.));
#64393=DIRECTION('',(0.,0.,-1.));
#64394=DIRECTION('',(0.,0.,-1.));
#64395=DIRECTION('',(0.,0.,-1.));
#64396=DIRECTION('',(0.,0.,-1.));
#64397=DIRECTION('',(0.,0.,-1.));
#64398=DIRECTION('',(0.,0.,-1.));
#64399=DIRECTION('',(0.,0.,-1.));
#64400=DIRECTION('',(0.,0.,-1.));
#64401=DIRECTION('',(0.,0.,-1.));
#64402=DIRECTION('',(0.,0.,-1.));
#64403=DIRECTION('center_axis',(0.,0.,1.));
#64404=DIRECTION('ref_axis',(1.,0.,0.));
#64405=DIRECTION('center_axis',(0.,0.,1.));
#64406=DIRECTION('ref_axis',(0.,-1.,0.));
#64407=DIRECTION('',(0.,0.,-1.));
#64408=DIRECTION('',(0.,0.,-1.));
#64409=DIRECTION('',(0.,0.,-1.));
#64410=DIRECTION('',(0.,0.,-1.));
#64411=DIRECTION('',(0.,0.,-1.));
#64412=DIRECTION('',(0.,0.,-1.));
#64413=DIRECTION('',(0.,0.,-1.));
#64414=DIRECTION('',(0.,0.,-1.));
#64415=DIRECTION('',(0.,0.,-1.));
#64416=DIRECTION('',(0.,0.,-1.));
#64417=DIRECTION('',(0.,0.,-1.));
#64418=DIRECTION('',(0.,0.,-1.));
#64419=DIRECTION('',(0.,0.,-1.));
#64420=DIRECTION('',(0.,0.,-1.));
#64421=DIRECTION('',(0.,0.,-1.));
#64422=DIRECTION('',(0.,0.,-1.));
#64423=DIRECTION('',(0.,0.,-1.));
#64424=DIRECTION('',(0.,0.,-1.));
#64425=DIRECTION('',(0.,0.,-1.));
#64426=DIRECTION('',(0.,0.,-1.));
#64427=DIRECTION('center_axis',(0.,0.,1.));
#64428=DIRECTION('ref_axis',(1.,0.,0.));
#64429=DIRECTION('center_axis',(0.,1.,0.));
#64430=DIRECTION('ref_axis',(1.,0.,0.));
#64431=DIRECTION('',(1.,0.,0.));
#64432=DIRECTION('',(0.,0.,-1.));
#64433=DIRECTION('',(1.,0.,0.));
#64434=DIRECTION('',(0.,0.,-1.));
#64435=DIRECTION('',(0.,0.,-1.));
#64436=DIRECTION('',(0.,0.,-1.));
#64437=DIRECTION('center_axis',(-1.,0.,0.));
#64438=DIRECTION('ref_axis',(0.,1.,0.));
#64439=DIRECTION('',(0.,1.,0.));
#64440=DIRECTION('',(0.,0.,-1.));
#64441=DIRECTION('',(0.,1.,0.));
#64442=DIRECTION('',(0.,0.,-1.));
#64443=DIRECTION('',(0.,0.,-1.));
#64444=DIRECTION('center_axis',(-1.,0.,0.));
#64445=DIRECTION('ref_axis',(0.,1.,0.));
#64446=DIRECTION('',(0.,1.,0.));
#64447=DIRECTION('',(0.,0.,-1.));
#64448=DIRECTION('',(0.,1.,0.));
#64449=DIRECTION('center_axis',(0.,-1.,0.));
#64450=DIRECTION('ref_axis',(-1.,0.,0.));
#64451=DIRECTION('',(-1.,0.,0.));
#64452=DIRECTION('',(0.,0.,-1.));
#64453=DIRECTION('',(-1.,0.,0.));
#64454=DIRECTION('center_axis',(1.,0.,0.));
#64455=DIRECTION('ref_axis',(0.,-1.,0.));
#64456=DIRECTION('',(0.,-1.,0.));
#64457=DIRECTION('',(0.,-1.,0.));
#64458=DIRECTION('center_axis',(0.,0.,1.));
#64459=DIRECTION('ref_axis',(1.,0.,0.));
#64460=DIRECTION('center_axis',(0.,0.,1.));
#64461=DIRECTION('ref_axis',(0.,-1.,0.));
#64462=DIRECTION('',(0.,0.,-1.));
#64463=DIRECTION('',(0.,0.,-1.));
#64464=DIRECTION('',(0.,0.,-1.));
#64465=DIRECTION('',(0.,0.,-1.));
#64466=DIRECTION('',(0.,0.,-1.));
#64467=DIRECTION('',(0.,0.,-1.));
#64468=DIRECTION('',(0.,0.,-1.));
#64469=DIRECTION('',(0.,0.,-1.));
#64470=DIRECTION('',(0.,0.,-1.));
#64471=DIRECTION('',(0.,0.,-1.));
#64472=DIRECTION('',(0.,0.,-1.));
#64473=DIRECTION('',(0.,0.,-1.));
#64474=DIRECTION('',(0.,0.,-1.));
#64475=DIRECTION('',(0.,0.,-1.));
#64476=DIRECTION('',(0.,0.,-1.));
#64477=DIRECTION('',(0.,0.,-1.));
#64478=DIRECTION('',(0.,0.,-1.));
#64479=DIRECTION('',(0.,0.,-1.));
#64480=DIRECTION('',(0.,0.,-1.));
#64481=DIRECTION('',(0.,0.,-1.));
#64482=DIRECTION('center_axis',(0.,0.,1.));
#64483=DIRECTION('ref_axis',(1.,0.,0.));
#64484=DIRECTION('',(0.,0.,-1.));
#64485=DIRECTION('',(0.,0.,-1.));
#64486=DIRECTION('',(0.,0.,-1.));
#64487=DIRECTION('',(0.,0.,-1.));
#64488=DIRECTION('',(0.,0.,-1.));
#64489=DIRECTION('',(0.,0.,-1.));
#64490=DIRECTION('',(0.,0.,-1.));
#64491=DIRECTION('',(0.,0.,-1.));
#64492=DIRECTION('',(0.,0.,-1.));
#64493=DIRECTION('',(0.,0.,-1.));
#64494=DIRECTION('center_axis',(-0.102165169950561,-0.99476744923071,0.));
#64495=DIRECTION('ref_axis',(-0.99476744923071,0.102165169950561,0.));
#64496=DIRECTION('',(-0.99476744923071,0.102165169950561,0.));
#64497=DIRECTION('',(0.,0.,-1.));
#64498=DIRECTION('',(-0.99476744923071,0.102165169950561,0.));
#64499=DIRECTION('',(0.,0.,-1.));
#64500=DIRECTION('',(0.,0.,-1.));
#64501=DIRECTION('',(0.,0.,-1.));
#64502=DIRECTION('',(0.,0.,-1.));
#64503=DIRECTION('',(0.,0.,-1.));
#64504=DIRECTION('',(0.,0.,-1.));
#64505=DIRECTION('',(0.,0.,-1.));
#64506=DIRECTION('',(0.,0.,-1.));
#64507=DIRECTION('',(0.,0.,-1.));
#64508=DIRECTION('center_axis',(0.,-1.,0.));
#64509=DIRECTION('ref_axis',(-1.,0.,0.));
#64510=DIRECTION('',(-1.,0.,0.));
#64511=DIRECTION('',(0.,0.,-1.));
#64512=DIRECTION('',(-1.,0.,0.));
#64513=DIRECTION('center_axis',(1.,0.,0.));
#64514=DIRECTION('ref_axis',(0.,-1.,0.));
#64515=DIRECTION('',(0.,-1.,0.));
#64516=DIRECTION('',(0.,0.,-1.));
#64517=DIRECTION('',(0.,-1.,0.));
#64518=DIRECTION('center_axis',(0.,1.,0.));
#64519=DIRECTION('ref_axis',(1.,0.,0.));
#64520=DIRECTION('',(1.,0.,0.));
#64521=DIRECTION('',(1.,0.,0.));
#64522=DIRECTION('center_axis',(0.,0.,1.));
#64523=DIRECTION('ref_axis',(1.,0.,0.));
#64524=DIRECTION('center_axis',(0.,0.,1.));
#64525=DIRECTION('ref_axis',(0.,-1.,0.));
#64526=DIRECTION('',(0.,0.,-1.));
#64527=DIRECTION('',(0.,0.,-1.));
#64528=DIRECTION('',(0.,0.,-1.));
#64529=DIRECTION('',(0.,0.,-1.));
#64530=DIRECTION('',(0.,0.,-1.));
#64531=DIRECTION('',(0.,0.,-1.));
#64532=DIRECTION('',(0.,0.,-1.));
#64533=DIRECTION('',(0.,0.,-1.));
#64534=DIRECTION('',(0.,0.,-1.));
#64535=DIRECTION('',(0.,0.,-1.));
#64536=DIRECTION('',(0.,0.,-1.));
#64537=DIRECTION('',(0.,0.,-1.));
#64538=DIRECTION('',(0.,0.,-1.));
#64539=DIRECTION('',(0.,0.,-1.));
#64540=DIRECTION('',(0.,0.,-1.));
#64541=DIRECTION('',(0.,0.,-1.));
#64542=DIRECTION('',(0.,0.,-1.));
#64543=DIRECTION('',(0.,0.,-1.));
#64544=DIRECTION('',(0.,0.,-1.));
#64545=DIRECTION('',(0.,0.,-1.));
#64546=DIRECTION('center_axis',(0.,0.,1.));
#64547=DIRECTION('ref_axis',(1.,0.,0.));
#64548=DIRECTION('',(0.,0.,-1.));
#64549=DIRECTION('',(0.,0.,-1.));
#64550=DIRECTION('',(0.,0.,-1.));
#64551=DIRECTION('',(0.,0.,-1.));
#64552=DIRECTION('',(0.,0.,-1.));
#64553=DIRECTION('',(0.,0.,-1.));
#64554=DIRECTION('',(0.,0.,-1.));
#64555=DIRECTION('',(0.,0.,-1.));
#64556=DIRECTION('',(0.,0.,-1.));
#64557=DIRECTION('',(0.,0.,-1.));
#64558=DIRECTION('',(0.,0.,-1.));
#64559=DIRECTION('',(0.,0.,-1.));
#64560=DIRECTION('',(0.,0.,-1.));
#64561=DIRECTION('center_axis',(-0.175033346417238,-0.984562505705952,0.));
#64562=DIRECTION('ref_axis',(-0.984562505705952,0.175033346417238,0.));
#64563=DIRECTION('',(-0.984562505705952,0.175033346417238,0.));
#64564=DIRECTION('',(0.,0.,-1.));
#64565=DIRECTION('',(-0.984562505705952,0.175033346417238,0.));
#64566=DIRECTION('',(0.,0.,-1.));
#64567=DIRECTION('',(0.,0.,-1.));
#64568=DIRECTION('',(0.,0.,-1.));
#64569=DIRECTION('',(0.,0.,-1.));
#64570=DIRECTION('',(0.,0.,-1.));
#64571=DIRECTION('',(0.,0.,-1.));
#64572=DIRECTION('',(0.,0.,-1.));
#64573=DIRECTION('center_axis',(-0.992083480553514,0.125580124274607,0.));
#64574=DIRECTION('ref_axis',(0.125580124274607,0.992083480553514,0.));
#64575=DIRECTION('',(0.125580124274607,0.992083480553514,0.));
#64576=DIRECTION('',(0.,0.,-1.));
#64577=DIRECTION('',(0.125580124274607,0.992083480553514,0.));
#64578=DIRECTION('',(0.,0.,-1.));
#64579=DIRECTION('',(0.,0.,-1.));
#64580=DIRECTION('',(0.,0.,-1.));
#64581=DIRECTION('',(0.,0.,-1.));
#64582=DIRECTION('',(0.,0.,-1.));
#64583=DIRECTION('',(0.,0.,-1.));
#64584=DIRECTION('',(0.,0.,-1.));
#64585=DIRECTION('center_axis',(-0.132163863358704,0.991227881580266,0.));
#64586=DIRECTION('ref_axis',(0.991227881580266,0.132163863358704,0.));
#64587=DIRECTION('',(0.991227881580266,0.132163863358704,0.));
#64588=DIRECTION('',(0.,0.,-1.));
#64589=DIRECTION('',(0.991227881580266,0.132163863358704,0.));
#64590=DIRECTION('center_axis',(0.,0.,1.));
#64591=DIRECTION('ref_axis',(1.,0.,0.));
#64592=DIRECTION('center_axis',(0.,0.,1.));
#64593=DIRECTION('ref_axis',(0.,-1.,0.));
#64594=DIRECTION('',(0.,0.,-1.));
#64595=DIRECTION('',(0.,0.,-1.));
#64596=DIRECTION('',(0.,0.,-1.));
#64597=DIRECTION('',(0.,0.,-1.));
#64598=DIRECTION('',(0.,0.,-1.));
#64599=DIRECTION('',(0.,0.,-1.));
#64600=DIRECTION('',(0.,0.,-1.));
#64601=DIRECTION('',(0.,0.,-1.));
#64602=DIRECTION('',(0.,0.,-1.));
#64603=DIRECTION('',(0.,0.,-1.));
#64604=DIRECTION('',(0.,0.,-1.));
#64605=DIRECTION('',(0.,0.,-1.));
#64606=DIRECTION('',(0.,0.,-1.));
#64607=DIRECTION('',(0.,0.,-1.));
#64608=DIRECTION('',(0.,0.,-1.));
#64609=DIRECTION('',(0.,0.,-1.));
#64610=DIRECTION('',(0.,0.,-1.));
#64611=DIRECTION('',(0.,0.,-1.));
#64612=DIRECTION('',(0.,0.,-1.));
#64613=DIRECTION('',(0.,0.,-1.));
#64614=DIRECTION('center_axis',(0.,0.,1.));
#64615=DIRECTION('ref_axis',(1.,0.,0.));
#64616=DIRECTION('center_axis',(0.821386116423605,-0.570372551712079,0.));
#64617=DIRECTION('ref_axis',(-0.570372551712079,-0.821386116423605,0.));
#64618=DIRECTION('',(-0.570372551712079,-0.821386116423605,0.));
#64619=DIRECTION('',(0.,0.,-1.));
#64620=DIRECTION('',(-0.570372551712079,-0.821386116423605,0.));
#64621=DIRECTION('',(0.,0.,-1.));
#64622=DIRECTION('center_axis',(-1.,0.,0.));
#64623=DIRECTION('ref_axis',(0.,1.,0.));
#64624=DIRECTION('',(0.,1.,0.));
#64625=DIRECTION('',(0.,0.,-1.));
#64626=DIRECTION('',(0.,1.,0.));
#64627=DIRECTION('center_axis',(0.,1.,0.));
#64628=DIRECTION('ref_axis',(1.,0.,0.));
#64629=DIRECTION('',(1.,0.,0.));
#64630=DIRECTION('',(1.,0.,0.));
#64631=DIRECTION('center_axis',(1.,0.,0.));
#64632=DIRECTION('ref_axis',(0.,-1.,0.));
#64633=DIRECTION('',(0.,-1.,0.));
#64634=DIRECTION('',(0.,0.,-1.));
#64635=DIRECTION('',(0.,-1.,0.));
#64636=DIRECTION('',(0.,0.,-1.));
#64637=DIRECTION('center_axis',(0.,-1.,0.));
#64638=DIRECTION('ref_axis',(-1.,0.,0.));
#64639=DIRECTION('',(-1.,0.,0.));
#64640=DIRECTION('',(0.,0.,-1.));
#64641=DIRECTION('',(-1.,0.,0.));
#64642=DIRECTION('center_axis',(1.,0.,0.));
#64643=DIRECTION('ref_axis',(0.,-1.,0.));
#64644=DIRECTION('',(0.,-1.,0.));
#64645=DIRECTION('',(0.,0.,-1.));
#64646=DIRECTION('',(0.,-1.,0.));
#64647=DIRECTION('center_axis',(0.,1.,0.));
#64648=DIRECTION('ref_axis',(1.,0.,0.));
#64649=DIRECTION('',(1.,0.,0.));
#64650=DIRECTION('',(0.,0.,-1.));
#64651=DIRECTION('',(1.,0.,0.));
#64652=DIRECTION('center_axis',(1.,0.,0.));
#64653=DIRECTION('ref_axis',(0.,-1.,0.));
#64654=DIRECTION('',(0.,-1.,0.));
#64655=DIRECTION('',(0.,0.,-1.));
#64656=DIRECTION('',(0.,-1.,0.));
#64657=DIRECTION('center_axis',(0.,1.,0.));
#64658=DIRECTION('ref_axis',(1.,0.,0.));
#64659=DIRECTION('',(1.,0.,0.));
#64660=DIRECTION('',(0.,0.,-1.));
#64661=DIRECTION('',(1.,0.,0.));
#64662=DIRECTION('center_axis',(-0.817611346967032,0.575770514450641,0.));
#64663=DIRECTION('ref_axis',(0.575770514450641,0.817611346967032,0.));
#64664=DIRECTION('',(0.575770514450641,0.817611346967032,0.));
#64665=DIRECTION('',(0.,0.,-1.));
#64666=DIRECTION('',(0.575770514450641,0.817611346967032,0.));
#64667=DIRECTION('center_axis',(-1.,0.,0.));
#64668=DIRECTION('ref_axis',(0.,1.,0.));
#64669=DIRECTION('',(0.,1.,0.));
#64670=DIRECTION('',(0.,0.,-1.));
#64671=DIRECTION('',(0.,1.,0.));
#64672=DIRECTION('center_axis',(0.,-1.,0.));
#64673=DIRECTION('ref_axis',(-1.,0.,0.));
#64674=DIRECTION('',(-1.,0.,0.));
#64675=DIRECTION('',(0.,0.,-1.));
#64676=DIRECTION('',(-1.,0.,0.));
#64677=DIRECTION('center_axis',(-1.,0.,0.));
#64678=DIRECTION('ref_axis',(0.,1.,0.));
#64679=DIRECTION('',(0.,1.,0.));
#64680=DIRECTION('',(0.,0.,-1.));
#64681=DIRECTION('',(0.,1.,0.));
#64682=DIRECTION('center_axis',(0.,-1.,0.));
#64683=DIRECTION('ref_axis',(-1.,0.,0.));
#64684=DIRECTION('',(-1.,0.,0.));
#64685=DIRECTION('',(-1.,0.,0.));
#64686=DIRECTION('center_axis',(0.,0.,-1.));
#64687=DIRECTION('ref_axis',(-1.,0.,0.));
#64688=DIRECTION('center_axis',(0.,0.,1.));
#64689=DIRECTION('ref_axis',(0.,-1.,0.));
#64690=DIRECTION('center_axis',(0.,0.,1.));
#64691=DIRECTION('ref_axis',(0.,-1.,0.));
#64692=DIRECTION('',(0.,0.,-1.));
#64693=DIRECTION('',(0.,0.,-1.));
#64694=DIRECTION('',(0.,0.,-1.));
#64695=DIRECTION('',(0.,0.,-1.));
#64696=DIRECTION('',(0.,0.,-1.));
#64697=DIRECTION('',(0.,0.,-1.));
#64698=DIRECTION('',(0.,0.,-1.));
#64699=DIRECTION('',(0.,0.,-1.));
#64700=DIRECTION('',(0.,0.,-1.));
#64701=DIRECTION('',(0.,0.,-1.));
#64702=DIRECTION('',(0.,0.,-1.));
#64703=DIRECTION('',(0.,0.,-1.));
#64704=DIRECTION('',(0.,0.,-1.));
#64705=DIRECTION('',(0.,0.,-1.));
#64706=DIRECTION('',(0.,0.,-1.));
#64707=DIRECTION('',(0.,0.,-1.));
#64708=DIRECTION('',(0.,0.,-1.));
#64709=DIRECTION('',(0.,0.,-1.));
#64710=DIRECTION('',(0.,0.,-1.));
#64711=DIRECTION('',(0.,0.,-1.));
#64712=DIRECTION('center_axis',(0.,0.,1.));
#64713=DIRECTION('ref_axis',(1.,0.,0.));
#64714=DIRECTION('',(0.,0.,-1.));
#64715=DIRECTION('',(0.,0.,-1.));
#64716=DIRECTION('',(0.,0.,-1.));
#64717=DIRECTION('',(0.,0.,-1.));
#64718=DIRECTION('',(0.,0.,-1.));
#64719=DIRECTION('',(0.,0.,-1.));
#64720=DIRECTION('',(0.,0.,-1.));
#64721=DIRECTION('center_axis',(0.980484873509324,-0.196594539139329,0.));
#64722=DIRECTION('ref_axis',(-0.196594539139329,-0.980484873509324,0.));
#64723=DIRECTION('',(-0.196594539139329,-0.980484873509324,0.));
#64724=DIRECTION('',(0.,0.,-1.));
#64725=DIRECTION('',(-0.196594539139329,-0.980484873509324,0.));
#64726=DIRECTION('center_axis',(0.,-1.,0.));
#64727=DIRECTION('ref_axis',(-1.,0.,0.));
#64728=DIRECTION('',(-1.,0.,0.));
#64729=DIRECTION('',(0.,0.,-1.));
#64730=DIRECTION('',(-1.,0.,0.));
#64731=DIRECTION('center_axis',(1.,0.,0.));
#64732=DIRECTION('ref_axis',(0.,-1.,0.));
#64733=DIRECTION('',(0.,-1.,0.));
#64734=DIRECTION('',(0.,0.,-1.));
#64735=DIRECTION('',(0.,-1.,0.));
#64736=DIRECTION('center_axis',(0.,1.,0.));
#64737=DIRECTION('ref_axis',(1.,0.,0.));
#64738=DIRECTION('',(1.,0.,0.));
#64739=DIRECTION('',(0.,0.,-1.));
#64740=DIRECTION('',(1.,0.,0.));
#64741=DIRECTION('center_axis',(-0.982679588991295,0.185312777163097,0.));
#64742=DIRECTION('ref_axis',(0.185312777163097,0.982679588991295,0.));
#64743=DIRECTION('',(0.185312777163097,0.982679588991295,0.));
#64744=DIRECTION('',(0.,0.,-1.));
#64745=DIRECTION('',(0.185312777163097,0.982679588991295,0.));
#64746=DIRECTION('center_axis',(-0.129088379836863,-0.991633092525201,0.));
#64747=DIRECTION('ref_axis',(-0.991633092525201,0.129088379836863,0.));
#64748=DIRECTION('',(-0.991633092525201,0.129088379836863,0.));
#64749=DIRECTION('',(0.,0.,-1.));
#64750=DIRECTION('',(-0.991633092525201,0.129088379836863,0.));
#64751=DIRECTION('',(0.,0.,-1.));
#64752=DIRECTION('',(0.,0.,-1.));
#64753=DIRECTION('',(0.,0.,-1.));
#64754=DIRECTION('',(0.,0.,-1.));
#64755=DIRECTION('',(0.,0.,-1.));
#64756=DIRECTION('',(0.,0.,-1.));
#64757=DIRECTION('',(0.,0.,-1.));
#64758=DIRECTION('',(0.,0.,-1.));
#64759=DIRECTION('center_axis',(-0.0843540635911639,0.99643584437517,0.));
#64760=DIRECTION('ref_axis',(0.99643584437517,0.0843540635911639,0.));
#64761=DIRECTION('',(0.99643584437517,0.0843540635911639,0.));
#64762=DIRECTION('',(0.,0.,-1.));
#64763=DIRECTION('',(0.99643584437517,0.0843540635911639,0.));
#64764=DIRECTION('center_axis',(0.,0.,1.));
#64765=DIRECTION('ref_axis',(1.,0.,0.));
#64766=DIRECTION('center_axis',(0.,0.,1.));
#64767=DIRECTION('ref_axis',(0.,-1.,0.));
#64768=DIRECTION('',(0.,0.,-1.));
#64769=DIRECTION('',(0.,0.,-1.));
#64770=DIRECTION('',(0.,0.,-1.));
#64771=DIRECTION('',(0.,0.,-1.));
#64772=DIRECTION('',(0.,0.,-1.));
#64773=DIRECTION('',(0.,0.,-1.));
#64774=DIRECTION('',(0.,0.,-1.));
#64775=DIRECTION('',(0.,0.,-1.));
#64776=DIRECTION('',(0.,0.,-1.));
#64777=DIRECTION('',(0.,0.,-1.));
#64778=DIRECTION('',(0.,0.,-1.));
#64779=DIRECTION('',(0.,0.,-1.));
#64780=DIRECTION('',(0.,0.,-1.));
#64781=DIRECTION('',(0.,0.,-1.));
#64782=DIRECTION('',(0.,0.,-1.));
#64783=DIRECTION('',(0.,0.,-1.));
#64784=DIRECTION('',(0.,0.,-1.));
#64785=DIRECTION('',(0.,0.,-1.));
#64786=DIRECTION('',(0.,0.,-1.));
#64787=DIRECTION('',(0.,0.,-1.));
#64788=DIRECTION('center_axis',(0.,0.,1.));
#64789=DIRECTION('ref_axis',(1.,0.,0.));
#64790=DIRECTION('',(0.,0.,-1.));
#64791=DIRECTION('',(0.,0.,-1.));
#64792=DIRECTION('',(0.,0.,-1.));
#64793=DIRECTION('',(0.,0.,-1.));
#64794=DIRECTION('',(0.,0.,-1.));
#64795=DIRECTION('',(0.,0.,-1.));
#64796=DIRECTION('',(0.,0.,-1.));
#64797=DIRECTION('',(0.,0.,-1.));
#64798=DIRECTION('',(0.,0.,-1.));
#64799=DIRECTION('',(0.,0.,-1.));
#64800=DIRECTION('',(0.,0.,-1.));
#64801=DIRECTION('',(0.,0.,-1.));
#64802=DIRECTION('',(0.,0.,-1.));
#64803=DIRECTION('',(0.,0.,-1.));
#64804=DIRECTION('',(0.,0.,-1.));
#64805=DIRECTION('',(0.,0.,-1.));
#64806=DIRECTION('',(0.,0.,-1.));
#64807=DIRECTION('',(0.,0.,-1.));
#64808=DIRECTION('',(0.,0.,-1.));
#64809=DIRECTION('',(0.,0.,-1.));
#64810=DIRECTION('',(0.,0.,-1.));
#64811=DIRECTION('',(0.,0.,-1.));
#64812=DIRECTION('',(0.,0.,-1.));
#64813=DIRECTION('',(0.,0.,-1.));
#64814=DIRECTION('',(0.,0.,-1.));
#64815=DIRECTION('',(0.,0.,-1.));
#64816=DIRECTION('',(0.,0.,-1.));
#64817=DIRECTION('center_axis',(0.0779743449792121,-0.99695536586402,0.));
#64818=DIRECTION('ref_axis',(-0.99695536586402,-0.0779743449792121,0.));
#64819=DIRECTION('',(-0.99695536586402,-0.0779743449792121,0.));
#64820=DIRECTION('',(0.,0.,-1.));
#64821=DIRECTION('',(-0.99695536586402,-0.0779743449792121,0.));
#64822=DIRECTION('center_axis',(0.,0.,1.));
#64823=DIRECTION('ref_axis',(1.,0.,0.));
#64824=DIRECTION('center_axis',(0.,0.,1.));
#64825=DIRECTION('ref_axis',(0.,-1.,0.));
#64826=DIRECTION('center_axis',(0.,0.,1.));
#64827=DIRECTION('ref_axis',(0.,-1.,0.));
#64828=DIRECTION('',(0.,0.,-1.));
#64829=DIRECTION('',(0.,0.,-1.));
#64830=DIRECTION('',(0.,0.,-1.));
#64831=DIRECTION('',(0.,0.,-1.));
#64832=DIRECTION('',(0.,0.,-1.));
#64833=DIRECTION('',(0.,0.,-1.));
#64834=DIRECTION('',(0.,0.,-1.));
#64835=DIRECTION('',(0.,0.,-1.));
#64836=DIRECTION('',(0.,0.,-1.));
#64837=DIRECTION('',(0.,0.,-1.));
#64838=DIRECTION('',(0.,0.,-1.));
#64839=DIRECTION('',(0.,0.,-1.));
#64840=DIRECTION('',(0.,0.,-1.));
#64841=DIRECTION('',(0.,0.,-1.));
#64842=DIRECTION('',(0.,0.,-1.));
#64843=DIRECTION('',(0.,0.,-1.));
#64844=DIRECTION('',(0.,0.,-1.));
#64845=DIRECTION('',(0.,0.,-1.));
#64846=DIRECTION('',(0.,0.,-1.));
#64847=DIRECTION('',(0.,0.,-1.));
#64848=DIRECTION('center_axis',(0.,0.,1.));
#64849=DIRECTION('ref_axis',(1.,0.,0.));
#64850=DIRECTION('',(0.,0.,-1.));
#64851=DIRECTION('',(0.,0.,-1.));
#64852=DIRECTION('',(0.,0.,-1.));
#64853=DIRECTION('',(0.,0.,-1.));
#64854=DIRECTION('center_axis',(0.,-1.,0.));
#64855=DIRECTION('ref_axis',(-1.,0.,0.));
#64856=DIRECTION('',(-1.,0.,0.));
#64857=DIRECTION('',(0.,0.,-1.));
#64858=DIRECTION('',(-1.,0.,0.));
#64859=DIRECTION('',(0.,0.,-1.));
#64860=DIRECTION('',(0.,0.,-1.));
#64861=DIRECTION('',(0.,0.,-1.));
#64862=DIRECTION('center_axis',(1.,0.,0.));
#64863=DIRECTION('ref_axis',(0.,-1.,0.));
#64864=DIRECTION('',(0.,-1.,0.));
#64865=DIRECTION('',(0.,0.,-1.));
#64866=DIRECTION('',(0.,-1.,0.));
#64867=DIRECTION('center_axis',(0.,1.,0.));
#64868=DIRECTION('ref_axis',(1.,0.,0.));
#64869=DIRECTION('',(1.,0.,0.));
#64870=DIRECTION('',(0.,0.,-1.));
#64871=DIRECTION('',(1.,0.,0.));
#64872=DIRECTION('center_axis',(-1.,0.,0.));
#64873=DIRECTION('ref_axis',(0.,1.,0.));
#64874=DIRECTION('',(0.,1.,0.));
#64875=DIRECTION('',(0.,0.,-1.));
#64876=DIRECTION('',(0.,1.,0.));
#64877=DIRECTION('center_axis',(0.,-1.,0.));
#64878=DIRECTION('ref_axis',(-1.,0.,0.));
#64879=DIRECTION('',(-1.,0.,0.));
#64880=DIRECTION('',(-1.,0.,0.));
#64881=DIRECTION('center_axis',(0.,0.,1.));
#64882=DIRECTION('ref_axis',(1.,0.,0.));
#64883=DIRECTION('center_axis',(0.,0.,1.));
#64884=DIRECTION('ref_axis',(0.,-1.,0.));
#64885=DIRECTION('',(0.,0.,-1.));
#64886=DIRECTION('',(0.,0.,-1.));
#64887=DIRECTION('',(0.,0.,-1.));
#64888=DIRECTION('',(0.,0.,-1.));
#64889=DIRECTION('',(0.,0.,-1.));
#64890=DIRECTION('',(0.,0.,-1.));
#64891=DIRECTION('',(0.,0.,-1.));
#64892=DIRECTION('',(0.,0.,-1.));
#64893=DIRECTION('',(0.,0.,-1.));
#64894=DIRECTION('',(0.,0.,-1.));
#64895=DIRECTION('',(0.,0.,-1.));
#64896=DIRECTION('',(0.,0.,-1.));
#64897=DIRECTION('',(0.,0.,-1.));
#64898=DIRECTION('',(0.,0.,-1.));
#64899=DIRECTION('',(0.,0.,-1.));
#64900=DIRECTION('',(0.,0.,-1.));
#64901=DIRECTION('',(0.,0.,-1.));
#64902=DIRECTION('',(0.,0.,-1.));
#64903=DIRECTION('',(0.,0.,-1.));
#64904=DIRECTION('',(0.,0.,-1.));
#64905=DIRECTION('center_axis',(0.,0.,1.));
#64906=DIRECTION('ref_axis',(1.,0.,0.));
#64907=DIRECTION('',(0.,0.,-1.));
#64908=DIRECTION('',(0.,0.,-1.));
#64909=DIRECTION('',(0.,0.,-1.));
#64910=DIRECTION('',(0.,0.,-1.));
#64911=DIRECTION('',(0.,0.,-1.));
#64912=DIRECTION('',(0.,0.,-1.));
#64913=DIRECTION('',(0.,0.,-1.));
#64914=DIRECTION('',(0.,0.,-1.));
#64915=DIRECTION('',(0.,0.,-1.));
#64916=DIRECTION('',(0.,0.,-1.));
#64917=DIRECTION('',(0.,0.,-1.));
#64918=DIRECTION('',(0.,0.,-1.));
#64919=DIRECTION('',(0.,0.,-1.));
#64920=DIRECTION('',(0.,0.,-1.));
#64921=DIRECTION('',(0.,0.,-1.));
#64922=DIRECTION('',(0.,0.,-1.));
#64923=DIRECTION('',(0.,0.,-1.));
#64924=DIRECTION('',(0.,0.,-1.));
#64925=DIRECTION('',(0.,0.,-1.));
#64926=DIRECTION('',(0.,0.,-1.));
#64927=DIRECTION('',(0.,0.,-1.));
#64928=DIRECTION('',(0.,0.,-1.));
#64929=DIRECTION('',(0.,0.,-1.));
#64930=DIRECTION('',(0.,0.,-1.));
#64931=DIRECTION('',(0.,0.,-1.));
#64932=DIRECTION('',(0.,0.,-1.));
#64933=DIRECTION('',(0.,0.,-1.));
#64934=DIRECTION('',(0.,0.,-1.));
#64935=DIRECTION('',(0.,0.,-1.));
#64936=DIRECTION('',(0.,0.,-1.));
#64937=DIRECTION('',(0.,0.,-1.));
#64938=DIRECTION('',(0.,0.,-1.));
#64939=DIRECTION('',(0.,0.,-1.));
#64940=DIRECTION('center_axis',(0.,0.,1.));
#64941=DIRECTION('ref_axis',(1.,0.,0.));
#64942=DIRECTION('center_axis',(0.,0.,1.));
#64943=DIRECTION('ref_axis',(0.,-1.,0.));
#64944=DIRECTION('center_axis',(0.,0.,1.));
#64945=DIRECTION('ref_axis',(0.,-1.,0.));
#64946=DIRECTION('center_axis',(0.,0.,1.));
#64947=DIRECTION('ref_axis',(0.,-1.,0.));
#64948=DIRECTION('',(0.,0.,-1.));
#64949=DIRECTION('',(0.,0.,-1.));
#64950=DIRECTION('',(0.,0.,-1.));
#64951=DIRECTION('',(0.,0.,-1.));
#64952=DIRECTION('',(0.,0.,-1.));
#64953=DIRECTION('',(0.,0.,-1.));
#64954=DIRECTION('',(0.,0.,-1.));
#64955=DIRECTION('',(0.,0.,-1.));
#64956=DIRECTION('',(0.,0.,-1.));
#64957=DIRECTION('',(0.,0.,-1.));
#64958=DIRECTION('',(0.,0.,-1.));
#64959=DIRECTION('',(0.,0.,-1.));
#64960=DIRECTION('',(0.,0.,-1.));
#64961=DIRECTION('',(0.,0.,-1.));
#64962=DIRECTION('',(0.,0.,-1.));
#64963=DIRECTION('',(0.,0.,-1.));
#64964=DIRECTION('',(0.,0.,-1.));
#64965=DIRECTION('',(0.,0.,-1.));
#64966=DIRECTION('',(0.,0.,-1.));
#64967=DIRECTION('',(0.,0.,-1.));
#64968=DIRECTION('center_axis',(0.,0.,1.));
#64969=DIRECTION('ref_axis',(1.,0.,0.));
#64970=DIRECTION('',(0.,0.,-1.));
#64971=DIRECTION('',(0.,0.,-1.));
#64972=DIRECTION('',(0.,0.,-1.));
#64973=DIRECTION('',(0.,0.,-1.));
#64974=DIRECTION('',(0.,0.,-1.));
#64975=DIRECTION('',(0.,0.,-1.));
#64976=DIRECTION('',(0.,0.,-1.));
#64977=DIRECTION('',(0.,0.,-1.));
#64978=DIRECTION('',(0.,0.,-1.));
#64979=DIRECTION('',(0.,0.,-1.));
#64980=DIRECTION('',(0.,0.,-1.));
#64981=DIRECTION('',(0.,0.,-1.));
#64982=DIRECTION('',(0.,0.,-1.));
#64983=DIRECTION('',(0.,0.,-1.));
#64984=DIRECTION('',(0.,0.,-1.));
#64985=DIRECTION('',(0.,0.,-1.));
#64986=DIRECTION('',(0.,0.,-1.));
#64987=DIRECTION('',(0.,0.,-1.));
#64988=DIRECTION('',(0.,0.,-1.));
#64989=DIRECTION('',(0.,0.,-1.));
#64990=DIRECTION('',(0.,0.,-1.));
#64991=DIRECTION('',(0.,0.,-1.));
#64992=DIRECTION('',(0.,0.,-1.));
#64993=DIRECTION('',(0.,0.,-1.));
#64994=DIRECTION('',(0.,0.,-1.));
#64995=DIRECTION('',(0.,0.,-1.));
#64996=DIRECTION('',(0.,0.,-1.));
#64997=DIRECTION('',(0.,0.,-1.));
#64998=DIRECTION('',(0.,0.,-1.));
#64999=DIRECTION('center_axis',(-0.0920922327212455,0.995750481130899,0.));
#65000=DIRECTION('ref_axis',(0.995750481130899,0.0920922327212455,0.));
#65001=DIRECTION('',(0.995750481130899,0.0920922327212455,0.));
#65002=DIRECTION('',(0.,0.,-1.));
#65003=DIRECTION('',(0.995750481130898,0.0920922327212455,0.));
#65004=DIRECTION('center_axis',(0.,0.,1.));
#65005=DIRECTION('ref_axis',(1.,0.,0.));
#65006=DIRECTION('center_axis',(0.,0.,1.));
#65007=DIRECTION('ref_axis',(0.,-1.,0.));
#65008=DIRECTION('center_axis',(0.,0.,1.));
#65009=DIRECTION('ref_axis',(0.,-1.,0.));
#65010=DIRECTION('center_axis',(0.,-1.,0.));
#65011=DIRECTION('ref_axis',(-1.,0.,0.));
#65012=DIRECTION('',(-1.,0.,0.));
#65013=DIRECTION('',(0.,0.,-1.));
#65014=DIRECTION('',(-1.,0.,0.));
#65015=DIRECTION('',(0.,0.,-1.));
#65016=DIRECTION('center_axis',(1.,0.,0.));
#65017=DIRECTION('ref_axis',(0.,-1.,0.));
#65018=DIRECTION('',(0.,-1.,0.));
#65019=DIRECTION('',(0.,0.,-1.));
#65020=DIRECTION('',(0.,-1.,0.));
#65021=DIRECTION('center_axis',(0.,1.,0.));
#65022=DIRECTION('ref_axis',(1.,0.,0.));
#65023=DIRECTION('',(1.,0.,0.));
#65024=DIRECTION('',(0.,0.,-1.));
#65025=DIRECTION('',(1.,0.,0.));
#65026=DIRECTION('center_axis',(-1.,0.,0.));
#65027=DIRECTION('ref_axis',(0.,1.,0.));
#65028=DIRECTION('',(0.,1.,0.));
#65029=DIRECTION('',(0.,1.,0.));
#65030=DIRECTION('center_axis',(0.,0.,-1.));
#65031=DIRECTION('ref_axis',(-1.,0.,0.));
#65032=DIRECTION('center_axis',(0.,-1.,0.));
#65033=DIRECTION('ref_axis',(-1.,0.,0.));
#65034=DIRECTION('',(-1.,0.,0.));
#65035=DIRECTION('',(0.,0.,-1.));
#65036=DIRECTION('',(-1.,0.,0.));
#65037=DIRECTION('',(0.,0.,-1.));
#65038=DIRECTION('center_axis',(1.,0.,0.));
#65039=DIRECTION('ref_axis',(0.,-1.,0.));
#65040=DIRECTION('',(0.,-1.,0.));
#65041=DIRECTION('',(0.,0.,-1.));
#65042=DIRECTION('',(0.,-1.,0.));
#65043=DIRECTION('center_axis',(0.,1.,0.));
#65044=DIRECTION('ref_axis',(1.,0.,0.));
#65045=DIRECTION('',(1.,0.,0.));
#65046=DIRECTION('',(0.,0.,-1.));
#65047=DIRECTION('',(1.,0.,0.));
#65048=DIRECTION('center_axis',(-1.,0.,0.));
#65049=DIRECTION('ref_axis',(0.,1.,0.));
#65050=DIRECTION('',(0.,1.,0.));
#65051=DIRECTION('',(0.,1.,0.));
#65052=DIRECTION('center_axis',(0.,0.,-1.));
#65053=DIRECTION('ref_axis',(-1.,0.,0.));
#65054=DIRECTION('center_axis',(0.,-1.,0.));
#65055=DIRECTION('ref_axis',(-1.,0.,0.));
#65056=DIRECTION('',(-1.,0.,0.));
#65057=DIRECTION('',(0.,0.,-1.));
#65058=DIRECTION('',(-1.,0.,0.));
#65059=DIRECTION('',(0.,0.,-1.));
#65060=DIRECTION('center_axis',(1.,0.,0.));
#65061=DIRECTION('ref_axis',(0.,-1.,0.));
#65062=DIRECTION('',(0.,-1.,0.));
#65063=DIRECTION('',(0.,0.,-1.));
#65064=DIRECTION('',(0.,-1.,0.));
#65065=DIRECTION('center_axis',(0.,1.,0.));
#65066=DIRECTION('ref_axis',(1.,0.,0.));
#65067=DIRECTION('',(1.,0.,0.));
#65068=DIRECTION('',(0.,0.,-1.));
#65069=DIRECTION('',(1.,0.,0.));
#65070=DIRECTION('center_axis',(-1.,0.,0.));
#65071=DIRECTION('ref_axis',(0.,1.,0.));
#65072=DIRECTION('',(0.,1.,0.));
#65073=DIRECTION('',(0.,1.,0.));
#65074=DIRECTION('center_axis',(0.,0.,-1.));
#65075=DIRECTION('ref_axis',(-1.,0.,0.));
#65076=DIRECTION('center_axis',(0.,-1.,0.));
#65077=DIRECTION('ref_axis',(-1.,0.,0.));
#65078=DIRECTION('',(-1.,0.,0.));
#65079=DIRECTION('',(0.,0.,-1.));
#65080=DIRECTION('',(-1.,0.,0.));
#65081=DIRECTION('',(0.,0.,-1.));
#65082=DIRECTION('center_axis',(1.,0.,0.));
#65083=DIRECTION('ref_axis',(0.,-1.,0.));
#65084=DIRECTION('',(0.,-1.,0.));
#65085=DIRECTION('',(0.,0.,-1.));
#65086=DIRECTION('',(0.,-1.,0.));
#65087=DIRECTION('center_axis',(0.,1.,0.));
#65088=DIRECTION('ref_axis',(1.,0.,0.));
#65089=DIRECTION('',(1.,0.,0.));
#65090=DIRECTION('',(0.,0.,-1.));
#65091=DIRECTION('',(1.,0.,0.));
#65092=DIRECTION('center_axis',(-1.,0.,0.));
#65093=DIRECTION('ref_axis',(0.,1.,0.));
#65094=DIRECTION('',(0.,1.,0.));
#65095=DIRECTION('',(0.,1.,0.));
#65096=DIRECTION('center_axis',(0.,0.,-1.));
#65097=DIRECTION('ref_axis',(-1.,0.,0.));
#65098=DIRECTION('center_axis',(0.,-1.,0.));
#65099=DIRECTION('ref_axis',(-1.,0.,0.));
#65100=DIRECTION('',(-1.,0.,0.));
#65101=DIRECTION('',(0.,0.,-1.));
#65102=DIRECTION('',(-1.,0.,0.));
#65103=DIRECTION('',(0.,0.,-1.));
#65104=DIRECTION('center_axis',(1.,0.,0.));
#65105=DIRECTION('ref_axis',(0.,-1.,0.));
#65106=DIRECTION('',(0.,-1.,0.));
#65107=DIRECTION('',(0.,0.,-1.));
#65108=DIRECTION('',(0.,-1.,0.));
#65109=DIRECTION('center_axis',(0.,1.,0.));
#65110=DIRECTION('ref_axis',(1.,0.,0.));
#65111=DIRECTION('',(1.,0.,0.));
#65112=DIRECTION('',(0.,0.,-1.));
#65113=DIRECTION('',(1.,0.,0.));
#65114=DIRECTION('center_axis',(-1.,0.,0.));
#65115=DIRECTION('ref_axis',(0.,1.,0.));
#65116=DIRECTION('',(0.,1.,0.));
#65117=DIRECTION('',(0.,1.,0.));
#65118=DIRECTION('center_axis',(0.,0.,-1.));
#65119=DIRECTION('ref_axis',(-1.,0.,0.));
#65120=DIRECTION('center_axis',(0.,-1.,0.));
#65121=DIRECTION('ref_axis',(-1.,0.,0.));
#65122=DIRECTION('',(-1.,0.,0.));
#65123=DIRECTION('',(0.,0.,-1.));
#65124=DIRECTION('',(-1.,0.,0.));
#65125=DIRECTION('',(0.,0.,-1.));
#65126=DIRECTION('center_axis',(1.,0.,0.));
#65127=DIRECTION('ref_axis',(0.,-1.,0.));
#65128=DIRECTION('',(0.,-1.,0.));
#65129=DIRECTION('',(0.,0.,-1.));
#65130=DIRECTION('',(0.,-1.,0.));
#65131=DIRECTION('center_axis',(0.,1.,0.));
#65132=DIRECTION('ref_axis',(1.,0.,0.));
#65133=DIRECTION('',(1.,0.,0.));
#65134=DIRECTION('',(0.,0.,-1.));
#65135=DIRECTION('',(1.,0.,0.));
#65136=DIRECTION('center_axis',(-1.,0.,0.));
#65137=DIRECTION('ref_axis',(0.,1.,0.));
#65138=DIRECTION('',(0.,1.,0.));
#65139=DIRECTION('',(0.,1.,0.));
#65140=DIRECTION('center_axis',(0.,0.,-1.));
#65141=DIRECTION('ref_axis',(-1.,0.,0.));
#65142=DIRECTION('center_axis',(0.,-1.,0.));
#65143=DIRECTION('ref_axis',(-1.,0.,0.));
#65144=DIRECTION('',(-1.,0.,0.));
#65145=DIRECTION('',(0.,0.,-1.));
#65146=DIRECTION('',(-1.,0.,0.));
#65147=DIRECTION('',(0.,0.,-1.));
#65148=DIRECTION('center_axis',(1.,0.,0.));
#65149=DIRECTION('ref_axis',(0.,-1.,0.));
#65150=DIRECTION('',(0.,-1.,0.));
#65151=DIRECTION('',(0.,0.,-1.));
#65152=DIRECTION('',(0.,-1.,0.));
#65153=DIRECTION('center_axis',(0.,1.,0.));
#65154=DIRECTION('ref_axis',(1.,0.,0.));
#65155=DIRECTION('',(1.,0.,0.));
#65156=DIRECTION('',(0.,0.,-1.));
#65157=DIRECTION('',(1.,0.,0.));
#65158=DIRECTION('center_axis',(-1.,0.,0.));
#65159=DIRECTION('ref_axis',(0.,1.,0.));
#65160=DIRECTION('',(0.,1.,0.));
#65161=DIRECTION('',(0.,1.,0.));
#65162=DIRECTION('center_axis',(0.,0.,-1.));
#65163=DIRECTION('ref_axis',(-1.,0.,0.));
#65164=DIRECTION('center_axis',(0.,-1.,0.));
#65165=DIRECTION('ref_axis',(-1.,0.,0.));
#65166=DIRECTION('',(-1.,0.,0.));
#65167=DIRECTION('',(0.,0.,-1.));
#65168=DIRECTION('',(-1.,0.,0.));
#65169=DIRECTION('',(0.,0.,-1.));
#65170=DIRECTION('center_axis',(1.,0.,0.));
#65171=DIRECTION('ref_axis',(0.,-1.,0.));
#65172=DIRECTION('',(0.,-1.,0.));
#65173=DIRECTION('',(0.,0.,-1.));
#65174=DIRECTION('',(0.,-1.,0.));
#65175=DIRECTION('center_axis',(0.,1.,0.));
#65176=DIRECTION('ref_axis',(1.,0.,0.));
#65177=DIRECTION('',(1.,0.,0.));
#65178=DIRECTION('',(0.,0.,-1.));
#65179=DIRECTION('',(1.,0.,0.));
#65180=DIRECTION('center_axis',(-1.,0.,0.));
#65181=DIRECTION('ref_axis',(0.,1.,0.));
#65182=DIRECTION('',(0.,1.,0.));
#65183=DIRECTION('',(0.,1.,0.));
#65184=DIRECTION('center_axis',(0.,0.,-1.));
#65185=DIRECTION('ref_axis',(-1.,0.,0.));
#65186=DIRECTION('center_axis',(0.,-1.,0.));
#65187=DIRECTION('ref_axis',(-1.,0.,0.));
#65188=DIRECTION('',(-1.,0.,0.));
#65189=DIRECTION('',(0.,0.,-1.));
#65190=DIRECTION('',(-1.,0.,0.));
#65191=DIRECTION('',(0.,0.,-1.));
#65192=DIRECTION('center_axis',(1.,0.,0.));
#65193=DIRECTION('ref_axis',(0.,-1.,0.));
#65194=DIRECTION('',(0.,-1.,0.));
#65195=DIRECTION('',(0.,0.,-1.));
#65196=DIRECTION('',(0.,-1.,0.));
#65197=DIRECTION('center_axis',(0.,1.,0.));
#65198=DIRECTION('ref_axis',(1.,0.,0.));
#65199=DIRECTION('',(1.,0.,0.));
#65200=DIRECTION('',(0.,0.,-1.));
#65201=DIRECTION('',(1.,0.,0.));
#65202=DIRECTION('center_axis',(-1.,0.,0.));
#65203=DIRECTION('ref_axis',(0.,1.,0.));
#65204=DIRECTION('',(0.,1.,0.));
#65205=DIRECTION('',(0.,1.,0.));
#65206=DIRECTION('center_axis',(0.,0.,-1.));
#65207=DIRECTION('ref_axis',(-1.,0.,0.));
#65208=DIRECTION('center_axis',(0.,-1.,0.));
#65209=DIRECTION('ref_axis',(-1.,0.,0.));
#65210=DIRECTION('',(-1.,0.,0.));
#65211=DIRECTION('',(0.,0.,-1.));
#65212=DIRECTION('',(-1.,0.,0.));
#65213=DIRECTION('',(0.,0.,-1.));
#65214=DIRECTION('center_axis',(1.,0.,0.));
#65215=DIRECTION('ref_axis',(0.,-1.,0.));
#65216=DIRECTION('',(0.,-1.,0.));
#65217=DIRECTION('',(0.,0.,-1.));
#65218=DIRECTION('',(0.,-1.,0.));
#65219=DIRECTION('center_axis',(0.,1.,0.));
#65220=DIRECTION('ref_axis',(1.,0.,0.));
#65221=DIRECTION('',(1.,0.,0.));
#65222=DIRECTION('',(0.,0.,-1.));
#65223=DIRECTION('',(1.,0.,0.));
#65224=DIRECTION('center_axis',(-1.,0.,0.));
#65225=DIRECTION('ref_axis',(0.,1.,0.));
#65226=DIRECTION('',(0.,1.,0.));
#65227=DIRECTION('',(0.,1.,0.));
#65228=DIRECTION('center_axis',(0.,0.,-1.));
#65229=DIRECTION('ref_axis',(-1.,0.,0.));
#65230=DIRECTION('center_axis',(0.,-1.,0.));
#65231=DIRECTION('ref_axis',(-1.,0.,0.));
#65232=DIRECTION('',(-1.,0.,0.));
#65233=DIRECTION('',(0.,0.,-1.));
#65234=DIRECTION('',(-1.,0.,0.));
#65235=DIRECTION('',(0.,0.,-1.));
#65236=DIRECTION('center_axis',(1.,0.,0.));
#65237=DIRECTION('ref_axis',(0.,-1.,0.));
#65238=DIRECTION('',(0.,-1.,0.));
#65239=DIRECTION('',(0.,0.,-1.));
#65240=DIRECTION('',(0.,-1.,0.));
#65241=DIRECTION('center_axis',(0.,1.,0.));
#65242=DIRECTION('ref_axis',(1.,0.,0.));
#65243=DIRECTION('',(1.,0.,0.));
#65244=DIRECTION('',(0.,0.,-1.));
#65245=DIRECTION('',(1.,0.,0.));
#65246=DIRECTION('center_axis',(-1.,0.,0.));
#65247=DIRECTION('ref_axis',(0.,1.,0.));
#65248=DIRECTION('',(0.,1.,0.));
#65249=DIRECTION('',(0.,1.,0.));
#65250=DIRECTION('center_axis',(0.,0.,-1.));
#65251=DIRECTION('ref_axis',(-1.,0.,0.));
#65252=DIRECTION('center_axis',(0.,-1.,0.));
#65253=DIRECTION('ref_axis',(-1.,0.,0.));
#65254=DIRECTION('',(-1.,0.,0.));
#65255=DIRECTION('',(0.,0.,-1.));
#65256=DIRECTION('',(-1.,0.,0.));
#65257=DIRECTION('',(0.,0.,-1.));
#65258=DIRECTION('center_axis',(1.,0.,0.));
#65259=DIRECTION('ref_axis',(0.,-1.,0.));
#65260=DIRECTION('',(0.,-1.,0.));
#65261=DIRECTION('',(0.,0.,-1.));
#65262=DIRECTION('',(0.,-1.,0.));
#65263=DIRECTION('center_axis',(0.,1.,0.));
#65264=DIRECTION('ref_axis',(1.,0.,0.));
#65265=DIRECTION('',(1.,0.,0.));
#65266=DIRECTION('',(0.,0.,-1.));
#65267=DIRECTION('',(1.,0.,0.));
#65268=DIRECTION('center_axis',(-1.,0.,0.));
#65269=DIRECTION('ref_axis',(0.,1.,0.));
#65270=DIRECTION('',(0.,1.,0.));
#65271=DIRECTION('',(0.,1.,0.));
#65272=DIRECTION('center_axis',(0.,0.,-1.));
#65273=DIRECTION('ref_axis',(-1.,0.,0.));
#65274=DIRECTION('center_axis',(0.,-1.,0.));
#65275=DIRECTION('ref_axis',(-1.,0.,0.));
#65276=DIRECTION('',(-1.,0.,0.));
#65277=DIRECTION('',(0.,0.,-1.));
#65278=DIRECTION('',(-1.,0.,0.));
#65279=DIRECTION('',(0.,0.,-1.));
#65280=DIRECTION('center_axis',(1.,0.,0.));
#65281=DIRECTION('ref_axis',(0.,-1.,0.));
#65282=DIRECTION('',(0.,-1.,0.));
#65283=DIRECTION('',(0.,0.,-1.));
#65284=DIRECTION('',(0.,-1.,0.));
#65285=DIRECTION('center_axis',(0.,1.,0.));
#65286=DIRECTION('ref_axis',(1.,0.,0.));
#65287=DIRECTION('',(1.,0.,0.));
#65288=DIRECTION('',(0.,0.,-1.));
#65289=DIRECTION('',(1.,0.,0.));
#65290=DIRECTION('center_axis',(-1.,0.,0.));
#65291=DIRECTION('ref_axis',(0.,1.,0.));
#65292=DIRECTION('',(0.,1.,0.));
#65293=DIRECTION('',(0.,1.,0.));
#65294=DIRECTION('center_axis',(0.,0.,-1.));
#65295=DIRECTION('ref_axis',(-1.,0.,0.));
#65296=DIRECTION('center_axis',(0.,-1.,0.));
#65297=DIRECTION('ref_axis',(-1.,0.,0.));
#65298=DIRECTION('',(-1.,0.,0.));
#65299=DIRECTION('',(0.,0.,-1.));
#65300=DIRECTION('',(-1.,0.,0.));
#65301=DIRECTION('',(0.,0.,-1.));
#65302=DIRECTION('center_axis',(1.,0.,0.));
#65303=DIRECTION('ref_axis',(0.,-1.,0.));
#65304=DIRECTION('',(0.,-1.,0.));
#65305=DIRECTION('',(0.,0.,-1.));
#65306=DIRECTION('',(0.,-1.,0.));
#65307=DIRECTION('center_axis',(0.,1.,0.));
#65308=DIRECTION('ref_axis',(1.,0.,0.));
#65309=DIRECTION('',(1.,0.,0.));
#65310=DIRECTION('',(0.,0.,-1.));
#65311=DIRECTION('',(1.,0.,0.));
#65312=DIRECTION('center_axis',(-1.,0.,0.));
#65313=DIRECTION('ref_axis',(0.,1.,0.));
#65314=DIRECTION('',(0.,1.,0.));
#65315=DIRECTION('',(0.,1.,0.));
#65316=DIRECTION('center_axis',(0.,0.,-1.));
#65317=DIRECTION('ref_axis',(-1.,0.,0.));
#65318=DIRECTION('center_axis',(0.,-1.,0.));
#65319=DIRECTION('ref_axis',(-1.,0.,0.));
#65320=DIRECTION('',(-1.,0.,0.));
#65321=DIRECTION('',(0.,0.,-1.));
#65322=DIRECTION('',(-1.,0.,0.));
#65323=DIRECTION('',(0.,0.,-1.));
#65324=DIRECTION('center_axis',(1.,0.,0.));
#65325=DIRECTION('ref_axis',(0.,-1.,0.));
#65326=DIRECTION('',(0.,-1.,0.));
#65327=DIRECTION('',(0.,0.,-1.));
#65328=DIRECTION('',(0.,-1.,0.));
#65329=DIRECTION('center_axis',(0.,1.,0.));
#65330=DIRECTION('ref_axis',(1.,0.,0.));
#65331=DIRECTION('',(1.,0.,0.));
#65332=DIRECTION('',(0.,0.,-1.));
#65333=DIRECTION('',(1.,0.,0.));
#65334=DIRECTION('center_axis',(-1.,0.,0.));
#65335=DIRECTION('ref_axis',(0.,1.,0.));
#65336=DIRECTION('',(0.,1.,0.));
#65337=DIRECTION('',(0.,1.,0.));
#65338=DIRECTION('center_axis',(0.,0.,-1.));
#65339=DIRECTION('ref_axis',(-1.,0.,0.));
#65340=DIRECTION('center_axis',(0.,-1.,0.));
#65341=DIRECTION('ref_axis',(-1.,0.,0.));
#65342=DIRECTION('',(-1.,0.,0.));
#65343=DIRECTION('',(0.,0.,-1.));
#65344=DIRECTION('',(-1.,0.,0.));
#65345=DIRECTION('',(0.,0.,-1.));
#65346=DIRECTION('center_axis',(1.,0.,0.));
#65347=DIRECTION('ref_axis',(0.,-1.,0.));
#65348=DIRECTION('',(0.,-1.,0.));
#65349=DIRECTION('',(0.,0.,-1.));
#65350=DIRECTION('',(0.,-1.,0.));
#65351=DIRECTION('center_axis',(0.,1.,0.));
#65352=DIRECTION('ref_axis',(1.,0.,0.));
#65353=DIRECTION('',(1.,0.,0.));
#65354=DIRECTION('',(0.,0.,-1.));
#65355=DIRECTION('',(1.,0.,0.));
#65356=DIRECTION('center_axis',(-1.,0.,0.));
#65357=DIRECTION('ref_axis',(0.,1.,0.));
#65358=DIRECTION('',(0.,1.,0.));
#65359=DIRECTION('',(0.,1.,0.));
#65360=DIRECTION('center_axis',(0.,0.,-1.));
#65361=DIRECTION('ref_axis',(-1.,0.,0.));
#65362=DIRECTION('center_axis',(0.,-1.,0.));
#65363=DIRECTION('ref_axis',(-1.,0.,0.));
#65364=DIRECTION('',(-1.,0.,0.));
#65365=DIRECTION('',(0.,0.,-1.));
#65366=DIRECTION('',(-1.,0.,0.));
#65367=DIRECTION('',(0.,0.,-1.));
#65368=DIRECTION('center_axis',(1.,0.,0.));
#65369=DIRECTION('ref_axis',(0.,-1.,0.));
#65370=DIRECTION('',(0.,-1.,0.));
#65371=DIRECTION('',(0.,0.,-1.));
#65372=DIRECTION('',(0.,-1.,0.));
#65373=DIRECTION('center_axis',(0.,1.,0.));
#65374=DIRECTION('ref_axis',(1.,0.,0.));
#65375=DIRECTION('',(1.,0.,0.));
#65376=DIRECTION('',(0.,0.,-1.));
#65377=DIRECTION('',(1.,0.,0.));
#65378=DIRECTION('center_axis',(-1.,0.,0.));
#65379=DIRECTION('ref_axis',(0.,1.,0.));
#65380=DIRECTION('',(0.,1.,0.));
#65381=DIRECTION('',(0.,1.,0.));
#65382=DIRECTION('center_axis',(0.,0.,-1.));
#65383=DIRECTION('ref_axis',(-1.,0.,0.));
#65384=DIRECTION('center_axis',(0.,-1.,0.));
#65385=DIRECTION('ref_axis',(-1.,0.,0.));
#65386=DIRECTION('',(-1.,0.,0.));
#65387=DIRECTION('',(0.,0.,-1.));
#65388=DIRECTION('',(-1.,0.,0.));
#65389=DIRECTION('',(0.,0.,-1.));
#65390=DIRECTION('center_axis',(1.,0.,0.));
#65391=DIRECTION('ref_axis',(0.,-1.,0.));
#65392=DIRECTION('',(0.,-1.,0.));
#65393=DIRECTION('',(0.,0.,-1.));
#65394=DIRECTION('',(0.,-1.,0.));
#65395=DIRECTION('center_axis',(0.,1.,0.));
#65396=DIRECTION('ref_axis',(1.,0.,0.));
#65397=DIRECTION('',(1.,0.,0.));
#65398=DIRECTION('',(0.,0.,-1.));
#65399=DIRECTION('',(1.,0.,0.));
#65400=DIRECTION('center_axis',(-1.,0.,0.));
#65401=DIRECTION('ref_axis',(0.,1.,0.));
#65402=DIRECTION('',(0.,1.,0.));
#65403=DIRECTION('',(0.,1.,0.));
#65404=DIRECTION('center_axis',(0.,0.,-1.));
#65405=DIRECTION('ref_axis',(-1.,0.,0.));
#65406=DIRECTION('center_axis',(0.,-1.,0.));
#65407=DIRECTION('ref_axis',(-1.,0.,0.));
#65408=DIRECTION('',(-1.,0.,0.));
#65409=DIRECTION('',(0.,0.,-1.));
#65410=DIRECTION('',(-1.,0.,0.));
#65411=DIRECTION('',(0.,0.,-1.));
#65412=DIRECTION('center_axis',(1.,0.,0.));
#65413=DIRECTION('ref_axis',(0.,-1.,0.));
#65414=DIRECTION('',(0.,-1.,0.));
#65415=DIRECTION('',(0.,0.,-1.));
#65416=DIRECTION('',(0.,-1.,0.));
#65417=DIRECTION('center_axis',(0.,1.,0.));
#65418=DIRECTION('ref_axis',(1.,0.,0.));
#65419=DIRECTION('',(1.,0.,0.));
#65420=DIRECTION('',(0.,0.,-1.));
#65421=DIRECTION('',(1.,0.,0.));
#65422=DIRECTION('center_axis',(-1.,0.,0.));
#65423=DIRECTION('ref_axis',(0.,1.,0.));
#65424=DIRECTION('',(0.,1.,0.));
#65425=DIRECTION('',(0.,1.,0.));
#65426=DIRECTION('center_axis',(0.,0.,-1.));
#65427=DIRECTION('ref_axis',(-1.,0.,0.));
#65428=DIRECTION('center_axis',(0.,-1.,0.));
#65429=DIRECTION('ref_axis',(-1.,0.,0.));
#65430=DIRECTION('',(-1.,0.,0.));
#65431=DIRECTION('',(0.,0.,-1.));
#65432=DIRECTION('',(-1.,0.,0.));
#65433=DIRECTION('',(0.,0.,-1.));
#65434=DIRECTION('center_axis',(1.,0.,0.));
#65435=DIRECTION('ref_axis',(0.,-1.,0.));
#65436=DIRECTION('',(0.,-1.,0.));
#65437=DIRECTION('',(0.,0.,-1.));
#65438=DIRECTION('',(0.,-1.,0.));
#65439=DIRECTION('center_axis',(0.,1.,0.));
#65440=DIRECTION('ref_axis',(1.,0.,0.));
#65441=DIRECTION('',(1.,0.,0.));
#65442=DIRECTION('',(0.,0.,-1.));
#65443=DIRECTION('',(1.,0.,0.));
#65444=DIRECTION('center_axis',(-1.,0.,0.));
#65445=DIRECTION('ref_axis',(0.,1.,0.));
#65446=DIRECTION('',(0.,1.,0.));
#65447=DIRECTION('',(0.,1.,0.));
#65448=DIRECTION('center_axis',(0.,0.,-1.));
#65449=DIRECTION('ref_axis',(-1.,0.,0.));
#65450=DIRECTION('center_axis',(0.,-1.,0.));
#65451=DIRECTION('ref_axis',(-1.,0.,0.));
#65452=DIRECTION('',(-1.,0.,0.));
#65453=DIRECTION('',(0.,0.,-1.));
#65454=DIRECTION('',(-1.,0.,0.));
#65455=DIRECTION('',(0.,0.,-1.));
#65456=DIRECTION('center_axis',(1.,0.,0.));
#65457=DIRECTION('ref_axis',(0.,-1.,0.));
#65458=DIRECTION('',(0.,-1.,0.));
#65459=DIRECTION('',(0.,0.,-1.));
#65460=DIRECTION('',(0.,-1.,0.));
#65461=DIRECTION('center_axis',(0.,1.,0.));
#65462=DIRECTION('ref_axis',(1.,0.,0.));
#65463=DIRECTION('',(1.,0.,0.));
#65464=DIRECTION('',(0.,0.,-1.));
#65465=DIRECTION('',(1.,0.,0.));
#65466=DIRECTION('center_axis',(-1.,0.,0.));
#65467=DIRECTION('ref_axis',(0.,1.,0.));
#65468=DIRECTION('',(0.,1.,0.));
#65469=DIRECTION('',(0.,1.,0.));
#65470=DIRECTION('center_axis',(0.,0.,-1.));
#65471=DIRECTION('ref_axis',(-1.,0.,0.));
#65472=DIRECTION('center_axis',(0.,-1.,0.));
#65473=DIRECTION('ref_axis',(-1.,0.,0.));
#65474=DIRECTION('',(-1.,0.,0.));
#65475=DIRECTION('',(0.,0.,-1.));
#65476=DIRECTION('',(-1.,0.,0.));
#65477=DIRECTION('',(0.,0.,-1.));
#65478=DIRECTION('center_axis',(1.,0.,0.));
#65479=DIRECTION('ref_axis',(0.,-1.,0.));
#65480=DIRECTION('',(0.,-1.,0.));
#65481=DIRECTION('',(0.,0.,-1.));
#65482=DIRECTION('',(0.,-1.,0.));
#65483=DIRECTION('center_axis',(0.,1.,0.));
#65484=DIRECTION('ref_axis',(1.,0.,0.));
#65485=DIRECTION('',(1.,0.,0.));
#65486=DIRECTION('',(0.,0.,-1.));
#65487=DIRECTION('',(1.,0.,0.));
#65488=DIRECTION('center_axis',(-1.,0.,0.));
#65489=DIRECTION('ref_axis',(0.,1.,0.));
#65490=DIRECTION('',(0.,1.,0.));
#65491=DIRECTION('',(0.,1.,0.));
#65492=DIRECTION('center_axis',(0.,0.,-1.));
#65493=DIRECTION('ref_axis',(-1.,0.,0.));
#65494=DIRECTION('center_axis',(0.,-1.,0.));
#65495=DIRECTION('ref_axis',(-1.,0.,0.));
#65496=DIRECTION('',(-1.,0.,0.));
#65497=DIRECTION('',(0.,0.,-1.));
#65498=DIRECTION('',(-1.,0.,0.));
#65499=DIRECTION('',(0.,0.,-1.));
#65500=DIRECTION('center_axis',(1.,0.,0.));
#65501=DIRECTION('ref_axis',(0.,-1.,0.));
#65502=DIRECTION('',(0.,-1.,0.));
#65503=DIRECTION('',(0.,0.,-1.));
#65504=DIRECTION('',(0.,-1.,0.));
#65505=DIRECTION('center_axis',(0.,1.,0.));
#65506=DIRECTION('ref_axis',(1.,0.,0.));
#65507=DIRECTION('',(1.,0.,0.));
#65508=DIRECTION('',(0.,0.,-1.));
#65509=DIRECTION('',(1.,0.,0.));
#65510=DIRECTION('center_axis',(-1.,0.,0.));
#65511=DIRECTION('ref_axis',(0.,1.,0.));
#65512=DIRECTION('',(0.,1.,0.));
#65513=DIRECTION('',(0.,1.,0.));
#65514=DIRECTION('center_axis',(0.,0.,-1.));
#65515=DIRECTION('ref_axis',(-1.,0.,0.));
#65516=DIRECTION('center_axis',(0.,-1.,0.));
#65517=DIRECTION('ref_axis',(-1.,0.,0.));
#65518=DIRECTION('',(-1.,0.,0.));
#65519=DIRECTION('',(0.,0.,-1.));
#65520=DIRECTION('',(-1.,0.,0.));
#65521=DIRECTION('',(0.,0.,-1.));
#65522=DIRECTION('center_axis',(1.,0.,0.));
#65523=DIRECTION('ref_axis',(0.,-1.,0.));
#65524=DIRECTION('',(0.,-1.,0.));
#65525=DIRECTION('',(0.,0.,-1.));
#65526=DIRECTION('',(0.,-1.,0.));
#65527=DIRECTION('center_axis',(0.,1.,0.));
#65528=DIRECTION('ref_axis',(1.,0.,0.));
#65529=DIRECTION('',(1.,0.,0.));
#65530=DIRECTION('',(0.,0.,-1.));
#65531=DIRECTION('',(1.,0.,0.));
#65532=DIRECTION('center_axis',(-1.,0.,0.));
#65533=DIRECTION('ref_axis',(0.,1.,0.));
#65534=DIRECTION('',(0.,1.,0.));
#65535=DIRECTION('',(0.,1.,0.));
#65536=DIRECTION('center_axis',(0.,0.,-1.));
#65537=DIRECTION('ref_axis',(-1.,0.,0.));
#65538=DIRECTION('center_axis',(0.,-1.,0.));
#65539=DIRECTION('ref_axis',(-1.,0.,0.));
#65540=DIRECTION('',(-1.,0.,0.));
#65541=DIRECTION('',(0.,0.,-1.));
#65542=DIRECTION('',(-1.,0.,0.));
#65543=DIRECTION('',(0.,0.,-1.));
#65544=DIRECTION('center_axis',(1.,0.,0.));
#65545=DIRECTION('ref_axis',(0.,-1.,0.));
#65546=DIRECTION('',(0.,-1.,0.));
#65547=DIRECTION('',(0.,0.,-1.));
#65548=DIRECTION('',(0.,-1.,0.));
#65549=DIRECTION('center_axis',(0.,1.,0.));
#65550=DIRECTION('ref_axis',(1.,0.,0.));
#65551=DIRECTION('',(1.,0.,0.));
#65552=DIRECTION('',(0.,0.,-1.));
#65553=DIRECTION('',(1.,0.,0.));
#65554=DIRECTION('center_axis',(-1.,0.,0.));
#65555=DIRECTION('ref_axis',(0.,1.,0.));
#65556=DIRECTION('',(0.,1.,0.));
#65557=DIRECTION('',(0.,1.,0.));
#65558=DIRECTION('center_axis',(0.,0.,-1.));
#65559=DIRECTION('ref_axis',(-1.,0.,0.));
#65560=DIRECTION('center_axis',(0.,-1.,0.));
#65561=DIRECTION('ref_axis',(-1.,0.,0.));
#65562=DIRECTION('',(-1.,0.,0.));
#65563=DIRECTION('',(0.,0.,-1.));
#65564=DIRECTION('',(-1.,0.,0.));
#65565=DIRECTION('',(0.,0.,-1.));
#65566=DIRECTION('center_axis',(1.,0.,0.));
#65567=DIRECTION('ref_axis',(0.,-1.,0.));
#65568=DIRECTION('',(0.,-1.,0.));
#65569=DIRECTION('',(0.,0.,-1.));
#65570=DIRECTION('',(0.,-1.,0.));
#65571=DIRECTION('center_axis',(0.,1.,0.));
#65572=DIRECTION('ref_axis',(1.,0.,0.));
#65573=DIRECTION('',(1.,0.,0.));
#65574=DIRECTION('',(0.,0.,-1.));
#65575=DIRECTION('',(1.,0.,0.));
#65576=DIRECTION('center_axis',(-1.,0.,0.));
#65577=DIRECTION('ref_axis',(0.,1.,0.));
#65578=DIRECTION('',(0.,1.,0.));
#65579=DIRECTION('',(0.,1.,0.));
#65580=DIRECTION('center_axis',(0.,0.,-1.));
#65581=DIRECTION('ref_axis',(-1.,0.,0.));
#65582=DIRECTION('center_axis',(0.,-1.,0.));
#65583=DIRECTION('ref_axis',(-1.,0.,0.));
#65584=DIRECTION('',(-1.,0.,0.));
#65585=DIRECTION('',(0.,0.,-1.));
#65586=DIRECTION('',(-1.,0.,0.));
#65587=DIRECTION('',(0.,0.,-1.));
#65588=DIRECTION('center_axis',(1.,0.,0.));
#65589=DIRECTION('ref_axis',(0.,-1.,0.));
#65590=DIRECTION('',(0.,-1.,0.));
#65591=DIRECTION('',(0.,0.,-1.));
#65592=DIRECTION('',(0.,-1.,0.));
#65593=DIRECTION('center_axis',(0.,1.,0.));
#65594=DIRECTION('ref_axis',(1.,0.,0.));
#65595=DIRECTION('',(1.,0.,0.));
#65596=DIRECTION('',(0.,0.,-1.));
#65597=DIRECTION('',(1.,0.,0.));
#65598=DIRECTION('center_axis',(-1.,0.,0.));
#65599=DIRECTION('ref_axis',(0.,1.,0.));
#65600=DIRECTION('',(0.,1.,0.));
#65601=DIRECTION('',(0.,1.,0.));
#65602=DIRECTION('center_axis',(0.,0.,-1.));
#65603=DIRECTION('ref_axis',(-1.,0.,0.));
#65604=DIRECTION('center_axis',(0.,-1.,0.));
#65605=DIRECTION('ref_axis',(-1.,0.,0.));
#65606=DIRECTION('',(-1.,0.,0.));
#65607=DIRECTION('',(0.,0.,-1.));
#65608=DIRECTION('',(-1.,0.,0.));
#65609=DIRECTION('',(0.,0.,-1.));
#65610=DIRECTION('center_axis',(1.,0.,0.));
#65611=DIRECTION('ref_axis',(0.,-1.,0.));
#65612=DIRECTION('',(0.,-1.,0.));
#65613=DIRECTION('',(0.,0.,-1.));
#65614=DIRECTION('',(0.,-1.,0.));
#65615=DIRECTION('center_axis',(0.,1.,0.));
#65616=DIRECTION('ref_axis',(1.,0.,0.));
#65617=DIRECTION('',(1.,0.,0.));
#65618=DIRECTION('',(0.,0.,-1.));
#65619=DIRECTION('',(1.,0.,0.));
#65620=DIRECTION('center_axis',(-1.,0.,0.));
#65621=DIRECTION('ref_axis',(0.,1.,0.));
#65622=DIRECTION('',(0.,1.,0.));
#65623=DIRECTION('',(0.,1.,0.));
#65624=DIRECTION('center_axis',(0.,0.,-1.));
#65625=DIRECTION('ref_axis',(-1.,0.,0.));
#65626=DIRECTION('center_axis',(0.,-1.,0.));
#65627=DIRECTION('ref_axis',(-1.,0.,0.));
#65628=DIRECTION('',(-1.,0.,0.));
#65629=DIRECTION('',(0.,0.,-1.));
#65630=DIRECTION('',(-1.,0.,0.));
#65631=DIRECTION('',(0.,0.,-1.));
#65632=DIRECTION('center_axis',(1.,0.,0.));
#65633=DIRECTION('ref_axis',(0.,-1.,0.));
#65634=DIRECTION('',(0.,-1.,0.));
#65635=DIRECTION('',(0.,0.,-1.));
#65636=DIRECTION('',(0.,-1.,0.));
#65637=DIRECTION('center_axis',(0.,1.,0.));
#65638=DIRECTION('ref_axis',(1.,0.,0.));
#65639=DIRECTION('',(1.,0.,0.));
#65640=DIRECTION('',(0.,0.,-1.));
#65641=DIRECTION('',(1.,0.,0.));
#65642=DIRECTION('center_axis',(-1.,0.,0.));
#65643=DIRECTION('ref_axis',(0.,1.,0.));
#65644=DIRECTION('',(0.,1.,0.));
#65645=DIRECTION('',(0.,1.,0.));
#65646=DIRECTION('center_axis',(0.,0.,-1.));
#65647=DIRECTION('ref_axis',(-1.,0.,0.));
#65648=DIRECTION('center_axis',(0.,-1.,0.));
#65649=DIRECTION('ref_axis',(-1.,0.,0.));
#65650=DIRECTION('',(-1.,0.,0.));
#65651=DIRECTION('',(0.,0.,-1.));
#65652=DIRECTION('',(-1.,0.,0.));
#65653=DIRECTION('',(0.,0.,-1.));
#65654=DIRECTION('center_axis',(1.,0.,0.));
#65655=DIRECTION('ref_axis',(0.,-1.,0.));
#65656=DIRECTION('',(0.,-1.,0.));
#65657=DIRECTION('',(0.,0.,-1.));
#65658=DIRECTION('',(0.,-1.,0.));
#65659=DIRECTION('center_axis',(0.,1.,0.));
#65660=DIRECTION('ref_axis',(1.,0.,0.));
#65661=DIRECTION('',(1.,0.,0.));
#65662=DIRECTION('',(0.,0.,-1.));
#65663=DIRECTION('',(1.,0.,0.));
#65664=DIRECTION('center_axis',(-1.,0.,0.));
#65665=DIRECTION('ref_axis',(0.,1.,0.));
#65666=DIRECTION('',(0.,1.,0.));
#65667=DIRECTION('',(0.,1.,0.));
#65668=DIRECTION('center_axis',(0.,0.,-1.));
#65669=DIRECTION('ref_axis',(-1.,0.,0.));
#65670=DIRECTION('center_axis',(0.,-1.,0.));
#65671=DIRECTION('ref_axis',(-1.,0.,0.));
#65672=DIRECTION('',(-1.,0.,0.));
#65673=DIRECTION('',(0.,0.,-1.));
#65674=DIRECTION('',(-1.,0.,0.));
#65675=DIRECTION('',(0.,0.,-1.));
#65676=DIRECTION('center_axis',(1.,0.,0.));
#65677=DIRECTION('ref_axis',(0.,-1.,0.));
#65678=DIRECTION('',(0.,-1.,0.));
#65679=DIRECTION('',(0.,0.,-1.));
#65680=DIRECTION('',(0.,-1.,0.));
#65681=DIRECTION('center_axis',(0.,1.,0.));
#65682=DIRECTION('ref_axis',(1.,0.,0.));
#65683=DIRECTION('',(1.,0.,0.));
#65684=DIRECTION('',(0.,0.,-1.));
#65685=DIRECTION('',(1.,0.,0.));
#65686=DIRECTION('center_axis',(-1.,0.,0.));
#65687=DIRECTION('ref_axis',(0.,1.,0.));
#65688=DIRECTION('',(0.,1.,0.));
#65689=DIRECTION('',(0.,1.,0.));
#65690=DIRECTION('center_axis',(0.,0.,-1.));
#65691=DIRECTION('ref_axis',(-1.,0.,0.));
#65692=DIRECTION('center_axis',(0.,-1.,0.));
#65693=DIRECTION('ref_axis',(-1.,0.,0.));
#65694=DIRECTION('',(-1.,0.,0.));
#65695=DIRECTION('',(0.,0.,-1.));
#65696=DIRECTION('',(-1.,0.,0.));
#65697=DIRECTION('',(0.,0.,-1.));
#65698=DIRECTION('center_axis',(1.,0.,0.));
#65699=DIRECTION('ref_axis',(0.,-1.,0.));
#65700=DIRECTION('',(0.,-1.,0.));
#65701=DIRECTION('',(0.,0.,-1.));
#65702=DIRECTION('',(0.,-1.,0.));
#65703=DIRECTION('center_axis',(0.,1.,0.));
#65704=DIRECTION('ref_axis',(1.,0.,0.));
#65705=DIRECTION('',(1.,0.,0.));
#65706=DIRECTION('',(0.,0.,-1.));
#65707=DIRECTION('',(1.,0.,0.));
#65708=DIRECTION('center_axis',(-1.,0.,0.));
#65709=DIRECTION('ref_axis',(0.,1.,0.));
#65710=DIRECTION('',(0.,1.,0.));
#65711=DIRECTION('',(0.,1.,0.));
#65712=DIRECTION('center_axis',(0.,0.,-1.));
#65713=DIRECTION('ref_axis',(-1.,0.,0.));
#65714=DIRECTION('center_axis',(0.,-1.,0.));
#65715=DIRECTION('ref_axis',(-1.,0.,0.));
#65716=DIRECTION('',(-1.,0.,0.));
#65717=DIRECTION('',(0.,0.,-1.));
#65718=DIRECTION('',(-1.,0.,0.));
#65719=DIRECTION('',(0.,0.,-1.));
#65720=DIRECTION('center_axis',(1.,0.,0.));
#65721=DIRECTION('ref_axis',(0.,-1.,0.));
#65722=DIRECTION('',(0.,-1.,0.));
#65723=DIRECTION('',(0.,0.,-1.));
#65724=DIRECTION('',(0.,-1.,0.));
#65725=DIRECTION('center_axis',(0.,1.,0.));
#65726=DIRECTION('ref_axis',(1.,0.,0.));
#65727=DIRECTION('',(1.,0.,0.));
#65728=DIRECTION('',(0.,0.,-1.));
#65729=DIRECTION('',(1.,0.,0.));
#65730=DIRECTION('center_axis',(-1.,0.,0.));
#65731=DIRECTION('ref_axis',(0.,1.,0.));
#65732=DIRECTION('',(0.,1.,0.));
#65733=DIRECTION('',(0.,1.,0.));
#65734=DIRECTION('center_axis',(0.,0.,-1.));
#65735=DIRECTION('ref_axis',(-1.,0.,0.));
#65736=DIRECTION('center_axis',(0.,-1.,0.));
#65737=DIRECTION('ref_axis',(-1.,0.,0.));
#65738=DIRECTION('',(-1.,0.,0.));
#65739=DIRECTION('',(0.,0.,-1.));
#65740=DIRECTION('',(-1.,0.,0.));
#65741=DIRECTION('',(0.,0.,-1.));
#65742=DIRECTION('center_axis',(1.,0.,0.));
#65743=DIRECTION('ref_axis',(0.,-1.,0.));
#65744=DIRECTION('',(0.,-1.,0.));
#65745=DIRECTION('',(0.,0.,-1.));
#65746=DIRECTION('',(0.,-1.,0.));
#65747=DIRECTION('center_axis',(0.,1.,0.));
#65748=DIRECTION('ref_axis',(1.,0.,0.));
#65749=DIRECTION('',(1.,0.,0.));
#65750=DIRECTION('',(0.,0.,-1.));
#65751=DIRECTION('',(1.,0.,0.));
#65752=DIRECTION('center_axis',(-1.,0.,0.));
#65753=DIRECTION('ref_axis',(0.,1.,0.));
#65754=DIRECTION('',(0.,1.,0.));
#65755=DIRECTION('',(0.,1.,0.));
#65756=DIRECTION('center_axis',(0.,0.,-1.));
#65757=DIRECTION('ref_axis',(-1.,0.,0.));
#65758=DIRECTION('center_axis',(0.,-1.,0.));
#65759=DIRECTION('ref_axis',(-1.,0.,0.));
#65760=DIRECTION('',(-1.,0.,0.));
#65761=DIRECTION('',(0.,0.,-1.));
#65762=DIRECTION('',(-1.,0.,0.));
#65763=DIRECTION('',(0.,0.,-1.));
#65764=DIRECTION('center_axis',(1.,0.,0.));
#65765=DIRECTION('ref_axis',(0.,-1.,0.));
#65766=DIRECTION('',(0.,-1.,0.));
#65767=DIRECTION('',(0.,0.,-1.));
#65768=DIRECTION('',(0.,-1.,0.));
#65769=DIRECTION('center_axis',(0.,1.,0.));
#65770=DIRECTION('ref_axis',(1.,0.,0.));
#65771=DIRECTION('',(1.,0.,0.));
#65772=DIRECTION('',(0.,0.,-1.));
#65773=DIRECTION('',(1.,0.,0.));
#65774=DIRECTION('center_axis',(-1.,0.,0.));
#65775=DIRECTION('ref_axis',(0.,1.,0.));
#65776=DIRECTION('',(0.,1.,0.));
#65777=DIRECTION('',(0.,1.,0.));
#65778=DIRECTION('center_axis',(0.,0.,-1.));
#65779=DIRECTION('ref_axis',(-1.,0.,0.));
#65780=DIRECTION('center_axis',(0.,-1.,0.));
#65781=DIRECTION('ref_axis',(-1.,0.,0.));
#65782=DIRECTION('',(-1.,0.,0.));
#65783=DIRECTION('',(0.,0.,-1.));
#65784=DIRECTION('',(-1.,0.,0.));
#65785=DIRECTION('',(0.,0.,-1.));
#65786=DIRECTION('center_axis',(1.,0.,0.));
#65787=DIRECTION('ref_axis',(0.,-1.,0.));
#65788=DIRECTION('',(0.,-1.,0.));
#65789=DIRECTION('',(0.,0.,-1.));
#65790=DIRECTION('',(0.,-1.,0.));
#65791=DIRECTION('center_axis',(0.,1.,0.));
#65792=DIRECTION('ref_axis',(1.,0.,0.));
#65793=DIRECTION('',(1.,0.,0.));
#65794=DIRECTION('',(0.,0.,-1.));
#65795=DIRECTION('',(1.,0.,0.));
#65796=DIRECTION('center_axis',(-1.,0.,0.));
#65797=DIRECTION('ref_axis',(0.,1.,0.));
#65798=DIRECTION('',(0.,1.,0.));
#65799=DIRECTION('',(0.,1.,0.));
#65800=DIRECTION('center_axis',(0.,0.,-1.));
#65801=DIRECTION('ref_axis',(-1.,0.,0.));
#65802=DIRECTION('center_axis',(0.,-1.,0.));
#65803=DIRECTION('ref_axis',(-1.,0.,0.));
#65804=DIRECTION('',(-1.,0.,0.));
#65805=DIRECTION('',(0.,0.,-1.));
#65806=DIRECTION('',(-1.,0.,0.));
#65807=DIRECTION('',(0.,0.,-1.));
#65808=DIRECTION('center_axis',(1.,0.,0.));
#65809=DIRECTION('ref_axis',(0.,-1.,0.));
#65810=DIRECTION('',(0.,-1.,0.));
#65811=DIRECTION('',(0.,0.,-1.));
#65812=DIRECTION('',(0.,-1.,0.));
#65813=DIRECTION('center_axis',(0.,1.,0.));
#65814=DIRECTION('ref_axis',(1.,0.,0.));
#65815=DIRECTION('',(1.,0.,0.));
#65816=DIRECTION('',(0.,0.,-1.));
#65817=DIRECTION('',(1.,0.,0.));
#65818=DIRECTION('center_axis',(-1.,0.,0.));
#65819=DIRECTION('ref_axis',(0.,1.,0.));
#65820=DIRECTION('',(0.,1.,0.));
#65821=DIRECTION('',(0.,1.,0.));
#65822=DIRECTION('center_axis',(0.,0.,-1.));
#65823=DIRECTION('ref_axis',(-1.,0.,0.));
#65824=DIRECTION('center_axis',(0.,-1.,0.));
#65825=DIRECTION('ref_axis',(-1.,0.,0.));
#65826=DIRECTION('',(-1.,0.,0.));
#65827=DIRECTION('',(0.,0.,-1.));
#65828=DIRECTION('',(-1.,0.,0.));
#65829=DIRECTION('',(0.,0.,-1.));
#65830=DIRECTION('center_axis',(1.,0.,0.));
#65831=DIRECTION('ref_axis',(0.,-1.,0.));
#65832=DIRECTION('',(0.,-1.,0.));
#65833=DIRECTION('',(0.,0.,-1.));
#65834=DIRECTION('',(0.,-1.,0.));
#65835=DIRECTION('center_axis',(0.,1.,0.));
#65836=DIRECTION('ref_axis',(1.,0.,0.));
#65837=DIRECTION('',(1.,0.,0.));
#65838=DIRECTION('',(0.,0.,-1.));
#65839=DIRECTION('',(1.,0.,0.));
#65840=DIRECTION('center_axis',(-1.,0.,0.));
#65841=DIRECTION('ref_axis',(0.,1.,0.));
#65842=DIRECTION('',(0.,1.,0.));
#65843=DIRECTION('',(0.,1.,0.));
#65844=DIRECTION('center_axis',(0.,0.,-1.));
#65845=DIRECTION('ref_axis',(-1.,0.,0.));
#65846=DIRECTION('center_axis',(0.,-1.,0.));
#65847=DIRECTION('ref_axis',(-1.,0.,0.));
#65848=DIRECTION('',(-1.,0.,0.));
#65849=DIRECTION('',(0.,0.,-1.));
#65850=DIRECTION('',(-1.,0.,0.));
#65851=DIRECTION('',(0.,0.,-1.));
#65852=DIRECTION('center_axis',(1.,0.,0.));
#65853=DIRECTION('ref_axis',(0.,-1.,0.));
#65854=DIRECTION('',(0.,-1.,0.));
#65855=DIRECTION('',(0.,0.,-1.));
#65856=DIRECTION('',(0.,-1.,0.));
#65857=DIRECTION('center_axis',(0.,1.,0.));
#65858=DIRECTION('ref_axis',(1.,0.,0.));
#65859=DIRECTION('',(1.,0.,0.));
#65860=DIRECTION('',(0.,0.,-1.));
#65861=DIRECTION('',(1.,0.,0.));
#65862=DIRECTION('center_axis',(-1.,0.,0.));
#65863=DIRECTION('ref_axis',(0.,1.,0.));
#65864=DIRECTION('',(0.,1.,0.));
#65865=DIRECTION('',(0.,1.,0.));
#65866=DIRECTION('center_axis',(0.,0.,-1.));
#65867=DIRECTION('ref_axis',(-1.,0.,0.));
#65868=DIRECTION('center_axis',(0.,-1.,0.));
#65869=DIRECTION('ref_axis',(-1.,0.,0.));
#65870=DIRECTION('',(-1.,0.,0.));
#65871=DIRECTION('',(0.,0.,-1.));
#65872=DIRECTION('',(-1.,0.,0.));
#65873=DIRECTION('',(0.,0.,-1.));
#65874=DIRECTION('center_axis',(1.,0.,0.));
#65875=DIRECTION('ref_axis',(0.,-1.,0.));
#65876=DIRECTION('',(0.,-1.,0.));
#65877=DIRECTION('',(0.,0.,-1.));
#65878=DIRECTION('',(0.,-1.,0.));
#65879=DIRECTION('center_axis',(0.,1.,0.));
#65880=DIRECTION('ref_axis',(1.,0.,0.));
#65881=DIRECTION('',(1.,0.,0.));
#65882=DIRECTION('',(0.,0.,-1.));
#65883=DIRECTION('',(1.,0.,0.));
#65884=DIRECTION('center_axis',(-1.,0.,0.));
#65885=DIRECTION('ref_axis',(0.,1.,0.));
#65886=DIRECTION('',(0.,1.,0.));
#65887=DIRECTION('',(0.,1.,0.));
#65888=DIRECTION('center_axis',(0.,0.,-1.));
#65889=DIRECTION('ref_axis',(-1.,0.,0.));
#65890=DIRECTION('center_axis',(0.,-1.,0.));
#65891=DIRECTION('ref_axis',(-1.,0.,0.));
#65892=DIRECTION('',(-1.,0.,0.));
#65893=DIRECTION('',(0.,0.,-1.));
#65894=DIRECTION('',(-1.,0.,0.));
#65895=DIRECTION('',(0.,0.,-1.));
#65896=DIRECTION('center_axis',(1.,0.,0.));
#65897=DIRECTION('ref_axis',(0.,-1.,0.));
#65898=DIRECTION('',(0.,-1.,0.));
#65899=DIRECTION('',(0.,0.,-1.));
#65900=DIRECTION('',(0.,-1.,0.));
#65901=DIRECTION('center_axis',(0.,1.,0.));
#65902=DIRECTION('ref_axis',(1.,0.,0.));
#65903=DIRECTION('',(1.,0.,0.));
#65904=DIRECTION('',(0.,0.,-1.));
#65905=DIRECTION('',(1.,0.,0.));
#65906=DIRECTION('center_axis',(-1.,0.,0.));
#65907=DIRECTION('ref_axis',(0.,1.,0.));
#65908=DIRECTION('',(0.,1.,0.));
#65909=DIRECTION('',(0.,1.,0.));
#65910=DIRECTION('center_axis',(0.,0.,-1.));
#65911=DIRECTION('ref_axis',(-1.,0.,0.));
#65912=DIRECTION('center_axis',(0.,-1.,0.));
#65913=DIRECTION('ref_axis',(-1.,0.,0.));
#65914=DIRECTION('',(-1.,0.,0.));
#65915=DIRECTION('',(0.,0.,-1.));
#65916=DIRECTION('',(-1.,0.,0.));
#65917=DIRECTION('',(0.,0.,-1.));
#65918=DIRECTION('center_axis',(1.,0.,0.));
#65919=DIRECTION('ref_axis',(0.,-1.,0.));
#65920=DIRECTION('',(0.,-1.,0.));
#65921=DIRECTION('',(0.,0.,-1.));
#65922=DIRECTION('',(0.,-1.,0.));
#65923=DIRECTION('center_axis',(0.,1.,0.));
#65924=DIRECTION('ref_axis',(1.,0.,0.));
#65925=DIRECTION('',(1.,0.,0.));
#65926=DIRECTION('',(0.,0.,-1.));
#65927=DIRECTION('',(1.,0.,0.));
#65928=DIRECTION('center_axis',(-1.,0.,0.));
#65929=DIRECTION('ref_axis',(0.,1.,0.));
#65930=DIRECTION('',(0.,1.,0.));
#65931=DIRECTION('',(0.,1.,0.));
#65932=DIRECTION('center_axis',(0.,0.,-1.));
#65933=DIRECTION('ref_axis',(-1.,0.,0.));
#65934=DIRECTION('center_axis',(0.,-1.,0.));
#65935=DIRECTION('ref_axis',(-1.,0.,0.));
#65936=DIRECTION('',(-1.,0.,0.));
#65937=DIRECTION('',(0.,0.,-1.));
#65938=DIRECTION('',(-1.,0.,0.));
#65939=DIRECTION('',(0.,0.,-1.));
#65940=DIRECTION('center_axis',(1.,0.,0.));
#65941=DIRECTION('ref_axis',(0.,-1.,0.));
#65942=DIRECTION('',(0.,-1.,0.));
#65943=DIRECTION('',(0.,0.,-1.));
#65944=DIRECTION('',(0.,-1.,0.));
#65945=DIRECTION('center_axis',(0.,1.,0.));
#65946=DIRECTION('ref_axis',(1.,0.,0.));
#65947=DIRECTION('',(1.,0.,0.));
#65948=DIRECTION('',(0.,0.,-1.));
#65949=DIRECTION('',(1.,0.,0.));
#65950=DIRECTION('center_axis',(-1.,0.,0.));
#65951=DIRECTION('ref_axis',(0.,1.,0.));
#65952=DIRECTION('',(0.,1.,0.));
#65953=DIRECTION('',(0.,1.,0.));
#65954=DIRECTION('center_axis',(0.,0.,-1.));
#65955=DIRECTION('ref_axis',(-1.,0.,0.));
#65956=DIRECTION('center_axis',(0.,-1.,0.));
#65957=DIRECTION('ref_axis',(-1.,0.,0.));
#65958=DIRECTION('',(-1.,0.,0.));
#65959=DIRECTION('',(0.,0.,-1.));
#65960=DIRECTION('',(-1.,0.,0.));
#65961=DIRECTION('',(0.,0.,-1.));
#65962=DIRECTION('center_axis',(1.,0.,0.));
#65963=DIRECTION('ref_axis',(0.,-1.,0.));
#65964=DIRECTION('',(0.,-1.,0.));
#65965=DIRECTION('',(0.,0.,-1.));
#65966=DIRECTION('',(0.,-1.,0.));
#65967=DIRECTION('center_axis',(0.,1.,0.));
#65968=DIRECTION('ref_axis',(1.,0.,0.));
#65969=DIRECTION('',(1.,0.,0.));
#65970=DIRECTION('',(0.,0.,-1.));
#65971=DIRECTION('',(1.,0.,0.));
#65972=DIRECTION('center_axis',(-1.,0.,0.));
#65973=DIRECTION('ref_axis',(0.,1.,0.));
#65974=DIRECTION('',(0.,1.,0.));
#65975=DIRECTION('',(0.,1.,0.));
#65976=DIRECTION('center_axis',(0.,0.,-1.));
#65977=DIRECTION('ref_axis',(-1.,0.,0.));
#65978=DIRECTION('center_axis',(0.,-1.,0.));
#65979=DIRECTION('ref_axis',(-1.,0.,0.));
#65980=DIRECTION('',(-1.,0.,0.));
#65981=DIRECTION('',(0.,0.,-1.));
#65982=DIRECTION('',(-1.,0.,0.));
#65983=DIRECTION('',(0.,0.,-1.));
#65984=DIRECTION('center_axis',(1.,0.,0.));
#65985=DIRECTION('ref_axis',(0.,-1.,0.));
#65986=DIRECTION('',(0.,-1.,0.));
#65987=DIRECTION('',(0.,0.,-1.));
#65988=DIRECTION('',(0.,-1.,0.));
#65989=DIRECTION('center_axis',(0.,1.,0.));
#65990=DIRECTION('ref_axis',(1.,0.,0.));
#65991=DIRECTION('',(1.,0.,0.));
#65992=DIRECTION('',(0.,0.,-1.));
#65993=DIRECTION('',(1.,0.,0.));
#65994=DIRECTION('center_axis',(-1.,0.,0.));
#65995=DIRECTION('ref_axis',(0.,1.,0.));
#65996=DIRECTION('',(0.,1.,0.));
#65997=DIRECTION('',(0.,1.,0.));
#65998=DIRECTION('center_axis',(0.,0.,-1.));
#65999=DIRECTION('ref_axis',(-1.,0.,0.));
#66000=DIRECTION('center_axis',(0.,-1.,0.));
#66001=DIRECTION('ref_axis',(-1.,0.,0.));
#66002=DIRECTION('',(-1.,0.,0.));
#66003=DIRECTION('',(0.,0.,-1.));
#66004=DIRECTION('',(-1.,0.,0.));
#66005=DIRECTION('',(0.,0.,-1.));
#66006=DIRECTION('center_axis',(1.,0.,0.));
#66007=DIRECTION('ref_axis',(0.,-1.,0.));
#66008=DIRECTION('',(0.,-1.,0.));
#66009=DIRECTION('',(0.,0.,-1.));
#66010=DIRECTION('',(0.,-1.,0.));
#66011=DIRECTION('center_axis',(0.,1.,0.));
#66012=DIRECTION('ref_axis',(1.,0.,0.));
#66013=DIRECTION('',(1.,0.,0.));
#66014=DIRECTION('',(0.,0.,-1.));
#66015=DIRECTION('',(1.,0.,0.));
#66016=DIRECTION('center_axis',(-1.,0.,0.));
#66017=DIRECTION('ref_axis',(0.,1.,0.));
#66018=DIRECTION('',(0.,1.,0.));
#66019=DIRECTION('',(0.,1.,0.));
#66020=DIRECTION('center_axis',(0.,0.,-1.));
#66021=DIRECTION('ref_axis',(-1.,0.,0.));
#66022=DIRECTION('center_axis',(0.,-1.,0.));
#66023=DIRECTION('ref_axis',(-1.,0.,0.));
#66024=DIRECTION('',(-1.,0.,0.));
#66025=DIRECTION('',(0.,0.,-1.));
#66026=DIRECTION('',(-1.,0.,0.));
#66027=DIRECTION('',(0.,0.,-1.));
#66028=DIRECTION('center_axis',(1.,0.,0.));
#66029=DIRECTION('ref_axis',(0.,-1.,0.));
#66030=DIRECTION('',(0.,-1.,0.));
#66031=DIRECTION('',(0.,0.,-1.));
#66032=DIRECTION('',(0.,-1.,0.));
#66033=DIRECTION('center_axis',(0.,1.,0.));
#66034=DIRECTION('ref_axis',(1.,0.,0.));
#66035=DIRECTION('',(1.,0.,0.));
#66036=DIRECTION('',(0.,0.,-1.));
#66037=DIRECTION('',(1.,0.,0.));
#66038=DIRECTION('center_axis',(-1.,0.,0.));
#66039=DIRECTION('ref_axis',(0.,1.,0.));
#66040=DIRECTION('',(0.,1.,0.));
#66041=DIRECTION('',(0.,1.,0.));
#66042=DIRECTION('center_axis',(0.,0.,-1.));
#66043=DIRECTION('ref_axis',(-1.,0.,0.));
#66044=DIRECTION('center_axis',(0.,-1.,0.));
#66045=DIRECTION('ref_axis',(-1.,0.,0.));
#66046=DIRECTION('',(-1.,0.,0.));
#66047=DIRECTION('',(0.,0.,-1.));
#66048=DIRECTION('',(-1.,0.,0.));
#66049=DIRECTION('',(0.,0.,-1.));
#66050=DIRECTION('center_axis',(1.,0.,0.));
#66051=DIRECTION('ref_axis',(0.,-1.,0.));
#66052=DIRECTION('',(0.,-1.,0.));
#66053=DIRECTION('',(0.,0.,-1.));
#66054=DIRECTION('',(0.,-1.,0.));
#66055=DIRECTION('center_axis',(0.,1.,0.));
#66056=DIRECTION('ref_axis',(1.,0.,0.));
#66057=DIRECTION('',(1.,0.,0.));
#66058=DIRECTION('',(0.,0.,-1.));
#66059=DIRECTION('',(1.,0.,0.));
#66060=DIRECTION('center_axis',(-1.,0.,0.));
#66061=DIRECTION('ref_axis',(0.,1.,0.));
#66062=DIRECTION('',(0.,1.,0.));
#66063=DIRECTION('',(0.,1.,0.));
#66064=DIRECTION('center_axis',(0.,0.,-1.));
#66065=DIRECTION('ref_axis',(-1.,0.,0.));
#66066=DIRECTION('center_axis',(0.,-1.,0.));
#66067=DIRECTION('ref_axis',(-1.,0.,0.));
#66068=DIRECTION('',(-1.,0.,0.));
#66069=DIRECTION('',(0.,0.,-1.));
#66070=DIRECTION('',(-1.,0.,0.));
#66071=DIRECTION('',(0.,0.,-1.));
#66072=DIRECTION('center_axis',(1.,0.,0.));
#66073=DIRECTION('ref_axis',(0.,-1.,0.));
#66074=DIRECTION('',(0.,-1.,0.));
#66075=DIRECTION('',(0.,0.,-1.));
#66076=DIRECTION('',(0.,-1.,0.));
#66077=DIRECTION('center_axis',(0.,1.,0.));
#66078=DIRECTION('ref_axis',(1.,0.,0.));
#66079=DIRECTION('',(1.,0.,0.));
#66080=DIRECTION('',(0.,0.,-1.));
#66081=DIRECTION('',(1.,0.,0.));
#66082=DIRECTION('center_axis',(-1.,0.,0.));
#66083=DIRECTION('ref_axis',(0.,1.,0.));
#66084=DIRECTION('',(0.,1.,0.));
#66085=DIRECTION('',(0.,1.,0.));
#66086=DIRECTION('center_axis',(0.,0.,-1.));
#66087=DIRECTION('ref_axis',(-1.,0.,0.));
#66088=DIRECTION('center_axis',(0.,-1.,0.));
#66089=DIRECTION('ref_axis',(-1.,0.,0.));
#66090=DIRECTION('',(-1.,0.,0.));
#66091=DIRECTION('',(0.,0.,-1.));
#66092=DIRECTION('',(-1.,0.,0.));
#66093=DIRECTION('',(0.,0.,-1.));
#66094=DIRECTION('center_axis',(1.,0.,0.));
#66095=DIRECTION('ref_axis',(0.,-1.,0.));
#66096=DIRECTION('',(0.,-1.,0.));
#66097=DIRECTION('',(0.,0.,-1.));
#66098=DIRECTION('',(0.,-1.,0.));
#66099=DIRECTION('center_axis',(0.,1.,0.));
#66100=DIRECTION('ref_axis',(1.,0.,0.));
#66101=DIRECTION('',(1.,0.,0.));
#66102=DIRECTION('',(0.,0.,-1.));
#66103=DIRECTION('',(1.,0.,0.));
#66104=DIRECTION('center_axis',(-1.,0.,0.));
#66105=DIRECTION('ref_axis',(0.,1.,0.));
#66106=DIRECTION('',(0.,1.,0.));
#66107=DIRECTION('',(0.,1.,0.));
#66108=DIRECTION('center_axis',(0.,0.,-1.));
#66109=DIRECTION('ref_axis',(-1.,0.,0.));
#66110=DIRECTION('center_axis',(0.,-1.,0.));
#66111=DIRECTION('ref_axis',(-1.,0.,0.));
#66112=DIRECTION('',(-1.,0.,0.));
#66113=DIRECTION('',(0.,0.,-1.));
#66114=DIRECTION('',(-1.,0.,0.));
#66115=DIRECTION('',(0.,0.,-1.));
#66116=DIRECTION('center_axis',(1.,0.,0.));
#66117=DIRECTION('ref_axis',(0.,-1.,0.));
#66118=DIRECTION('',(0.,-1.,0.));
#66119=DIRECTION('',(0.,0.,-1.));
#66120=DIRECTION('',(0.,-1.,0.));
#66121=DIRECTION('center_axis',(0.,1.,0.));
#66122=DIRECTION('ref_axis',(1.,0.,0.));
#66123=DIRECTION('',(1.,0.,0.));
#66124=DIRECTION('',(0.,0.,-1.));
#66125=DIRECTION('',(1.,0.,0.));
#66126=DIRECTION('center_axis',(-1.,0.,0.));
#66127=DIRECTION('ref_axis',(0.,1.,0.));
#66128=DIRECTION('',(0.,1.,0.));
#66129=DIRECTION('',(0.,1.,0.));
#66130=DIRECTION('center_axis',(0.,0.,-1.));
#66131=DIRECTION('ref_axis',(-1.,0.,0.));
#66132=DIRECTION('center_axis',(0.,-1.,0.));
#66133=DIRECTION('ref_axis',(-1.,0.,0.));
#66134=DIRECTION('',(-1.,0.,0.));
#66135=DIRECTION('',(0.,0.,-1.));
#66136=DIRECTION('',(-1.,0.,0.));
#66137=DIRECTION('',(0.,0.,-1.));
#66138=DIRECTION('center_axis',(1.,0.,0.));
#66139=DIRECTION('ref_axis',(0.,-1.,0.));
#66140=DIRECTION('',(0.,-1.,0.));
#66141=DIRECTION('',(0.,0.,-1.));
#66142=DIRECTION('',(0.,-1.,0.));
#66143=DIRECTION('center_axis',(0.,1.,0.));
#66144=DIRECTION('ref_axis',(1.,0.,0.));
#66145=DIRECTION('',(1.,0.,0.));
#66146=DIRECTION('',(0.,0.,-1.));
#66147=DIRECTION('',(1.,0.,0.));
#66148=DIRECTION('center_axis',(-1.,0.,0.));
#66149=DIRECTION('ref_axis',(0.,1.,0.));
#66150=DIRECTION('',(0.,1.,0.));
#66151=DIRECTION('',(0.,1.,0.));
#66152=DIRECTION('center_axis',(0.,0.,-1.));
#66153=DIRECTION('ref_axis',(-1.,0.,0.));
#66154=DIRECTION('center_axis',(0.,-1.,0.));
#66155=DIRECTION('ref_axis',(-1.,0.,0.));
#66156=DIRECTION('',(-1.,0.,0.));
#66157=DIRECTION('',(0.,0.,-1.));
#66158=DIRECTION('',(-1.,0.,0.));
#66159=DIRECTION('',(0.,0.,-1.));
#66160=DIRECTION('center_axis',(1.,0.,0.));
#66161=DIRECTION('ref_axis',(0.,-1.,0.));
#66162=DIRECTION('',(0.,-1.,0.));
#66163=DIRECTION('',(0.,0.,-1.));
#66164=DIRECTION('',(0.,-1.,0.));
#66165=DIRECTION('center_axis',(0.,1.,0.));
#66166=DIRECTION('ref_axis',(1.,0.,0.));
#66167=DIRECTION('',(1.,0.,0.));
#66168=DIRECTION('',(0.,0.,-1.));
#66169=DIRECTION('',(1.,0.,0.));
#66170=DIRECTION('center_axis',(-1.,0.,0.));
#66171=DIRECTION('ref_axis',(0.,1.,0.));
#66172=DIRECTION('',(0.,1.,0.));
#66173=DIRECTION('',(0.,1.,0.));
#66174=DIRECTION('center_axis',(0.,0.,-1.));
#66175=DIRECTION('ref_axis',(-1.,0.,0.));
#66176=DIRECTION('center_axis',(0.,-1.,0.));
#66177=DIRECTION('ref_axis',(-1.,0.,0.));
#66178=DIRECTION('',(-1.,0.,0.));
#66179=DIRECTION('',(0.,0.,-1.));
#66180=DIRECTION('',(-1.,0.,0.));
#66181=DIRECTION('',(0.,0.,-1.));
#66182=DIRECTION('center_axis',(1.,0.,0.));
#66183=DIRECTION('ref_axis',(0.,-1.,0.));
#66184=DIRECTION('',(0.,-1.,0.));
#66185=DIRECTION('',(0.,0.,-1.));
#66186=DIRECTION('',(0.,-1.,0.));
#66187=DIRECTION('center_axis',(0.,1.,0.));
#66188=DIRECTION('ref_axis',(1.,0.,0.));
#66189=DIRECTION('',(1.,0.,0.));
#66190=DIRECTION('',(0.,0.,-1.));
#66191=DIRECTION('',(1.,0.,0.));
#66192=DIRECTION('center_axis',(-1.,0.,0.));
#66193=DIRECTION('ref_axis',(0.,1.,0.));
#66194=DIRECTION('',(0.,1.,0.));
#66195=DIRECTION('',(0.,1.,0.));
#66196=DIRECTION('center_axis',(0.,0.,-1.));
#66197=DIRECTION('ref_axis',(-1.,0.,0.));
#66198=DIRECTION('center_axis',(0.,-1.,0.));
#66199=DIRECTION('ref_axis',(-1.,0.,0.));
#66200=DIRECTION('',(-1.,0.,0.));
#66201=DIRECTION('',(0.,0.,-1.));
#66202=DIRECTION('',(-1.,0.,0.));
#66203=DIRECTION('',(0.,0.,-1.));
#66204=DIRECTION('center_axis',(1.,0.,0.));
#66205=DIRECTION('ref_axis',(0.,-1.,0.));
#66206=DIRECTION('',(0.,-1.,0.));
#66207=DIRECTION('',(0.,0.,-1.));
#66208=DIRECTION('',(0.,-1.,0.));
#66209=DIRECTION('center_axis',(0.,1.,0.));
#66210=DIRECTION('ref_axis',(1.,0.,0.));
#66211=DIRECTION('',(1.,0.,0.));
#66212=DIRECTION('',(0.,0.,-1.));
#66213=DIRECTION('',(1.,0.,0.));
#66214=DIRECTION('center_axis',(-1.,0.,0.));
#66215=DIRECTION('ref_axis',(0.,1.,0.));
#66216=DIRECTION('',(0.,1.,0.));
#66217=DIRECTION('',(0.,1.,0.));
#66218=DIRECTION('center_axis',(0.,0.,-1.));
#66219=DIRECTION('ref_axis',(-1.,0.,0.));
#66220=DIRECTION('center_axis',(0.,-1.,0.));
#66221=DIRECTION('ref_axis',(-1.,0.,0.));
#66222=DIRECTION('',(-1.,0.,0.));
#66223=DIRECTION('',(0.,0.,-1.));
#66224=DIRECTION('',(-1.,0.,0.));
#66225=DIRECTION('',(0.,0.,-1.));
#66226=DIRECTION('center_axis',(1.,0.,0.));
#66227=DIRECTION('ref_axis',(0.,-1.,0.));
#66228=DIRECTION('',(0.,-1.,0.));
#66229=DIRECTION('',(0.,0.,-1.));
#66230=DIRECTION('',(0.,-1.,0.));
#66231=DIRECTION('center_axis',(0.,1.,0.));
#66232=DIRECTION('ref_axis',(1.,0.,0.));
#66233=DIRECTION('',(1.,0.,0.));
#66234=DIRECTION('',(0.,0.,-1.));
#66235=DIRECTION('',(1.,0.,0.));
#66236=DIRECTION('center_axis',(-1.,0.,0.));
#66237=DIRECTION('ref_axis',(0.,1.,0.));
#66238=DIRECTION('',(0.,1.,0.));
#66239=DIRECTION('',(0.,1.,0.));
#66240=DIRECTION('center_axis',(0.,0.,-1.));
#66241=DIRECTION('ref_axis',(-1.,0.,0.));
#66242=DIRECTION('center_axis',(0.,-1.,0.));
#66243=DIRECTION('ref_axis',(-1.,0.,0.));
#66244=DIRECTION('',(-1.,0.,0.));
#66245=DIRECTION('',(0.,0.,-1.));
#66246=DIRECTION('',(-1.,0.,0.));
#66247=DIRECTION('',(0.,0.,-1.));
#66248=DIRECTION('center_axis',(1.,0.,0.));
#66249=DIRECTION('ref_axis',(0.,-1.,0.));
#66250=DIRECTION('',(0.,-1.,0.));
#66251=DIRECTION('',(0.,0.,-1.));
#66252=DIRECTION('',(0.,-1.,0.));
#66253=DIRECTION('center_axis',(0.,1.,0.));
#66254=DIRECTION('ref_axis',(1.,0.,0.));
#66255=DIRECTION('',(1.,0.,0.));
#66256=DIRECTION('',(0.,0.,-1.));
#66257=DIRECTION('',(1.,0.,0.));
#66258=DIRECTION('center_axis',(-1.,0.,0.));
#66259=DIRECTION('ref_axis',(0.,1.,0.));
#66260=DIRECTION('',(0.,1.,0.));
#66261=DIRECTION('',(0.,1.,0.));
#66262=DIRECTION('center_axis',(0.,0.,-1.));
#66263=DIRECTION('ref_axis',(-1.,0.,0.));
#66264=DIRECTION('center_axis',(0.,-1.,0.));
#66265=DIRECTION('ref_axis',(-1.,0.,0.));
#66266=DIRECTION('',(-1.,0.,0.));
#66267=DIRECTION('',(0.,0.,-1.));
#66268=DIRECTION('',(-1.,0.,0.));
#66269=DIRECTION('',(0.,0.,-1.));
#66270=DIRECTION('center_axis',(1.,0.,0.));
#66271=DIRECTION('ref_axis',(0.,-1.,0.));
#66272=DIRECTION('',(0.,-1.,0.));
#66273=DIRECTION('',(0.,0.,-1.));
#66274=DIRECTION('',(0.,-1.,0.));
#66275=DIRECTION('center_axis',(0.,1.,0.));
#66276=DIRECTION('ref_axis',(1.,0.,0.));
#66277=DIRECTION('',(1.,0.,0.));
#66278=DIRECTION('',(0.,0.,-1.));
#66279=DIRECTION('',(1.,0.,0.));
#66280=DIRECTION('center_axis',(-1.,0.,0.));
#66281=DIRECTION('ref_axis',(0.,1.,0.));
#66282=DIRECTION('',(0.,1.,0.));
#66283=DIRECTION('',(0.,1.,0.));
#66284=DIRECTION('center_axis',(0.,0.,-1.));
#66285=DIRECTION('ref_axis',(-1.,0.,0.));
#66286=DIRECTION('center_axis',(0.,-1.,0.));
#66287=DIRECTION('ref_axis',(-1.,0.,0.));
#66288=DIRECTION('',(-1.,0.,0.));
#66289=DIRECTION('',(0.,0.,-1.));
#66290=DIRECTION('',(-1.,0.,0.));
#66291=DIRECTION('',(0.,0.,-1.));
#66292=DIRECTION('center_axis',(1.,0.,0.));
#66293=DIRECTION('ref_axis',(0.,-1.,0.));
#66294=DIRECTION('',(0.,-1.,0.));
#66295=DIRECTION('',(0.,0.,-1.));
#66296=DIRECTION('',(0.,-1.,0.));
#66297=DIRECTION('center_axis',(0.,1.,0.));
#66298=DIRECTION('ref_axis',(1.,0.,0.));
#66299=DIRECTION('',(1.,0.,0.));
#66300=DIRECTION('',(0.,0.,-1.));
#66301=DIRECTION('',(1.,0.,0.));
#66302=DIRECTION('center_axis',(-1.,0.,0.));
#66303=DIRECTION('ref_axis',(0.,1.,0.));
#66304=DIRECTION('',(0.,1.,0.));
#66305=DIRECTION('',(0.,1.,0.));
#66306=DIRECTION('center_axis',(0.,0.,-1.));
#66307=DIRECTION('ref_axis',(-1.,0.,0.));
#66308=DIRECTION('center_axis',(0.,-1.,0.));
#66309=DIRECTION('ref_axis',(-1.,0.,0.));
#66310=DIRECTION('',(-1.,0.,0.));
#66311=DIRECTION('',(0.,0.,-1.));
#66312=DIRECTION('',(-1.,0.,0.));
#66313=DIRECTION('',(0.,0.,-1.));
#66314=DIRECTION('center_axis',(1.,0.,0.));
#66315=DIRECTION('ref_axis',(0.,-1.,0.));
#66316=DIRECTION('',(0.,-1.,0.));
#66317=DIRECTION('',(0.,0.,-1.));
#66318=DIRECTION('',(0.,-1.,0.));
#66319=DIRECTION('center_axis',(0.,1.,0.));
#66320=DIRECTION('ref_axis',(1.,0.,0.));
#66321=DIRECTION('',(1.,0.,0.));
#66322=DIRECTION('',(0.,0.,-1.));
#66323=DIRECTION('',(1.,0.,0.));
#66324=DIRECTION('center_axis',(-1.,0.,0.));
#66325=DIRECTION('ref_axis',(0.,1.,0.));
#66326=DIRECTION('',(0.,1.,0.));
#66327=DIRECTION('',(0.,1.,0.));
#66328=DIRECTION('center_axis',(0.,0.,-1.));
#66329=DIRECTION('ref_axis',(-1.,0.,0.));
#66330=DIRECTION('center_axis',(0.,-1.,0.));
#66331=DIRECTION('ref_axis',(-1.,0.,0.));
#66332=DIRECTION('',(-1.,0.,0.));
#66333=DIRECTION('',(0.,0.,-1.));
#66334=DIRECTION('',(-1.,0.,0.));
#66335=DIRECTION('',(0.,0.,-1.));
#66336=DIRECTION('center_axis',(1.,0.,0.));
#66337=DIRECTION('ref_axis',(0.,-1.,0.));
#66338=DIRECTION('',(0.,-1.,0.));
#66339=DIRECTION('',(0.,0.,-1.));
#66340=DIRECTION('',(0.,-1.,0.));
#66341=DIRECTION('center_axis',(0.,1.,0.));
#66342=DIRECTION('ref_axis',(1.,0.,0.));
#66343=DIRECTION('',(1.,0.,0.));
#66344=DIRECTION('',(0.,0.,-1.));
#66345=DIRECTION('',(1.,0.,0.));
#66346=DIRECTION('center_axis',(-1.,0.,0.));
#66347=DIRECTION('ref_axis',(0.,1.,0.));
#66348=DIRECTION('',(0.,1.,0.));
#66349=DIRECTION('',(0.,1.,0.));
#66350=DIRECTION('center_axis',(0.,0.,-1.));
#66351=DIRECTION('ref_axis',(-1.,0.,0.));
#66352=DIRECTION('center_axis',(0.,-1.,0.));
#66353=DIRECTION('ref_axis',(-1.,0.,0.));
#66354=DIRECTION('',(-1.,0.,0.));
#66355=DIRECTION('',(0.,0.,-1.));
#66356=DIRECTION('',(-1.,0.,0.));
#66357=DIRECTION('',(0.,0.,-1.));
#66358=DIRECTION('center_axis',(1.,0.,0.));
#66359=DIRECTION('ref_axis',(0.,-1.,0.));
#66360=DIRECTION('',(0.,-1.,0.));
#66361=DIRECTION('',(0.,0.,-1.));
#66362=DIRECTION('',(0.,-1.,0.));
#66363=DIRECTION('center_axis',(0.,1.,0.));
#66364=DIRECTION('ref_axis',(1.,0.,0.));
#66365=DIRECTION('',(1.,0.,0.));
#66366=DIRECTION('',(0.,0.,-1.));
#66367=DIRECTION('',(1.,0.,0.));
#66368=DIRECTION('center_axis',(-1.,0.,0.));
#66369=DIRECTION('ref_axis',(0.,1.,0.));
#66370=DIRECTION('',(0.,1.,0.));
#66371=DIRECTION('',(0.,1.,0.));
#66372=DIRECTION('center_axis',(0.,0.,-1.));
#66373=DIRECTION('ref_axis',(-1.,0.,0.));
#66374=DIRECTION('center_axis',(0.,-1.,0.));
#66375=DIRECTION('ref_axis',(-1.,0.,0.));
#66376=DIRECTION('',(-1.,0.,0.));
#66377=DIRECTION('',(0.,0.,-1.));
#66378=DIRECTION('',(-1.,0.,0.));
#66379=DIRECTION('',(0.,0.,-1.));
#66380=DIRECTION('center_axis',(1.,0.,0.));
#66381=DIRECTION('ref_axis',(0.,-1.,0.));
#66382=DIRECTION('',(0.,-1.,0.));
#66383=DIRECTION('',(0.,0.,-1.));
#66384=DIRECTION('',(0.,-1.,0.));
#66385=DIRECTION('center_axis',(0.,1.,0.));
#66386=DIRECTION('ref_axis',(1.,0.,0.));
#66387=DIRECTION('',(1.,0.,0.));
#66388=DIRECTION('',(0.,0.,-1.));
#66389=DIRECTION('',(1.,0.,0.));
#66390=DIRECTION('center_axis',(-1.,0.,0.));
#66391=DIRECTION('ref_axis',(0.,1.,0.));
#66392=DIRECTION('',(0.,1.,0.));
#66393=DIRECTION('',(0.,1.,0.));
#66394=DIRECTION('center_axis',(0.,0.,-1.));
#66395=DIRECTION('ref_axis',(-1.,0.,0.));
#66396=DIRECTION('center_axis',(0.,-1.,0.));
#66397=DIRECTION('ref_axis',(-1.,0.,0.));
#66398=DIRECTION('',(-1.,0.,0.));
#66399=DIRECTION('',(0.,0.,-1.));
#66400=DIRECTION('',(-1.,0.,0.));
#66401=DIRECTION('',(0.,0.,-1.));
#66402=DIRECTION('center_axis',(1.,0.,0.));
#66403=DIRECTION('ref_axis',(0.,-1.,0.));
#66404=DIRECTION('',(0.,-1.,0.));
#66405=DIRECTION('',(0.,0.,-1.));
#66406=DIRECTION('',(0.,-1.,0.));
#66407=DIRECTION('center_axis',(0.,1.,0.));
#66408=DIRECTION('ref_axis',(1.,0.,0.));
#66409=DIRECTION('',(1.,0.,0.));
#66410=DIRECTION('',(0.,0.,-1.));
#66411=DIRECTION('',(1.,0.,0.));
#66412=DIRECTION('center_axis',(-1.,0.,0.));
#66413=DIRECTION('ref_axis',(0.,1.,0.));
#66414=DIRECTION('',(0.,1.,0.));
#66415=DIRECTION('',(0.,1.,0.));
#66416=DIRECTION('center_axis',(0.,0.,-1.));
#66417=DIRECTION('ref_axis',(-1.,0.,0.));
#66418=DIRECTION('center_axis',(0.,-1.,0.));
#66419=DIRECTION('ref_axis',(-1.,0.,0.));
#66420=DIRECTION('',(-1.,0.,0.));
#66421=DIRECTION('',(0.,0.,-1.));
#66422=DIRECTION('',(-1.,0.,0.));
#66423=DIRECTION('',(0.,0.,-1.));
#66424=DIRECTION('center_axis',(1.,0.,0.));
#66425=DIRECTION('ref_axis',(0.,-1.,0.));
#66426=DIRECTION('',(0.,-1.,0.));
#66427=DIRECTION('',(0.,0.,-1.));
#66428=DIRECTION('',(0.,-1.,0.));
#66429=DIRECTION('center_axis',(0.,1.,0.));
#66430=DIRECTION('ref_axis',(1.,0.,0.));
#66431=DIRECTION('',(1.,0.,0.));
#66432=DIRECTION('',(0.,0.,-1.));
#66433=DIRECTION('',(1.,0.,0.));
#66434=DIRECTION('center_axis',(-1.,0.,0.));
#66435=DIRECTION('ref_axis',(0.,1.,0.));
#66436=DIRECTION('',(0.,1.,0.));
#66437=DIRECTION('',(0.,1.,0.));
#66438=DIRECTION('center_axis',(0.,0.,-1.));
#66439=DIRECTION('ref_axis',(-1.,0.,0.));
#66440=DIRECTION('center_axis',(0.,-1.,0.));
#66441=DIRECTION('ref_axis',(-1.,0.,0.));
#66442=DIRECTION('',(-1.,0.,0.));
#66443=DIRECTION('',(0.,0.,-1.));
#66444=DIRECTION('',(-1.,0.,0.));
#66445=DIRECTION('',(0.,0.,-1.));
#66446=DIRECTION('center_axis',(1.,0.,0.));
#66447=DIRECTION('ref_axis',(0.,-1.,0.));
#66448=DIRECTION('',(0.,-1.,0.));
#66449=DIRECTION('',(0.,0.,-1.));
#66450=DIRECTION('',(0.,-1.,0.));
#66451=DIRECTION('center_axis',(0.,1.,0.));
#66452=DIRECTION('ref_axis',(1.,0.,0.));
#66453=DIRECTION('',(1.,0.,0.));
#66454=DIRECTION('',(0.,0.,-1.));
#66455=DIRECTION('',(1.,0.,0.));
#66456=DIRECTION('center_axis',(-1.,0.,0.));
#66457=DIRECTION('ref_axis',(0.,1.,0.));
#66458=DIRECTION('',(0.,1.,0.));
#66459=DIRECTION('',(0.,1.,0.));
#66460=DIRECTION('center_axis',(0.,0.,-1.));
#66461=DIRECTION('ref_axis',(-1.,0.,0.));
#66462=DIRECTION('center_axis',(0.,-1.,0.));
#66463=DIRECTION('ref_axis',(-1.,0.,0.));
#66464=DIRECTION('',(-1.,0.,0.));
#66465=DIRECTION('',(0.,0.,-1.));
#66466=DIRECTION('',(-1.,0.,0.));
#66467=DIRECTION('',(0.,0.,-1.));
#66468=DIRECTION('center_axis',(1.,0.,0.));
#66469=DIRECTION('ref_axis',(0.,-1.,0.));
#66470=DIRECTION('',(0.,-1.,0.));
#66471=DIRECTION('',(0.,0.,-1.));
#66472=DIRECTION('',(0.,-1.,0.));
#66473=DIRECTION('center_axis',(0.,1.,0.));
#66474=DIRECTION('ref_axis',(1.,0.,0.));
#66475=DIRECTION('',(1.,0.,0.));
#66476=DIRECTION('',(0.,0.,-1.));
#66477=DIRECTION('',(1.,0.,0.));
#66478=DIRECTION('center_axis',(-1.,0.,0.));
#66479=DIRECTION('ref_axis',(0.,1.,0.));
#66480=DIRECTION('',(0.,1.,0.));
#66481=DIRECTION('',(0.,1.,0.));
#66482=DIRECTION('center_axis',(0.,0.,-1.));
#66483=DIRECTION('ref_axis',(-1.,0.,0.));
#66484=DIRECTION('center_axis',(0.,-1.,0.));
#66485=DIRECTION('ref_axis',(-1.,0.,0.));
#66486=DIRECTION('',(-1.,0.,0.));
#66487=DIRECTION('',(0.,0.,-1.));
#66488=DIRECTION('',(-1.,0.,0.));
#66489=DIRECTION('',(0.,0.,-1.));
#66490=DIRECTION('center_axis',(1.,0.,0.));
#66491=DIRECTION('ref_axis',(0.,-1.,0.));
#66492=DIRECTION('',(0.,-1.,0.));
#66493=DIRECTION('',(0.,0.,-1.));
#66494=DIRECTION('',(0.,-1.,0.));
#66495=DIRECTION('center_axis',(0.,1.,0.));
#66496=DIRECTION('ref_axis',(1.,0.,0.));
#66497=DIRECTION('',(1.,0.,0.));
#66498=DIRECTION('',(0.,0.,-1.));
#66499=DIRECTION('',(1.,0.,0.));
#66500=DIRECTION('center_axis',(-1.,0.,0.));
#66501=DIRECTION('ref_axis',(0.,1.,0.));
#66502=DIRECTION('',(0.,1.,0.));
#66503=DIRECTION('',(0.,1.,0.));
#66504=DIRECTION('center_axis',(0.,0.,-1.));
#66505=DIRECTION('ref_axis',(-1.,0.,0.));
#66506=DIRECTION('center_axis',(0.,-1.,0.));
#66507=DIRECTION('ref_axis',(-1.,0.,0.));
#66508=DIRECTION('',(-1.,0.,0.));
#66509=DIRECTION('',(0.,0.,-1.));
#66510=DIRECTION('',(-1.,0.,0.));
#66511=DIRECTION('',(0.,0.,-1.));
#66512=DIRECTION('center_axis',(1.,0.,0.));
#66513=DIRECTION('ref_axis',(0.,-1.,0.));
#66514=DIRECTION('',(0.,-1.,0.));
#66515=DIRECTION('',(0.,0.,-1.));
#66516=DIRECTION('',(0.,-1.,0.));
#66517=DIRECTION('center_axis',(0.,1.,0.));
#66518=DIRECTION('ref_axis',(1.,0.,0.));
#66519=DIRECTION('',(1.,0.,0.));
#66520=DIRECTION('',(0.,0.,-1.));
#66521=DIRECTION('',(1.,0.,0.));
#66522=DIRECTION('center_axis',(-1.,0.,0.));
#66523=DIRECTION('ref_axis',(0.,1.,0.));
#66524=DIRECTION('',(0.,1.,0.));
#66525=DIRECTION('',(0.,1.,0.));
#66526=DIRECTION('center_axis',(0.,0.,-1.));
#66527=DIRECTION('ref_axis',(-1.,0.,0.));
#66528=DIRECTION('center_axis',(0.,-1.,0.));
#66529=DIRECTION('ref_axis',(-1.,0.,0.));
#66530=DIRECTION('',(-1.,0.,0.));
#66531=DIRECTION('',(0.,0.,-1.));
#66532=DIRECTION('',(-1.,0.,0.));
#66533=DIRECTION('',(0.,0.,-1.));
#66534=DIRECTION('center_axis',(1.,0.,0.));
#66535=DIRECTION('ref_axis',(0.,-1.,0.));
#66536=DIRECTION('',(0.,-1.,0.));
#66537=DIRECTION('',(0.,0.,-1.));
#66538=DIRECTION('',(0.,-1.,0.));
#66539=DIRECTION('center_axis',(0.,1.,0.));
#66540=DIRECTION('ref_axis',(1.,0.,0.));
#66541=DIRECTION('',(1.,0.,0.));
#66542=DIRECTION('',(0.,0.,-1.));
#66543=DIRECTION('',(1.,0.,0.));
#66544=DIRECTION('center_axis',(-1.,0.,0.));
#66545=DIRECTION('ref_axis',(0.,1.,0.));
#66546=DIRECTION('',(0.,1.,0.));
#66547=DIRECTION('',(0.,1.,0.));
#66548=DIRECTION('center_axis',(0.,0.,-1.));
#66549=DIRECTION('ref_axis',(-1.,0.,0.));
#66550=DIRECTION('center_axis',(0.,-1.,0.));
#66551=DIRECTION('ref_axis',(-1.,0.,0.));
#66552=DIRECTION('',(-1.,0.,0.));
#66553=DIRECTION('',(0.,0.,-1.));
#66554=DIRECTION('',(-1.,0.,0.));
#66555=DIRECTION('',(0.,0.,-1.));
#66556=DIRECTION('center_axis',(1.,0.,0.));
#66557=DIRECTION('ref_axis',(0.,-1.,0.));
#66558=DIRECTION('',(0.,-1.,0.));
#66559=DIRECTION('',(0.,0.,-1.));
#66560=DIRECTION('',(0.,-1.,0.));
#66561=DIRECTION('center_axis',(0.,1.,0.));
#66562=DIRECTION('ref_axis',(1.,0.,0.));
#66563=DIRECTION('',(1.,0.,0.));
#66564=DIRECTION('',(0.,0.,-1.));
#66565=DIRECTION('',(1.,0.,0.));
#66566=DIRECTION('center_axis',(-1.,0.,0.));
#66567=DIRECTION('ref_axis',(0.,1.,0.));
#66568=DIRECTION('',(0.,1.,0.));
#66569=DIRECTION('',(0.,1.,0.));
#66570=DIRECTION('center_axis',(0.,0.,-1.));
#66571=DIRECTION('ref_axis',(-1.,0.,0.));
#66572=DIRECTION('center_axis',(0.,-1.,0.));
#66573=DIRECTION('ref_axis',(-1.,0.,0.));
#66574=DIRECTION('',(-1.,0.,0.));
#66575=DIRECTION('',(0.,0.,-1.));
#66576=DIRECTION('',(-1.,0.,0.));
#66577=DIRECTION('',(0.,0.,-1.));
#66578=DIRECTION('center_axis',(1.,0.,0.));
#66579=DIRECTION('ref_axis',(0.,-1.,0.));
#66580=DIRECTION('',(0.,-1.,0.));
#66581=DIRECTION('',(0.,0.,-1.));
#66582=DIRECTION('',(0.,-1.,0.));
#66583=DIRECTION('center_axis',(0.,1.,0.));
#66584=DIRECTION('ref_axis',(1.,0.,0.));
#66585=DIRECTION('',(1.,0.,0.));
#66586=DIRECTION('',(0.,0.,-1.));
#66587=DIRECTION('',(1.,0.,0.));
#66588=DIRECTION('center_axis',(-1.,0.,0.));
#66589=DIRECTION('ref_axis',(0.,1.,0.));
#66590=DIRECTION('',(0.,1.,0.));
#66591=DIRECTION('',(0.,1.,0.));
#66592=DIRECTION('center_axis',(0.,0.,-1.));
#66593=DIRECTION('ref_axis',(-1.,0.,0.));
#66594=DIRECTION('center_axis',(0.,-1.,0.));
#66595=DIRECTION('ref_axis',(-1.,0.,0.));
#66596=DIRECTION('',(-1.,0.,0.));
#66597=DIRECTION('',(0.,0.,-1.));
#66598=DIRECTION('',(-1.,0.,0.));
#66599=DIRECTION('',(0.,0.,-1.));
#66600=DIRECTION('center_axis',(1.,0.,0.));
#66601=DIRECTION('ref_axis',(0.,-1.,0.));
#66602=DIRECTION('',(0.,-1.,0.));
#66603=DIRECTION('',(0.,0.,-1.));
#66604=DIRECTION('',(0.,-1.,0.));
#66605=DIRECTION('center_axis',(0.,1.,0.));
#66606=DIRECTION('ref_axis',(1.,0.,0.));
#66607=DIRECTION('',(1.,0.,0.));
#66608=DIRECTION('',(0.,0.,-1.));
#66609=DIRECTION('',(1.,0.,0.));
#66610=DIRECTION('center_axis',(-1.,0.,0.));
#66611=DIRECTION('ref_axis',(0.,1.,0.));
#66612=DIRECTION('',(0.,1.,0.));
#66613=DIRECTION('',(0.,1.,0.));
#66614=DIRECTION('center_axis',(0.,0.,-1.));
#66615=DIRECTION('ref_axis',(-1.,0.,0.));
#66616=DIRECTION('center_axis',(0.,-1.,0.));
#66617=DIRECTION('ref_axis',(-1.,0.,0.));
#66618=DIRECTION('',(-1.,0.,0.));
#66619=DIRECTION('',(0.,0.,-1.));
#66620=DIRECTION('',(-1.,0.,0.));
#66621=DIRECTION('',(0.,0.,-1.));
#66622=DIRECTION('center_axis',(1.,0.,0.));
#66623=DIRECTION('ref_axis',(0.,-1.,0.));
#66624=DIRECTION('',(0.,-1.,0.));
#66625=DIRECTION('',(0.,0.,-1.));
#66626=DIRECTION('',(0.,-1.,0.));
#66627=DIRECTION('center_axis',(0.,1.,0.));
#66628=DIRECTION('ref_axis',(1.,0.,0.));
#66629=DIRECTION('',(1.,0.,0.));
#66630=DIRECTION('',(0.,0.,-1.));
#66631=DIRECTION('',(1.,0.,0.));
#66632=DIRECTION('center_axis',(-1.,0.,0.));
#66633=DIRECTION('ref_axis',(0.,1.,0.));
#66634=DIRECTION('',(0.,1.,0.));
#66635=DIRECTION('',(0.,1.,0.));
#66636=DIRECTION('center_axis',(0.,0.,-1.));
#66637=DIRECTION('ref_axis',(-1.,0.,0.));
#66638=DIRECTION('center_axis',(0.,-1.,0.));
#66639=DIRECTION('ref_axis',(-1.,0.,0.));
#66640=DIRECTION('',(-1.,0.,0.));
#66641=DIRECTION('',(0.,0.,-1.));
#66642=DIRECTION('',(-1.,0.,0.));
#66643=DIRECTION('',(0.,0.,-1.));
#66644=DIRECTION('center_axis',(1.,0.,0.));
#66645=DIRECTION('ref_axis',(0.,-1.,0.));
#66646=DIRECTION('',(0.,-1.,0.));
#66647=DIRECTION('',(0.,0.,-1.));
#66648=DIRECTION('',(0.,-1.,0.));
#66649=DIRECTION('center_axis',(0.,1.,0.));
#66650=DIRECTION('ref_axis',(1.,0.,0.));
#66651=DIRECTION('',(1.,0.,0.));
#66652=DIRECTION('',(0.,0.,-1.));
#66653=DIRECTION('',(1.,0.,0.));
#66654=DIRECTION('center_axis',(-1.,0.,0.));
#66655=DIRECTION('ref_axis',(0.,1.,0.));
#66656=DIRECTION('',(0.,1.,0.));
#66657=DIRECTION('',(0.,1.,0.));
#66658=DIRECTION('center_axis',(0.,0.,-1.));
#66659=DIRECTION('ref_axis',(-1.,0.,0.));
#66660=DIRECTION('center_axis',(0.,-1.,0.));
#66661=DIRECTION('ref_axis',(-1.,0.,0.));
#66662=DIRECTION('',(-1.,0.,0.));
#66663=DIRECTION('',(0.,0.,-1.));
#66664=DIRECTION('',(-1.,0.,0.));
#66665=DIRECTION('',(0.,0.,-1.));
#66666=DIRECTION('center_axis',(1.,0.,0.));
#66667=DIRECTION('ref_axis',(0.,-1.,0.));
#66668=DIRECTION('',(0.,-1.,0.));
#66669=DIRECTION('',(0.,0.,-1.));
#66670=DIRECTION('',(0.,-1.,0.));
#66671=DIRECTION('center_axis',(0.,1.,0.));
#66672=DIRECTION('ref_axis',(1.,0.,0.));
#66673=DIRECTION('',(1.,0.,0.));
#66674=DIRECTION('',(0.,0.,-1.));
#66675=DIRECTION('',(1.,0.,0.));
#66676=DIRECTION('center_axis',(-1.,0.,0.));
#66677=DIRECTION('ref_axis',(0.,1.,0.));
#66678=DIRECTION('',(0.,1.,0.));
#66679=DIRECTION('',(0.,1.,0.));
#66680=DIRECTION('center_axis',(0.,0.,-1.));
#66681=DIRECTION('ref_axis',(-1.,0.,0.));
#66682=DIRECTION('center_axis',(0.,-1.,0.));
#66683=DIRECTION('ref_axis',(-1.,0.,0.));
#66684=DIRECTION('',(-1.,0.,0.));
#66685=DIRECTION('',(0.,0.,-1.));
#66686=DIRECTION('',(-1.,0.,0.));
#66687=DIRECTION('',(0.,0.,-1.));
#66688=DIRECTION('center_axis',(1.,0.,0.));
#66689=DIRECTION('ref_axis',(0.,-1.,0.));
#66690=DIRECTION('',(0.,-1.,0.));
#66691=DIRECTION('',(0.,0.,-1.));
#66692=DIRECTION('',(0.,-1.,0.));
#66693=DIRECTION('center_axis',(0.,1.,0.));
#66694=DIRECTION('ref_axis',(1.,0.,0.));
#66695=DIRECTION('',(1.,0.,0.));
#66696=DIRECTION('',(0.,0.,-1.));
#66697=DIRECTION('',(1.,0.,0.));
#66698=DIRECTION('center_axis',(-1.,0.,0.));
#66699=DIRECTION('ref_axis',(0.,1.,0.));
#66700=DIRECTION('',(0.,1.,0.));
#66701=DIRECTION('',(0.,1.,0.));
#66702=DIRECTION('center_axis',(0.,0.,-1.));
#66703=DIRECTION('ref_axis',(-1.,0.,0.));
#66704=DIRECTION('center_axis',(0.,-1.,0.));
#66705=DIRECTION('ref_axis',(-1.,0.,0.));
#66706=DIRECTION('',(-1.,0.,0.));
#66707=DIRECTION('',(0.,0.,-1.));
#66708=DIRECTION('',(-1.,0.,0.));
#66709=DIRECTION('',(0.,0.,-1.));
#66710=DIRECTION('center_axis',(1.,0.,0.));
#66711=DIRECTION('ref_axis',(0.,-1.,0.));
#66712=DIRECTION('',(0.,-1.,0.));
#66713=DIRECTION('',(0.,0.,-1.));
#66714=DIRECTION('',(0.,-1.,0.));
#66715=DIRECTION('center_axis',(0.,1.,0.));
#66716=DIRECTION('ref_axis',(1.,0.,0.));
#66717=DIRECTION('',(1.,0.,0.));
#66718=DIRECTION('',(0.,0.,-1.));
#66719=DIRECTION('',(1.,0.,0.));
#66720=DIRECTION('center_axis',(-1.,0.,0.));
#66721=DIRECTION('ref_axis',(0.,1.,0.));
#66722=DIRECTION('',(0.,1.,0.));
#66723=DIRECTION('',(0.,1.,0.));
#66724=DIRECTION('center_axis',(0.,0.,-1.));
#66725=DIRECTION('ref_axis',(-1.,0.,0.));
#66726=DIRECTION('center_axis',(0.,-1.,0.));
#66727=DIRECTION('ref_axis',(-1.,0.,0.));
#66728=DIRECTION('',(-1.,0.,0.));
#66729=DIRECTION('',(0.,0.,-1.));
#66730=DIRECTION('',(-1.,0.,0.));
#66731=DIRECTION('',(0.,0.,-1.));
#66732=DIRECTION('center_axis',(1.,0.,0.));
#66733=DIRECTION('ref_axis',(0.,-1.,0.));
#66734=DIRECTION('',(0.,-1.,0.));
#66735=DIRECTION('',(0.,0.,-1.));
#66736=DIRECTION('',(0.,-1.,0.));
#66737=DIRECTION('center_axis',(0.,1.,0.));
#66738=DIRECTION('ref_axis',(1.,0.,0.));
#66739=DIRECTION('',(1.,0.,0.));
#66740=DIRECTION('',(0.,0.,-1.));
#66741=DIRECTION('',(1.,0.,0.));
#66742=DIRECTION('center_axis',(-1.,0.,0.));
#66743=DIRECTION('ref_axis',(0.,1.,0.));
#66744=DIRECTION('',(0.,1.,0.));
#66745=DIRECTION('',(0.,1.,0.));
#66746=DIRECTION('center_axis',(0.,0.,-1.));
#66747=DIRECTION('ref_axis',(-1.,0.,0.));
#66748=DIRECTION('center_axis',(0.,-1.,0.));
#66749=DIRECTION('ref_axis',(-1.,0.,0.));
#66750=DIRECTION('',(-1.,0.,0.));
#66751=DIRECTION('',(0.,0.,-1.));
#66752=DIRECTION('',(-1.,0.,0.));
#66753=DIRECTION('',(0.,0.,-1.));
#66754=DIRECTION('center_axis',(1.,0.,0.));
#66755=DIRECTION('ref_axis',(0.,-1.,0.));
#66756=DIRECTION('',(0.,-1.,0.));
#66757=DIRECTION('',(0.,0.,-1.));
#66758=DIRECTION('',(0.,-1.,0.));
#66759=DIRECTION('center_axis',(0.,1.,0.));
#66760=DIRECTION('ref_axis',(1.,0.,0.));
#66761=DIRECTION('',(1.,0.,0.));
#66762=DIRECTION('',(0.,0.,-1.));
#66763=DIRECTION('',(1.,0.,0.));
#66764=DIRECTION('center_axis',(-1.,0.,0.));
#66765=DIRECTION('ref_axis',(0.,1.,0.));
#66766=DIRECTION('',(0.,1.,0.));
#66767=DIRECTION('',(0.,1.,0.));
#66768=DIRECTION('center_axis',(0.,0.,-1.));
#66769=DIRECTION('ref_axis',(-1.,0.,0.));
#66770=DIRECTION('center_axis',(0.,-1.,0.));
#66771=DIRECTION('ref_axis',(-1.,0.,0.));
#66772=DIRECTION('',(-1.,0.,0.));
#66773=DIRECTION('',(0.,0.,-1.));
#66774=DIRECTION('',(-1.,0.,0.));
#66775=DIRECTION('',(0.,0.,-1.));
#66776=DIRECTION('center_axis',(1.,0.,0.));
#66777=DIRECTION('ref_axis',(0.,-1.,0.));
#66778=DIRECTION('',(0.,-1.,0.));
#66779=DIRECTION('',(0.,0.,-1.));
#66780=DIRECTION('',(0.,-1.,0.));
#66781=DIRECTION('center_axis',(0.,1.,0.));
#66782=DIRECTION('ref_axis',(1.,0.,0.));
#66783=DIRECTION('',(1.,0.,0.));
#66784=DIRECTION('',(0.,0.,-1.));
#66785=DIRECTION('',(1.,0.,0.));
#66786=DIRECTION('center_axis',(-1.,0.,0.));
#66787=DIRECTION('ref_axis',(0.,1.,0.));
#66788=DIRECTION('',(0.,1.,0.));
#66789=DIRECTION('',(0.,1.,0.));
#66790=DIRECTION('center_axis',(0.,0.,-1.));
#66791=DIRECTION('ref_axis',(-1.,0.,0.));
#66792=DIRECTION('center_axis',(0.,-1.,0.));
#66793=DIRECTION('ref_axis',(-1.,0.,0.));
#66794=DIRECTION('',(-1.,0.,0.));
#66795=DIRECTION('',(0.,0.,-1.));
#66796=DIRECTION('',(-1.,0.,0.));
#66797=DIRECTION('',(0.,0.,-1.));
#66798=DIRECTION('center_axis',(1.,0.,0.));
#66799=DIRECTION('ref_axis',(0.,-1.,0.));
#66800=DIRECTION('',(0.,-1.,0.));
#66801=DIRECTION('',(0.,0.,-1.));
#66802=DIRECTION('',(0.,-1.,0.));
#66803=DIRECTION('center_axis',(0.,1.,0.));
#66804=DIRECTION('ref_axis',(1.,0.,0.));
#66805=DIRECTION('',(1.,0.,0.));
#66806=DIRECTION('',(0.,0.,-1.));
#66807=DIRECTION('',(1.,0.,0.));
#66808=DIRECTION('center_axis',(-1.,0.,0.));
#66809=DIRECTION('ref_axis',(0.,1.,0.));
#66810=DIRECTION('',(0.,1.,0.));
#66811=DIRECTION('',(0.,1.,0.));
#66812=DIRECTION('center_axis',(0.,0.,-1.));
#66813=DIRECTION('ref_axis',(-1.,0.,0.));
#66814=DIRECTION('center_axis',(0.,-1.,0.));
#66815=DIRECTION('ref_axis',(-1.,0.,0.));
#66816=DIRECTION('',(-1.,0.,0.));
#66817=DIRECTION('',(0.,0.,-1.));
#66818=DIRECTION('',(-1.,0.,0.));
#66819=DIRECTION('',(0.,0.,-1.));
#66820=DIRECTION('center_axis',(1.,0.,0.));
#66821=DIRECTION('ref_axis',(0.,-1.,0.));
#66822=DIRECTION('',(0.,-1.,0.));
#66823=DIRECTION('',(0.,0.,-1.));
#66824=DIRECTION('',(0.,-1.,0.));
#66825=DIRECTION('center_axis',(0.,1.,0.));
#66826=DIRECTION('ref_axis',(1.,0.,0.));
#66827=DIRECTION('',(1.,0.,0.));
#66828=DIRECTION('',(0.,0.,-1.));
#66829=DIRECTION('',(1.,0.,0.));
#66830=DIRECTION('center_axis',(-1.,0.,0.));
#66831=DIRECTION('ref_axis',(0.,1.,0.));
#66832=DIRECTION('',(0.,1.,0.));
#66833=DIRECTION('',(0.,1.,0.));
#66834=DIRECTION('center_axis',(0.,0.,-1.));
#66835=DIRECTION('ref_axis',(-1.,0.,0.));
#66836=DIRECTION('center_axis',(0.,-1.,0.));
#66837=DIRECTION('ref_axis',(-1.,0.,0.));
#66838=DIRECTION('',(-1.,0.,0.));
#66839=DIRECTION('',(0.,0.,-1.));
#66840=DIRECTION('',(-1.,0.,0.));
#66841=DIRECTION('',(0.,0.,-1.));
#66842=DIRECTION('center_axis',(1.,0.,0.));
#66843=DIRECTION('ref_axis',(0.,-1.,0.));
#66844=DIRECTION('',(0.,-1.,0.));
#66845=DIRECTION('',(0.,0.,-1.));
#66846=DIRECTION('',(0.,-1.,0.));
#66847=DIRECTION('center_axis',(0.,1.,0.));
#66848=DIRECTION('ref_axis',(1.,0.,0.));
#66849=DIRECTION('',(1.,0.,0.));
#66850=DIRECTION('',(0.,0.,-1.));
#66851=DIRECTION('',(1.,0.,0.));
#66852=DIRECTION('center_axis',(-1.,0.,0.));
#66853=DIRECTION('ref_axis',(0.,1.,0.));
#66854=DIRECTION('',(0.,1.,0.));
#66855=DIRECTION('',(0.,1.,0.));
#66856=DIRECTION('center_axis',(0.,0.,-1.));
#66857=DIRECTION('ref_axis',(-1.,0.,0.));
#66858=DIRECTION('center_axis',(0.,-1.,0.));
#66859=DIRECTION('ref_axis',(-1.,0.,0.));
#66860=DIRECTION('',(-1.,0.,0.));
#66861=DIRECTION('',(0.,0.,-1.));
#66862=DIRECTION('',(-1.,0.,0.));
#66863=DIRECTION('',(0.,0.,-1.));
#66864=DIRECTION('center_axis',(1.,0.,0.));
#66865=DIRECTION('ref_axis',(0.,-1.,0.));
#66866=DIRECTION('',(0.,-1.,0.));
#66867=DIRECTION('',(0.,0.,-1.));
#66868=DIRECTION('',(0.,-1.,0.));
#66869=DIRECTION('center_axis',(0.,1.,0.));
#66870=DIRECTION('ref_axis',(1.,0.,0.));
#66871=DIRECTION('',(1.,0.,0.));
#66872=DIRECTION('',(0.,0.,-1.));
#66873=DIRECTION('',(1.,0.,0.));
#66874=DIRECTION('center_axis',(-1.,0.,0.));
#66875=DIRECTION('ref_axis',(0.,1.,0.));
#66876=DIRECTION('',(0.,1.,0.));
#66877=DIRECTION('',(0.,1.,0.));
#66878=DIRECTION('center_axis',(0.,0.,-1.));
#66879=DIRECTION('ref_axis',(-1.,0.,0.));
#66880=DIRECTION('center_axis',(0.,-1.,0.));
#66881=DIRECTION('ref_axis',(-1.,0.,0.));
#66882=DIRECTION('',(-1.,0.,0.));
#66883=DIRECTION('',(0.,0.,-1.));
#66884=DIRECTION('',(-1.,0.,0.));
#66885=DIRECTION('',(0.,0.,-1.));
#66886=DIRECTION('center_axis',(1.,0.,0.));
#66887=DIRECTION('ref_axis',(0.,-1.,0.));
#66888=DIRECTION('',(0.,-1.,0.));
#66889=DIRECTION('',(0.,0.,-1.));
#66890=DIRECTION('',(0.,-1.,0.));
#66891=DIRECTION('center_axis',(0.,1.,0.));
#66892=DIRECTION('ref_axis',(1.,0.,0.));
#66893=DIRECTION('',(1.,0.,0.));
#66894=DIRECTION('',(0.,0.,-1.));
#66895=DIRECTION('',(1.,0.,0.));
#66896=DIRECTION('center_axis',(-1.,0.,0.));
#66897=DIRECTION('ref_axis',(0.,1.,0.));
#66898=DIRECTION('',(0.,1.,0.));
#66899=DIRECTION('',(0.,1.,0.));
#66900=DIRECTION('center_axis',(0.,0.,-1.));
#66901=DIRECTION('ref_axis',(-1.,0.,0.));
#66902=DIRECTION('center_axis',(0.,-1.,0.));
#66903=DIRECTION('ref_axis',(-1.,0.,0.));
#66904=DIRECTION('',(-1.,0.,0.));
#66905=DIRECTION('',(0.,0.,-1.));
#66906=DIRECTION('',(-1.,0.,0.));
#66907=DIRECTION('',(0.,0.,-1.));
#66908=DIRECTION('center_axis',(1.,0.,0.));
#66909=DIRECTION('ref_axis',(0.,-1.,0.));
#66910=DIRECTION('',(0.,-1.,0.));
#66911=DIRECTION('',(0.,0.,-1.));
#66912=DIRECTION('',(0.,-1.,0.));
#66913=DIRECTION('center_axis',(0.,1.,0.));
#66914=DIRECTION('ref_axis',(1.,0.,0.));
#66915=DIRECTION('',(1.,0.,0.));
#66916=DIRECTION('',(0.,0.,-1.));
#66917=DIRECTION('',(1.,0.,0.));
#66918=DIRECTION('center_axis',(-1.,0.,0.));
#66919=DIRECTION('ref_axis',(0.,1.,0.));
#66920=DIRECTION('',(0.,1.,0.));
#66921=DIRECTION('',(0.,1.,0.));
#66922=DIRECTION('center_axis',(0.,0.,-1.));
#66923=DIRECTION('ref_axis',(-1.,0.,0.));
#66924=DIRECTION('center_axis',(0.,-1.,0.));
#66925=DIRECTION('ref_axis',(-1.,0.,0.));
#66926=DIRECTION('',(-1.,0.,0.));
#66927=DIRECTION('',(0.,0.,-1.));
#66928=DIRECTION('',(-1.,0.,0.));
#66929=DIRECTION('',(0.,0.,-1.));
#66930=DIRECTION('center_axis',(1.,0.,0.));
#66931=DIRECTION('ref_axis',(0.,-1.,0.));
#66932=DIRECTION('',(0.,-1.,0.));
#66933=DIRECTION('',(0.,0.,-1.));
#66934=DIRECTION('',(0.,-1.,0.));
#66935=DIRECTION('center_axis',(0.,1.,0.));
#66936=DIRECTION('ref_axis',(1.,0.,0.));
#66937=DIRECTION('',(1.,0.,0.));
#66938=DIRECTION('',(0.,0.,-1.));
#66939=DIRECTION('',(1.,0.,0.));
#66940=DIRECTION('center_axis',(-1.,0.,0.));
#66941=DIRECTION('ref_axis',(0.,1.,0.));
#66942=DIRECTION('',(0.,1.,0.));
#66943=DIRECTION('',(0.,1.,0.));
#66944=DIRECTION('center_axis',(0.,0.,-1.));
#66945=DIRECTION('ref_axis',(-1.,0.,0.));
#66946=DIRECTION('center_axis',(0.,-1.,0.));
#66947=DIRECTION('ref_axis',(-1.,0.,0.));
#66948=DIRECTION('',(-1.,0.,0.));
#66949=DIRECTION('',(0.,0.,-1.));
#66950=DIRECTION('',(-1.,0.,0.));
#66951=DIRECTION('',(0.,0.,-1.));
#66952=DIRECTION('center_axis',(1.,0.,0.));
#66953=DIRECTION('ref_axis',(0.,-1.,0.));
#66954=DIRECTION('',(0.,-1.,0.));
#66955=DIRECTION('',(0.,0.,-1.));
#66956=DIRECTION('',(0.,-1.,0.));
#66957=DIRECTION('center_axis',(0.,1.,0.));
#66958=DIRECTION('ref_axis',(1.,0.,0.));
#66959=DIRECTION('',(1.,0.,0.));
#66960=DIRECTION('',(0.,0.,-1.));
#66961=DIRECTION('',(1.,0.,0.));
#66962=DIRECTION('center_axis',(-1.,0.,0.));
#66963=DIRECTION('ref_axis',(0.,1.,0.));
#66964=DIRECTION('',(0.,1.,0.));
#66965=DIRECTION('',(0.,1.,0.));
#66966=DIRECTION('center_axis',(0.,0.,-1.));
#66967=DIRECTION('ref_axis',(-1.,0.,0.));
#66968=DIRECTION('center_axis',(0.,-1.,0.));
#66969=DIRECTION('ref_axis',(-1.,0.,0.));
#66970=DIRECTION('',(-1.,0.,0.));
#66971=DIRECTION('',(0.,0.,-1.));
#66972=DIRECTION('',(-1.,0.,0.));
#66973=DIRECTION('',(0.,0.,-1.));
#66974=DIRECTION('center_axis',(1.,0.,0.));
#66975=DIRECTION('ref_axis',(0.,-1.,0.));
#66976=DIRECTION('',(0.,-1.,0.));
#66977=DIRECTION('',(0.,0.,-1.));
#66978=DIRECTION('',(0.,-1.,0.));
#66979=DIRECTION('center_axis',(0.,1.,0.));
#66980=DIRECTION('ref_axis',(1.,0.,0.));
#66981=DIRECTION('',(1.,0.,0.));
#66982=DIRECTION('',(0.,0.,-1.));
#66983=DIRECTION('',(1.,0.,0.));
#66984=DIRECTION('center_axis',(-1.,0.,0.));
#66985=DIRECTION('ref_axis',(0.,1.,0.));
#66986=DIRECTION('',(0.,1.,0.));
#66987=DIRECTION('',(0.,1.,0.));
#66988=DIRECTION('center_axis',(0.,0.,-1.));
#66989=DIRECTION('ref_axis',(-1.,0.,0.));
#66990=DIRECTION('center_axis',(0.,-1.,0.));
#66991=DIRECTION('ref_axis',(-1.,0.,0.));
#66992=DIRECTION('',(-1.,0.,0.));
#66993=DIRECTION('',(0.,0.,-1.));
#66994=DIRECTION('',(-1.,0.,0.));
#66995=DIRECTION('',(0.,0.,-1.));
#66996=DIRECTION('center_axis',(1.,0.,0.));
#66997=DIRECTION('ref_axis',(0.,-1.,0.));
#66998=DIRECTION('',(0.,-1.,0.));
#66999=DIRECTION('',(0.,0.,-1.));
#67000=DIRECTION('',(0.,-1.,0.));
#67001=DIRECTION('center_axis',(0.,1.,0.));
#67002=DIRECTION('ref_axis',(1.,0.,0.));
#67003=DIRECTION('',(1.,0.,0.));
#67004=DIRECTION('',(0.,0.,-1.));
#67005=DIRECTION('',(1.,0.,0.));
#67006=DIRECTION('center_axis',(-1.,0.,0.));
#67007=DIRECTION('ref_axis',(0.,1.,0.));
#67008=DIRECTION('',(0.,1.,0.));
#67009=DIRECTION('',(0.,1.,0.));
#67010=DIRECTION('center_axis',(0.,0.,-1.));
#67011=DIRECTION('ref_axis',(-1.,0.,0.));
#67012=DIRECTION('center_axis',(0.,-1.,0.));
#67013=DIRECTION('ref_axis',(-1.,0.,0.));
#67014=DIRECTION('',(-1.,0.,0.));
#67015=DIRECTION('',(0.,0.,-1.));
#67016=DIRECTION('',(-1.,0.,0.));
#67017=DIRECTION('',(0.,0.,-1.));
#67018=DIRECTION('center_axis',(1.,0.,0.));
#67019=DIRECTION('ref_axis',(0.,-1.,0.));
#67020=DIRECTION('',(0.,-1.,0.));
#67021=DIRECTION('',(0.,0.,-1.));
#67022=DIRECTION('',(0.,-1.,0.));
#67023=DIRECTION('center_axis',(0.,1.,0.));
#67024=DIRECTION('ref_axis',(1.,0.,0.));
#67025=DIRECTION('',(1.,0.,0.));
#67026=DIRECTION('',(0.,0.,-1.));
#67027=DIRECTION('',(1.,0.,0.));
#67028=DIRECTION('center_axis',(-1.,0.,0.));
#67029=DIRECTION('ref_axis',(0.,1.,0.));
#67030=DIRECTION('',(0.,1.,0.));
#67031=DIRECTION('',(0.,1.,0.));
#67032=DIRECTION('center_axis',(0.,0.,-1.));
#67033=DIRECTION('ref_axis',(-1.,0.,0.));
#67034=DIRECTION('center_axis',(0.,-1.,0.));
#67035=DIRECTION('ref_axis',(-1.,0.,0.));
#67036=DIRECTION('',(-1.,0.,0.));
#67037=DIRECTION('',(0.,0.,-1.));
#67038=DIRECTION('',(-1.,0.,0.));
#67039=DIRECTION('',(0.,0.,-1.));
#67040=DIRECTION('center_axis',(1.,0.,0.));
#67041=DIRECTION('ref_axis',(0.,-1.,0.));
#67042=DIRECTION('',(0.,-1.,0.));
#67043=DIRECTION('',(0.,0.,-1.));
#67044=DIRECTION('',(0.,-1.,0.));
#67045=DIRECTION('center_axis',(0.,1.,0.));
#67046=DIRECTION('ref_axis',(1.,0.,0.));
#67047=DIRECTION('',(1.,0.,0.));
#67048=DIRECTION('',(0.,0.,-1.));
#67049=DIRECTION('',(1.,0.,0.));
#67050=DIRECTION('center_axis',(-1.,0.,0.));
#67051=DIRECTION('ref_axis',(0.,1.,0.));
#67052=DIRECTION('',(0.,1.,0.));
#67053=DIRECTION('',(0.,1.,0.));
#67054=DIRECTION('center_axis',(0.,0.,-1.));
#67055=DIRECTION('ref_axis',(-1.,0.,0.));
#67056=DIRECTION('center_axis',(0.,-1.,0.));
#67057=DIRECTION('ref_axis',(-1.,0.,0.));
#67058=DIRECTION('',(-1.,0.,0.));
#67059=DIRECTION('',(0.,0.,-1.));
#67060=DIRECTION('',(-1.,0.,0.));
#67061=DIRECTION('',(0.,0.,-1.));
#67062=DIRECTION('center_axis',(1.,0.,0.));
#67063=DIRECTION('ref_axis',(0.,-1.,0.));
#67064=DIRECTION('',(0.,-1.,0.));
#67065=DIRECTION('',(0.,0.,-1.));
#67066=DIRECTION('',(0.,-1.,0.));
#67067=DIRECTION('center_axis',(0.,1.,0.));
#67068=DIRECTION('ref_axis',(1.,0.,0.));
#67069=DIRECTION('',(1.,0.,0.));
#67070=DIRECTION('',(0.,0.,-1.));
#67071=DIRECTION('',(1.,0.,0.));
#67072=DIRECTION('center_axis',(-1.,0.,0.));
#67073=DIRECTION('ref_axis',(0.,1.,0.));
#67074=DIRECTION('',(0.,1.,0.));
#67075=DIRECTION('',(0.,1.,0.));
#67076=DIRECTION('center_axis',(0.,0.,-1.));
#67077=DIRECTION('ref_axis',(-1.,0.,0.));
#67078=DIRECTION('center_axis',(0.,-1.,0.));
#67079=DIRECTION('ref_axis',(-1.,0.,0.));
#67080=DIRECTION('',(-1.,0.,0.));
#67081=DIRECTION('',(0.,0.,-1.));
#67082=DIRECTION('',(-1.,0.,0.));
#67083=DIRECTION('',(0.,0.,-1.));
#67084=DIRECTION('center_axis',(1.,0.,0.));
#67085=DIRECTION('ref_axis',(0.,-1.,0.));
#67086=DIRECTION('',(0.,-1.,0.));
#67087=DIRECTION('',(0.,0.,-1.));
#67088=DIRECTION('',(0.,-1.,0.));
#67089=DIRECTION('center_axis',(0.,1.,0.));
#67090=DIRECTION('ref_axis',(1.,0.,0.));
#67091=DIRECTION('',(1.,0.,0.));
#67092=DIRECTION('',(0.,0.,-1.));
#67093=DIRECTION('',(1.,0.,0.));
#67094=DIRECTION('center_axis',(-1.,0.,0.));
#67095=DIRECTION('ref_axis',(0.,1.,0.));
#67096=DIRECTION('',(0.,1.,0.));
#67097=DIRECTION('',(0.,1.,0.));
#67098=DIRECTION('center_axis',(0.,0.,-1.));
#67099=DIRECTION('ref_axis',(-1.,0.,0.));
#67100=DIRECTION('center_axis',(0.,-1.,0.));
#67101=DIRECTION('ref_axis',(-1.,0.,0.));
#67102=DIRECTION('',(-1.,0.,0.));
#67103=DIRECTION('',(0.,0.,-1.));
#67104=DIRECTION('',(-1.,0.,0.));
#67105=DIRECTION('',(0.,0.,-1.));
#67106=DIRECTION('center_axis',(1.,0.,0.));
#67107=DIRECTION('ref_axis',(0.,-1.,0.));
#67108=DIRECTION('',(0.,-1.,0.));
#67109=DIRECTION('',(0.,0.,-1.));
#67110=DIRECTION('',(0.,-1.,0.));
#67111=DIRECTION('center_axis',(0.,1.,0.));
#67112=DIRECTION('ref_axis',(1.,0.,0.));
#67113=DIRECTION('',(1.,0.,0.));
#67114=DIRECTION('',(0.,0.,-1.));
#67115=DIRECTION('',(1.,0.,0.));
#67116=DIRECTION('center_axis',(-1.,0.,0.));
#67117=DIRECTION('ref_axis',(0.,1.,0.));
#67118=DIRECTION('',(0.,1.,0.));
#67119=DIRECTION('',(0.,1.,0.));
#67120=DIRECTION('center_axis',(0.,0.,-1.));
#67121=DIRECTION('ref_axis',(-1.,0.,0.));
#67122=DIRECTION('center_axis',(0.,-1.,0.));
#67123=DIRECTION('ref_axis',(-1.,0.,0.));
#67124=DIRECTION('',(-1.,0.,0.));
#67125=DIRECTION('',(0.,0.,-1.));
#67126=DIRECTION('',(-1.,0.,0.));
#67127=DIRECTION('',(0.,0.,-1.));
#67128=DIRECTION('center_axis',(1.,0.,0.));
#67129=DIRECTION('ref_axis',(0.,-1.,0.));
#67130=DIRECTION('',(0.,-1.,0.));
#67131=DIRECTION('',(0.,0.,-1.));
#67132=DIRECTION('',(0.,-1.,0.));
#67133=DIRECTION('center_axis',(0.,1.,0.));
#67134=DIRECTION('ref_axis',(1.,0.,0.));
#67135=DIRECTION('',(1.,0.,0.));
#67136=DIRECTION('',(0.,0.,-1.));
#67137=DIRECTION('',(1.,0.,0.));
#67138=DIRECTION('center_axis',(-1.,0.,0.));
#67139=DIRECTION('ref_axis',(0.,1.,0.));
#67140=DIRECTION('',(0.,1.,0.));
#67141=DIRECTION('',(0.,1.,0.));
#67142=DIRECTION('center_axis',(0.,0.,-1.));
#67143=DIRECTION('ref_axis',(-1.,0.,0.));
#67144=DIRECTION('center_axis',(0.,-1.,0.));
#67145=DIRECTION('ref_axis',(-1.,0.,0.));
#67146=DIRECTION('',(-1.,0.,0.));
#67147=DIRECTION('',(0.,0.,-1.));
#67148=DIRECTION('',(-1.,0.,0.));
#67149=DIRECTION('',(0.,0.,-1.));
#67150=DIRECTION('center_axis',(1.,0.,0.));
#67151=DIRECTION('ref_axis',(0.,-1.,0.));
#67152=DIRECTION('',(0.,-1.,0.));
#67153=DIRECTION('',(0.,0.,-1.));
#67154=DIRECTION('',(0.,-1.,0.));
#67155=DIRECTION('center_axis',(0.,1.,0.));
#67156=DIRECTION('ref_axis',(1.,0.,0.));
#67157=DIRECTION('',(1.,0.,0.));
#67158=DIRECTION('',(0.,0.,-1.));
#67159=DIRECTION('',(1.,0.,0.));
#67160=DIRECTION('center_axis',(-1.,0.,0.));
#67161=DIRECTION('ref_axis',(0.,1.,0.));
#67162=DIRECTION('',(0.,1.,0.));
#67163=DIRECTION('',(0.,1.,0.));
#67164=DIRECTION('center_axis',(0.,0.,-1.));
#67165=DIRECTION('ref_axis',(-1.,0.,0.));
#67166=DIRECTION('center_axis',(0.,-1.,0.));
#67167=DIRECTION('ref_axis',(-1.,0.,0.));
#67168=DIRECTION('',(-1.,0.,0.));
#67169=DIRECTION('',(0.,0.,-1.));
#67170=DIRECTION('',(-1.,0.,0.));
#67171=DIRECTION('',(0.,0.,-1.));
#67172=DIRECTION('center_axis',(1.,0.,0.));
#67173=DIRECTION('ref_axis',(0.,-1.,0.));
#67174=DIRECTION('',(0.,-1.,0.));
#67175=DIRECTION('',(0.,0.,-1.));
#67176=DIRECTION('',(0.,-1.,0.));
#67177=DIRECTION('center_axis',(0.,1.,0.));
#67178=DIRECTION('ref_axis',(1.,0.,0.));
#67179=DIRECTION('',(1.,0.,0.));
#67180=DIRECTION('',(0.,0.,-1.));
#67181=DIRECTION('',(1.,0.,0.));
#67182=DIRECTION('center_axis',(-1.,0.,0.));
#67183=DIRECTION('ref_axis',(0.,1.,0.));
#67184=DIRECTION('',(0.,1.,0.));
#67185=DIRECTION('',(0.,1.,0.));
#67186=DIRECTION('center_axis',(0.,0.,-1.));
#67187=DIRECTION('ref_axis',(-1.,0.,0.));
#67188=DIRECTION('center_axis',(0.,-1.,0.));
#67189=DIRECTION('ref_axis',(-1.,0.,0.));
#67190=DIRECTION('',(-1.,0.,0.));
#67191=DIRECTION('',(0.,0.,-1.));
#67192=DIRECTION('',(-1.,0.,0.));
#67193=DIRECTION('',(0.,0.,-1.));
#67194=DIRECTION('center_axis',(1.,0.,0.));
#67195=DIRECTION('ref_axis',(0.,-1.,0.));
#67196=DIRECTION('',(0.,-1.,0.));
#67197=DIRECTION('',(0.,0.,-1.));
#67198=DIRECTION('',(0.,-1.,0.));
#67199=DIRECTION('center_axis',(0.,1.,0.));
#67200=DIRECTION('ref_axis',(1.,0.,0.));
#67201=DIRECTION('',(1.,0.,0.));
#67202=DIRECTION('',(0.,0.,-1.));
#67203=DIRECTION('',(1.,0.,0.));
#67204=DIRECTION('center_axis',(-1.,0.,0.));
#67205=DIRECTION('ref_axis',(0.,1.,0.));
#67206=DIRECTION('',(0.,1.,0.));
#67207=DIRECTION('',(0.,1.,0.));
#67208=DIRECTION('center_axis',(0.,0.,-1.));
#67209=DIRECTION('ref_axis',(-1.,0.,0.));
#67210=DIRECTION('center_axis',(0.,-1.,0.));
#67211=DIRECTION('ref_axis',(-1.,0.,0.));
#67212=DIRECTION('',(-1.,0.,0.));
#67213=DIRECTION('',(0.,0.,-1.));
#67214=DIRECTION('',(-1.,0.,0.));
#67215=DIRECTION('',(0.,0.,-1.));
#67216=DIRECTION('center_axis',(1.,0.,0.));
#67217=DIRECTION('ref_axis',(0.,-1.,0.));
#67218=DIRECTION('',(0.,-1.,0.));
#67219=DIRECTION('',(0.,0.,-1.));
#67220=DIRECTION('',(0.,-1.,0.));
#67221=DIRECTION('center_axis',(0.,1.,0.));
#67222=DIRECTION('ref_axis',(1.,0.,0.));
#67223=DIRECTION('',(1.,0.,0.));
#67224=DIRECTION('',(0.,0.,-1.));
#67225=DIRECTION('',(1.,0.,0.));
#67226=DIRECTION('center_axis',(-1.,0.,0.));
#67227=DIRECTION('ref_axis',(0.,1.,0.));
#67228=DIRECTION('',(0.,1.,0.));
#67229=DIRECTION('',(0.,1.,0.));
#67230=DIRECTION('center_axis',(0.,0.,-1.));
#67231=DIRECTION('ref_axis',(-1.,0.,0.));
#67232=DIRECTION('center_axis',(0.,-1.,0.));
#67233=DIRECTION('ref_axis',(-1.,0.,0.));
#67234=DIRECTION('',(-1.,0.,0.));
#67235=DIRECTION('',(0.,0.,-1.));
#67236=DIRECTION('',(-1.,0.,0.));
#67237=DIRECTION('',(0.,0.,-1.));
#67238=DIRECTION('center_axis',(1.,0.,0.));
#67239=DIRECTION('ref_axis',(0.,-1.,0.));
#67240=DIRECTION('',(0.,-1.,0.));
#67241=DIRECTION('',(0.,0.,-1.));
#67242=DIRECTION('',(0.,-1.,0.));
#67243=DIRECTION('center_axis',(0.,1.,0.));
#67244=DIRECTION('ref_axis',(1.,0.,0.));
#67245=DIRECTION('',(1.,0.,0.));
#67246=DIRECTION('',(0.,0.,-1.));
#67247=DIRECTION('',(1.,0.,0.));
#67248=DIRECTION('center_axis',(-1.,0.,0.));
#67249=DIRECTION('ref_axis',(0.,1.,0.));
#67250=DIRECTION('',(0.,1.,0.));
#67251=DIRECTION('',(0.,1.,0.));
#67252=DIRECTION('center_axis',(0.,0.,-1.));
#67253=DIRECTION('ref_axis',(-1.,0.,0.));
#67254=DIRECTION('center_axis',(0.,-1.,0.));
#67255=DIRECTION('ref_axis',(-1.,0.,0.));
#67256=DIRECTION('',(-1.,0.,0.));
#67257=DIRECTION('',(0.,0.,-1.));
#67258=DIRECTION('',(-1.,0.,0.));
#67259=DIRECTION('',(0.,0.,-1.));
#67260=DIRECTION('center_axis',(1.,0.,0.));
#67261=DIRECTION('ref_axis',(0.,-1.,0.));
#67262=DIRECTION('',(0.,-1.,0.));
#67263=DIRECTION('',(0.,0.,-1.));
#67264=DIRECTION('',(0.,-1.,0.));
#67265=DIRECTION('center_axis',(0.,1.,0.));
#67266=DIRECTION('ref_axis',(1.,0.,0.));
#67267=DIRECTION('',(1.,0.,0.));
#67268=DIRECTION('',(0.,0.,-1.));
#67269=DIRECTION('',(1.,0.,0.));
#67270=DIRECTION('center_axis',(-1.,0.,0.));
#67271=DIRECTION('ref_axis',(0.,1.,0.));
#67272=DIRECTION('',(0.,1.,0.));
#67273=DIRECTION('',(0.,1.,0.));
#67274=DIRECTION('center_axis',(0.,0.,-1.));
#67275=DIRECTION('ref_axis',(-1.,0.,0.));
#67276=DIRECTION('center_axis',(0.,-1.,0.));
#67277=DIRECTION('ref_axis',(-1.,0.,0.));
#67278=DIRECTION('',(-1.,0.,0.));
#67279=DIRECTION('',(0.,0.,-1.));
#67280=DIRECTION('',(-1.,0.,0.));
#67281=DIRECTION('',(0.,0.,-1.));
#67282=DIRECTION('center_axis',(1.,0.,0.));
#67283=DIRECTION('ref_axis',(0.,-1.,0.));
#67284=DIRECTION('',(0.,-1.,0.));
#67285=DIRECTION('',(0.,0.,-1.));
#67286=DIRECTION('',(0.,-1.,0.));
#67287=DIRECTION('center_axis',(0.,1.,0.));
#67288=DIRECTION('ref_axis',(1.,0.,0.));
#67289=DIRECTION('',(1.,0.,0.));
#67290=DIRECTION('',(0.,0.,-1.));
#67291=DIRECTION('',(1.,0.,0.));
#67292=DIRECTION('center_axis',(-1.,0.,0.));
#67293=DIRECTION('ref_axis',(0.,1.,0.));
#67294=DIRECTION('',(0.,1.,0.));
#67295=DIRECTION('',(0.,1.,0.));
#67296=DIRECTION('center_axis',(0.,0.,-1.));
#67297=DIRECTION('ref_axis',(-1.,0.,0.));
#67298=DIRECTION('center_axis',(0.,-1.,0.));
#67299=DIRECTION('ref_axis',(-1.,0.,0.));
#67300=DIRECTION('',(-1.,0.,0.));
#67301=DIRECTION('',(0.,0.,-1.));
#67302=DIRECTION('',(-1.,0.,0.));
#67303=DIRECTION('',(0.,0.,-1.));
#67304=DIRECTION('center_axis',(1.,0.,0.));
#67305=DIRECTION('ref_axis',(0.,-1.,0.));
#67306=DIRECTION('',(0.,-1.,0.));
#67307=DIRECTION('',(0.,0.,-1.));
#67308=DIRECTION('',(0.,-1.,0.));
#67309=DIRECTION('center_axis',(0.,1.,0.));
#67310=DIRECTION('ref_axis',(1.,0.,0.));
#67311=DIRECTION('',(1.,0.,0.));
#67312=DIRECTION('',(0.,0.,-1.));
#67313=DIRECTION('',(1.,0.,0.));
#67314=DIRECTION('center_axis',(-1.,0.,0.));
#67315=DIRECTION('ref_axis',(0.,1.,0.));
#67316=DIRECTION('',(0.,1.,0.));
#67317=DIRECTION('',(0.,1.,0.));
#67318=DIRECTION('center_axis',(0.,0.,-1.));
#67319=DIRECTION('ref_axis',(-1.,0.,0.));
#67320=DIRECTION('center_axis',(0.,-1.,0.));
#67321=DIRECTION('ref_axis',(-1.,0.,0.));
#67322=DIRECTION('',(-1.,0.,0.));
#67323=DIRECTION('',(0.,0.,-1.));
#67324=DIRECTION('',(-1.,0.,0.));
#67325=DIRECTION('',(0.,0.,-1.));
#67326=DIRECTION('center_axis',(1.,0.,0.));
#67327=DIRECTION('ref_axis',(0.,-1.,0.));
#67328=DIRECTION('',(0.,-1.,0.));
#67329=DIRECTION('',(0.,0.,-1.));
#67330=DIRECTION('',(0.,-1.,0.));
#67331=DIRECTION('center_axis',(0.,1.,0.));
#67332=DIRECTION('ref_axis',(1.,0.,0.));
#67333=DIRECTION('',(1.,0.,0.));
#67334=DIRECTION('',(0.,0.,-1.));
#67335=DIRECTION('',(1.,0.,0.));
#67336=DIRECTION('center_axis',(-1.,0.,0.));
#67337=DIRECTION('ref_axis',(0.,1.,0.));
#67338=DIRECTION('',(0.,1.,0.));
#67339=DIRECTION('',(0.,1.,0.));
#67340=DIRECTION('center_axis',(0.,0.,-1.));
#67341=DIRECTION('ref_axis',(-1.,0.,0.));
#67342=DIRECTION('center_axis',(0.,-1.,0.));
#67343=DIRECTION('ref_axis',(-1.,0.,0.));
#67344=DIRECTION('',(-1.,0.,0.));
#67345=DIRECTION('',(0.,0.,-1.));
#67346=DIRECTION('',(-1.,0.,0.));
#67347=DIRECTION('',(0.,0.,-1.));
#67348=DIRECTION('center_axis',(1.,0.,0.));
#67349=DIRECTION('ref_axis',(0.,-1.,0.));
#67350=DIRECTION('',(0.,-1.,0.));
#67351=DIRECTION('',(0.,0.,-1.));
#67352=DIRECTION('',(0.,-1.,0.));
#67353=DIRECTION('center_axis',(0.,1.,0.));
#67354=DIRECTION('ref_axis',(1.,0.,0.));
#67355=DIRECTION('',(1.,0.,0.));
#67356=DIRECTION('',(0.,0.,-1.));
#67357=DIRECTION('',(1.,0.,0.));
#67358=DIRECTION('center_axis',(-1.,0.,0.));
#67359=DIRECTION('ref_axis',(0.,1.,0.));
#67360=DIRECTION('',(0.,1.,0.));
#67361=DIRECTION('',(0.,1.,0.));
#67362=DIRECTION('center_axis',(0.,0.,-1.));
#67363=DIRECTION('ref_axis',(-1.,0.,0.));
#67364=DIRECTION('center_axis',(0.,-1.,0.));
#67365=DIRECTION('ref_axis',(-1.,0.,0.));
#67366=DIRECTION('',(-1.,0.,0.));
#67367=DIRECTION('',(0.,0.,-1.));
#67368=DIRECTION('',(-1.,0.,0.));
#67369=DIRECTION('',(0.,0.,-1.));
#67370=DIRECTION('center_axis',(1.,0.,0.));
#67371=DIRECTION('ref_axis',(0.,-1.,0.));
#67372=DIRECTION('',(0.,-1.,0.));
#67373=DIRECTION('',(0.,0.,-1.));
#67374=DIRECTION('',(0.,-1.,0.));
#67375=DIRECTION('center_axis',(0.,1.,0.));
#67376=DIRECTION('ref_axis',(1.,0.,0.));
#67377=DIRECTION('',(1.,0.,0.));
#67378=DIRECTION('',(0.,0.,-1.));
#67379=DIRECTION('',(1.,0.,0.));
#67380=DIRECTION('center_axis',(-1.,0.,0.));
#67381=DIRECTION('ref_axis',(0.,1.,0.));
#67382=DIRECTION('',(0.,1.,0.));
#67383=DIRECTION('',(0.,1.,0.));
#67384=DIRECTION('center_axis',(0.,0.,-1.));
#67385=DIRECTION('ref_axis',(-1.,0.,0.));
#67386=DIRECTION('center_axis',(0.,-1.,0.));
#67387=DIRECTION('ref_axis',(-1.,0.,0.));
#67388=DIRECTION('',(-1.,0.,0.));
#67389=DIRECTION('',(0.,0.,-1.));
#67390=DIRECTION('',(-1.,0.,0.));
#67391=DIRECTION('',(0.,0.,-1.));
#67392=DIRECTION('center_axis',(1.,0.,0.));
#67393=DIRECTION('ref_axis',(0.,-1.,0.));
#67394=DIRECTION('',(0.,-1.,0.));
#67395=DIRECTION('',(0.,0.,-1.));
#67396=DIRECTION('',(0.,-1.,0.));
#67397=DIRECTION('center_axis',(0.,1.,0.));
#67398=DIRECTION('ref_axis',(1.,0.,0.));
#67399=DIRECTION('',(1.,0.,0.));
#67400=DIRECTION('',(0.,0.,-1.));
#67401=DIRECTION('',(1.,0.,0.));
#67402=DIRECTION('center_axis',(-1.,0.,0.));
#67403=DIRECTION('ref_axis',(0.,1.,0.));
#67404=DIRECTION('',(0.,1.,0.));
#67405=DIRECTION('',(0.,1.,0.));
#67406=DIRECTION('center_axis',(0.,0.,-1.));
#67407=DIRECTION('ref_axis',(-1.,0.,0.));
#67408=DIRECTION('center_axis',(0.,-1.,0.));
#67409=DIRECTION('ref_axis',(-1.,0.,0.));
#67410=DIRECTION('',(-1.,0.,0.));
#67411=DIRECTION('',(0.,0.,-1.));
#67412=DIRECTION('',(-1.,0.,0.));
#67413=DIRECTION('',(0.,0.,-1.));
#67414=DIRECTION('center_axis',(1.,0.,0.));
#67415=DIRECTION('ref_axis',(0.,-1.,0.));
#67416=DIRECTION('',(0.,-1.,0.));
#67417=DIRECTION('',(0.,0.,-1.));
#67418=DIRECTION('',(0.,-1.,0.));
#67419=DIRECTION('center_axis',(0.,1.,0.));
#67420=DIRECTION('ref_axis',(1.,0.,0.));
#67421=DIRECTION('',(1.,0.,0.));
#67422=DIRECTION('',(0.,0.,-1.));
#67423=DIRECTION('',(1.,0.,0.));
#67424=DIRECTION('center_axis',(-1.,0.,0.));
#67425=DIRECTION('ref_axis',(0.,1.,0.));
#67426=DIRECTION('',(0.,1.,0.));
#67427=DIRECTION('',(0.,1.,0.));
#67428=DIRECTION('center_axis',(0.,0.,-1.));
#67429=DIRECTION('ref_axis',(-1.,0.,0.));
#67430=DIRECTION('center_axis',(0.,-1.,0.));
#67431=DIRECTION('ref_axis',(-1.,0.,0.));
#67432=DIRECTION('',(-1.,0.,0.));
#67433=DIRECTION('',(0.,0.,-1.));
#67434=DIRECTION('',(-1.,0.,0.));
#67435=DIRECTION('',(0.,0.,-1.));
#67436=DIRECTION('center_axis',(1.,0.,0.));
#67437=DIRECTION('ref_axis',(0.,-1.,0.));
#67438=DIRECTION('',(0.,-1.,0.));
#67439=DIRECTION('',(0.,0.,-1.));
#67440=DIRECTION('',(0.,-1.,0.));
#67441=DIRECTION('center_axis',(0.,1.,0.));
#67442=DIRECTION('ref_axis',(1.,0.,0.));
#67443=DIRECTION('',(1.,0.,0.));
#67444=DIRECTION('',(0.,0.,-1.));
#67445=DIRECTION('',(1.,0.,0.));
#67446=DIRECTION('center_axis',(-1.,0.,0.));
#67447=DIRECTION('ref_axis',(0.,1.,0.));
#67448=DIRECTION('',(0.,1.,0.));
#67449=DIRECTION('',(0.,1.,0.));
#67450=DIRECTION('center_axis',(0.,0.,-1.));
#67451=DIRECTION('ref_axis',(-1.,0.,0.));
#67452=DIRECTION('center_axis',(0.,-1.,0.));
#67453=DIRECTION('ref_axis',(-1.,0.,0.));
#67454=DIRECTION('',(-1.,0.,0.));
#67455=DIRECTION('',(0.,0.,-1.));
#67456=DIRECTION('',(-1.,0.,0.));
#67457=DIRECTION('',(0.,0.,-1.));
#67458=DIRECTION('center_axis',(1.,0.,0.));
#67459=DIRECTION('ref_axis',(0.,-1.,0.));
#67460=DIRECTION('',(0.,-1.,0.));
#67461=DIRECTION('',(0.,0.,-1.));
#67462=DIRECTION('',(0.,-1.,0.));
#67463=DIRECTION('center_axis',(0.,1.,0.));
#67464=DIRECTION('ref_axis',(1.,0.,0.));
#67465=DIRECTION('',(1.,0.,0.));
#67466=DIRECTION('',(0.,0.,-1.));
#67467=DIRECTION('',(1.,0.,0.));
#67468=DIRECTION('center_axis',(-1.,0.,0.));
#67469=DIRECTION('ref_axis',(0.,1.,0.));
#67470=DIRECTION('',(0.,1.,0.));
#67471=DIRECTION('',(0.,1.,0.));
#67472=DIRECTION('center_axis',(0.,0.,-1.));
#67473=DIRECTION('ref_axis',(-1.,0.,0.));
#67474=DIRECTION('center_axis',(0.,-1.,0.));
#67475=DIRECTION('ref_axis',(-1.,0.,0.));
#67476=DIRECTION('',(-1.,0.,0.));
#67477=DIRECTION('',(0.,0.,-1.));
#67478=DIRECTION('',(-1.,0.,0.));
#67479=DIRECTION('',(0.,0.,-1.));
#67480=DIRECTION('center_axis',(1.,0.,0.));
#67481=DIRECTION('ref_axis',(0.,-1.,0.));
#67482=DIRECTION('',(0.,-1.,0.));
#67483=DIRECTION('',(0.,0.,-1.));
#67484=DIRECTION('',(0.,-1.,0.));
#67485=DIRECTION('center_axis',(0.,1.,0.));
#67486=DIRECTION('ref_axis',(1.,0.,0.));
#67487=DIRECTION('',(1.,0.,0.));
#67488=DIRECTION('',(0.,0.,-1.));
#67489=DIRECTION('',(1.,0.,0.));
#67490=DIRECTION('center_axis',(-1.,0.,0.));
#67491=DIRECTION('ref_axis',(0.,1.,0.));
#67492=DIRECTION('',(0.,1.,0.));
#67493=DIRECTION('',(0.,1.,0.));
#67494=DIRECTION('center_axis',(0.,0.,-1.));
#67495=DIRECTION('ref_axis',(-1.,0.,0.));
#67496=DIRECTION('center_axis',(0.,-1.,0.));
#67497=DIRECTION('ref_axis',(-1.,0.,0.));
#67498=DIRECTION('',(-1.,0.,0.));
#67499=DIRECTION('',(0.,0.,-1.));
#67500=DIRECTION('',(-1.,0.,0.));
#67501=DIRECTION('',(0.,0.,-1.));
#67502=DIRECTION('center_axis',(1.,0.,0.));
#67503=DIRECTION('ref_axis',(0.,-1.,0.));
#67504=DIRECTION('',(0.,-1.,0.));
#67505=DIRECTION('',(0.,0.,-1.));
#67506=DIRECTION('',(0.,-1.,0.));
#67507=DIRECTION('center_axis',(0.,1.,0.));
#67508=DIRECTION('ref_axis',(1.,0.,0.));
#67509=DIRECTION('',(1.,0.,0.));
#67510=DIRECTION('',(0.,0.,-1.));
#67511=DIRECTION('',(1.,0.,0.));
#67512=DIRECTION('center_axis',(-1.,0.,0.));
#67513=DIRECTION('ref_axis',(0.,1.,0.));
#67514=DIRECTION('',(0.,1.,0.));
#67515=DIRECTION('',(0.,1.,0.));
#67516=DIRECTION('center_axis',(0.,0.,-1.));
#67517=DIRECTION('ref_axis',(-1.,0.,0.));
#67518=DIRECTION('center_axis',(0.,-1.,0.));
#67519=DIRECTION('ref_axis',(-1.,0.,0.));
#67520=DIRECTION('',(-1.,0.,0.));
#67521=DIRECTION('',(0.,0.,-1.));
#67522=DIRECTION('',(-1.,0.,0.));
#67523=DIRECTION('',(0.,0.,-1.));
#67524=DIRECTION('center_axis',(1.,0.,0.));
#67525=DIRECTION('ref_axis',(0.,-1.,0.));
#67526=DIRECTION('',(0.,-1.,0.));
#67527=DIRECTION('',(0.,0.,-1.));
#67528=DIRECTION('',(0.,-1.,0.));
#67529=DIRECTION('center_axis',(0.,1.,0.));
#67530=DIRECTION('ref_axis',(1.,0.,0.));
#67531=DIRECTION('',(1.,0.,0.));
#67532=DIRECTION('',(0.,0.,-1.));
#67533=DIRECTION('',(1.,0.,0.));
#67534=DIRECTION('center_axis',(-1.,0.,0.));
#67535=DIRECTION('ref_axis',(0.,1.,0.));
#67536=DIRECTION('',(0.,1.,0.));
#67537=DIRECTION('',(0.,1.,0.));
#67538=DIRECTION('center_axis',(0.,0.,-1.));
#67539=DIRECTION('ref_axis',(-1.,0.,0.));
#67540=DIRECTION('center_axis',(0.,-1.,0.));
#67541=DIRECTION('ref_axis',(-1.,0.,0.));
#67542=DIRECTION('',(-1.,0.,0.));
#67543=DIRECTION('',(0.,0.,-1.));
#67544=DIRECTION('',(-1.,0.,0.));
#67545=DIRECTION('',(0.,0.,-1.));
#67546=DIRECTION('center_axis',(1.,0.,0.));
#67547=DIRECTION('ref_axis',(0.,-1.,0.));
#67548=DIRECTION('',(0.,-1.,0.));
#67549=DIRECTION('',(0.,0.,-1.));
#67550=DIRECTION('',(0.,-1.,0.));
#67551=DIRECTION('center_axis',(0.,1.,0.));
#67552=DIRECTION('ref_axis',(1.,0.,0.));
#67553=DIRECTION('',(1.,0.,0.));
#67554=DIRECTION('',(0.,0.,-1.));
#67555=DIRECTION('',(1.,0.,0.));
#67556=DIRECTION('center_axis',(-1.,0.,0.));
#67557=DIRECTION('ref_axis',(0.,1.,0.));
#67558=DIRECTION('',(0.,1.,0.));
#67559=DIRECTION('',(0.,1.,0.));
#67560=DIRECTION('center_axis',(0.,0.,-1.));
#67561=DIRECTION('ref_axis',(-1.,0.,0.));
#67562=DIRECTION('center_axis',(0.,-1.,0.));
#67563=DIRECTION('ref_axis',(-1.,0.,0.));
#67564=DIRECTION('',(-1.,0.,0.));
#67565=DIRECTION('',(0.,0.,-1.));
#67566=DIRECTION('',(-1.,0.,0.));
#67567=DIRECTION('',(0.,0.,-1.));
#67568=DIRECTION('center_axis',(1.,0.,0.));
#67569=DIRECTION('ref_axis',(0.,-1.,0.));
#67570=DIRECTION('',(0.,-1.,0.));
#67571=DIRECTION('',(0.,0.,-1.));
#67572=DIRECTION('',(0.,-1.,0.));
#67573=DIRECTION('center_axis',(0.,1.,0.));
#67574=DIRECTION('ref_axis',(1.,0.,0.));
#67575=DIRECTION('',(1.,0.,0.));
#67576=DIRECTION('',(0.,0.,-1.));
#67577=DIRECTION('',(1.,0.,0.));
#67578=DIRECTION('center_axis',(-1.,0.,0.));
#67579=DIRECTION('ref_axis',(0.,1.,0.));
#67580=DIRECTION('',(0.,1.,0.));
#67581=DIRECTION('',(0.,1.,0.));
#67582=DIRECTION('center_axis',(0.,0.,-1.));
#67583=DIRECTION('ref_axis',(-1.,0.,0.));
#67584=DIRECTION('center_axis',(0.,-1.,0.));
#67585=DIRECTION('ref_axis',(-1.,0.,0.));
#67586=DIRECTION('',(-1.,0.,0.));
#67587=DIRECTION('',(0.,0.,-1.));
#67588=DIRECTION('',(-1.,0.,0.));
#67589=DIRECTION('',(0.,0.,-1.));
#67590=DIRECTION('center_axis',(1.,0.,0.));
#67591=DIRECTION('ref_axis',(0.,-1.,0.));
#67592=DIRECTION('',(0.,-1.,0.));
#67593=DIRECTION('',(0.,0.,-1.));
#67594=DIRECTION('',(0.,-1.,0.));
#67595=DIRECTION('center_axis',(0.,1.,0.));
#67596=DIRECTION('ref_axis',(1.,0.,0.));
#67597=DIRECTION('',(1.,0.,0.));
#67598=DIRECTION('',(0.,0.,-1.));
#67599=DIRECTION('',(1.,0.,0.));
#67600=DIRECTION('center_axis',(-1.,0.,0.));
#67601=DIRECTION('ref_axis',(0.,1.,0.));
#67602=DIRECTION('',(0.,1.,0.));
#67603=DIRECTION('',(0.,1.,0.));
#67604=DIRECTION('center_axis',(0.,0.,-1.));
#67605=DIRECTION('ref_axis',(-1.,0.,0.));
#67606=DIRECTION('center_axis',(0.,-1.,0.));
#67607=DIRECTION('ref_axis',(-1.,0.,0.));
#67608=DIRECTION('',(-1.,0.,0.));
#67609=DIRECTION('',(0.,0.,-1.));
#67610=DIRECTION('',(-1.,0.,0.));
#67611=DIRECTION('',(0.,0.,-1.));
#67612=DIRECTION('center_axis',(1.,0.,0.));
#67613=DIRECTION('ref_axis',(0.,-1.,0.));
#67614=DIRECTION('',(0.,-1.,0.));
#67615=DIRECTION('',(0.,0.,-1.));
#67616=DIRECTION('',(0.,-1.,0.));
#67617=DIRECTION('center_axis',(0.,1.,0.));
#67618=DIRECTION('ref_axis',(1.,0.,0.));
#67619=DIRECTION('',(1.,0.,0.));
#67620=DIRECTION('',(0.,0.,-1.));
#67621=DIRECTION('',(1.,0.,0.));
#67622=DIRECTION('center_axis',(-1.,0.,0.));
#67623=DIRECTION('ref_axis',(0.,1.,0.));
#67624=DIRECTION('',(0.,1.,0.));
#67625=DIRECTION('',(0.,1.,0.));
#67626=DIRECTION('center_axis',(0.,0.,-1.));
#67627=DIRECTION('ref_axis',(-1.,0.,0.));
#67628=DIRECTION('center_axis',(0.,-1.,0.));
#67629=DIRECTION('ref_axis',(-1.,0.,0.));
#67630=DIRECTION('',(-1.,0.,0.));
#67631=DIRECTION('',(0.,0.,-1.));
#67632=DIRECTION('',(-1.,0.,0.));
#67633=DIRECTION('',(0.,0.,-1.));
#67634=DIRECTION('center_axis',(1.,0.,0.));
#67635=DIRECTION('ref_axis',(0.,-1.,0.));
#67636=DIRECTION('',(0.,-1.,0.));
#67637=DIRECTION('',(0.,0.,-1.));
#67638=DIRECTION('',(0.,-1.,0.));
#67639=DIRECTION('center_axis',(0.,1.,0.));
#67640=DIRECTION('ref_axis',(1.,0.,0.));
#67641=DIRECTION('',(1.,0.,0.));
#67642=DIRECTION('',(0.,0.,-1.));
#67643=DIRECTION('',(1.,0.,0.));
#67644=DIRECTION('center_axis',(-1.,0.,0.));
#67645=DIRECTION('ref_axis',(0.,1.,0.));
#67646=DIRECTION('',(0.,1.,0.));
#67647=DIRECTION('',(0.,1.,0.));
#67648=DIRECTION('center_axis',(0.,0.,-1.));
#67649=DIRECTION('ref_axis',(-1.,0.,0.));
#67650=DIRECTION('center_axis',(0.,-1.,0.));
#67651=DIRECTION('ref_axis',(-1.,0.,0.));
#67652=DIRECTION('',(-1.,0.,0.));
#67653=DIRECTION('',(0.,0.,-1.));
#67654=DIRECTION('',(-1.,0.,0.));
#67655=DIRECTION('',(0.,0.,-1.));
#67656=DIRECTION('center_axis',(1.,0.,0.));
#67657=DIRECTION('ref_axis',(0.,-1.,0.));
#67658=DIRECTION('',(0.,-1.,0.));
#67659=DIRECTION('',(0.,0.,-1.));
#67660=DIRECTION('',(0.,-1.,0.));
#67661=DIRECTION('center_axis',(0.,1.,0.));
#67662=DIRECTION('ref_axis',(1.,0.,0.));
#67663=DIRECTION('',(1.,0.,0.));
#67664=DIRECTION('',(0.,0.,-1.));
#67665=DIRECTION('',(1.,0.,0.));
#67666=DIRECTION('center_axis',(-1.,0.,0.));
#67667=DIRECTION('ref_axis',(0.,1.,0.));
#67668=DIRECTION('',(0.,1.,0.));
#67669=DIRECTION('',(0.,1.,0.));
#67670=DIRECTION('center_axis',(0.,0.,-1.));
#67671=DIRECTION('ref_axis',(-1.,0.,0.));
#67672=DIRECTION('center_axis',(0.,-1.,0.));
#67673=DIRECTION('ref_axis',(-1.,0.,0.));
#67674=DIRECTION('',(-1.,0.,0.));
#67675=DIRECTION('',(0.,0.,-1.));
#67676=DIRECTION('',(-1.,0.,0.));
#67677=DIRECTION('',(0.,0.,-1.));
#67678=DIRECTION('center_axis',(1.,0.,0.));
#67679=DIRECTION('ref_axis',(0.,-1.,0.));
#67680=DIRECTION('',(0.,-1.,0.));
#67681=DIRECTION('',(0.,0.,-1.));
#67682=DIRECTION('',(0.,-1.,0.));
#67683=DIRECTION('center_axis',(0.,1.,0.));
#67684=DIRECTION('ref_axis',(1.,0.,0.));
#67685=DIRECTION('',(1.,0.,0.));
#67686=DIRECTION('',(0.,0.,-1.));
#67687=DIRECTION('',(1.,0.,0.));
#67688=DIRECTION('center_axis',(-1.,0.,0.));
#67689=DIRECTION('ref_axis',(0.,1.,0.));
#67690=DIRECTION('',(0.,1.,0.));
#67691=DIRECTION('',(0.,1.,0.));
#67692=DIRECTION('center_axis',(0.,0.,-1.));
#67693=DIRECTION('ref_axis',(-1.,0.,0.));
#67694=DIRECTION('center_axis',(0.,-1.,0.));
#67695=DIRECTION('ref_axis',(-1.,0.,0.));
#67696=DIRECTION('',(-1.,0.,0.));
#67697=DIRECTION('',(0.,0.,-1.));
#67698=DIRECTION('',(-1.,0.,0.));
#67699=DIRECTION('',(0.,0.,-1.));
#67700=DIRECTION('center_axis',(1.,0.,0.));
#67701=DIRECTION('ref_axis',(0.,-1.,0.));
#67702=DIRECTION('',(0.,-1.,0.));
#67703=DIRECTION('',(0.,0.,-1.));
#67704=DIRECTION('',(0.,-1.,0.));
#67705=DIRECTION('center_axis',(0.,1.,0.));
#67706=DIRECTION('ref_axis',(1.,0.,0.));
#67707=DIRECTION('',(1.,0.,0.));
#67708=DIRECTION('',(0.,0.,-1.));
#67709=DIRECTION('',(1.,0.,0.));
#67710=DIRECTION('center_axis',(-1.,0.,0.));
#67711=DIRECTION('ref_axis',(0.,1.,0.));
#67712=DIRECTION('',(0.,1.,0.));
#67713=DIRECTION('',(0.,1.,0.));
#67714=DIRECTION('center_axis',(0.,0.,-1.));
#67715=DIRECTION('ref_axis',(-1.,0.,0.));
#67716=DIRECTION('center_axis',(0.,-1.,0.));
#67717=DIRECTION('ref_axis',(-1.,0.,0.));
#67718=DIRECTION('',(-1.,0.,0.));
#67719=DIRECTION('',(0.,0.,-1.));
#67720=DIRECTION('',(-1.,0.,0.));
#67721=DIRECTION('',(0.,0.,-1.));
#67722=DIRECTION('center_axis',(1.,0.,0.));
#67723=DIRECTION('ref_axis',(0.,-1.,0.));
#67724=DIRECTION('',(0.,-1.,0.));
#67725=DIRECTION('',(0.,0.,-1.));
#67726=DIRECTION('',(0.,-1.,0.));
#67727=DIRECTION('center_axis',(0.,1.,0.));
#67728=DIRECTION('ref_axis',(1.,0.,0.));
#67729=DIRECTION('',(1.,0.,0.));
#67730=DIRECTION('',(0.,0.,-1.));
#67731=DIRECTION('',(1.,0.,0.));
#67732=DIRECTION('center_axis',(-1.,0.,0.));
#67733=DIRECTION('ref_axis',(0.,1.,0.));
#67734=DIRECTION('',(0.,1.,0.));
#67735=DIRECTION('',(0.,1.,0.));
#67736=DIRECTION('center_axis',(0.,0.,-1.));
#67737=DIRECTION('ref_axis',(-1.,0.,0.));
#67738=DIRECTION('center_axis',(0.,-1.,0.));
#67739=DIRECTION('ref_axis',(-1.,0.,0.));
#67740=DIRECTION('',(-1.,0.,0.));
#67741=DIRECTION('',(0.,0.,-1.));
#67742=DIRECTION('',(-1.,0.,0.));
#67743=DIRECTION('',(0.,0.,-1.));
#67744=DIRECTION('center_axis',(1.,0.,0.));
#67745=DIRECTION('ref_axis',(0.,-1.,0.));
#67746=DIRECTION('',(0.,-1.,0.));
#67747=DIRECTION('',(0.,0.,-1.));
#67748=DIRECTION('',(0.,-1.,0.));
#67749=DIRECTION('center_axis',(0.,1.,0.));
#67750=DIRECTION('ref_axis',(1.,0.,0.));
#67751=DIRECTION('',(1.,0.,0.));
#67752=DIRECTION('',(0.,0.,-1.));
#67753=DIRECTION('',(1.,0.,0.));
#67754=DIRECTION('center_axis',(-1.,0.,0.));
#67755=DIRECTION('ref_axis',(0.,1.,0.));
#67756=DIRECTION('',(0.,1.,0.));
#67757=DIRECTION('',(0.,1.,0.));
#67758=DIRECTION('center_axis',(0.,0.,-1.));
#67759=DIRECTION('ref_axis',(-1.,0.,0.));
#67760=DIRECTION('center_axis',(0.,-1.,0.));
#67761=DIRECTION('ref_axis',(-1.,0.,0.));
#67762=DIRECTION('',(-1.,0.,0.));
#67763=DIRECTION('',(0.,0.,-1.));
#67764=DIRECTION('',(-1.,0.,0.));
#67765=DIRECTION('',(0.,0.,-1.));
#67766=DIRECTION('center_axis',(1.,0.,0.));
#67767=DIRECTION('ref_axis',(0.,-1.,0.));
#67768=DIRECTION('',(0.,-1.,0.));
#67769=DIRECTION('',(0.,0.,-1.));
#67770=DIRECTION('',(0.,-1.,0.));
#67771=DIRECTION('center_axis',(0.,1.,0.));
#67772=DIRECTION('ref_axis',(1.,0.,0.));
#67773=DIRECTION('',(1.,0.,0.));
#67774=DIRECTION('',(0.,0.,-1.));
#67775=DIRECTION('',(1.,0.,0.));
#67776=DIRECTION('center_axis',(-1.,0.,0.));
#67777=DIRECTION('ref_axis',(0.,1.,0.));
#67778=DIRECTION('',(0.,1.,0.));
#67779=DIRECTION('',(0.,1.,0.));
#67780=DIRECTION('center_axis',(0.,0.,-1.));
#67781=DIRECTION('ref_axis',(-1.,0.,0.));
#67782=DIRECTION('center_axis',(0.,-1.,0.));
#67783=DIRECTION('ref_axis',(-1.,0.,0.));
#67784=DIRECTION('',(-1.,0.,0.));
#67785=DIRECTION('',(0.,0.,-1.));
#67786=DIRECTION('',(-1.,0.,0.));
#67787=DIRECTION('',(0.,0.,-1.));
#67788=DIRECTION('center_axis',(1.,0.,0.));
#67789=DIRECTION('ref_axis',(0.,-1.,0.));
#67790=DIRECTION('',(0.,-1.,0.));
#67791=DIRECTION('',(0.,0.,-1.));
#67792=DIRECTION('',(0.,-1.,0.));
#67793=DIRECTION('center_axis',(0.,1.,0.));
#67794=DIRECTION('ref_axis',(1.,0.,0.));
#67795=DIRECTION('',(1.,0.,0.));
#67796=DIRECTION('',(0.,0.,-1.));
#67797=DIRECTION('',(1.,0.,0.));
#67798=DIRECTION('center_axis',(-1.,0.,0.));
#67799=DIRECTION('ref_axis',(0.,1.,0.));
#67800=DIRECTION('',(0.,1.,0.));
#67801=DIRECTION('',(0.,1.,0.));
#67802=DIRECTION('center_axis',(0.,0.,-1.));
#67803=DIRECTION('ref_axis',(-1.,0.,0.));
#67804=DIRECTION('center_axis',(0.,-1.,0.));
#67805=DIRECTION('ref_axis',(-1.,0.,0.));
#67806=DIRECTION('',(-1.,0.,0.));
#67807=DIRECTION('',(0.,0.,-1.));
#67808=DIRECTION('',(-1.,0.,0.));
#67809=DIRECTION('',(0.,0.,-1.));
#67810=DIRECTION('center_axis',(1.,0.,0.));
#67811=DIRECTION('ref_axis',(0.,-1.,0.));
#67812=DIRECTION('',(0.,-1.,0.));
#67813=DIRECTION('',(0.,0.,-1.));
#67814=DIRECTION('',(0.,-1.,0.));
#67815=DIRECTION('center_axis',(0.,1.,0.));
#67816=DIRECTION('ref_axis',(1.,0.,0.));
#67817=DIRECTION('',(1.,0.,0.));
#67818=DIRECTION('',(0.,0.,-1.));
#67819=DIRECTION('',(1.,0.,0.));
#67820=DIRECTION('center_axis',(-1.,0.,0.));
#67821=DIRECTION('ref_axis',(0.,1.,0.));
#67822=DIRECTION('',(0.,1.,0.));
#67823=DIRECTION('',(0.,1.,0.));
#67824=DIRECTION('center_axis',(0.,0.,-1.));
#67825=DIRECTION('ref_axis',(-1.,0.,0.));
#67826=DIRECTION('center_axis',(0.,-1.,0.));
#67827=DIRECTION('ref_axis',(-1.,0.,0.));
#67828=DIRECTION('',(-1.,0.,0.));
#67829=DIRECTION('',(0.,0.,-1.));
#67830=DIRECTION('',(-1.,0.,0.));
#67831=DIRECTION('',(0.,0.,-1.));
#67832=DIRECTION('center_axis',(1.,0.,0.));
#67833=DIRECTION('ref_axis',(0.,-1.,0.));
#67834=DIRECTION('',(0.,-1.,0.));
#67835=DIRECTION('',(0.,0.,-1.));
#67836=DIRECTION('',(0.,-1.,0.));
#67837=DIRECTION('center_axis',(0.,1.,0.));
#67838=DIRECTION('ref_axis',(1.,0.,0.));
#67839=DIRECTION('',(1.,0.,0.));
#67840=DIRECTION('',(0.,0.,-1.));
#67841=DIRECTION('',(1.,0.,0.));
#67842=DIRECTION('center_axis',(-1.,0.,0.));
#67843=DIRECTION('ref_axis',(0.,1.,0.));
#67844=DIRECTION('',(0.,1.,0.));
#67845=DIRECTION('',(0.,1.,0.));
#67846=DIRECTION('center_axis',(0.,0.,-1.));
#67847=DIRECTION('ref_axis',(-1.,0.,0.));
#67848=DIRECTION('center_axis',(0.,-1.,0.));
#67849=DIRECTION('ref_axis',(-1.,0.,0.));
#67850=DIRECTION('',(-1.,0.,0.));
#67851=DIRECTION('',(0.,0.,-1.));
#67852=DIRECTION('',(-1.,0.,0.));
#67853=DIRECTION('',(0.,0.,-1.));
#67854=DIRECTION('center_axis',(1.,0.,0.));
#67855=DIRECTION('ref_axis',(0.,-1.,0.));
#67856=DIRECTION('',(0.,-1.,0.));
#67857=DIRECTION('',(0.,0.,-1.));
#67858=DIRECTION('',(0.,-1.,0.));
#67859=DIRECTION('center_axis',(0.,1.,0.));
#67860=DIRECTION('ref_axis',(1.,0.,0.));
#67861=DIRECTION('',(1.,0.,0.));
#67862=DIRECTION('',(0.,0.,-1.));
#67863=DIRECTION('',(1.,0.,0.));
#67864=DIRECTION('center_axis',(-1.,0.,0.));
#67865=DIRECTION('ref_axis',(0.,1.,0.));
#67866=DIRECTION('',(0.,1.,0.));
#67867=DIRECTION('',(0.,1.,0.));
#67868=DIRECTION('center_axis',(0.,0.,-1.));
#67869=DIRECTION('ref_axis',(-1.,0.,0.));
#67870=DIRECTION('center_axis',(0.,-1.,0.));
#67871=DIRECTION('ref_axis',(-1.,0.,0.));
#67872=DIRECTION('',(-1.,0.,0.));
#67873=DIRECTION('',(0.,0.,-1.));
#67874=DIRECTION('',(-1.,0.,0.));
#67875=DIRECTION('',(0.,0.,-1.));
#67876=DIRECTION('center_axis',(1.,0.,0.));
#67877=DIRECTION('ref_axis',(0.,-1.,0.));
#67878=DIRECTION('',(0.,-1.,0.));
#67879=DIRECTION('',(0.,0.,-1.));
#67880=DIRECTION('',(0.,-1.,0.));
#67881=DIRECTION('center_axis',(0.,1.,0.));
#67882=DIRECTION('ref_axis',(1.,0.,0.));
#67883=DIRECTION('',(1.,0.,0.));
#67884=DIRECTION('',(0.,0.,-1.));
#67885=DIRECTION('',(1.,0.,0.));
#67886=DIRECTION('center_axis',(-1.,0.,0.));
#67887=DIRECTION('ref_axis',(0.,1.,0.));
#67888=DIRECTION('',(0.,1.,0.));
#67889=DIRECTION('',(0.,1.,0.));
#67890=DIRECTION('center_axis',(0.,0.,-1.));
#67891=DIRECTION('ref_axis',(-1.,0.,0.));
#67892=DIRECTION('center_axis',(0.,-1.,0.));
#67893=DIRECTION('ref_axis',(-1.,0.,0.));
#67894=DIRECTION('',(-1.,0.,0.));
#67895=DIRECTION('',(0.,0.,-1.));
#67896=DIRECTION('',(-1.,0.,0.));
#67897=DIRECTION('',(0.,0.,-1.));
#67898=DIRECTION('center_axis',(1.,0.,0.));
#67899=DIRECTION('ref_axis',(0.,-1.,0.));
#67900=DIRECTION('',(0.,-1.,0.));
#67901=DIRECTION('',(0.,0.,-1.));
#67902=DIRECTION('',(0.,-1.,0.));
#67903=DIRECTION('center_axis',(0.,1.,0.));
#67904=DIRECTION('ref_axis',(1.,0.,0.));
#67905=DIRECTION('',(1.,0.,0.));
#67906=DIRECTION('',(0.,0.,-1.));
#67907=DIRECTION('',(1.,0.,0.));
#67908=DIRECTION('center_axis',(-1.,0.,0.));
#67909=DIRECTION('ref_axis',(0.,1.,0.));
#67910=DIRECTION('',(0.,1.,0.));
#67911=DIRECTION('',(0.,1.,0.));
#67912=DIRECTION('center_axis',(0.,0.,-1.));
#67913=DIRECTION('ref_axis',(-1.,0.,0.));
#67914=DIRECTION('center_axis',(0.,-1.,0.));
#67915=DIRECTION('ref_axis',(-1.,0.,0.));
#67916=DIRECTION('',(-1.,0.,0.));
#67917=DIRECTION('',(0.,0.,-1.));
#67918=DIRECTION('',(-1.,0.,0.));
#67919=DIRECTION('',(0.,0.,-1.));
#67920=DIRECTION('center_axis',(1.,0.,0.));
#67921=DIRECTION('ref_axis',(0.,-1.,0.));
#67922=DIRECTION('',(0.,-1.,0.));
#67923=DIRECTION('',(0.,0.,-1.));
#67924=DIRECTION('',(0.,-1.,0.));
#67925=DIRECTION('center_axis',(0.,1.,0.));
#67926=DIRECTION('ref_axis',(1.,0.,0.));
#67927=DIRECTION('',(1.,0.,0.));
#67928=DIRECTION('',(0.,0.,-1.));
#67929=DIRECTION('',(1.,0.,0.));
#67930=DIRECTION('center_axis',(-1.,0.,0.));
#67931=DIRECTION('ref_axis',(0.,1.,0.));
#67932=DIRECTION('',(0.,1.,0.));
#67933=DIRECTION('',(0.,1.,0.));
#67934=DIRECTION('center_axis',(0.,0.,-1.));
#67935=DIRECTION('ref_axis',(-1.,0.,0.));
#67936=DIRECTION('center_axis',(0.,-1.,0.));
#67937=DIRECTION('ref_axis',(-1.,0.,0.));
#67938=DIRECTION('',(-1.,0.,0.));
#67939=DIRECTION('',(0.,0.,-1.));
#67940=DIRECTION('',(-1.,0.,0.));
#67941=DIRECTION('',(0.,0.,-1.));
#67942=DIRECTION('center_axis',(1.,0.,0.));
#67943=DIRECTION('ref_axis',(0.,-1.,0.));
#67944=DIRECTION('',(0.,-1.,0.));
#67945=DIRECTION('',(0.,0.,-1.));
#67946=DIRECTION('',(0.,-1.,0.));
#67947=DIRECTION('center_axis',(0.,1.,0.));
#67948=DIRECTION('ref_axis',(1.,0.,0.));
#67949=DIRECTION('',(1.,0.,0.));
#67950=DIRECTION('',(0.,0.,-1.));
#67951=DIRECTION('',(1.,0.,0.));
#67952=DIRECTION('center_axis',(-1.,0.,0.));
#67953=DIRECTION('ref_axis',(0.,1.,0.));
#67954=DIRECTION('',(0.,1.,0.));
#67955=DIRECTION('',(0.,1.,0.));
#67956=DIRECTION('center_axis',(0.,0.,-1.));
#67957=DIRECTION('ref_axis',(-1.,0.,0.));
#67958=DIRECTION('center_axis',(0.,-1.,0.));
#67959=DIRECTION('ref_axis',(-1.,0.,0.));
#67960=DIRECTION('',(-1.,0.,0.));
#67961=DIRECTION('',(0.,0.,-1.));
#67962=DIRECTION('',(-1.,0.,0.));
#67963=DIRECTION('',(0.,0.,-1.));
#67964=DIRECTION('center_axis',(1.,0.,0.));
#67965=DIRECTION('ref_axis',(0.,-1.,0.));
#67966=DIRECTION('',(0.,-1.,0.));
#67967=DIRECTION('',(0.,0.,-1.));
#67968=DIRECTION('',(0.,-1.,0.));
#67969=DIRECTION('center_axis',(0.,1.,0.));
#67970=DIRECTION('ref_axis',(1.,0.,0.));
#67971=DIRECTION('',(1.,0.,0.));
#67972=DIRECTION('',(0.,0.,-1.));
#67973=DIRECTION('',(1.,0.,0.));
#67974=DIRECTION('center_axis',(-1.,0.,0.));
#67975=DIRECTION('ref_axis',(0.,1.,0.));
#67976=DIRECTION('',(0.,1.,0.));
#67977=DIRECTION('',(0.,1.,0.));
#67978=DIRECTION('center_axis',(0.,0.,-1.));
#67979=DIRECTION('ref_axis',(-1.,0.,0.));
#67980=DIRECTION('center_axis',(0.,-1.,0.));
#67981=DIRECTION('ref_axis',(-1.,0.,0.));
#67982=DIRECTION('',(-1.,0.,0.));
#67983=DIRECTION('',(0.,0.,-1.));
#67984=DIRECTION('',(-1.,0.,0.));
#67985=DIRECTION('',(0.,0.,-1.));
#67986=DIRECTION('center_axis',(1.,0.,0.));
#67987=DIRECTION('ref_axis',(0.,-1.,0.));
#67988=DIRECTION('',(0.,-1.,0.));
#67989=DIRECTION('',(0.,0.,-1.));
#67990=DIRECTION('',(0.,-1.,0.));
#67991=DIRECTION('center_axis',(0.,1.,0.));
#67992=DIRECTION('ref_axis',(1.,0.,0.));
#67993=DIRECTION('',(1.,0.,0.));
#67994=DIRECTION('',(0.,0.,-1.));
#67995=DIRECTION('',(1.,0.,0.));
#67996=DIRECTION('center_axis',(-1.,0.,0.));
#67997=DIRECTION('ref_axis',(0.,1.,0.));
#67998=DIRECTION('',(0.,1.,0.));
#67999=DIRECTION('',(0.,1.,0.));
#68000=DIRECTION('center_axis',(0.,0.,-1.));
#68001=DIRECTION('ref_axis',(-1.,0.,0.));
#68002=DIRECTION('center_axis',(0.,-1.,0.));
#68003=DIRECTION('ref_axis',(-1.,0.,0.));
#68004=DIRECTION('',(-1.,0.,0.));
#68005=DIRECTION('',(0.,0.,-1.));
#68006=DIRECTION('',(-1.,0.,0.));
#68007=DIRECTION('',(0.,0.,-1.));
#68008=DIRECTION('center_axis',(1.,0.,0.));
#68009=DIRECTION('ref_axis',(0.,-1.,0.));
#68010=DIRECTION('',(0.,-1.,0.));
#68011=DIRECTION('',(0.,0.,-1.));
#68012=DIRECTION('',(0.,-1.,0.));
#68013=DIRECTION('center_axis',(0.,1.,0.));
#68014=DIRECTION('ref_axis',(1.,0.,0.));
#68015=DIRECTION('',(1.,0.,0.));
#68016=DIRECTION('',(0.,0.,-1.));
#68017=DIRECTION('',(1.,0.,0.));
#68018=DIRECTION('center_axis',(-1.,0.,0.));
#68019=DIRECTION('ref_axis',(0.,1.,0.));
#68020=DIRECTION('',(0.,1.,0.));
#68021=DIRECTION('',(0.,1.,0.));
#68022=DIRECTION('center_axis',(0.,0.,-1.));
#68023=DIRECTION('ref_axis',(-1.,0.,0.));
#68024=DIRECTION('center_axis',(0.,-1.,0.));
#68025=DIRECTION('ref_axis',(-1.,0.,0.));
#68026=DIRECTION('',(-1.,0.,0.));
#68027=DIRECTION('',(0.,0.,-1.));
#68028=DIRECTION('',(-1.,0.,0.));
#68029=DIRECTION('',(0.,0.,-1.));
#68030=DIRECTION('center_axis',(1.,0.,0.));
#68031=DIRECTION('ref_axis',(0.,-1.,0.));
#68032=DIRECTION('',(0.,-1.,0.));
#68033=DIRECTION('',(0.,0.,-1.));
#68034=DIRECTION('',(0.,-1.,0.));
#68035=DIRECTION('center_axis',(0.,1.,0.));
#68036=DIRECTION('ref_axis',(1.,0.,0.));
#68037=DIRECTION('',(1.,0.,0.));
#68038=DIRECTION('',(0.,0.,-1.));
#68039=DIRECTION('',(1.,0.,0.));
#68040=DIRECTION('center_axis',(-1.,0.,0.));
#68041=DIRECTION('ref_axis',(0.,1.,0.));
#68042=DIRECTION('',(0.,1.,0.));
#68043=DIRECTION('',(0.,1.,0.));
#68044=DIRECTION('center_axis',(0.,0.,-1.));
#68045=DIRECTION('ref_axis',(-1.,0.,0.));
#68046=DIRECTION('center_axis',(0.,-1.,0.));
#68047=DIRECTION('ref_axis',(-1.,0.,0.));
#68048=DIRECTION('',(-1.,0.,0.));
#68049=DIRECTION('',(0.,0.,-1.));
#68050=DIRECTION('',(-1.,0.,0.));
#68051=DIRECTION('',(0.,0.,-1.));
#68052=DIRECTION('center_axis',(1.,0.,0.));
#68053=DIRECTION('ref_axis',(0.,-1.,0.));
#68054=DIRECTION('',(0.,-1.,0.));
#68055=DIRECTION('',(0.,0.,-1.));
#68056=DIRECTION('',(0.,-1.,0.));
#68057=DIRECTION('center_axis',(0.,1.,0.));
#68058=DIRECTION('ref_axis',(1.,0.,0.));
#68059=DIRECTION('',(1.,0.,0.));
#68060=DIRECTION('',(0.,0.,-1.));
#68061=DIRECTION('',(1.,0.,0.));
#68062=DIRECTION('center_axis',(-1.,0.,0.));
#68063=DIRECTION('ref_axis',(0.,1.,0.));
#68064=DIRECTION('',(0.,1.,0.));
#68065=DIRECTION('',(0.,1.,0.));
#68066=DIRECTION('center_axis',(0.,0.,-1.));
#68067=DIRECTION('ref_axis',(-1.,0.,0.));
#68068=DIRECTION('center_axis',(0.,-1.,0.));
#68069=DIRECTION('ref_axis',(-1.,0.,0.));
#68070=DIRECTION('',(-1.,0.,0.));
#68071=DIRECTION('',(0.,0.,-1.));
#68072=DIRECTION('',(-1.,0.,0.));
#68073=DIRECTION('',(0.,0.,-1.));
#68074=DIRECTION('center_axis',(1.,0.,0.));
#68075=DIRECTION('ref_axis',(0.,-1.,0.));
#68076=DIRECTION('',(0.,-1.,0.));
#68077=DIRECTION('',(0.,0.,-1.));
#68078=DIRECTION('',(0.,-1.,0.));
#68079=DIRECTION('center_axis',(0.,1.,0.));
#68080=DIRECTION('ref_axis',(1.,0.,0.));
#68081=DIRECTION('',(1.,0.,0.));
#68082=DIRECTION('',(0.,0.,-1.));
#68083=DIRECTION('',(1.,0.,0.));
#68084=DIRECTION('center_axis',(-1.,0.,0.));
#68085=DIRECTION('ref_axis',(0.,1.,0.));
#68086=DIRECTION('',(0.,1.,0.));
#68087=DIRECTION('',(0.,1.,0.));
#68088=DIRECTION('center_axis',(0.,0.,-1.));
#68089=DIRECTION('ref_axis',(-1.,0.,0.));
#68090=DIRECTION('center_axis',(0.,-1.,0.));
#68091=DIRECTION('ref_axis',(-1.,0.,0.));
#68092=DIRECTION('',(-1.,0.,0.));
#68093=DIRECTION('',(0.,0.,-1.));
#68094=DIRECTION('',(-1.,0.,0.));
#68095=DIRECTION('',(0.,0.,-1.));
#68096=DIRECTION('center_axis',(1.,0.,0.));
#68097=DIRECTION('ref_axis',(0.,-1.,0.));
#68098=DIRECTION('',(0.,-1.,0.));
#68099=DIRECTION('',(0.,0.,-1.));
#68100=DIRECTION('',(0.,-1.,0.));
#68101=DIRECTION('center_axis',(0.,1.,0.));
#68102=DIRECTION('ref_axis',(1.,0.,0.));
#68103=DIRECTION('',(1.,0.,0.));
#68104=DIRECTION('',(0.,0.,-1.));
#68105=DIRECTION('',(1.,0.,0.));
#68106=DIRECTION('center_axis',(-1.,0.,0.));
#68107=DIRECTION('ref_axis',(0.,1.,0.));
#68108=DIRECTION('',(0.,1.,0.));
#68109=DIRECTION('',(0.,1.,0.));
#68110=DIRECTION('center_axis',(0.,0.,-1.));
#68111=DIRECTION('ref_axis',(-1.,0.,0.));
#68112=DIRECTION('center_axis',(0.,-1.,0.));
#68113=DIRECTION('ref_axis',(-1.,0.,0.));
#68114=DIRECTION('',(-1.,0.,0.));
#68115=DIRECTION('',(0.,0.,-1.));
#68116=DIRECTION('',(-1.,0.,0.));
#68117=DIRECTION('',(0.,0.,-1.));
#68118=DIRECTION('center_axis',(1.,0.,0.));
#68119=DIRECTION('ref_axis',(0.,-1.,0.));
#68120=DIRECTION('',(0.,-1.,0.));
#68121=DIRECTION('',(0.,0.,-1.));
#68122=DIRECTION('',(0.,-1.,0.));
#68123=DIRECTION('center_axis',(0.,1.,0.));
#68124=DIRECTION('ref_axis',(1.,0.,0.));
#68125=DIRECTION('',(1.,0.,0.));
#68126=DIRECTION('',(0.,0.,-1.));
#68127=DIRECTION('',(1.,0.,0.));
#68128=DIRECTION('center_axis',(-1.,0.,0.));
#68129=DIRECTION('ref_axis',(0.,1.,0.));
#68130=DIRECTION('',(0.,1.,0.));
#68131=DIRECTION('',(0.,1.,0.));
#68132=DIRECTION('center_axis',(0.,0.,-1.));
#68133=DIRECTION('ref_axis',(-1.,0.,0.));
#68134=DIRECTION('center_axis',(0.,-1.,0.));
#68135=DIRECTION('ref_axis',(-1.,0.,0.));
#68136=DIRECTION('',(-1.,0.,0.));
#68137=DIRECTION('',(0.,0.,-1.));
#68138=DIRECTION('',(-1.,0.,0.));
#68139=DIRECTION('',(0.,0.,-1.));
#68140=DIRECTION('center_axis',(1.,0.,0.));
#68141=DIRECTION('ref_axis',(0.,-1.,0.));
#68142=DIRECTION('',(0.,-1.,0.));
#68143=DIRECTION('',(0.,0.,-1.));
#68144=DIRECTION('',(0.,-1.,0.));
#68145=DIRECTION('center_axis',(0.,1.,0.));
#68146=DIRECTION('ref_axis',(1.,0.,0.));
#68147=DIRECTION('',(1.,0.,0.));
#68148=DIRECTION('',(0.,0.,-1.));
#68149=DIRECTION('',(1.,0.,0.));
#68150=DIRECTION('center_axis',(-1.,0.,0.));
#68151=DIRECTION('ref_axis',(0.,1.,0.));
#68152=DIRECTION('',(0.,1.,0.));
#68153=DIRECTION('',(0.,1.,0.));
#68154=DIRECTION('center_axis',(0.,0.,-1.));
#68155=DIRECTION('ref_axis',(-1.,0.,0.));
#68156=DIRECTION('center_axis',(0.,-1.,0.));
#68157=DIRECTION('ref_axis',(-1.,0.,0.));
#68158=DIRECTION('',(-1.,0.,0.));
#68159=DIRECTION('',(0.,0.,-1.));
#68160=DIRECTION('',(-1.,0.,0.));
#68161=DIRECTION('',(0.,0.,-1.));
#68162=DIRECTION('center_axis',(1.,0.,0.));
#68163=DIRECTION('ref_axis',(0.,-1.,0.));
#68164=DIRECTION('',(0.,-1.,0.));
#68165=DIRECTION('',(0.,0.,-1.));
#68166=DIRECTION('',(0.,-1.,0.));
#68167=DIRECTION('center_axis',(0.,1.,0.));
#68168=DIRECTION('ref_axis',(1.,0.,0.));
#68169=DIRECTION('',(1.,0.,0.));
#68170=DIRECTION('',(0.,0.,-1.));
#68171=DIRECTION('',(1.,0.,0.));
#68172=DIRECTION('center_axis',(-1.,0.,0.));
#68173=DIRECTION('ref_axis',(0.,1.,0.));
#68174=DIRECTION('',(0.,1.,0.));
#68175=DIRECTION('',(0.,1.,0.));
#68176=DIRECTION('center_axis',(0.,0.,-1.));
#68177=DIRECTION('ref_axis',(-1.,0.,0.));
#68178=DIRECTION('center_axis',(0.,-1.,0.));
#68179=DIRECTION('ref_axis',(-1.,0.,0.));
#68180=DIRECTION('',(-1.,0.,0.));
#68181=DIRECTION('',(0.,0.,-1.));
#68182=DIRECTION('',(-1.,0.,0.));
#68183=DIRECTION('',(0.,0.,-1.));
#68184=DIRECTION('center_axis',(1.,0.,0.));
#68185=DIRECTION('ref_axis',(0.,-1.,0.));
#68186=DIRECTION('',(0.,-1.,0.));
#68187=DIRECTION('',(0.,0.,-1.));
#68188=DIRECTION('',(0.,-1.,0.));
#68189=DIRECTION('center_axis',(0.,1.,0.));
#68190=DIRECTION('ref_axis',(1.,0.,0.));
#68191=DIRECTION('',(1.,0.,0.));
#68192=DIRECTION('',(0.,0.,-1.));
#68193=DIRECTION('',(1.,0.,0.));
#68194=DIRECTION('center_axis',(-1.,0.,0.));
#68195=DIRECTION('ref_axis',(0.,1.,0.));
#68196=DIRECTION('',(0.,1.,0.));
#68197=DIRECTION('',(0.,1.,0.));
#68198=DIRECTION('center_axis',(0.,0.,-1.));
#68199=DIRECTION('ref_axis',(-1.,0.,0.));
#68200=DIRECTION('center_axis',(0.,-1.,0.));
#68201=DIRECTION('ref_axis',(-1.,0.,0.));
#68202=DIRECTION('',(-1.,0.,0.));
#68203=DIRECTION('',(0.,0.,-1.));
#68204=DIRECTION('',(-1.,0.,0.));
#68205=DIRECTION('',(0.,0.,-1.));
#68206=DIRECTION('center_axis',(1.,0.,0.));
#68207=DIRECTION('ref_axis',(0.,-1.,0.));
#68208=DIRECTION('',(0.,-1.,0.));
#68209=DIRECTION('',(0.,0.,-1.));
#68210=DIRECTION('',(0.,-1.,0.));
#68211=DIRECTION('center_axis',(0.,1.,0.));
#68212=DIRECTION('ref_axis',(1.,0.,0.));
#68213=DIRECTION('',(1.,0.,0.));
#68214=DIRECTION('',(0.,0.,-1.));
#68215=DIRECTION('',(1.,0.,0.));
#68216=DIRECTION('center_axis',(-1.,0.,0.));
#68217=DIRECTION('ref_axis',(0.,1.,0.));
#68218=DIRECTION('',(0.,1.,0.));
#68219=DIRECTION('',(0.,1.,0.));
#68220=DIRECTION('center_axis',(0.,0.,-1.));
#68221=DIRECTION('ref_axis',(-1.,0.,0.));
#68222=DIRECTION('center_axis',(0.,-1.,0.));
#68223=DIRECTION('ref_axis',(-1.,0.,0.));
#68224=DIRECTION('',(-1.,0.,0.));
#68225=DIRECTION('',(0.,0.,-1.));
#68226=DIRECTION('',(-1.,0.,0.));
#68227=DIRECTION('',(0.,0.,-1.));
#68228=DIRECTION('center_axis',(1.,0.,0.));
#68229=DIRECTION('ref_axis',(0.,-1.,0.));
#68230=DIRECTION('',(0.,-1.,0.));
#68231=DIRECTION('',(0.,0.,-1.));
#68232=DIRECTION('',(0.,-1.,0.));
#68233=DIRECTION('center_axis',(0.,1.,0.));
#68234=DIRECTION('ref_axis',(1.,0.,0.));
#68235=DIRECTION('',(1.,0.,0.));
#68236=DIRECTION('',(0.,0.,-1.));
#68237=DIRECTION('',(1.,0.,0.));
#68238=DIRECTION('center_axis',(-1.,0.,0.));
#68239=DIRECTION('ref_axis',(0.,1.,0.));
#68240=DIRECTION('',(0.,1.,0.));
#68241=DIRECTION('',(0.,1.,0.));
#68242=DIRECTION('center_axis',(0.,0.,-1.));
#68243=DIRECTION('ref_axis',(-1.,0.,0.));
#68244=DIRECTION('center_axis',(0.,-1.,0.));
#68245=DIRECTION('ref_axis',(-1.,0.,0.));
#68246=DIRECTION('',(-1.,0.,0.));
#68247=DIRECTION('',(0.,0.,-1.));
#68248=DIRECTION('',(-1.,0.,0.));
#68249=DIRECTION('',(0.,0.,-1.));
#68250=DIRECTION('center_axis',(1.,0.,0.));
#68251=DIRECTION('ref_axis',(0.,-1.,0.));
#68252=DIRECTION('',(0.,-1.,0.));
#68253=DIRECTION('',(0.,0.,-1.));
#68254=DIRECTION('',(0.,-1.,0.));
#68255=DIRECTION('center_axis',(0.,1.,0.));
#68256=DIRECTION('ref_axis',(1.,0.,0.));
#68257=DIRECTION('',(1.,0.,0.));
#68258=DIRECTION('',(0.,0.,-1.));
#68259=DIRECTION('',(1.,0.,0.));
#68260=DIRECTION('center_axis',(-1.,0.,0.));
#68261=DIRECTION('ref_axis',(0.,1.,0.));
#68262=DIRECTION('',(0.,1.,0.));
#68263=DIRECTION('',(0.,1.,0.));
#68264=DIRECTION('center_axis',(0.,0.,-1.));
#68265=DIRECTION('ref_axis',(-1.,0.,0.));
#68266=DIRECTION('center_axis',(0.,-1.,0.));
#68267=DIRECTION('ref_axis',(-1.,0.,0.));
#68268=DIRECTION('',(-1.,0.,0.));
#68269=DIRECTION('',(0.,0.,-1.));
#68270=DIRECTION('',(-1.,0.,0.));
#68271=DIRECTION('',(0.,0.,-1.));
#68272=DIRECTION('center_axis',(1.,0.,0.));
#68273=DIRECTION('ref_axis',(0.,-1.,0.));
#68274=DIRECTION('',(0.,-1.,0.));
#68275=DIRECTION('',(0.,0.,-1.));
#68276=DIRECTION('',(0.,-1.,0.));
#68277=DIRECTION('center_axis',(0.,1.,0.));
#68278=DIRECTION('ref_axis',(1.,0.,0.));
#68279=DIRECTION('',(1.,0.,0.));
#68280=DIRECTION('',(0.,0.,-1.));
#68281=DIRECTION('',(1.,0.,0.));
#68282=DIRECTION('center_axis',(-1.,0.,0.));
#68283=DIRECTION('ref_axis',(0.,1.,0.));
#68284=DIRECTION('',(0.,1.,0.));
#68285=DIRECTION('',(0.,1.,0.));
#68286=DIRECTION('center_axis',(0.,0.,-1.));
#68287=DIRECTION('ref_axis',(-1.,0.,0.));
#68288=DIRECTION('center_axis',(0.,-1.,0.));
#68289=DIRECTION('ref_axis',(-1.,0.,0.));
#68290=DIRECTION('',(-1.,0.,0.));
#68291=DIRECTION('',(0.,0.,-1.));
#68292=DIRECTION('',(-1.,0.,0.));
#68293=DIRECTION('',(0.,0.,-1.));
#68294=DIRECTION('center_axis',(1.,0.,0.));
#68295=DIRECTION('ref_axis',(0.,-1.,0.));
#68296=DIRECTION('',(0.,-1.,0.));
#68297=DIRECTION('',(0.,0.,-1.));
#68298=DIRECTION('',(0.,-1.,0.));
#68299=DIRECTION('center_axis',(0.,1.,0.));
#68300=DIRECTION('ref_axis',(1.,0.,0.));
#68301=DIRECTION('',(1.,0.,0.));
#68302=DIRECTION('',(0.,0.,-1.));
#68303=DIRECTION('',(1.,0.,0.));
#68304=DIRECTION('center_axis',(-1.,0.,0.));
#68305=DIRECTION('ref_axis',(0.,1.,0.));
#68306=DIRECTION('',(0.,1.,0.));
#68307=DIRECTION('',(0.,1.,0.));
#68308=DIRECTION('center_axis',(0.,0.,-1.));
#68309=DIRECTION('ref_axis',(-1.,0.,0.));
#68310=DIRECTION('center_axis',(0.,-1.,0.));
#68311=DIRECTION('ref_axis',(-1.,0.,0.));
#68312=DIRECTION('',(-1.,0.,0.));
#68313=DIRECTION('',(0.,0.,-1.));
#68314=DIRECTION('',(-1.,0.,0.));
#68315=DIRECTION('',(0.,0.,-1.));
#68316=DIRECTION('center_axis',(1.,0.,0.));
#68317=DIRECTION('ref_axis',(0.,-1.,0.));
#68318=DIRECTION('',(0.,-1.,0.));
#68319=DIRECTION('',(0.,0.,-1.));
#68320=DIRECTION('',(0.,-1.,0.));
#68321=DIRECTION('center_axis',(0.,1.,0.));
#68322=DIRECTION('ref_axis',(1.,0.,0.));
#68323=DIRECTION('',(1.,0.,0.));
#68324=DIRECTION('',(0.,0.,-1.));
#68325=DIRECTION('',(1.,0.,0.));
#68326=DIRECTION('center_axis',(-1.,0.,0.));
#68327=DIRECTION('ref_axis',(0.,1.,0.));
#68328=DIRECTION('',(0.,1.,0.));
#68329=DIRECTION('',(0.,1.,0.));
#68330=DIRECTION('center_axis',(0.,0.,-1.));
#68331=DIRECTION('ref_axis',(-1.,0.,0.));
#68332=DIRECTION('center_axis',(0.,-1.,0.));
#68333=DIRECTION('ref_axis',(-1.,0.,0.));
#68334=DIRECTION('',(-1.,0.,0.));
#68335=DIRECTION('',(0.,0.,-1.));
#68336=DIRECTION('',(-1.,0.,0.));
#68337=DIRECTION('',(0.,0.,-1.));
#68338=DIRECTION('center_axis',(1.,0.,0.));
#68339=DIRECTION('ref_axis',(0.,-1.,0.));
#68340=DIRECTION('',(0.,-1.,0.));
#68341=DIRECTION('',(0.,0.,-1.));
#68342=DIRECTION('',(0.,-1.,0.));
#68343=DIRECTION('center_axis',(0.,1.,0.));
#68344=DIRECTION('ref_axis',(1.,0.,0.));
#68345=DIRECTION('',(1.,0.,0.));
#68346=DIRECTION('',(0.,0.,-1.));
#68347=DIRECTION('',(1.,0.,0.));
#68348=DIRECTION('center_axis',(-1.,0.,0.));
#68349=DIRECTION('ref_axis',(0.,1.,0.));
#68350=DIRECTION('',(0.,1.,0.));
#68351=DIRECTION('',(0.,1.,0.));
#68352=DIRECTION('center_axis',(0.,0.,-1.));
#68353=DIRECTION('ref_axis',(-1.,0.,0.));
#68354=DIRECTION('center_axis',(0.,-1.,0.));
#68355=DIRECTION('ref_axis',(-1.,0.,0.));
#68356=DIRECTION('',(-1.,0.,0.));
#68357=DIRECTION('',(0.,0.,-1.));
#68358=DIRECTION('',(-1.,0.,0.));
#68359=DIRECTION('',(0.,0.,-1.));
#68360=DIRECTION('center_axis',(1.,0.,0.));
#68361=DIRECTION('ref_axis',(0.,-1.,0.));
#68362=DIRECTION('',(0.,-1.,0.));
#68363=DIRECTION('',(0.,0.,-1.));
#68364=DIRECTION('',(0.,-1.,0.));
#68365=DIRECTION('center_axis',(0.,1.,0.));
#68366=DIRECTION('ref_axis',(1.,0.,0.));
#68367=DIRECTION('',(1.,0.,0.));
#68368=DIRECTION('',(0.,0.,-1.));
#68369=DIRECTION('',(1.,0.,0.));
#68370=DIRECTION('center_axis',(-1.,0.,0.));
#68371=DIRECTION('ref_axis',(0.,1.,0.));
#68372=DIRECTION('',(0.,1.,0.));
#68373=DIRECTION('',(0.,1.,0.));
#68374=DIRECTION('center_axis',(0.,0.,-1.));
#68375=DIRECTION('ref_axis',(-1.,0.,0.));
#68376=DIRECTION('center_axis',(0.,-1.,0.));
#68377=DIRECTION('ref_axis',(-1.,0.,0.));
#68378=DIRECTION('',(-1.,0.,0.));
#68379=DIRECTION('',(0.,0.,-1.));
#68380=DIRECTION('',(-1.,0.,0.));
#68381=DIRECTION('',(0.,0.,-1.));
#68382=DIRECTION('center_axis',(1.,0.,0.));
#68383=DIRECTION('ref_axis',(0.,-1.,0.));
#68384=DIRECTION('',(0.,-1.,0.));
#68385=DIRECTION('',(0.,0.,-1.));
#68386=DIRECTION('',(0.,-1.,0.));
#68387=DIRECTION('center_axis',(0.,1.,0.));
#68388=DIRECTION('ref_axis',(1.,0.,0.));
#68389=DIRECTION('',(1.,0.,0.));
#68390=DIRECTION('',(0.,0.,-1.));
#68391=DIRECTION('',(1.,0.,0.));
#68392=DIRECTION('center_axis',(-1.,0.,0.));
#68393=DIRECTION('ref_axis',(0.,1.,0.));
#68394=DIRECTION('',(0.,1.,0.));
#68395=DIRECTION('',(0.,1.,0.));
#68396=DIRECTION('center_axis',(0.,0.,-1.));
#68397=DIRECTION('ref_axis',(-1.,0.,0.));
#68398=DIRECTION('center_axis',(0.,-1.,0.));
#68399=DIRECTION('ref_axis',(-1.,0.,0.));
#68400=DIRECTION('',(-1.,0.,0.));
#68401=DIRECTION('',(0.,0.,-1.));
#68402=DIRECTION('',(-1.,0.,0.));
#68403=DIRECTION('',(0.,0.,-1.));
#68404=DIRECTION('center_axis',(1.,0.,0.));
#68405=DIRECTION('ref_axis',(0.,-1.,0.));
#68406=DIRECTION('',(0.,-1.,0.));
#68407=DIRECTION('',(0.,0.,-1.));
#68408=DIRECTION('',(0.,-1.,0.));
#68409=DIRECTION('center_axis',(0.,1.,0.));
#68410=DIRECTION('ref_axis',(1.,0.,0.));
#68411=DIRECTION('',(1.,0.,0.));
#68412=DIRECTION('',(0.,0.,-1.));
#68413=DIRECTION('',(1.,0.,0.));
#68414=DIRECTION('center_axis',(-1.,0.,0.));
#68415=DIRECTION('ref_axis',(0.,1.,0.));
#68416=DIRECTION('',(0.,1.,0.));
#68417=DIRECTION('',(0.,1.,0.));
#68418=DIRECTION('center_axis',(0.,0.,-1.));
#68419=DIRECTION('ref_axis',(-1.,0.,0.));
#68420=DIRECTION('center_axis',(0.,-1.,0.));
#68421=DIRECTION('ref_axis',(-1.,0.,0.));
#68422=DIRECTION('',(-1.,0.,0.));
#68423=DIRECTION('',(0.,0.,-1.));
#68424=DIRECTION('',(-1.,0.,0.));
#68425=DIRECTION('',(0.,0.,-1.));
#68426=DIRECTION('center_axis',(1.,0.,0.));
#68427=DIRECTION('ref_axis',(0.,-1.,0.));
#68428=DIRECTION('',(0.,-1.,0.));
#68429=DIRECTION('',(0.,0.,-1.));
#68430=DIRECTION('',(0.,-1.,0.));
#68431=DIRECTION('center_axis',(0.,1.,0.));
#68432=DIRECTION('ref_axis',(1.,0.,0.));
#68433=DIRECTION('',(1.,0.,0.));
#68434=DIRECTION('',(0.,0.,-1.));
#68435=DIRECTION('',(1.,0.,0.));
#68436=DIRECTION('center_axis',(-1.,0.,0.));
#68437=DIRECTION('ref_axis',(0.,1.,0.));
#68438=DIRECTION('',(0.,1.,0.));
#68439=DIRECTION('',(0.,1.,0.));
#68440=DIRECTION('center_axis',(0.,0.,-1.));
#68441=DIRECTION('ref_axis',(-1.,0.,0.));
#68442=DIRECTION('center_axis',(0.,-1.,0.));
#68443=DIRECTION('ref_axis',(-1.,0.,0.));
#68444=DIRECTION('',(-1.,0.,0.));
#68445=DIRECTION('',(0.,0.,-1.));
#68446=DIRECTION('',(-1.,0.,0.));
#68447=DIRECTION('',(0.,0.,-1.));
#68448=DIRECTION('center_axis',(1.,0.,0.));
#68449=DIRECTION('ref_axis',(0.,-1.,0.));
#68450=DIRECTION('',(0.,-1.,0.));
#68451=DIRECTION('',(0.,0.,-1.));
#68452=DIRECTION('',(0.,-1.,0.));
#68453=DIRECTION('center_axis',(0.,1.,0.));
#68454=DIRECTION('ref_axis',(1.,0.,0.));
#68455=DIRECTION('',(1.,0.,0.));
#68456=DIRECTION('',(0.,0.,-1.));
#68457=DIRECTION('',(1.,0.,0.));
#68458=DIRECTION('center_axis',(-1.,0.,0.));
#68459=DIRECTION('ref_axis',(0.,1.,0.));
#68460=DIRECTION('',(0.,1.,0.));
#68461=DIRECTION('',(0.,1.,0.));
#68462=DIRECTION('center_axis',(0.,0.,-1.));
#68463=DIRECTION('ref_axis',(-1.,0.,0.));
#68464=DIRECTION('center_axis',(0.,-1.,0.));
#68465=DIRECTION('ref_axis',(-1.,0.,0.));
#68466=DIRECTION('',(-1.,0.,0.));
#68467=DIRECTION('',(0.,0.,-1.));
#68468=DIRECTION('',(-1.,0.,0.));
#68469=DIRECTION('',(0.,0.,-1.));
#68470=DIRECTION('center_axis',(1.,0.,0.));
#68471=DIRECTION('ref_axis',(0.,-1.,0.));
#68472=DIRECTION('',(0.,-1.,0.));
#68473=DIRECTION('',(0.,0.,-1.));
#68474=DIRECTION('',(0.,-1.,0.));
#68475=DIRECTION('center_axis',(0.,1.,0.));
#68476=DIRECTION('ref_axis',(1.,0.,0.));
#68477=DIRECTION('',(1.,0.,0.));
#68478=DIRECTION('',(0.,0.,-1.));
#68479=DIRECTION('',(1.,0.,0.));
#68480=DIRECTION('center_axis',(-1.,0.,0.));
#68481=DIRECTION('ref_axis',(0.,1.,0.));
#68482=DIRECTION('',(0.,1.,0.));
#68483=DIRECTION('',(0.,1.,0.));
#68484=DIRECTION('center_axis',(0.,0.,-1.));
#68485=DIRECTION('ref_axis',(-1.,0.,0.));
#68486=DIRECTION('center_axis',(0.,-1.,0.));
#68487=DIRECTION('ref_axis',(-1.,0.,0.));
#68488=DIRECTION('',(-1.,0.,0.));
#68489=DIRECTION('',(0.,0.,-1.));
#68490=DIRECTION('',(-1.,0.,0.));
#68491=DIRECTION('',(0.,0.,-1.));
#68492=DIRECTION('center_axis',(1.,0.,0.));
#68493=DIRECTION('ref_axis',(0.,-1.,0.));
#68494=DIRECTION('',(0.,-1.,0.));
#68495=DIRECTION('',(0.,0.,-1.));
#68496=DIRECTION('',(0.,-1.,0.));
#68497=DIRECTION('center_axis',(0.,1.,0.));
#68498=DIRECTION('ref_axis',(1.,0.,0.));
#68499=DIRECTION('',(1.,0.,0.));
#68500=DIRECTION('',(0.,0.,-1.));
#68501=DIRECTION('',(1.,0.,0.));
#68502=DIRECTION('center_axis',(-1.,0.,0.));
#68503=DIRECTION('ref_axis',(0.,1.,0.));
#68504=DIRECTION('',(0.,1.,0.));
#68505=DIRECTION('',(0.,1.,0.));
#68506=DIRECTION('center_axis',(0.,0.,-1.));
#68507=DIRECTION('ref_axis',(-1.,0.,0.));
#68508=DIRECTION('center_axis',(0.,-1.,0.));
#68509=DIRECTION('ref_axis',(-1.,0.,0.));
#68510=DIRECTION('',(-1.,0.,0.));
#68511=DIRECTION('',(0.,0.,-1.));
#68512=DIRECTION('',(-1.,0.,0.));
#68513=DIRECTION('',(0.,0.,-1.));
#68514=DIRECTION('center_axis',(1.,0.,0.));
#68515=DIRECTION('ref_axis',(0.,-1.,0.));
#68516=DIRECTION('',(0.,-1.,0.));
#68517=DIRECTION('',(0.,0.,-1.));
#68518=DIRECTION('',(0.,-1.,0.));
#68519=DIRECTION('center_axis',(0.,1.,0.));
#68520=DIRECTION('ref_axis',(1.,0.,0.));
#68521=DIRECTION('',(1.,0.,0.));
#68522=DIRECTION('',(0.,0.,-1.));
#68523=DIRECTION('',(1.,0.,0.));
#68524=DIRECTION('center_axis',(-1.,0.,0.));
#68525=DIRECTION('ref_axis',(0.,1.,0.));
#68526=DIRECTION('',(0.,1.,0.));
#68527=DIRECTION('',(0.,1.,0.));
#68528=DIRECTION('center_axis',(0.,0.,-1.));
#68529=DIRECTION('ref_axis',(-1.,0.,0.));
#68530=DIRECTION('center_axis',(0.,-1.,0.));
#68531=DIRECTION('ref_axis',(-1.,0.,0.));
#68532=DIRECTION('',(-1.,0.,0.));
#68533=DIRECTION('',(0.,0.,-1.));
#68534=DIRECTION('',(-1.,0.,0.));
#68535=DIRECTION('',(0.,0.,-1.));
#68536=DIRECTION('center_axis',(1.,0.,0.));
#68537=DIRECTION('ref_axis',(0.,-1.,0.));
#68538=DIRECTION('',(0.,-1.,0.));
#68539=DIRECTION('',(0.,0.,-1.));
#68540=DIRECTION('',(0.,-1.,0.));
#68541=DIRECTION('center_axis',(0.,1.,0.));
#68542=DIRECTION('ref_axis',(1.,0.,0.));
#68543=DIRECTION('',(1.,0.,0.));
#68544=DIRECTION('',(0.,0.,-1.));
#68545=DIRECTION('',(1.,0.,0.));
#68546=DIRECTION('center_axis',(-1.,0.,0.));
#68547=DIRECTION('ref_axis',(0.,1.,0.));
#68548=DIRECTION('',(0.,1.,0.));
#68549=DIRECTION('',(0.,1.,0.));
#68550=DIRECTION('center_axis',(0.,0.,-1.));
#68551=DIRECTION('ref_axis',(-1.,0.,0.));
#68552=DIRECTION('center_axis',(0.,-1.,0.));
#68553=DIRECTION('ref_axis',(-1.,0.,0.));
#68554=DIRECTION('',(-1.,0.,0.));
#68555=DIRECTION('',(0.,0.,-1.));
#68556=DIRECTION('',(-1.,0.,0.));
#68557=DIRECTION('',(0.,0.,-1.));
#68558=DIRECTION('center_axis',(1.,0.,0.));
#68559=DIRECTION('ref_axis',(0.,-1.,0.));
#68560=DIRECTION('',(0.,-1.,0.));
#68561=DIRECTION('',(0.,0.,-1.));
#68562=DIRECTION('',(0.,-1.,0.));
#68563=DIRECTION('center_axis',(0.,1.,0.));
#68564=DIRECTION('ref_axis',(1.,0.,0.));
#68565=DIRECTION('',(1.,0.,0.));
#68566=DIRECTION('',(0.,0.,-1.));
#68567=DIRECTION('',(1.,0.,0.));
#68568=DIRECTION('center_axis',(-1.,0.,0.));
#68569=DIRECTION('ref_axis',(0.,1.,0.));
#68570=DIRECTION('',(0.,1.,0.));
#68571=DIRECTION('',(0.,1.,0.));
#68572=DIRECTION('center_axis',(0.,0.,-1.));
#68573=DIRECTION('ref_axis',(-1.,0.,0.));
#68574=DIRECTION('center_axis',(0.,-1.,0.));
#68575=DIRECTION('ref_axis',(-1.,0.,0.));
#68576=DIRECTION('',(-1.,0.,0.));
#68577=DIRECTION('',(0.,0.,-1.));
#68578=DIRECTION('',(-1.,0.,0.));
#68579=DIRECTION('',(0.,0.,-1.));
#68580=DIRECTION('center_axis',(1.,0.,0.));
#68581=DIRECTION('ref_axis',(0.,-1.,0.));
#68582=DIRECTION('',(0.,-1.,0.));
#68583=DIRECTION('',(0.,0.,-1.));
#68584=DIRECTION('',(0.,-1.,0.));
#68585=DIRECTION('center_axis',(0.,1.,0.));
#68586=DIRECTION('ref_axis',(1.,0.,0.));
#68587=DIRECTION('',(1.,0.,0.));
#68588=DIRECTION('',(0.,0.,-1.));
#68589=DIRECTION('',(1.,0.,0.));
#68590=DIRECTION('center_axis',(-1.,0.,0.));
#68591=DIRECTION('ref_axis',(0.,1.,0.));
#68592=DIRECTION('',(0.,1.,0.));
#68593=DIRECTION('',(0.,1.,0.));
#68594=DIRECTION('center_axis',(0.,0.,-1.));
#68595=DIRECTION('ref_axis',(-1.,0.,0.));
#68596=DIRECTION('center_axis',(0.,-1.,0.));
#68597=DIRECTION('ref_axis',(-1.,0.,0.));
#68598=DIRECTION('',(-1.,0.,0.));
#68599=DIRECTION('',(0.,0.,-1.));
#68600=DIRECTION('',(-1.,0.,0.));
#68601=DIRECTION('',(0.,0.,-1.));
#68602=DIRECTION('center_axis',(1.,0.,0.));
#68603=DIRECTION('ref_axis',(0.,-1.,0.));
#68604=DIRECTION('',(0.,-1.,0.));
#68605=DIRECTION('',(0.,0.,-1.));
#68606=DIRECTION('',(0.,-1.,0.));
#68607=DIRECTION('center_axis',(0.,1.,0.));
#68608=DIRECTION('ref_axis',(1.,0.,0.));
#68609=DIRECTION('',(1.,0.,0.));
#68610=DIRECTION('',(0.,0.,-1.));
#68611=DIRECTION('',(1.,0.,0.));
#68612=DIRECTION('center_axis',(-1.,0.,0.));
#68613=DIRECTION('ref_axis',(0.,1.,0.));
#68614=DIRECTION('',(0.,1.,0.));
#68615=DIRECTION('',(0.,1.,0.));
#68616=DIRECTION('center_axis',(0.,0.,-1.));
#68617=DIRECTION('ref_axis',(-1.,0.,0.));
#68618=DIRECTION('center_axis',(0.,-1.,0.));
#68619=DIRECTION('ref_axis',(-1.,0.,0.));
#68620=DIRECTION('',(-1.,0.,0.));
#68621=DIRECTION('',(0.,0.,-1.));
#68622=DIRECTION('',(-1.,0.,0.));
#68623=DIRECTION('',(0.,0.,-1.));
#68624=DIRECTION('center_axis',(1.,0.,0.));
#68625=DIRECTION('ref_axis',(0.,-1.,0.));
#68626=DIRECTION('',(0.,-1.,0.));
#68627=DIRECTION('',(0.,0.,-1.));
#68628=DIRECTION('',(0.,-1.,0.));
#68629=DIRECTION('center_axis',(0.,1.,0.));
#68630=DIRECTION('ref_axis',(1.,0.,0.));
#68631=DIRECTION('',(1.,0.,0.));
#68632=DIRECTION('',(0.,0.,-1.));
#68633=DIRECTION('',(1.,0.,0.));
#68634=DIRECTION('center_axis',(-1.,0.,0.));
#68635=DIRECTION('ref_axis',(0.,1.,0.));
#68636=DIRECTION('',(0.,1.,0.));
#68637=DIRECTION('',(0.,1.,0.));
#68638=DIRECTION('center_axis',(0.,0.,-1.));
#68639=DIRECTION('ref_axis',(-1.,0.,0.));
#68640=DIRECTION('center_axis',(0.,-1.,0.));
#68641=DIRECTION('ref_axis',(-1.,0.,0.));
#68642=DIRECTION('',(-1.,0.,0.));
#68643=DIRECTION('',(0.,0.,-1.));
#68644=DIRECTION('',(-1.,0.,0.));
#68645=DIRECTION('',(0.,0.,-1.));
#68646=DIRECTION('center_axis',(1.,0.,0.));
#68647=DIRECTION('ref_axis',(0.,-1.,0.));
#68648=DIRECTION('',(0.,-1.,0.));
#68649=DIRECTION('',(0.,0.,-1.));
#68650=DIRECTION('',(0.,-1.,0.));
#68651=DIRECTION('center_axis',(0.,1.,0.));
#68652=DIRECTION('ref_axis',(1.,0.,0.));
#68653=DIRECTION('',(1.,0.,0.));
#68654=DIRECTION('',(0.,0.,-1.));
#68655=DIRECTION('',(1.,0.,0.));
#68656=DIRECTION('center_axis',(-1.,0.,0.));
#68657=DIRECTION('ref_axis',(0.,1.,0.));
#68658=DIRECTION('',(0.,1.,0.));
#68659=DIRECTION('',(0.,1.,0.));
#68660=DIRECTION('center_axis',(0.,0.,-1.));
#68661=DIRECTION('ref_axis',(-1.,0.,0.));
#68662=DIRECTION('center_axis',(0.,-1.,0.));
#68663=DIRECTION('ref_axis',(-1.,0.,0.));
#68664=DIRECTION('',(-1.,0.,0.));
#68665=DIRECTION('',(0.,0.,-1.));
#68666=DIRECTION('',(-1.,0.,0.));
#68667=DIRECTION('',(0.,0.,-1.));
#68668=DIRECTION('center_axis',(1.,0.,0.));
#68669=DIRECTION('ref_axis',(0.,-1.,0.));
#68670=DIRECTION('',(0.,-1.,0.));
#68671=DIRECTION('',(0.,0.,-1.));
#68672=DIRECTION('',(0.,-1.,0.));
#68673=DIRECTION('center_axis',(0.,1.,0.));
#68674=DIRECTION('ref_axis',(1.,0.,0.));
#68675=DIRECTION('',(1.,0.,0.));
#68676=DIRECTION('',(0.,0.,-1.));
#68677=DIRECTION('',(1.,0.,0.));
#68678=DIRECTION('center_axis',(-1.,0.,0.));
#68679=DIRECTION('ref_axis',(0.,1.,0.));
#68680=DIRECTION('',(0.,1.,0.));
#68681=DIRECTION('',(0.,1.,0.));
#68682=DIRECTION('center_axis',(0.,0.,-1.));
#68683=DIRECTION('ref_axis',(-1.,0.,0.));
#68684=DIRECTION('center_axis',(0.,-1.,0.));
#68685=DIRECTION('ref_axis',(-1.,0.,0.));
#68686=DIRECTION('',(-1.,0.,0.));
#68687=DIRECTION('',(0.,0.,-1.));
#68688=DIRECTION('',(-1.,0.,0.));
#68689=DIRECTION('',(0.,0.,-1.));
#68690=DIRECTION('center_axis',(1.,0.,0.));
#68691=DIRECTION('ref_axis',(0.,-1.,0.));
#68692=DIRECTION('',(0.,-1.,0.));
#68693=DIRECTION('',(0.,0.,-1.));
#68694=DIRECTION('',(0.,-1.,0.));
#68695=DIRECTION('center_axis',(0.,1.,0.));
#68696=DIRECTION('ref_axis',(1.,0.,0.));
#68697=DIRECTION('',(1.,0.,0.));
#68698=DIRECTION('',(0.,0.,-1.));
#68699=DIRECTION('',(1.,0.,0.));
#68700=DIRECTION('center_axis',(-1.,0.,0.));
#68701=DIRECTION('ref_axis',(0.,1.,0.));
#68702=DIRECTION('',(0.,1.,0.));
#68703=DIRECTION('',(0.,1.,0.));
#68704=DIRECTION('center_axis',(0.,0.,-1.));
#68705=DIRECTION('ref_axis',(-1.,0.,0.));
#68706=DIRECTION('center_axis',(0.,-1.,0.));
#68707=DIRECTION('ref_axis',(-1.,0.,0.));
#68708=DIRECTION('',(-1.,0.,0.));
#68709=DIRECTION('',(0.,0.,-1.));
#68710=DIRECTION('',(-1.,0.,0.));
#68711=DIRECTION('',(0.,0.,-1.));
#68712=DIRECTION('center_axis',(1.,0.,0.));
#68713=DIRECTION('ref_axis',(0.,-1.,0.));
#68714=DIRECTION('',(0.,-1.,0.));
#68715=DIRECTION('',(0.,0.,-1.));
#68716=DIRECTION('',(0.,-1.,0.));
#68717=DIRECTION('center_axis',(0.,1.,0.));
#68718=DIRECTION('ref_axis',(1.,0.,0.));
#68719=DIRECTION('',(1.,0.,0.));
#68720=DIRECTION('',(0.,0.,-1.));
#68721=DIRECTION('',(1.,0.,0.));
#68722=DIRECTION('center_axis',(-1.,0.,0.));
#68723=DIRECTION('ref_axis',(0.,1.,0.));
#68724=DIRECTION('',(0.,1.,0.));
#68725=DIRECTION('',(0.,1.,0.));
#68726=DIRECTION('center_axis',(0.,0.,-1.));
#68727=DIRECTION('ref_axis',(-1.,0.,0.));
#68728=DIRECTION('center_axis',(0.,-1.,0.));
#68729=DIRECTION('ref_axis',(-1.,0.,0.));
#68730=DIRECTION('',(-1.,0.,0.));
#68731=DIRECTION('',(0.,0.,-1.));
#68732=DIRECTION('',(-1.,0.,0.));
#68733=DIRECTION('',(0.,0.,-1.));
#68734=DIRECTION('center_axis',(1.,0.,0.));
#68735=DIRECTION('ref_axis',(0.,-1.,0.));
#68736=DIRECTION('',(0.,-1.,0.));
#68737=DIRECTION('',(0.,0.,-1.));
#68738=DIRECTION('',(0.,-1.,0.));
#68739=DIRECTION('center_axis',(0.,1.,0.));
#68740=DIRECTION('ref_axis',(1.,0.,0.));
#68741=DIRECTION('',(1.,0.,0.));
#68742=DIRECTION('',(0.,0.,-1.));
#68743=DIRECTION('',(1.,0.,0.));
#68744=DIRECTION('center_axis',(-1.,0.,0.));
#68745=DIRECTION('ref_axis',(0.,1.,0.));
#68746=DIRECTION('',(0.,1.,0.));
#68747=DIRECTION('',(0.,1.,0.));
#68748=DIRECTION('center_axis',(0.,0.,-1.));
#68749=DIRECTION('ref_axis',(-1.,0.,0.));
#68750=DIRECTION('center_axis',(0.,-1.,0.));
#68751=DIRECTION('ref_axis',(-1.,0.,0.));
#68752=DIRECTION('',(-1.,0.,0.));
#68753=DIRECTION('',(0.,0.,-1.));
#68754=DIRECTION('',(-1.,0.,0.));
#68755=DIRECTION('',(0.,0.,-1.));
#68756=DIRECTION('center_axis',(1.,0.,0.));
#68757=DIRECTION('ref_axis',(0.,-1.,0.));
#68758=DIRECTION('',(0.,-1.,0.));
#68759=DIRECTION('',(0.,0.,-1.));
#68760=DIRECTION('',(0.,-1.,0.));
#68761=DIRECTION('center_axis',(0.,1.,0.));
#68762=DIRECTION('ref_axis',(1.,0.,0.));
#68763=DIRECTION('',(1.,0.,0.));
#68764=DIRECTION('',(0.,0.,-1.));
#68765=DIRECTION('',(1.,0.,0.));
#68766=DIRECTION('center_axis',(-1.,0.,0.));
#68767=DIRECTION('ref_axis',(0.,1.,0.));
#68768=DIRECTION('',(0.,1.,0.));
#68769=DIRECTION('',(0.,1.,0.));
#68770=DIRECTION('center_axis',(0.,0.,-1.));
#68771=DIRECTION('ref_axis',(-1.,0.,0.));
#68772=DIRECTION('center_axis',(0.,-1.,0.));
#68773=DIRECTION('ref_axis',(-1.,0.,0.));
#68774=DIRECTION('',(-1.,0.,0.));
#68775=DIRECTION('',(0.,0.,-1.));
#68776=DIRECTION('',(-1.,0.,0.));
#68777=DIRECTION('',(0.,0.,-1.));
#68778=DIRECTION('center_axis',(1.,0.,0.));
#68779=DIRECTION('ref_axis',(0.,-1.,0.));
#68780=DIRECTION('',(0.,-1.,0.));
#68781=DIRECTION('',(0.,0.,-1.));
#68782=DIRECTION('',(0.,-1.,0.));
#68783=DIRECTION('center_axis',(0.,1.,0.));
#68784=DIRECTION('ref_axis',(1.,0.,0.));
#68785=DIRECTION('',(1.,0.,0.));
#68786=DIRECTION('',(0.,0.,-1.));
#68787=DIRECTION('',(1.,0.,0.));
#68788=DIRECTION('center_axis',(-1.,0.,0.));
#68789=DIRECTION('ref_axis',(0.,1.,0.));
#68790=DIRECTION('',(0.,1.,0.));
#68791=DIRECTION('',(0.,1.,0.));
#68792=DIRECTION('center_axis',(0.,0.,-1.));
#68793=DIRECTION('ref_axis',(-1.,0.,0.));
#68794=DIRECTION('center_axis',(0.,-1.,0.));
#68795=DIRECTION('ref_axis',(-1.,0.,0.));
#68796=DIRECTION('',(-1.,0.,0.));
#68797=DIRECTION('',(0.,0.,-1.));
#68798=DIRECTION('',(-1.,0.,0.));
#68799=DIRECTION('',(0.,0.,-1.));
#68800=DIRECTION('center_axis',(1.,0.,0.));
#68801=DIRECTION('ref_axis',(0.,-1.,0.));
#68802=DIRECTION('',(0.,-1.,0.));
#68803=DIRECTION('',(0.,0.,-1.));
#68804=DIRECTION('',(0.,-1.,0.));
#68805=DIRECTION('center_axis',(0.,1.,0.));
#68806=DIRECTION('ref_axis',(1.,0.,0.));
#68807=DIRECTION('',(1.,0.,0.));
#68808=DIRECTION('',(0.,0.,-1.));
#68809=DIRECTION('',(1.,0.,0.));
#68810=DIRECTION('center_axis',(-1.,0.,0.));
#68811=DIRECTION('ref_axis',(0.,1.,0.));
#68812=DIRECTION('',(0.,1.,0.));
#68813=DIRECTION('',(0.,1.,0.));
#68814=DIRECTION('center_axis',(0.,0.,-1.));
#68815=DIRECTION('ref_axis',(-1.,0.,0.));
#68816=DIRECTION('center_axis',(0.,-1.,0.));
#68817=DIRECTION('ref_axis',(-1.,0.,0.));
#68818=DIRECTION('',(-1.,0.,0.));
#68819=DIRECTION('',(0.,0.,-1.));
#68820=DIRECTION('',(-1.,0.,0.));
#68821=DIRECTION('',(0.,0.,-1.));
#68822=DIRECTION('center_axis',(1.,0.,0.));
#68823=DIRECTION('ref_axis',(0.,-1.,0.));
#68824=DIRECTION('',(0.,-1.,0.));
#68825=DIRECTION('',(0.,0.,-1.));
#68826=DIRECTION('',(0.,-1.,0.));
#68827=DIRECTION('center_axis',(0.,1.,0.));
#68828=DIRECTION('ref_axis',(1.,0.,0.));
#68829=DIRECTION('',(1.,0.,0.));
#68830=DIRECTION('',(0.,0.,-1.));
#68831=DIRECTION('',(1.,0.,0.));
#68832=DIRECTION('center_axis',(-1.,0.,0.));
#68833=DIRECTION('ref_axis',(0.,1.,0.));
#68834=DIRECTION('',(0.,1.,0.));
#68835=DIRECTION('',(0.,1.,0.));
#68836=DIRECTION('center_axis',(0.,0.,-1.));
#68837=DIRECTION('ref_axis',(-1.,0.,0.));
#68838=DIRECTION('center_axis',(0.,-1.,0.));
#68839=DIRECTION('ref_axis',(-1.,0.,0.));
#68840=DIRECTION('',(-1.,0.,0.));
#68841=DIRECTION('',(0.,0.,-1.));
#68842=DIRECTION('',(-1.,0.,0.));
#68843=DIRECTION('',(0.,0.,-1.));
#68844=DIRECTION('center_axis',(1.,0.,0.));
#68845=DIRECTION('ref_axis',(0.,-1.,0.));
#68846=DIRECTION('',(0.,-1.,0.));
#68847=DIRECTION('',(0.,0.,-1.));
#68848=DIRECTION('',(0.,-1.,0.));
#68849=DIRECTION('center_axis',(0.,1.,0.));
#68850=DIRECTION('ref_axis',(1.,0.,0.));
#68851=DIRECTION('',(1.,0.,0.));
#68852=DIRECTION('',(0.,0.,-1.));
#68853=DIRECTION('',(1.,0.,0.));
#68854=DIRECTION('center_axis',(-1.,0.,0.));
#68855=DIRECTION('ref_axis',(0.,1.,0.));
#68856=DIRECTION('',(0.,1.,0.));
#68857=DIRECTION('',(0.,1.,0.));
#68858=DIRECTION('center_axis',(0.,0.,-1.));
#68859=DIRECTION('ref_axis',(-1.,0.,0.));
#68860=DIRECTION('center_axis',(0.,-1.,0.));
#68861=DIRECTION('ref_axis',(-1.,0.,0.));
#68862=DIRECTION('',(-1.,0.,0.));
#68863=DIRECTION('',(0.,0.,-1.));
#68864=DIRECTION('',(-1.,0.,0.));
#68865=DIRECTION('',(0.,0.,-1.));
#68866=DIRECTION('center_axis',(1.,0.,0.));
#68867=DIRECTION('ref_axis',(0.,-1.,0.));
#68868=DIRECTION('',(0.,-1.,0.));
#68869=DIRECTION('',(0.,0.,-1.));
#68870=DIRECTION('',(0.,-1.,0.));
#68871=DIRECTION('center_axis',(0.,1.,0.));
#68872=DIRECTION('ref_axis',(1.,0.,0.));
#68873=DIRECTION('',(1.,0.,0.));
#68874=DIRECTION('',(0.,0.,-1.));
#68875=DIRECTION('',(1.,0.,0.));
#68876=DIRECTION('center_axis',(-1.,0.,0.));
#68877=DIRECTION('ref_axis',(0.,1.,0.));
#68878=DIRECTION('',(0.,1.,0.));
#68879=DIRECTION('',(0.,1.,0.));
#68880=DIRECTION('center_axis',(0.,0.,-1.));
#68881=DIRECTION('ref_axis',(-1.,0.,0.));
#68882=DIRECTION('center_axis',(0.,-1.,0.));
#68883=DIRECTION('ref_axis',(-1.,0.,0.));
#68884=DIRECTION('',(-1.,0.,0.));
#68885=DIRECTION('',(0.,0.,-1.));
#68886=DIRECTION('',(-1.,0.,0.));
#68887=DIRECTION('',(0.,0.,-1.));
#68888=DIRECTION('center_axis',(1.,0.,0.));
#68889=DIRECTION('ref_axis',(0.,-1.,0.));
#68890=DIRECTION('',(0.,-1.,0.));
#68891=DIRECTION('',(0.,0.,-1.));
#68892=DIRECTION('',(0.,-1.,0.));
#68893=DIRECTION('center_axis',(0.,1.,0.));
#68894=DIRECTION('ref_axis',(1.,0.,0.));
#68895=DIRECTION('',(1.,0.,0.));
#68896=DIRECTION('',(0.,0.,-1.));
#68897=DIRECTION('',(1.,0.,0.));
#68898=DIRECTION('center_axis',(-1.,0.,0.));
#68899=DIRECTION('ref_axis',(0.,1.,0.));
#68900=DIRECTION('',(0.,1.,0.));
#68901=DIRECTION('',(0.,1.,0.));
#68902=DIRECTION('center_axis',(0.,0.,-1.));
#68903=DIRECTION('ref_axis',(-1.,0.,0.));
#68904=DIRECTION('center_axis',(0.,-1.,0.));
#68905=DIRECTION('ref_axis',(-1.,0.,0.));
#68906=DIRECTION('',(-1.,0.,0.));
#68907=DIRECTION('',(0.,0.,-1.));
#68908=DIRECTION('',(-1.,0.,0.));
#68909=DIRECTION('',(0.,0.,-1.));
#68910=DIRECTION('center_axis',(1.,0.,0.));
#68911=DIRECTION('ref_axis',(0.,-1.,0.));
#68912=DIRECTION('',(0.,-1.,0.));
#68913=DIRECTION('',(0.,0.,-1.));
#68914=DIRECTION('',(0.,-1.,0.));
#68915=DIRECTION('center_axis',(0.,1.,0.));
#68916=DIRECTION('ref_axis',(1.,0.,0.));
#68917=DIRECTION('',(1.,0.,0.));
#68918=DIRECTION('',(0.,0.,-1.));
#68919=DIRECTION('',(1.,0.,0.));
#68920=DIRECTION('center_axis',(-1.,0.,0.));
#68921=DIRECTION('ref_axis',(0.,1.,0.));
#68922=DIRECTION('',(0.,1.,0.));
#68923=DIRECTION('',(0.,1.,0.));
#68924=DIRECTION('center_axis',(0.,0.,-1.));
#68925=DIRECTION('ref_axis',(-1.,0.,0.));
#68926=DIRECTION('center_axis',(0.,-1.,0.));
#68927=DIRECTION('ref_axis',(-1.,0.,0.));
#68928=DIRECTION('',(-1.,0.,0.));
#68929=DIRECTION('',(0.,0.,-1.));
#68930=DIRECTION('',(-1.,0.,0.));
#68931=DIRECTION('',(0.,0.,-1.));
#68932=DIRECTION('center_axis',(1.,0.,0.));
#68933=DIRECTION('ref_axis',(0.,-1.,0.));
#68934=DIRECTION('',(0.,-1.,0.));
#68935=DIRECTION('',(0.,0.,-1.));
#68936=DIRECTION('',(0.,-1.,0.));
#68937=DIRECTION('center_axis',(0.,1.,0.));
#68938=DIRECTION('ref_axis',(1.,0.,0.));
#68939=DIRECTION('',(1.,0.,0.));
#68940=DIRECTION('',(0.,0.,-1.));
#68941=DIRECTION('',(1.,0.,0.));
#68942=DIRECTION('center_axis',(-1.,0.,0.));
#68943=DIRECTION('ref_axis',(0.,1.,0.));
#68944=DIRECTION('',(0.,1.,0.));
#68945=DIRECTION('',(0.,1.,0.));
#68946=DIRECTION('center_axis',(0.,0.,-1.));
#68947=DIRECTION('ref_axis',(-1.,0.,0.));
#68948=DIRECTION('center_axis',(0.,-1.,0.));
#68949=DIRECTION('ref_axis',(-1.,0.,0.));
#68950=DIRECTION('',(-1.,0.,0.));
#68951=DIRECTION('',(0.,0.,-1.));
#68952=DIRECTION('',(-1.,0.,0.));
#68953=DIRECTION('',(0.,0.,-1.));
#68954=DIRECTION('center_axis',(1.,0.,0.));
#68955=DIRECTION('ref_axis',(0.,-1.,0.));
#68956=DIRECTION('',(0.,-1.,0.));
#68957=DIRECTION('',(0.,0.,-1.));
#68958=DIRECTION('',(0.,-1.,0.));
#68959=DIRECTION('center_axis',(0.,1.,0.));
#68960=DIRECTION('ref_axis',(1.,0.,0.));
#68961=DIRECTION('',(1.,0.,0.));
#68962=DIRECTION('',(0.,0.,-1.));
#68963=DIRECTION('',(1.,0.,0.));
#68964=DIRECTION('center_axis',(-1.,0.,0.));
#68965=DIRECTION('ref_axis',(0.,1.,0.));
#68966=DIRECTION('',(0.,1.,0.));
#68967=DIRECTION('',(0.,1.,0.));
#68968=DIRECTION('center_axis',(0.,0.,-1.));
#68969=DIRECTION('ref_axis',(-1.,0.,0.));
#68970=DIRECTION('center_axis',(0.,-1.,0.));
#68971=DIRECTION('ref_axis',(-1.,0.,0.));
#68972=DIRECTION('',(-1.,0.,0.));
#68973=DIRECTION('',(0.,0.,-1.));
#68974=DIRECTION('',(-1.,0.,0.));
#68975=DIRECTION('',(0.,0.,-1.));
#68976=DIRECTION('center_axis',(1.,0.,0.));
#68977=DIRECTION('ref_axis',(0.,-1.,0.));
#68978=DIRECTION('',(0.,-1.,0.));
#68979=DIRECTION('',(0.,0.,-1.));
#68980=DIRECTION('',(0.,-1.,0.));
#68981=DIRECTION('center_axis',(0.,1.,0.));
#68982=DIRECTION('ref_axis',(1.,0.,0.));
#68983=DIRECTION('',(1.,0.,0.));
#68984=DIRECTION('',(0.,0.,-1.));
#68985=DIRECTION('',(1.,0.,0.));
#68986=DIRECTION('center_axis',(-1.,0.,0.));
#68987=DIRECTION('ref_axis',(0.,1.,0.));
#68988=DIRECTION('',(0.,1.,0.));
#68989=DIRECTION('',(0.,1.,0.));
#68990=DIRECTION('center_axis',(0.,0.,-1.));
#68991=DIRECTION('ref_axis',(-1.,0.,0.));
#68992=DIRECTION('center_axis',(0.,0.,-1.));
#68993=DIRECTION('ref_axis',(-1.,0.,0.));
#68994=DIRECTION('',(-0.707106781186561,-0.707106781186534,0.));
#68995=DIRECTION('',(0.,-1.,0.));
#68996=DIRECTION('',(-1.,0.,0.));
#68997=DIRECTION('',(0.,1.,0.));
#68998=DIRECTION('',(-0.707106781186548,0.707106781186548,0.));
#68999=DIRECTION('',(-1.,0.,0.));
#69000=DIRECTION('center_axis',(0.,0.,1.));
#69001=DIRECTION('ref_axis',(1.,0.,0.));
#69002=DIRECTION('',(0.707106781186561,0.707106781186534,0.));
#69003=DIRECTION('',(1.,0.,0.));
#69004=DIRECTION('',(0.707106781186548,-0.707106781186548,0.));
#69005=DIRECTION('',(0.,-1.,0.));
#69006=DIRECTION('',(1.,0.,0.));
#69007=DIRECTION('',(0.,1.,0.));
#69008=DIRECTION('center_axis',(0.,1.,0.));
#69009=DIRECTION('ref_axis',(0.,0.,1.));
#69010=DIRECTION('',(0.,0.,1.));
#69011=DIRECTION('',(0.,0.,-1.));
#69012=DIRECTION('center_axis',(1.,0.,0.));
#69013=DIRECTION('ref_axis',(0.,0.,-1.));
#69014=DIRECTION('',(0.,0.,-1.));
#69015=DIRECTION('',(0.,-0.707106781186542,-0.707106781186553));
#69016=DIRECTION('',(0.,-1.,0.));
#69017=DIRECTION('',(0.,-0.707106781186549,0.707106781186546));
#69018=DIRECTION('',(0.,0.,1.));
#69019=DIRECTION('center_axis',(1.,0.,0.));
#69020=DIRECTION('ref_axis',(0.,0.,-1.));
#69021=DIRECTION('',(0.,-0.866025403784439,-0.499999999999999));
#69022=DIRECTION('',(0.,-0.866025403784432,0.500000000000012));
#69023=DIRECTION('',(0.,0.,1.));
#69024=DIRECTION('',(0.,1.,0.));
#69025=DIRECTION('',(0.,0.,1.));
#69026=DIRECTION('',(0.,-1.,0.));
#69027=DIRECTION('',(0.,0.,1.));
#69028=DIRECTION('',(0.,0.86602540378444,0.499999999999997));
#69029=DIRECTION('',(0.,0.866025403784439,-0.5));
#69030=DIRECTION('center_axis',(1.,0.,0.));
#69031=DIRECTION('ref_axis',(0.,0.,-1.));
#69032=DIRECTION('',(0.,0.,1.));
#69033=DIRECTION('',(0.,0.707106781186548,0.707106781186547));
#69034=DIRECTION('',(0.,1.,0.));
#69035=DIRECTION('',(0.,0.707106781186548,-0.707106781186547));
#69036=DIRECTION('',(0.,0.,-1.));
#69037=DIRECTION('center_axis',(0.707106781186534,-0.707106781186561,0.));
#69038=DIRECTION('ref_axis',(0.,0.,-1.));
#69039=DIRECTION('',(0.,0.,1.));
#69040=DIRECTION('',(-0.678598344545862,-0.678598344545838,0.281084637714804));
#69041=DIRECTION('',(0.,0.,-1.));
#69042=DIRECTION('center_axis',(0.707106781186534,-0.707106781186561,0.));
#69043=DIRECTION('ref_axis',(0.,0.,-1.));
#69044=DIRECTION('',(0.,0.,-1.));
#69045=DIRECTION('',(-0.678598344545863,-0.678598344545837,-0.281084637714805));
#69046=DIRECTION('',(0.,0.,1.));
#69047=DIRECTION('center_axis',(-0.707106781186548,-0.707106781186548,0.));
#69048=DIRECTION('ref_axis',(0.,0.,1.));
#69049=DIRECTION('',(0.,0.,1.));
#69050=DIRECTION('',(0.678598344545849,-0.678598344545849,0.28108463771481));
#69051=DIRECTION('center_axis',(0.,-1.,0.));
#69052=DIRECTION('ref_axis',(0.,0.,-1.));
#69053=DIRECTION('',(1.,0.,0.));
#69054=DIRECTION('center_axis',(0.,-1.,0.));
#69055=DIRECTION('ref_axis',(1.,0.,0.));
#69056=DIRECTION('center_axis',(0.,-1.,0.));
#69057=DIRECTION('ref_axis',(1.,0.,0.));
#69058=DIRECTION('center_axis',(0.,-1.,0.));
#69059=DIRECTION('ref_axis',(1.,0.,0.));
#69060=DIRECTION('center_axis',(0.,1.,0.));
#69061=DIRECTION('ref_axis',(1.,0.,0.));
#69062=DIRECTION('center_axis',(0.,-1.,0.));
#69063=DIRECTION('ref_axis',(1.,0.,0.));
#69064=DIRECTION('',(0.857167300702107,-0.515038074910062,1.04972719113861E-16));
#69065=DIRECTION('center_axis',(0.,1.,0.));
#69066=DIRECTION('ref_axis',(1.,0.,0.));
#69067=DIRECTION('center_axis',(0.,-1.,0.));
#69068=DIRECTION('ref_axis',(1.,0.,0.));
#69069=DIRECTION('',(0.857167300702112,-0.515038074910054,1.04972719113862E-16));
#69070=DIRECTION('center_axis',(0.,-1.,0.));
#69071=DIRECTION('ref_axis',(1.,0.,0.));
#69072=DIRECTION('center_axis',(0.,-1.,0.));
#69073=DIRECTION('ref_axis',(1.,0.,0.));
#69074=DIRECTION('',(0.,-1.,0.));
#69075=DIRECTION('center_axis',(0.,-1.,0.));
#69076=DIRECTION('ref_axis',(1.,0.,0.));
#69077=DIRECTION('center_axis',(0.,-1.,0.));
#69078=DIRECTION('ref_axis',(1.,0.,0.));
#69079=DIRECTION('',(0.,-1.,0.));
#69080=DIRECTION('center_axis',(0.,1.,0.));
#69081=DIRECTION('ref_axis',(1.,0.,0.));
#69082=DIRECTION('center_axis',(0.,1.,0.));
#69083=DIRECTION('ref_axis',(1.,0.,0.));
#69084=DIRECTION('',(0.70710678118654,-0.707106781186555,-8.65956056235483E-17));
#69085=DIRECTION('center_axis',(0.,-1.,0.));
#69086=DIRECTION('ref_axis',(1.,0.,0.));
#69087=DIRECTION('center_axis',(0.,-1.,0.));
#69088=DIRECTION('ref_axis',(1.,0.,0.));
#69089=DIRECTION('',(0.,-1.,0.));
#69090=DIRECTION('center_axis',(0.,-1.,0.));
#69091=DIRECTION('ref_axis',(1.,0.,0.));
#69092=DIRECTION('center_axis',(0.,-1.,0.));
#69093=DIRECTION('ref_axis',(0.,0.,-1.));
#69094=DIRECTION('',(0.,0.,1.));
#69095=DIRECTION('',(1.,0.,0.));
#69096=DIRECTION('',(0.,0.,-1.));
#69097=DIRECTION('',(1.,0.,0.));
#69098=DIRECTION('center_axis',(0.,1.,0.));
#69099=DIRECTION('ref_axis',(1.,0.,0.));
#69100=DIRECTION('center_axis',(0.,1.,0.));
#69101=DIRECTION('ref_axis',(1.,0.,0.));
#69102=DIRECTION('',(0.857167300702117,-0.515038074910047,1.04972719113862E-16));
#69103=DIRECTION('center_axis',(0.,1.,0.));
#69104=DIRECTION('ref_axis',(1.,0.,0.));
#69105=DIRECTION('',(0.707106781186547,-0.707106781186547,-8.65956056235493E-17));
#69106=DIRECTION('center_axis',(0.,-1.,0.));
#69107=DIRECTION('ref_axis',(1.,0.,0.));
#69108=DIRECTION('center_axis',(0.,-1.,0.));
#69109=DIRECTION('ref_axis',(1.,0.,0.));
#69110=DIRECTION('',(0.,-1.,0.));
#69111=DIRECTION('center_axis',(0.,-1.,0.));
#69112=DIRECTION('ref_axis',(1.,0.,0.));
#69113=DIRECTION('center_axis',(0.,1.,0.));
#69114=DIRECTION('ref_axis',(1.,0.,0.));
#69115=DIRECTION('',(0.857167300702112,-0.515038074910054,1.04972719113862E-16));
#69116=DIRECTION('center_axis',(0.,-1.,0.));
#69117=DIRECTION('ref_axis',(1.,0.,0.));
#69118=DIRECTION('center_axis',(0.,-1.,0.));
#69119=DIRECTION('ref_axis',(1.,0.,0.));
#69120=DIRECTION('',(0.,-1.,0.));
#69121=DIRECTION('center_axis',(0.,-1.,0.));
#69122=DIRECTION('ref_axis',(1.,0.,0.));
#69123=DIRECTION('center_axis',(0.,1.,0.));
#69124=DIRECTION('ref_axis',(1.,0.,0.));
#69125=DIRECTION('center_axis',(0.,1.,0.));
#69126=DIRECTION('ref_axis',(1.,0.,0.));
#69127=DIRECTION('center_axis',(0.,-1.,0.));
#69128=DIRECTION('ref_axis',(1.,0.,0.));
#69129=DIRECTION('center_axis',(0.,-1.,0.));
#69130=DIRECTION('ref_axis',(1.,0.,0.));
#69131=DIRECTION('',(0.,-1.,0.));
#69132=DIRECTION('center_axis',(0.,-1.,0.));
#69133=DIRECTION('ref_axis',(1.,0.,0.));
#69134=DIRECTION('center_axis',(0.,1.,0.));
#69135=DIRECTION('ref_axis',(1.,0.,0.));
#69136=DIRECTION('center_axis',(0.,1.,0.));
#69137=DIRECTION('ref_axis',(1.,0.,0.));
#69138=DIRECTION('center_axis',(0.,-1.,0.));
#69139=DIRECTION('ref_axis',(1.,0.,0.));
#69140=DIRECTION('center_axis',(0.,-1.,0.));
#69141=DIRECTION('ref_axis',(1.,0.,0.));
#69142=DIRECTION('',(0.,-1.,0.));
#69143=DIRECTION('center_axis',(0.,-1.,0.));
#69144=DIRECTION('ref_axis',(1.,0.,0.));
#69145=DIRECTION('center_axis',(0.,1.,0.));
#69146=DIRECTION('ref_axis',(1.,0.,0.));
#69147=DIRECTION('center_axis',(0.,1.,0.));
#69148=DIRECTION('ref_axis',(1.,0.,0.));
#69149=DIRECTION('center_axis',(0.,-1.,0.));
#69150=DIRECTION('ref_axis',(1.,0.,0.));
#69151=DIRECTION('center_axis',(0.,-1.,0.));
#69152=DIRECTION('ref_axis',(1.,0.,0.));
#69153=DIRECTION('',(0.,-1.,0.));
#69154=DIRECTION('center_axis',(0.,-1.,0.));
#69155=DIRECTION('ref_axis',(1.,0.,0.));
#69156=DIRECTION('center_axis',(0.,1.,0.));
#69157=DIRECTION('ref_axis',(1.,0.,0.));
#69158=DIRECTION('center_axis',(0.,1.,0.));
#69159=DIRECTION('ref_axis',(1.,0.,0.));
#69160=DIRECTION('center_axis',(0.,-1.,0.));
#69161=DIRECTION('ref_axis',(1.,0.,0.));
#69162=DIRECTION('center_axis',(0.,-1.,0.));
#69163=DIRECTION('ref_axis',(1.,0.,0.));
#69164=DIRECTION('',(0.,-1.,0.));
#69165=DIRECTION('center_axis',(0.,-1.,0.));
#69166=DIRECTION('ref_axis',(1.,0.,0.));
#69167=DIRECTION('center_axis',(0.,1.,0.));
#69168=DIRECTION('ref_axis',(1.,0.,0.));
#69169=DIRECTION('center_axis',(0.,1.,0.));
#69170=DIRECTION('ref_axis',(1.,0.,0.));
#69171=DIRECTION('center_axis',(0.,-1.,0.));
#69172=DIRECTION('ref_axis',(1.,0.,0.));
#69173=DIRECTION('center_axis',(0.,-1.,0.));
#69174=DIRECTION('ref_axis',(1.,0.,0.));
#69175=DIRECTION('',(0.,-1.,0.));
#69176=DIRECTION('center_axis',(0.,-1.,0.));
#69177=DIRECTION('ref_axis',(1.,0.,0.));
#69178=DIRECTION('center_axis',(0.,1.,0.));
#69179=DIRECTION('ref_axis',(1.,0.,0.));
#69180=DIRECTION('center_axis',(0.,1.,0.));
#69181=DIRECTION('ref_axis',(1.,0.,0.));
#69182=DIRECTION('center_axis',(0.,-1.,0.));
#69183=DIRECTION('ref_axis',(1.,0.,0.));
#69184=DIRECTION('',(0.707106781186561,0.707106781186534,8.6595605623551E-17));
#69185=DIRECTION('center_axis',(0.,1.,0.));
#69186=DIRECTION('ref_axis',(1.,0.,0.));
#69187=DIRECTION('center_axis',(0.,-1.,0.));
#69188=DIRECTION('ref_axis',(0.,0.,-1.));
#69189=DIRECTION('',(0.,0.,1.));
#69190=DIRECTION('',(-1.,0.,0.));
#69191=DIRECTION('center_axis',(0.,-1.,0.));
#69192=DIRECTION('ref_axis',(1.,0.,0.));
#69193=DIRECTION('center_axis',(0.,-1.,0.));
#69194=DIRECTION('ref_axis',(1.,0.,0.));
#69195=DIRECTION('center_axis',(0.,-1.,0.));
#69196=DIRECTION('ref_axis',(1.,0.,0.));
#69197=DIRECTION('center_axis',(0.,1.,0.));
#69198=DIRECTION('ref_axis',(1.,0.,0.));
#69199=DIRECTION('',(0.,1.,0.));
#69200=DIRECTION('center_axis',(0.,-1.,0.));
#69201=DIRECTION('ref_axis',(1.,0.,0.));
#69202=DIRECTION('',(0.70710678118654,0.707106781186555,8.65956056235484E-17));
#69203=DIRECTION('center_axis',(0.,1.,0.));
#69204=DIRECTION('ref_axis',(1.,0.,0.));
#69205=DIRECTION('center_axis',(0.,1.,0.));
#69206=DIRECTION('ref_axis',(1.,0.,0.));
#69207=DIRECTION('',(0.,1.,0.));
#69208=DIRECTION('center_axis',(0.,-1.,0.));
#69209=DIRECTION('ref_axis',(1.,0.,0.));
#69210=DIRECTION('',(0.70710678118654,0.707106781186555,8.65956056235484E-17));
#69211=DIRECTION('center_axis',(0.,1.,0.));
#69212=DIRECTION('ref_axis',(1.,0.,0.));
#69213=DIRECTION('center_axis',(0.,1.,0.));
#69214=DIRECTION('ref_axis',(1.,0.,0.));
#69215=DIRECTION('',(0.,1.,0.));
#69216=DIRECTION('center_axis',(0.,-1.,0.));
#69217=DIRECTION('ref_axis',(1.,0.,0.));
#69218=DIRECTION('',(0.707106781186545,0.70710678118655,8.6595605623549E-17));
#69219=DIRECTION('center_axis',(0.,1.,0.));
#69220=DIRECTION('ref_axis',(1.,0.,0.));
#69221=DIRECTION('center_axis',(0.,1.,0.));
#69222=DIRECTION('ref_axis',(1.,0.,0.));
#69223=DIRECTION('',(0.,1.,0.));
#69224=DIRECTION('center_axis',(0.,-1.,0.));
#69225=DIRECTION('ref_axis',(1.,0.,0.));
#69226=DIRECTION('',(0.707106781186545,0.70710678118655,8.6595605623549E-17));
#69227=DIRECTION('center_axis',(0.,1.,0.));
#69228=DIRECTION('ref_axis',(1.,0.,0.));
#69229=DIRECTION('center_axis',(0.,1.,0.));
#69230=DIRECTION('ref_axis',(1.,0.,0.));
#69231=DIRECTION('',(0.,1.,0.));
#69232=DIRECTION('center_axis',(0.,-1.,0.));
#69233=DIRECTION('ref_axis',(1.,0.,0.));
#69234=DIRECTION('',(0.707106781186561,0.707106781186534,8.6595605623551E-17));
#69235=DIRECTION('center_axis',(0.,1.,0.));
#69236=DIRECTION('ref_axis',(1.,0.,0.));
#69237=DIRECTION('center_axis',(0.,1.,0.));
#69238=DIRECTION('ref_axis',(1.,0.,0.));
#69239=DIRECTION('',(0.,1.,0.));
#69240=DIRECTION('center_axis',(0.70710678118653,-0.353553390593282,0.61237243569581));
#69241=DIRECTION('ref_axis',(0.654653670707996,0.,-0.755928946018439));
#69242=DIRECTION('',(0.,-0.866025403784439,-0.499999999999999));
#69243=DIRECTION('center_axis',(-0.70710678118653,0.353553390593282,-0.61237243569581));
#69244=DIRECTION('ref_axis',(0.707106781186565,0.353553390593265,-0.61237243569578));
#69245=DIRECTION('',(0.,0.866025403784439,0.499999999999999));
#69246=DIRECTION('',(-0.654653670707999,-1.45362315675074E-14,0.755928946018435));
#69247=DIRECTION('center_axis',(0.707106781186532,0.35355339059329,0.612372435695804));
#69248=DIRECTION('ref_axis',(0.654653670707991,0.,-0.755928946018442));
#69249=DIRECTION('',(0.,0.866025403784432,-0.500000000000012));
#69250=DIRECTION('',(-0.654653670708,0.654653670707976,0.377964473009189));
#69251=DIRECTION('',(0.,-0.866025403784432,0.500000000000012));
#69252=DIRECTION('center_axis',(0.707106781186534,0.707106781186561,0.));
#69253=DIRECTION('ref_axis',(0.,0.,-1.));
#69254=DIRECTION('',(0.,0.,-1.));
#69255=DIRECTION('',(-0.577350269189639,0.577350269189617,-0.577350269189622));
#69256=DIRECTION('',(0.,0.,1.));
#69257=DIRECTION('center_axis',(0.707106781186532,0.,0.707106781186563));
#69258=DIRECTION('ref_axis',(0.707106781186563,0.,-0.707106781186532));
#69259=DIRECTION('',(0.,1.,0.));
#69260=DIRECTION('',(-0.577350269189641,0.57735026918962,0.577350269189616));
#69261=DIRECTION('',(0.,-1.,0.));
#69262=DIRECTION('',(0.577350269189641,-0.57735026918962,-0.577350269189616));
#69263=DIRECTION('center_axis',(0.707106781186534,0.707106781186561,0.));
#69264=DIRECTION('ref_axis',(0.,0.,-1.));
#69265=DIRECTION('',(0.,0.,-1.));
#69266=DIRECTION('',(-0.654653670707992,0.654653670707968,-0.377964473009218));
#69267=DIRECTION('',(0.,0.,1.));
#69268=DIRECTION('center_axis',(0.707106781186533,0.353553390593279,-0.612372435695809));
#69269=DIRECTION('ref_axis',(-0.654653670707994,0.,-0.75592894601844));
#69270=DIRECTION('',(0.,-0.86602540378444,-0.499999999999997));
#69271=DIRECTION('',(-0.654653670707994,-4.84541052250242E-15,-0.75592894601844));
#69272=DIRECTION('',(0.,0.86602540378444,0.499999999999997));
#69273=DIRECTION('center_axis',(0.707106781186535,-0.35355339059328,-0.612372435695805));
#69274=DIRECTION('ref_axis',(-0.65465367070799,0.,-0.755928946018443));
#69275=DIRECTION('',(0.,-0.866025403784439,0.5));
#69276=DIRECTION('center_axis',(-0.707106781186535,0.35355339059328,0.612372435695805));
#69277=DIRECTION('ref_axis',(-0.70710678118656,-0.353553390593267,-0.612372435695784));
#69278=DIRECTION('',(0.,0.866025403784439,-0.5));
#69279=DIRECTION('center_axis',(0.707106781186534,0.707106781186561,0.));
#69280=DIRECTION('ref_axis',(0.,0.,-1.));
#69281=DIRECTION('',(0.,0.,-1.));
#69282=DIRECTION('',(0.577350269189639,-0.577350269189617,0.577350269189622));
#69283=DIRECTION('center_axis',(0.707106781186537,0.,-0.707106781186558));
#69284=DIRECTION('ref_axis',(-0.707106781186558,0.,-0.707106781186537));
#69285=DIRECTION('',(0.,-1.,0.));
#69286=DIRECTION('',(0.,1.,0.));
#69287=DIRECTION('center_axis',(1.,0.,0.));
#69288=DIRECTION('ref_axis',(0.,0.,-1.));
#69289=DIRECTION('',(1.,0.,0.));
#69290=DIRECTION('center_axis',(0.707106781186544,0.353553390593275,-0.612372435695798));
#69291=DIRECTION('ref_axis',(-0.707106781186551,0.353553390593271,-0.612372435695791));
#69292=DIRECTION('center_axis',(0.707106781186548,-0.707106781186547,0.));
#69293=DIRECTION('ref_axis',(0.707106781186547,0.707106781186548,0.));
#69294=DIRECTION('',(-1.,0.,0.));
#69295=DIRECTION('center_axis',(-0.707106781186534,-0.707106781186561,0.));
#69296=DIRECTION('ref_axis',(-0.707106781186561,0.707106781186534,0.));
#69297=DIRECTION('center_axis',(-1.,0.,0.));
#69298=DIRECTION('ref_axis',(0.,0.,-1.));
#69299=DIRECTION('center_axis',(0.,-0.499999999999999,0.866025403784439));
#69300=DIRECTION('ref_axis',(0.,-0.866025403784439,-0.499999999999999));
#69301=DIRECTION('',(1.,0.,0.));
#69302=DIRECTION('',(0.,0.866025403784439,0.499999999999999));
#69303=DIRECTION('center_axis',(0.,0.500000000000012,0.866025403784432));
#69304=DIRECTION('ref_axis',(1.,0.,0.));
#69305=DIRECTION('',(-1.,0.,0.));
#69306=DIRECTION('',(0.,0.866025403784432,-0.500000000000012));
#69307=DIRECTION('center_axis',(0.,1.,0.));
#69308=DIRECTION('ref_axis',(0.,0.,1.));
#69309=DIRECTION('',(-1.,0.,0.));
#69310=DIRECTION('',(0.,0.,-1.));
#69311=DIRECTION('center_axis',(0.,0.,1.));
#69312=DIRECTION('ref_axis',(0.,-1.,0.));
#69313=DIRECTION('',(0.,-1.,0.));
#69314=DIRECTION('center_axis',(0.,0.,-1.));
#69315=DIRECTION('ref_axis',(0.,1.,0.));
#69316=DIRECTION('',(1.,0.,0.));
#69317=DIRECTION('',(0.,1.,0.));
#69318=DIRECTION('center_axis',(0.707106781186534,0.707106781186561,0.));
#69319=DIRECTION('ref_axis',(0.,0.,-1.));
#69320=DIRECTION('',(0.,0.,1.));
#69321=DIRECTION('center_axis',(-0.707106781186534,-0.707106781186561,0.));
#69322=DIRECTION('ref_axis',(-0.707106781186561,0.707106781186534,0.));
#69323=DIRECTION('',(0.,0.,-1.));
#69324=DIRECTION('',(-0.678598344545864,0.678598344545836,-0.281084637714807));
#69325=DIRECTION('center_axis',(0.707106781186528,0.500000000000013,-0.500000000000014));
#69326=DIRECTION('ref_axis',(-0.577350269189647,0.,-0.816496580927711));
#69327=DIRECTION('',(0.,-0.707106781186548,-0.707106781186547));
#69328=DIRECTION('',(-0.678598344545863,0.281084637714805,-0.678598344545838));
#69329=DIRECTION('',(0.,0.707106781186548,0.707106781186547));
#69330=DIRECTION('center_axis',(0.707106781186534,0.,-0.707106781186561));
#69331=DIRECTION('ref_axis',(-0.707106781186561,0.,-0.707106781186534));
#69332=DIRECTION('',(0.,-1.,0.));
#69333=DIRECTION('',(-0.678598344545862,-0.281084637714807,-0.678598344545837));
#69334=DIRECTION('',(0.,1.,0.));
#69335=DIRECTION('center_axis',(0.707106781186531,-0.500000000000011,-0.500000000000012));
#69336=DIRECTION('ref_axis',(-0.577350269189644,0.,-0.816496580927713));
#69337=DIRECTION('',(0.,-0.707106781186548,0.707106781186547));
#69338=DIRECTION('',(0.,0.707106781186548,-0.707106781186547));
#69339=DIRECTION('center_axis',(0.70710678118653,-0.500000000000016,0.500000000000009));
#69340=DIRECTION('ref_axis',(0.577350269189642,0.,-0.816496580927714));
#69341=DIRECTION('',(0.,0.707106781186542,0.707106781186553));
#69342=DIRECTION('',(-0.678598344545859,-0.281084637714809,0.678598344545839));
#69343=DIRECTION('',(0.,-0.707106781186542,-0.707106781186553));
#69344=DIRECTION('center_axis',(0.707106781186537,0.,0.707106781186558));
#69345=DIRECTION('ref_axis',(0.707106781186558,0.,-0.707106781186537));
#69346=DIRECTION('',(0.,1.,0.));
#69347=DIRECTION('',(-0.678598344545856,0.281084637714825,0.678598344545836));
#69348=DIRECTION('',(0.,-1.,0.));
#69349=DIRECTION('center_axis',(0.707106781186538,0.500000000000006,0.500000000000008));
#69350=DIRECTION('ref_axis',(0.577350269189637,0.,-0.816496580927718));
#69351=DIRECTION('',(0.,0.707106781186549,-0.707106781186546));
#69352=DIRECTION('',(-0.678598344545859,0.678598344545834,0.281084637714823));
#69353=DIRECTION('',(0.,-0.707106781186549,0.707106781186546));
#69354=DIRECTION('center_axis',(0.707106781186534,0.707106781186561,0.));
#69355=DIRECTION('ref_axis',(0.,0.,-1.));
#69356=DIRECTION('',(0.,0.,-1.));
#69357=DIRECTION('',(0.,0.,1.));
#69358=DIRECTION('center_axis',(0.,1.,0.));
#69359=DIRECTION('ref_axis',(0.,0.,1.));
#69360=DIRECTION('',(1.,0.,0.));
#69361=DIRECTION('',(0.,0.,-1.));
#69362=DIRECTION('',(1.,0.,0.));
#69363=DIRECTION('center_axis',(0.,0.707106781186547,-0.707106781186548));
#69364=DIRECTION('ref_axis',(-1.,0.,0.));
#69365=DIRECTION('',(-1.,0.,0.));
#69366=DIRECTION('',(0.,-0.707106781186548,-0.707106781186547));
#69367=DIRECTION('center_axis',(0.,0.,-1.));
#69368=DIRECTION('ref_axis',(0.,1.,0.));
#69369=DIRECTION('',(1.,0.,0.));
#69370=DIRECTION('',(0.,-1.,0.));
#69371=DIRECTION('center_axis',(0.,-0.707106781186547,-0.707106781186548));
#69372=DIRECTION('ref_axis',(-1.,0.,0.));
#69373=DIRECTION('',(0.,-0.707106781186548,0.707106781186547));
#69374=DIRECTION('center_axis',(0.,-0.707106781186553,0.707106781186542));
#69375=DIRECTION('ref_axis',(1.,0.,0.));
#69376=DIRECTION('',(-1.,0.,0.));
#69377=DIRECTION('',(0.,0.707106781186542,0.707106781186553));
#69378=DIRECTION('center_axis',(0.,0.,1.));
#69379=DIRECTION('ref_axis',(0.,-1.,0.));
#69380=DIRECTION('',(1.,0.,0.));
#69381=DIRECTION('',(0.,1.,0.));
#69382=DIRECTION('center_axis',(0.,0.707106781186546,0.707106781186549));
#69383=DIRECTION('ref_axis',(1.,0.,0.));
#69384=DIRECTION('',(-1.,0.,0.));
#69385=DIRECTION('',(0.,0.707106781186549,-0.707106781186546));
#69386=DIRECTION('center_axis',(0.,1.,0.));
#69387=DIRECTION('ref_axis',(0.,0.,1.));
#69388=DIRECTION('',(0.,0.,-1.));
#69389=DIRECTION('center_axis',(-0.707106781186549,-0.353553390593273,-0.612372435695794));
#69390=DIRECTION('ref_axis',(-0.654653670707976,0.,0.755928946018455));
#69391=DIRECTION('',(0.,-0.866025403784439,0.5));
#69392=DIRECTION('center_axis',(0.707106781186549,0.353553390593273,0.612372435695794));
#69393=DIRECTION('ref_axis',(0.707106781186546,-0.353553390593274,-0.612372435695796));
#69394=DIRECTION('',(0.65465367070798,-4.8454105225025E-15,-0.755928946018452));
#69395=DIRECTION('center_axis',(-0.707106781186546,0.353553390593272,-0.612372435695797));
#69396=DIRECTION('ref_axis',(-0.65465367070798,0.,0.755928946018452));
#69397=DIRECTION('',(0.654653670707978,0.654653670707978,-0.377964473009224));
#69398=DIRECTION('',(0.,-0.86602540378444,-0.499999999999997));
#69399=DIRECTION('center_axis',(-0.707106781186548,0.707106781186547,0.));
#69400=DIRECTION('ref_axis',(0.,0.,1.));
#69401=DIRECTION('',(0.577350269189627,0.577350269189627,0.577350269189623));
#69402=DIRECTION('',(0.,0.,-1.));
#69403=DIRECTION('center_axis',(-0.707106781186545,0.,0.70710678118655));
#69404=DIRECTION('ref_axis',(0.70710678118655,0.,0.707106781186545));
#69405=DIRECTION('',(0.577350269189627,0.577350269189627,0.577350269189623));
#69406=DIRECTION('center_axis',(-0.707106781186548,0.707106781186547,0.));
#69407=DIRECTION('ref_axis',(0.,0.,1.));
#69408=DIRECTION('',(0.577350269189624,0.577350269189625,-0.577350269189629));
#69409=DIRECTION('center_axis',(-0.70710678118655,0.,-0.707106781186545));
#69410=DIRECTION('ref_axis',(-0.707106781186545,0.,0.70710678118655));
#69411=DIRECTION('',(0.577350269189624,0.577350269189625,-0.577350269189629));
#69412=DIRECTION('center_axis',(-0.707106781186548,0.707106781186547,0.));
#69413=DIRECTION('ref_axis',(0.,0.,1.));
#69414=DIRECTION('',(0.654653670707986,0.654653670707987,0.377964473009195));
#69415=DIRECTION('center_axis',(-0.707106781186545,0.353553390593283,0.612372435695792));
#69416=DIRECTION('ref_axis',(0.654653670707977,0.,0.755928946018455));
#69417=DIRECTION('',(0.654653670707985,-1.45362315675076E-14,0.755928946018448));
#69418=DIRECTION('center_axis',(-0.707106781186544,-0.353553390593275,0.612372435695798));
#69419=DIRECTION('ref_axis',(0.654653670707981,0.,0.755928946018451));
#69420=DIRECTION('center_axis',(-0.707106781186548,0.707106781186547,0.));
#69421=DIRECTION('ref_axis',(0.,0.,1.));
#69422=DIRECTION('',(0.678598344545843,0.678598344545848,0.281084637714827));
#69423=DIRECTION('center_axis',(-0.707106781186551,0.499999999999997,0.499999999999999));
#69424=DIRECTION('ref_axis',(0.577350269189623,0.,0.816496580927728));
#69425=DIRECTION('',(0.678598344545843,0.281084637714827,0.678598344545848));
#69426=DIRECTION('center_axis',(-0.70710678118655,0.,0.707106781186545));
#69427=DIRECTION('ref_axis',(0.707106781186545,0.,0.70710678118655));
#69428=DIRECTION('',(0.678598344545845,-0.281084637714814,0.678598344545851));
#69429=DIRECTION('center_axis',(-0.707106781186543,-0.500000000000007,0.5));
#69430=DIRECTION('ref_axis',(0.577350269189628,0.,0.816496580927724));
#69431=DIRECTION('center_axis',(-0.707106781186548,-0.707106781186548,0.));
#69432=DIRECTION('ref_axis',(0.,0.,1.));
#69433=DIRECTION('',(0.678598344545846,-0.678598344545855,-0.281084637714803));
#69434=DIRECTION('center_axis',(-0.707106781186544,-0.500000000000002,-0.500000000000003));
#69435=DIRECTION('ref_axis',(-0.57735026918963,0.,0.816496580927723));
#69436=DIRECTION('',(0.678598344545849,-0.281084637714812,-0.678598344545849));
#69437=DIRECTION('center_axis',(-0.707106781186548,0.,-0.707106781186547));
#69438=DIRECTION('ref_axis',(-0.707106781186547,0.,0.707106781186548));
#69439=DIRECTION('',(0.678598344545848,0.281084637714809,-0.678598344545851));
#69440=DIRECTION('center_axis',(-0.707106781186542,0.500000000000004,-0.500000000000005));
#69441=DIRECTION('ref_axis',(-0.577350269189633,0.,0.816496580927721));
#69442=DIRECTION('',(0.678598344545849,0.67859834454585,-0.28108463771481));
#69443=DIRECTION('center_axis',(-0.707106781186548,0.707106781186547,0.));
#69444=DIRECTION('ref_axis',(0.,0.,1.));
#69445=DIRECTION('center_axis',(0.707106781186548,-0.707106781186547,0.));
#69446=DIRECTION('ref_axis',(0.707106781186547,0.707106781186548,0.));
#69447=DIRECTION('center_axis',(1.,0.,0.));
#69448=DIRECTION('ref_axis',(0.,0.,-1.));
#69449=DIRECTION('center_axis',(-1.,0.,0.));
#69450=DIRECTION('ref_axis',(0.,0.,-1.));
#69451=DIRECTION('center_axis',(0.,1.,0.));
#69452=DIRECTION('ref_axis',(0.,0.,1.));
#69453=DIRECTION('',(1.,0.,0.));
#69454=DIRECTION('center_axis',(1.,0.,0.));
#69455=DIRECTION('ref_axis',(0.,-0.500000000000001,0.866025403784438));
#69456=DIRECTION('',(-1.,0.,0.));
#69457=DIRECTION('center_axis',(0.,0.499999999999997,-0.86602540378444));
#69458=DIRECTION('ref_axis',(-1.,0.,0.));
#69459=DIRECTION('',(-1.,0.,0.));
#69460=DIRECTION('center_axis',(0.,-0.5,-0.866025403784439));
#69461=DIRECTION('ref_axis',(0.,0.866025403784439,-0.5));
#69462=DIRECTION('axis',(0.,0.,1.));
#69463=DIRECTION('refdir',(1.,0.,0.));
#69464=DIRECTION('center_axis',(0.,0.,-1.));
#69465=DIRECTION('ref_axis',(1.,0.,0.));
#69466=DIRECTION('',(0.707106781186548,-8.65956056235494E-17,0.707106781186548));
#69467=DIRECTION('center_axis',(0.,0.,-1.));
#69468=DIRECTION('ref_axis',(1.,0.,0.));
#69469=DIRECTION('center_axis',(0.,0.,1.));
#69470=DIRECTION('ref_axis',(1.,0.,0.));
#69471=DIRECTION('center_axis',(0.,0.,1.));
#69472=DIRECTION('ref_axis',(1.,0.,0.));
#69473=DIRECTION('center_axis',(0.,0.,1.));
#69474=DIRECTION('ref_axis',(1.,0.,0.));
#69475=DIRECTION('',(0.707106781186568,8.65956056235519E-17,-0.707106781186527));
#69476=DIRECTION('center_axis',(0.,0.,-1.));
#69477=DIRECTION('ref_axis',(1.,0.,0.));
#69478=DIRECTION('center_axis',(0.,0.,1.));
#69479=DIRECTION('ref_axis',(1.,0.,0.));
#69480=DIRECTION('center_axis',(0.,0.,1.));
#69481=DIRECTION('ref_axis',(0.,-1.,0.));
#69482=DIRECTION('',(0.,1.,0.));
#69483=DIRECTION('',(-1.,0.,0.));
#69484=DIRECTION('center_axis',(0.,0.,1.));
#69485=DIRECTION('ref_axis',(1.,0.,0.));
#69486=DIRECTION('center_axis',(0.,0.,1.));
#69487=DIRECTION('ref_axis',(1.,0.,0.));
#69488=DIRECTION('',(-1.,0.,0.));
#69489=DIRECTION('',(-1.,0.,0.));
#69490=DIRECTION('',(0.,-1.,0.));
#69491=DIRECTION('',(1.,0.,0.));
#69492=DIRECTION('center_axis',(0.,0.,1.));
#69493=DIRECTION('ref_axis',(1.,0.,0.));
#69494=DIRECTION('center_axis',(0.,0.,-1.));
#69495=DIRECTION('ref_axis',(1.,0.,0.));
#69496=DIRECTION('',(0.,0.,-1.));
#69497=DIRECTION('center_axis',(0.,0.,-1.));
#69498=DIRECTION('ref_axis',(1.,0.,0.));
#69499=DIRECTION('center_axis',(0.,0.,1.));
#69500=DIRECTION('ref_axis',(1.,0.,0.));
#69501=DIRECTION('',(0.707106781186568,8.65956056235519E-17,-0.707106781186527));
#69502=DIRECTION('center_axis',(0.,0.,-1.));
#69503=DIRECTION('ref_axis',(1.,0.,0.));
#69504=DIRECTION('center_axis',(0.,0.,-1.));
#69505=DIRECTION('ref_axis',(1.,0.,0.));
#69506=DIRECTION('',(0.,0.,-1.));
#69507=DIRECTION('center_axis',(0.,0.,-1.));
#69508=DIRECTION('ref_axis',(1.,0.,0.));
#69509=DIRECTION('center_axis',(0.,0.,1.));
#69510=DIRECTION('ref_axis',(1.,0.,0.));
#69511=DIRECTION('',(-0.857167300702113,-1.04972719113862E-16,0.515038074910054));
#69512=DIRECTION('center_axis',(0.,0.,1.));
#69513=DIRECTION('ref_axis',(1.,0.,0.));
#69514=DIRECTION('',(-0.857167300702109,-1.04972719113861E-16,0.51503807491006));
#69515=DIRECTION('center_axis',(0.,0.,-1.));
#69516=DIRECTION('ref_axis',(1.,0.,0.));
#69517=DIRECTION('center_axis',(0.,0.,-1.));
#69518=DIRECTION('ref_axis',(1.,0.,0.));
#69519=DIRECTION('',(0.707106781186552,-8.65956056235499E-17,0.707106781186543));
#69520=DIRECTION('center_axis',(0.,0.,1.));
#69521=DIRECTION('ref_axis',(1.,0.,0.));
#69522=DIRECTION('center_axis',(0.,0.,-1.));
#69523=DIRECTION('ref_axis',(1.,0.,0.));
#69524=DIRECTION('center_axis',(0.,-0.707106781186546,-0.707106781186549));
#69525=DIRECTION('ref_axis',(-1.,0.,0.));
#69526=DIRECTION('',(1.,0.,0.));
#69527=DIRECTION('',(0.,-0.707106781186549,0.707106781186546));
#69528=DIRECTION('',(-1.,0.,0.));
#69529=DIRECTION('',(0.,0.707106781186549,-0.707106781186546));
#69530=DIRECTION('',(1.,0.,0.));
#69531=DIRECTION('',(1.,0.,0.));
#69532=DIRECTION('',(1.,0.,0.));
#69533=DIRECTION('center_axis',(0.,0.,1.));
#69534=DIRECTION('ref_axis',(1.,0.,0.));
#69535=DIRECTION('',(0.,0.,1.));
#69536=DIRECTION('center_axis',(0.,-0.5,-0.866025403784439));
#69537=DIRECTION('ref_axis',(0.,0.866025403784439,-0.5));
#69538=DIRECTION('center_axis',(0.,0.,-1.));
#69539=DIRECTION('ref_axis',(1.,0.,0.));
#69540=DIRECTION('center_axis',(0.,0.,-1.));
#69541=DIRECTION('ref_axis',(1.,0.,0.));
#69542=DIRECTION('',(0.707106781186552,-8.65956056235499E-17,0.707106781186543));
#69543=DIRECTION('center_axis',(0.,0.,1.));
#69544=DIRECTION('ref_axis',(1.,0.,0.));
#69545=DIRECTION('center_axis',(0.,0.,-1.));
#69546=DIRECTION('ref_axis',(1.,0.,0.));
#69547=DIRECTION('center_axis',(0.,0.,1.));
#69548=DIRECTION('ref_axis',(1.,0.,0.));
#69549=DIRECTION('',(0.,0.,1.));
#69550=DIRECTION('center_axis',(0.,-0.5,-0.866025403784439));
#69551=DIRECTION('ref_axis',(0.,0.866025403784439,-0.5));
#69552=DIRECTION('center_axis',(0.,0.,-1.));
#69553=DIRECTION('ref_axis',(1.,0.,0.));
#69554=DIRECTION('center_axis',(0.,0.,1.));
#69555=DIRECTION('ref_axis',(1.,0.,0.));
#69556=DIRECTION('center_axis',(0.,0.,-1.));
#69557=DIRECTION('ref_axis',(1.,0.,0.));
#69558=DIRECTION('center_axis',(0.,0.,1.));
#69559=DIRECTION('ref_axis',(1.,0.,0.));
#69560=DIRECTION('',(0.,0.,1.));
#69561=DIRECTION('center_axis',(0.,-0.5,-0.866025403784439));
#69562=DIRECTION('ref_axis',(0.,0.866025403784439,-0.5));
#69563=DIRECTION('center_axis',(0.,0.,-1.));
#69564=DIRECTION('ref_axis',(0.,1.,0.));
#69565=DIRECTION('',(0.,-1.,0.));
#69566=DIRECTION('',(-1.,0.,0.));
#69567=DIRECTION('',(0.,1.,0.));
#69568=DIRECTION('center_axis',(0.,1.,0.));
#69569=DIRECTION('ref_axis',(1.,0.,0.));
#69570=DIRECTION('center_axis',(0.,1.,0.));
#69571=DIRECTION('ref_axis',(1.,0.,0.));
#69572=DIRECTION('',(0.707106781186537,-0.707106781186558,-8.6595605623548E-17));
#69573=DIRECTION('center_axis',(0.,-1.,0.));
#69574=DIRECTION('ref_axis',(1.,0.,0.));
#69575=DIRECTION('center_axis',(0.,1.,0.));
#69576=DIRECTION('ref_axis',(1.,0.,0.));
#69577=DIRECTION('center_axis',(0.,0.707106781186548,0.707106781186548));
#69578=DIRECTION('ref_axis',(1.,0.,0.));
#69579=DIRECTION('',(-1.,0.,0.));
#69580=DIRECTION('',(0.,-0.707106781186548,0.707106781186548));
#69581=DIRECTION('',(0.,0.707106781186548,-0.707106781186548));
#69582=DIRECTION('',(-1.,0.,0.));
#69583=DIRECTION('center_axis',(0.,-1.,0.));
#69584=DIRECTION('ref_axis',(1.,0.,0.));
#69585=DIRECTION('',(0.,-1.,0.));
#69586=DIRECTION('center_axis',(0.,-1.,0.));
#69587=DIRECTION('ref_axis',(1.,0.,0.));
#69588=DIRECTION('center_axis',(0.,-1.,0.));
#69589=DIRECTION('ref_axis',(1.,0.,0.));
#69590=DIRECTION('center_axis',(0.,-1.,0.));
#69591=DIRECTION('ref_axis',(1.,0.,0.));
#69592=DIRECTION('center_axis',(0.,1.,0.));
#69593=DIRECTION('ref_axis',(1.,0.,0.));
#69594=DIRECTION('center_axis',(0.,1.,0.));
#69595=DIRECTION('ref_axis',(1.,0.,0.));
#69596=DIRECTION('',(0.707106781186558,-0.707106781186537,-8.65956056235506E-17));
#69597=DIRECTION('center_axis',(0.,-1.,0.));
#69598=DIRECTION('ref_axis',(1.,0.,0.));
#69599=DIRECTION('center_axis',(0.,1.,0.));
#69600=DIRECTION('ref_axis',(0.,0.,1.));
#69601=DIRECTION('',(0.,0.,1.));
#69602=DIRECTION('',(1.,0.,0.));
#69603=DIRECTION('',(0.,0.,-1.));
#69604=DIRECTION('center_axis',(0.,1.,0.));
#69605=DIRECTION('ref_axis',(1.,0.,0.));
#69606=DIRECTION('center_axis',(0.,1.,0.));
#69607=DIRECTION('ref_axis',(1.,0.,0.));
#69608=DIRECTION('center_axis',(0.,1.,0.));
#69609=DIRECTION('ref_axis',(1.,0.,0.));
#69610=DIRECTION('center_axis',(0.,1.,0.));
#69611=DIRECTION('ref_axis',(1.,0.,0.));
#69612=DIRECTION('center_axis',(0.,1.,0.));
#69613=DIRECTION('ref_axis',(1.,0.,0.));
#69614=DIRECTION('center_axis',(0.,-1.,0.));
#69615=DIRECTION('ref_axis',(1.,0.,0.));
#69616=DIRECTION('',(0.,-1.,0.));
#69617=DIRECTION('center_axis',(0.,-1.,0.));
#69618=DIRECTION('ref_axis',(1.,0.,0.));
#69619=DIRECTION('center_axis',(0.,-1.,0.));
#69620=DIRECTION('ref_axis',(1.,0.,0.));
#69621=DIRECTION('center_axis',(0.,-1.,0.));
#69622=DIRECTION('ref_axis',(1.,0.,0.));
#69623=DIRECTION('center_axis',(0.,1.,0.));
#69624=DIRECTION('ref_axis',(1.,0.,0.));
#69625=DIRECTION('',(0.707106781186558,-0.707106781186537,-8.65956056235506E-17));
#69626=DIRECTION('center_axis',(0.,-1.,0.));
#69627=DIRECTION('ref_axis',(1.,0.,0.));
#69628=DIRECTION('center_axis',(0.,-1.,0.));
#69629=DIRECTION('ref_axis',(1.,0.,0.));
#69630=DIRECTION('',(0.,-1.,0.));
#69631=DIRECTION('center_axis',(0.,-1.,0.));
#69632=DIRECTION('ref_axis',(1.,0.,0.));
#69633=DIRECTION('center_axis',(0.,-1.,0.));
#69634=DIRECTION('ref_axis',(1.,0.,0.));
#69635=DIRECTION('center_axis',(0.,-1.,0.));
#69636=DIRECTION('ref_axis',(1.,0.,0.));
#69637=DIRECTION('center_axis',(0.,1.,0.));
#69638=DIRECTION('ref_axis',(1.,0.,0.));
#69639=DIRECTION('',(0.,0.,1.));
#69640=DIRECTION('center_axis',(0.,1.,0.));
#69641=DIRECTION('ref_axis',(1.,0.,0.));
#69642=DIRECTION('',(0.,0.,1.));
#69643=DIRECTION('center_axis',(0.,1.,0.));
#69644=DIRECTION('ref_axis',(1.,0.,0.));
#69645=DIRECTION('',(0.,0.,1.));
#69646=DIRECTION('center_axis',(0.,1.,0.));
#69647=DIRECTION('ref_axis',(1.,0.,0.));
#69648=DIRECTION('',(0.,0.,1.));
#69649=DIRECTION('center_axis',(0.,1.,0.));
#69650=DIRECTION('ref_axis',(1.,0.,0.));
#69651=DIRECTION('',(0.,0.,1.));
#69652=DIRECTION('center_axis',(0.,1.,0.));
#69653=DIRECTION('ref_axis',(1.,0.,0.));
#69654=DIRECTION('',(0.,0.,1.));
#69655=DIRECTION('center_axis',(0.,1.,0.));
#69656=DIRECTION('ref_axis',(1.,0.,0.));
#69657=DIRECTION('',(0.707106781186554,-0.707106781186541,-8.65956056235501E-17));
#69658=DIRECTION('center_axis',(0.,-1.,0.));
#69659=DIRECTION('ref_axis',(1.,0.,0.));
#69660=DIRECTION('center_axis',(0.,-1.,0.));
#69661=DIRECTION('ref_axis',(1.,0.,0.));
#69662=DIRECTION('',(0.,-1.,0.));
#69663=DIRECTION('center_axis',(0.,-1.,0.));
#69664=DIRECTION('ref_axis',(1.,0.,0.));
#69665=DIRECTION('center_axis',(0.,1.,0.));
#69666=DIRECTION('ref_axis',(1.,0.,0.));
#69667=DIRECTION('',(0.707106781186554,-0.707106781186541,-8.65956056235501E-17));
#69668=DIRECTION('center_axis',(0.,-1.,0.));
#69669=DIRECTION('ref_axis',(1.,0.,0.));
#69670=DIRECTION('center_axis',(0.,-1.,0.));
#69671=DIRECTION('ref_axis',(1.,0.,0.));
#69672=DIRECTION('',(0.,-1.,0.));
#69673=DIRECTION('center_axis',(0.,-1.,0.));
#69674=DIRECTION('ref_axis',(1.,0.,0.));
#69675=DIRECTION('center_axis',(0.,1.,0.));
#69676=DIRECTION('ref_axis',(1.,0.,0.));
#69677=DIRECTION('',(0.707106781186554,-0.707106781186541,-8.65956056235501E-17));
#69678=DIRECTION('center_axis',(0.,-1.,0.));
#69679=DIRECTION('ref_axis',(1.,0.,0.));
#69680=DIRECTION('center_axis',(0.,-1.,0.));
#69681=DIRECTION('ref_axis',(1.,0.,0.));
#69682=DIRECTION('',(0.,-1.,0.));
#69683=DIRECTION('center_axis',(0.,-1.,0.));
#69684=DIRECTION('ref_axis',(1.,0.,0.));
#69685=DIRECTION('center_axis',(0.,1.,0.));
#69686=DIRECTION('ref_axis',(1.,0.,0.));
#69687=DIRECTION('',(0.707106781186554,-0.707106781186541,-8.65956056235501E-17));
#69688=DIRECTION('center_axis',(0.,-1.,0.));
#69689=DIRECTION('ref_axis',(1.,0.,0.));
#69690=DIRECTION('center_axis',(0.,-1.,0.));
#69691=DIRECTION('ref_axis',(1.,0.,0.));
#69692=DIRECTION('',(0.,-1.,0.));
#69693=DIRECTION('center_axis',(0.,-1.,0.));
#69694=DIRECTION('ref_axis',(1.,0.,0.));
#69695=DIRECTION('center_axis',(0.,1.,0.));
#69696=DIRECTION('ref_axis',(1.,0.,0.));
#69697=DIRECTION('',(0.857167300702111,-0.515038074910056,1.04972719113862E-16));
#69698=DIRECTION('center_axis',(0.,1.,0.));
#69699=DIRECTION('ref_axis',(1.,0.,0.));
#69700=DIRECTION('',(0.857167300702111,-0.515038074910056,1.04972719113862E-16));
#69701=DIRECTION('center_axis',(0.,1.,0.));
#69702=DIRECTION('ref_axis',(1.,0.,0.));
#69703=DIRECTION('',(0.857167300702111,-0.515038074910056,1.04972719113862E-16));
#69704=DIRECTION('center_axis',(0.,1.,0.));
#69705=DIRECTION('ref_axis',(1.,0.,0.));
#69706=DIRECTION('',(0.857167300702111,-0.515038074910056,1.04972719113862E-16));
#69707=DIRECTION('center_axis',(0.,0.,1.));
#69708=DIRECTION('ref_axis',(1.,0.,0.));
#69709=DIRECTION('',(0.707106781186537,8.6595605623548E-17,-0.707106781186558));
#69710=DIRECTION('center_axis',(0.,0.,-1.));
#69711=DIRECTION('ref_axis',(1.,0.,0.));
#69712=DIRECTION('center_axis',(0.,0.,-1.));
#69713=DIRECTION('ref_axis',(1.,0.,0.));
#69714=DIRECTION('center_axis',(0.,0.,-1.));
#69715=DIRECTION('ref_axis',(6.12323399573677E-17,-1.,0.));
#69716=DIRECTION('',(0.,0.,-1.));
#69717=DIRECTION('',(0.,0.,-1.));
#69718=DIRECTION('',(0.,0.,-1.));
#69719=DIRECTION('',(0.,0.,-1.));
#69720=DIRECTION('center_axis',(0.,0.,-1.));
#69721=DIRECTION('ref_axis',(1.,0.,0.));
#69722=DIRECTION('',(0.,0.,-1.));
#69723=DIRECTION('center_axis',(0.,0.,1.));
#69724=DIRECTION('ref_axis',(1.,0.,0.));
#69725=DIRECTION('',(0.,0.,1.));
#69726=DIRECTION('center_axis',(0.,0.,-1.));
#69727=DIRECTION('ref_axis',(1.,0.,0.));
#69728=DIRECTION('center_axis',(0.,0.,1.));
#69729=DIRECTION('ref_axis',(1.,0.,0.));
#69730=DIRECTION('',(-0.857167300702114,-1.04972719113862E-16,0.515038074910052));
#69731=DIRECTION('center_axis',(0.,0.,-1.));
#69732=DIRECTION('ref_axis',(1.,0.,0.));
#69733=DIRECTION('center_axis',(0.,0.,-1.));
#69734=DIRECTION('ref_axis',(1.,0.,0.));
#69735=DIRECTION('center_axis',(0.,0.,-1.));
#69736=DIRECTION('ref_axis',(1.,0.,0.));
#69737=DIRECTION('',(0.,0.,-1.));
#69738=DIRECTION('center_axis',(0.,0.,1.));
#69739=DIRECTION('ref_axis',(1.,0.,0.));
#69740=DIRECTION('',(-1.,0.,0.));
#69741=DIRECTION('center_axis',(0.,1.,0.));
#69742=DIRECTION('ref_axis',(0.,0.,1.));
#69743=DIRECTION('',(1.,0.,0.));
#69744=DIRECTION('',(0.,0.,1.));
#69745=DIRECTION('',(1.,0.,0.));
#69746=DIRECTION('',(0.,0.,-1.));
#69747=DIRECTION('',(1.,0.,0.));
#69748=DIRECTION('center_axis',(0.,0.,-1.));
#69749=DIRECTION('ref_axis',(0.,1.,0.));
#69750=DIRECTION('',(-1.,0.,0.));
#69751=DIRECTION('',(0.,-1.,0.));
#69752=DIRECTION('',(0.,1.,0.));
#69753=DIRECTION('center_axis',(0.,0.,1.));
#69754=DIRECTION('ref_axis',(0.,-1.,0.));
#69755=DIRECTION('',(0.,1.,0.));
#69756=DIRECTION('',(1.,0.,0.));
#69757=DIRECTION('',(0.,-1.,0.));
#69758=DIRECTION('center_axis',(1.,0.,0.));
#69759=DIRECTION('ref_axis',(0.,0.,-1.));
#69760=DIRECTION('',(0.,0.,1.));
#69761=DIRECTION('',(0.,-0.866025403784439,-0.499999999999999));
#69762=DIRECTION('',(0.,0.,-1.));
#69763=DIRECTION('',(0.,-1.,0.));
#69764=DIRECTION('',(0.,0.,1.));
#69765=DIRECTION('',(0.,1.,0.));
#69766=DIRECTION('',(0.,0.,-1.));
#69767=DIRECTION('',(0.,0.866025403784439,-0.5));
#69768=DIRECTION('',(0.,0.,1.));
#69769=DIRECTION('center_axis',(0.,1.,0.));
#69770=DIRECTION('ref_axis',(0.,0.,1.));
#69771=DIRECTION('',(0.,0.,-1.));
#69772=DIRECTION('',(1.,0.,0.));
#69773=DIRECTION('center_axis',(0.,-0.499999999999999,0.866025403784439));
#69774=DIRECTION('ref_axis',(0.,-0.866025403784439,-0.499999999999999));
#69775=DIRECTION('',(0.654653670707982,-0.654653670707974,-0.377964473009224));
#69776=DIRECTION('',(0.,0.866025403784439,0.499999999999999));
#69777=DIRECTION('',(0.654653670707982,0.654653670707974,0.377964473009224));
#69778=DIRECTION('',(1.,0.,0.));
#69779=DIRECTION('center_axis',(0.,-0.5,-0.866025403784439));
#69780=DIRECTION('ref_axis',(0.,0.866025403784439,-0.5));
#69781=DIRECTION('',(-0.654653670707982,0.654653670707974,-0.377964473009225));
#69782=DIRECTION('',(-1.,0.,0.));
#69783=DIRECTION('',(-0.654653670707982,-0.654653670707974,0.377964473009225));
#69784=DIRECTION('',(0.,-0.866025403784439,0.5));
#69785=DIRECTION('',(1.,0.,0.));
#69786=DIRECTION('center_axis',(0.,1.,0.));
#69787=DIRECTION('ref_axis',(0.,0.,1.));
#69788=DIRECTION('',(0.,0.,-1.));
#69789=DIRECTION('center_axis',(-0.707106781186543,-0.707106781186552,0.));
#69790=DIRECTION('ref_axis',(0.,0.,1.));
#69791=DIRECTION('',(0.,0.,1.));
#69792=DIRECTION('',(-0.707106781186552,0.707106781186543,1.25607396694701E-14));
#69793=DIRECTION('center_axis',(-0.707106781186543,-0.707106781186552,0.));
#69794=DIRECTION('ref_axis',(0.,0.,1.));
#69795=DIRECTION('',(0.707106781186552,-0.707106781186543,0.));
#69796=DIRECTION('',(0.,0.,1.));
#69797=DIRECTION('center_axis',(0.,-1.,0.));
#69798=DIRECTION('ref_axis',(0.,0.,-1.));
#69799=DIRECTION('',(0.,0.,-1.));
#69800=DIRECTION('',(1.,0.,0.));
#69801=DIRECTION('center_axis',(0.707106781186543,-0.707106781186552,0.));
#69802=DIRECTION('ref_axis',(0.,0.,-1.));
#69803=DIRECTION('',(0.,0.,1.));
#69804=DIRECTION('',(-0.707106781186552,-0.707106781186543,-1.25607396694701E-14));
#69805=DIRECTION('center_axis',(0.577350269189616,-0.577350269189634,0.577350269189627));
#69806=DIRECTION('ref_axis',(0.707106781186554,0.,-0.707106781186541));
#69807=DIRECTION('',(0.707106781186554,0.,-0.707106781186541));
#69808=DIRECTION('',(0.,0.707106781186543,0.707106781186552));
#69809=DIRECTION('center_axis',(0.577350269189619,0.577350269189629,0.577350269189629));
#69810=DIRECTION('ref_axis',(0.707106781186554,0.,-0.707106781186541));
#69811=DIRECTION('',(0.707106781186554,-0.707106781186541,0.));
#69812=DIRECTION('',(-0.707106781186554,0.,0.707106781186541));
#69813=DIRECTION('center_axis',(-0.577350269189616,-0.577350269189634,0.577350269189627));
#69814=DIRECTION('ref_axis',(0.707106781186554,0.,0.707106781186541));
#69815=DIRECTION('',(0.,-0.707106781186543,-0.707106781186552));
#69816=DIRECTION('',(0.707106781186554,0.,0.707106781186541));
#69817=DIRECTION('center_axis',(0.577350269189621,-0.577350269189627,-0.57735026918963));
#69818=DIRECTION('ref_axis',(-0.707106781186553,0.,-0.707106781186542));
#69819=DIRECTION('',(0.707106781186552,0.707106781186543,0.));
#69820=DIRECTION('',(-0.707106781186552,1.57009245868376E-15,-0.707106781186543));
#69821=DIRECTION('center_axis',(-0.577350269189619,0.577350269189629,0.577350269189629));
#69822=DIRECTION('ref_axis',(0.707106781186554,0.,0.707106781186541));
#69823=DIRECTION('',(0.707106781186554,0.707106781186541,0.));
#69824=DIRECTION('',(-0.707106781186554,0.,-0.707106781186541));
#69825=DIRECTION('center_axis',(0.57735026918962,0.577350269189629,-0.577350269189628));
#69826=DIRECTION('ref_axis',(-0.707106781186552,0.,-0.707106781186543));
#69827=DIRECTION('',(0.707106781186552,0.,0.707106781186543));
#69828=DIRECTION('',(0.,-0.707106781186547,-0.707106781186548));
#69829=DIRECTION('',(-0.707106781186554,0.707106781186541,-1.57009245868377E-15));
#69830=DIRECTION('center_axis',(-0.57735026918962,-0.577350269189628,-0.577350269189629));
#69831=DIRECTION('ref_axis',(-0.707106781186553,0.,0.707106781186542));
#69832=DIRECTION('',(-0.707106781186552,-1.57009245868376E-15,0.707106781186543));
#69833=DIRECTION('center_axis',(-0.57735026918962,0.577350269189629,-0.577350269189628));
#69834=DIRECTION('ref_axis',(-0.707106781186552,0.,0.707106781186543));
#69835=DIRECTION('',(0.707106781186552,0.,-0.707106781186543));
#69836=DIRECTION('',(-0.707106781186554,-0.707106781186541,1.57009245868377E-15));
#69837=DIRECTION('',(0.,0.707106781186547,0.707106781186548));
#69838=DIRECTION('center_axis',(-0.707106781186541,0.707106781186554,0.));
#69839=DIRECTION('ref_axis',(0.,0.,1.));
#69840=DIRECTION('center_axis',(0.,0.707106781186548,-0.707106781186547));
#69841=DIRECTION('ref_axis',(-1.,0.,0.));
#69842=DIRECTION('center_axis',(-0.707106781186543,0.,-0.707106781186552));
#69843=DIRECTION('ref_axis',(-0.707106781186552,0.,0.707106781186543));
#69844=DIRECTION('center_axis',(0.707106781186541,0.707106781186554,0.));
#69845=DIRECTION('ref_axis',(0.,0.,-1.));
#69846=DIRECTION('',(0.,0.,-1.));
#69847=DIRECTION('center_axis',(0.707106781186543,0.,-0.707106781186552));
#69848=DIRECTION('ref_axis',(-0.707106781186552,0.,-0.707106781186543));
#69849=DIRECTION('',(0.,-1.,0.));
#69850=DIRECTION('center_axis',(-0.707106781186541,0.,0.707106781186554));
#69851=DIRECTION('ref_axis',(0.707106781186554,0.,0.707106781186541));
#69852=DIRECTION('center_axis',(0.707106781186543,-0.707106781186552,0.));
#69853=DIRECTION('ref_axis',(0.,0.,-1.));
#69854=DIRECTION('',(0.,0.,-1.));
#69855=DIRECTION('',(0.,0.,1.));
#69856=DIRECTION('center_axis',(0.,-0.707106781186552,0.707106781186543));
#69857=DIRECTION('ref_axis',(1.,0.,0.));
#69858=DIRECTION('center_axis',(0.707106781186541,0.,0.707106781186554));
#69859=DIRECTION('ref_axis',(0.707106781186554,0.,-0.707106781186541));
#69860=DIRECTION('',(0.,1.,0.));
#69861=DIRECTION('center_axis',(0.,-1.,0.));
#69862=DIRECTION('ref_axis',(0.,0.,-1.));
#69863=DIRECTION('center_axis',(1.,0.,0.));
#69864=DIRECTION('ref_axis',(0.,0.,-1.));
#69865=DIRECTION('axis',(0.,0.,1.));
#69866=DIRECTION('refdir',(1.,0.,0.));
#69867=DIRECTION('center_axis',(0.,0.,-1.));
#69868=DIRECTION('ref_axis',(1.,0.,0.));
#69869=DIRECTION('center_axis',(0.,0.5,0.866025403784439));
#69870=DIRECTION('ref_axis',(2.56395024851139E-14,-0.866025403784439,0.5));
#69871=DIRECTION('',(0.707106781186549,8.65956056235495E-17,0.707106781186546));
#69872=DIRECTION('center_axis',(0.,0.,-1.));
#69873=DIRECTION('ref_axis',(1.,0.,0.));
#69874=DIRECTION('center_axis',(0.,0.5,0.866025403784439));
#69875=DIRECTION('ref_axis',(2.56395024851139E-14,-0.866025403784439,0.5));
#69876=DIRECTION('',(0.707106781186549,8.65956056235495E-17,0.707106781186546));
#69877=DIRECTION('center_axis',(0.,0.,-1.));
#69878=DIRECTION('ref_axis',(1.,0.,0.));
#69879=DIRECTION('center_axis',(0.,0.5,0.866025403784439));
#69880=DIRECTION('ref_axis',(2.56395024851139E-14,-0.866025403784439,0.5));
#69881=DIRECTION('',(0.707106781186549,8.65956056235495E-17,0.707106781186546));
#69882=DIRECTION('center_axis',(0.707106781186555,0.70710678118654,0.));
#69883=DIRECTION('ref_axis',(0.,0.,-1.));
#69884=DIRECTION('',(0.,0.,-1.));
#69885=DIRECTION('',(-0.447213595499949,0.447213595499959,-0.774596669241488));
#69886=DIRECTION('',(0.,0.,1.));
#69887=DIRECTION('',(-0.654653670707967,0.654653670707982,0.377964473009236));
#69888=DIRECTION('center_axis',(0.707106781186556,-0.35355339059327,-0.612372435695787));
#69889=DIRECTION('ref_axis',(-0.654653670707968,0.,-0.755928946018463));
#69890=DIRECTION('',(0.,-0.866025403784439,0.5));
#69891=DIRECTION('',(-0.654653670707969,-0.654653670707984,-0.37796447300923));
#69892=DIRECTION('',(0.,0.866025403784439,-0.5));
#69893=DIRECTION('center_axis',(0.707106781186555,-0.70710678118654,0.));
#69894=DIRECTION('ref_axis',(0.,0.,-1.));
#69895=DIRECTION('',(0.,0.,1.));
#69896=DIRECTION('',(-0.447213595499949,-0.447213595499959,0.774596669241488));
#69897=DIRECTION('',(0.,0.,-1.));
#69898=DIRECTION('center_axis',(0.707106781186556,0.35355339059327,0.612372435695787));
#69899=DIRECTION('ref_axis',(0.654653670707968,0.,-0.755928946018463));
#69900=DIRECTION('',(0.,-0.866025403784439,0.5));
#69901=DIRECTION('',(0.,0.866025403784439,-0.5));
#69902=DIRECTION('center_axis',(0.,0.5,0.866025403784439));
#69903=DIRECTION('ref_axis',(0.,-0.866025403784439,0.5));
#69904=DIRECTION('',(1.,0.,0.));
#69905=DIRECTION('',(0.,0.866025403784439,-0.5));
#69906=DIRECTION('',(1.,0.,0.));
#69907=DIRECTION('center_axis',(0.,1.,0.));
#69908=DIRECTION('ref_axis',(0.,0.,1.));
#69909=DIRECTION('',(1.,0.,0.));
#69910=DIRECTION('',(0.,0.,-1.));
#69911=DIRECTION('center_axis',(1.,0.,0.));
#69912=DIRECTION('ref_axis',(0.,0.,-1.));
#69913=DIRECTION('center_axis',(-0.707106781186555,0.70710678118654,0.));
#69914=DIRECTION('ref_axis',(0.,0.,1.));
#69915=DIRECTION('',(0.,0.,1.));
#69916=DIRECTION('',(0.654653670707967,0.654653670707982,0.377964473009236));
#69917=DIRECTION('',(0.447213595499949,0.447213595499959,-0.774596669241488));
#69918=DIRECTION('center_axis',(-0.707106781186556,0.35355339059327,0.612372435695787));
#69919=DIRECTION('ref_axis',(0.654653670707968,0.,0.755928946018463));
#69920=DIRECTION('',(0.,-0.866025403784439,0.5));
#69921=DIRECTION('',(0.447213595499949,-0.447213595499959,0.774596669241488));
#69922=DIRECTION('center_axis',(-0.707106781186556,-0.35355339059327,-0.612372435695787));
#69923=DIRECTION('ref_axis',(-0.654653670707968,0.,0.755928946018463));
#69924=DIRECTION('',(0.,-0.866025403784439,0.5));
#69925=DIRECTION('',(-0.654653670707969,0.654653670707984,0.37796447300923));
#69926=DIRECTION('',(0.,0.866025403784439,-0.5));
#69927=DIRECTION('center_axis',(-0.707106781186555,-0.70710678118654,0.));
#69928=DIRECTION('ref_axis',(0.,0.,1.));
#69929=DIRECTION('',(0.,0.,-1.));
#69930=DIRECTION('',(0.,0.,1.));
#69931=DIRECTION('center_axis',(0.,-0.5,-0.866025403784439));
#69932=DIRECTION('ref_axis',(0.,0.866025403784439,-0.5));
#69933=DIRECTION('',(1.,0.,0.));
#69934=DIRECTION('center_axis',(1.,0.,0.));
#69935=DIRECTION('ref_axis',(0.,0.,-1.));
#69936=DIRECTION('center_axis',(0.,-1.,0.));
#69937=DIRECTION('ref_axis',(0.,0.,-1.));
#69938=DIRECTION('axis',(0.,0.,1.));
#69939=DIRECTION('refdir',(1.,0.,0.));
#69940=DIRECTION('center_axis',(0.,0.,-1.));
#69941=DIRECTION('ref_axis',(-1.,0.,0.));
#69942=DIRECTION('center_axis',(0.,0.,-1.));
#69943=DIRECTION('ref_axis',(1.,0.,0.));
#69944=DIRECTION('',(1.,0.,0.));
#69945=DIRECTION('center_axis',(0.,0.,1.));
#69946=DIRECTION('ref_axis',(1.,0.,0.));
#69947=DIRECTION('center_axis',(0.,0.,1.));
#69948=DIRECTION('ref_axis',(1.,0.,0.));
#69949=DIRECTION('',(-1.,0.,0.));
#69950=DIRECTION('center_axis',(0.,1.,0.));
#69951=DIRECTION('ref_axis',(1.,0.,0.));
#69952=DIRECTION('',(0.,0.,-1.));
#69953=DIRECTION('',(0.,0.,1.));
#69954=DIRECTION('center_axis',(0.,0.,-1.));
#69955=DIRECTION('ref_axis',(-1.,0.,0.));
#69956=DIRECTION('center_axis',(0.,0.,-1.));
#69957=DIRECTION('ref_axis',(1.,0.,0.));
#69958=DIRECTION('',(1.,0.,0.));
#69959=DIRECTION('center_axis',(0.,0.,1.));
#69960=DIRECTION('ref_axis',(1.,0.,0.));
#69961=DIRECTION('center_axis',(0.,0.,1.));
#69962=DIRECTION('ref_axis',(1.,0.,0.));
#69963=DIRECTION('',(-1.,0.,0.));
#69964=DIRECTION('center_axis',(0.,1.,0.));
#69965=DIRECTION('ref_axis',(1.,0.,0.));
#69966=DIRECTION('',(0.,0.,-1.));
#69967=DIRECTION('',(0.,0.,1.));
#69968=DIRECTION('center_axis',(0.,0.,-1.));
#69969=DIRECTION('ref_axis',(-1.,0.,0.));
#69970=DIRECTION('center_axis',(0.,0.,1.));
#69971=DIRECTION('ref_axis',(1.,0.,0.));
#69972=DIRECTION('center_axis',(0.,0.,1.));
#69973=DIRECTION('ref_axis',(1.,0.,0.));
#69974=DIRECTION('center_axis',(0.,0.,1.));
#69975=DIRECTION('ref_axis',(1.,0.,0.));
#69976=DIRECTION('',(0.70710678118654,8.65956056235484E-17,-0.707106781186555));
#69977=DIRECTION('center_axis',(0.,0.,1.));
#69978=DIRECTION('ref_axis',(1.,0.,0.));
#69979=DIRECTION('center_axis',(0.,0.,1.));
#69980=DIRECTION('ref_axis',(1.,0.,0.));
#69981=DIRECTION('',(0.,0.,-1.));
#69982=DIRECTION('center_axis',(0.,0.,-1.));
#69983=DIRECTION('ref_axis',(1.,0.,0.));
#69984=DIRECTION('center_axis',(0.,0.,1.));
#69985=DIRECTION('ref_axis',(1.,0.,0.));
#69986=DIRECTION('',(-0.707106781186548,-8.65956056235493E-17,-0.707106781186548));
#69987=DIRECTION('center_axis',(0.,0.,1.));
#69988=DIRECTION('ref_axis',(1.,0.,0.));
#69989=DIRECTION('axis',(0.,0.,1.));
#69990=DIRECTION('refdir',(1.,0.,0.));
#69991=DIRECTION('center_axis',(0.,1.,0.));
#69992=DIRECTION('ref_axis',(1.,0.,0.));
#69993=DIRECTION('',(0.,0.,-1.));
#69994=DIRECTION('center_axis',(0.,-1.,0.));
#69995=DIRECTION('ref_axis',(1.,0.,0.));
#69996=DIRECTION('center_axis',(0.,-1.,0.));
#69997=DIRECTION('ref_axis',(1.,0.,0.));
#69998=DIRECTION('',(0.,-1.,0.));
#69999=DIRECTION('center_axis',(0.,-1.,0.));
#70000=DIRECTION('ref_axis',(1.,0.,0.));
#70001=DIRECTION('center_axis',(0.,-1.,0.));
#70002=DIRECTION('ref_axis',(1.,0.,0.));
#70003=DIRECTION('center_axis',(0.,1.,0.));
#70004=DIRECTION('ref_axis',(1.,0.,0.));
#70005=DIRECTION('',(0.,0.,1.));
#70006=DIRECTION('center_axis',(0.959768443582426,-0.280792689903722,0.));
#70007=DIRECTION('ref_axis',(-0.280792689903722,-0.959768443582426,0.));
#70008=DIRECTION('',(0.,0.,-1.));
#70009=DIRECTION('',(0.280792689903722,0.959768443582426,0.));
#70010=DIRECTION('',(0.,0.,-1.));
#70011=DIRECTION('',(-0.280792689903722,-0.959768443582426,0.));
#70012=DIRECTION('center_axis',(-0.877209189964524,0.48010835968746,0.));
#70013=DIRECTION('ref_axis',(0.48010835968746,0.877209189964524,0.));
#70014=DIRECTION('',(0.,0.,1.));
#70015=DIRECTION('',(0.48010835968746,0.877209189964524,0.));
#70016=DIRECTION('',(0.,0.,-1.));
#70017=DIRECTION('',(-0.48010835968746,-0.877209189964524,0.));
#70018=DIRECTION('',(0.,0.,-1.));
#70019=DIRECTION('center_axis',(0.,0.,-1.));
#70020=DIRECTION('ref_axis',(-0.412031471605199,-0.911169614510303,0.));
#70021=DIRECTION('center_axis',(0.,0.,1.));
#70022=DIRECTION('ref_axis',(-0.412031471605199,-0.911169614510303,0.));
#70023=DIRECTION('center_axis',(0.,0.,-1.));
#70024=DIRECTION('ref_axis',(-0.412031471605199,-0.911169614510303,0.));
#70025=DIRECTION('',(0.,0.,-1.));
#70026=DIRECTION('center_axis',(0.,0.,1.));
#70027=DIRECTION('ref_axis',(0.923879532511286,-0.38268343236509,0.));
#70028=DIRECTION('center_axis',(0.,0.,1.));
#70029=DIRECTION('ref_axis',(1.,0.,0.));
#70030=DIRECTION('center_axis',(0.,0.,1.));
#70031=DIRECTION('ref_axis',(1.,0.,0.));
#70032=DIRECTION('center_axis',(0.,0.,1.));
#70033=DIRECTION('ref_axis',(1.,0.,0.));
#70034=DIRECTION('',(0.,0.,-1.));
#70035=DIRECTION('center_axis',(0.,0.,1.));
#70036=DIRECTION('ref_axis',(1.,0.,0.));
#70037=DIRECTION('',(0.,0.,-1.));
#70038=DIRECTION('center_axis',(0.,0.,1.));
#70039=DIRECTION('ref_axis',(1.,0.,0.));
#70040=DIRECTION('',(0.,0.,1.));
#70041=DIRECTION('center_axis',(0.,0.,1.));
#70042=DIRECTION('ref_axis',(1.,0.,0.));
#70043=DIRECTION('',(0.,0.,-1.));
#70044=DIRECTION('center_axis',(0.,0.,1.));
#70045=DIRECTION('ref_axis',(1.,0.,0.));
#70046=DIRECTION('',(0.,0.,1.));
#70047=DIRECTION('center_axis',(0.,0.,1.));
#70048=DIRECTION('ref_axis',(1.,0.,0.));
#70049=DIRECTION('',(0.,0.,-1.));
#70050=DIRECTION('center_axis',(0.,0.,1.));
#70051=DIRECTION('ref_axis',(1.,0.,0.));
#70052=DIRECTION('center_axis',(0.,0.,1.));
#70053=DIRECTION('ref_axis',(1.,0.,0.));
#70054=DIRECTION('',(0.,0.,1.));
#70055=DIRECTION('center_axis',(0.,0.,1.));
#70056=DIRECTION('ref_axis',(1.,0.,0.));
#70057=DIRECTION('',(0.,0.,-1.));
#70058=DIRECTION('center_axis',(0.,0.,1.));
#70059=DIRECTION('ref_axis',(1.,0.,0.));
#70060=DIRECTION('',(0.,0.,1.));
#70061=DIRECTION('center_axis',(0.,0.,1.));
#70062=DIRECTION('ref_axis',(1.,0.,0.));
#70063=DIRECTION('',(0.,0.,-1.));
#70064=DIRECTION('center_axis',(0.,0.,1.));
#70065=DIRECTION('ref_axis',(1.,0.,0.));
#70066=DIRECTION('',(0.,0.,1.));
#70067=DIRECTION('center_axis',(0.,0.,1.));
#70068=DIRECTION('ref_axis',(1.,0.,0.));
#70069=DIRECTION('',(0.,0.,-1.));
#70070=DIRECTION('center_axis',(0.,0.,1.));
#70071=DIRECTION('ref_axis',(1.,0.,0.));
#70072=DIRECTION('',(0.,0.,1.));
#70073=DIRECTION('center_axis',(0.,0.,1.));
#70074=DIRECTION('ref_axis',(1.,0.,0.));
#70075=DIRECTION('',(0.,0.,-1.));
#70076=DIRECTION('center_axis',(0.,0.,1.));
#70077=DIRECTION('ref_axis',(1.,0.,0.));
#70078=DIRECTION('',(0.,0.,1.));
#70079=DIRECTION('center_axis',(0.,0.,1.));
#70080=DIRECTION('ref_axis',(1.,0.,0.));
#70081=DIRECTION('',(0.,0.,-1.));
#70082=DIRECTION('center_axis',(0.,0.,1.));
#70083=DIRECTION('ref_axis',(1.,0.,0.));
#70084=DIRECTION('',(0.,0.,1.));
#70085=DIRECTION('center_axis',(0.,0.,1.));
#70086=DIRECTION('ref_axis',(1.,0.,0.));
#70087=DIRECTION('',(0.,0.,-1.));
#70088=DIRECTION('center_axis',(0.,0.,1.));
#70089=DIRECTION('ref_axis',(1.,0.,0.));
#70090=DIRECTION('',(0.,0.,1.));
#70091=DIRECTION('center_axis',(0.,0.,1.));
#70092=DIRECTION('ref_axis',(1.,0.,0.));
#70093=DIRECTION('',(0.,0.,-1.));
#70094=DIRECTION('center_axis',(0.,0.,1.));
#70095=DIRECTION('ref_axis',(1.,0.,0.));
#70096=DIRECTION('',(0.,0.,1.));
#70097=DIRECTION('center_axis',(0.,0.,1.));
#70098=DIRECTION('ref_axis',(1.,0.,0.));
#70099=DIRECTION('',(0.,0.,-1.));
#70100=DIRECTION('center_axis',(0.,0.,1.));
#70101=DIRECTION('ref_axis',(1.,0.,0.));
#70102=DIRECTION('',(0.,0.,1.));
#70103=DIRECTION('center_axis',(0.,0.,1.));
#70104=DIRECTION('ref_axis',(1.,0.,0.));
#70105=DIRECTION('',(0.,0.,-1.));
#70106=DIRECTION('center_axis',(0.,0.,1.));
#70107=DIRECTION('ref_axis',(1.,0.,0.));
#70108=DIRECTION('',(0.,0.,1.));
#70109=DIRECTION('center_axis',(0.,0.,1.));
#70110=DIRECTION('ref_axis',(1.,0.,0.));
#70111=DIRECTION('',(0.,0.,-1.));
#70112=DIRECTION('center_axis',(0.,0.,1.));
#70113=DIRECTION('ref_axis',(1.,0.,0.));
#70114=DIRECTION('',(0.,0.,1.));
#70115=DIRECTION('center_axis',(0.,0.,1.));
#70116=DIRECTION('ref_axis',(1.,0.,0.));
#70117=DIRECTION('',(0.,0.,-1.));
#70118=DIRECTION('center_axis',(0.,0.,1.));
#70119=DIRECTION('ref_axis',(1.,0.,0.));
#70120=DIRECTION('',(0.,0.,1.));
#70121=DIRECTION('center_axis',(0.,0.,1.));
#70122=DIRECTION('ref_axis',(1.,0.,0.));
#70123=DIRECTION('',(0.,0.,-1.));
#70124=DIRECTION('center_axis',(0.,0.,1.));
#70125=DIRECTION('ref_axis',(1.,0.,0.));
#70126=DIRECTION('',(0.,0.,1.));
#70127=DIRECTION('center_axis',(0.,0.,1.));
#70128=DIRECTION('ref_axis',(1.,0.,0.));
#70129=DIRECTION('center_axis',(0.779255710620635,-0.626706101346659,0.));
#70130=DIRECTION('ref_axis',(-0.626706101346659,-0.779255710620635,0.));
#70131=DIRECTION('',(0.626706101346659,0.779255710620635,0.));
#70132=DIRECTION('',(0.,0.,-1.));
#70133=DIRECTION('',(-0.626706101346659,-0.779255710620635,0.));
#70134=DIRECTION('center_axis',(-0.626706101346659,0.779255710620635,0.));
#70135=DIRECTION('ref_axis',(0.779255710620635,0.626706101346659,0.));
#70136=DIRECTION('',(0.779255710620635,0.626706101346659,0.));
#70137=DIRECTION('',(0.,0.,-1.));
#70138=DIRECTION('',(-0.779255710620635,-0.626706101346659,0.));
#70139=DIRECTION('',(0.,0.,-1.));
#70140=DIRECTION('center_axis',(0.,0.,-1.));
#70141=DIRECTION('ref_axis',(-0.729356958914127,-0.684133339695952,0.));
#70142=DIRECTION('center_axis',(0.,0.,1.));
#70143=DIRECTION('ref_axis',(-0.729356958914127,-0.684133339695952,0.));
#70144=DIRECTION('center_axis',(0.,0.,-1.));
#70145=DIRECTION('ref_axis',(-0.729356958914127,-0.684133339695952,0.));
#70146=DIRECTION('',(0.,0.,-1.));
#70147=DIRECTION('center_axis',(0.,0.,1.));
#70148=DIRECTION('ref_axis',(0.707106781186547,-0.707106781186548,0.));
#70149=DIRECTION('center_axis',(0.48010835968746,-0.877209189964524,0.));
#70150=DIRECTION('ref_axis',(-0.877209189964524,-0.48010835968746,0.));
#70151=DIRECTION('',(0.877209189964524,0.48010835968746,0.));
#70152=DIRECTION('',(0.,0.,-1.));
#70153=DIRECTION('',(-0.877209189964524,-0.48010835968746,0.));
#70154=DIRECTION('center_axis',(-0.280792689903721,0.959768443582426,0.));
#70155=DIRECTION('ref_axis',(0.959768443582426,0.280792689903721,0.));
#70156=DIRECTION('',(0.959768443582426,0.280792689903721,0.));
#70157=DIRECTION('',(0.,0.,-1.));
#70158=DIRECTION('',(-0.959768443582426,-0.280792689903721,0.));
#70159=DIRECTION('',(0.,0.,-1.));
#70160=DIRECTION('center_axis',(0.,0.,-1.));
#70161=DIRECTION('ref_axis',(-0.935644460865676,-0.35294396559706,0.));
#70162=DIRECTION('center_axis',(0.,0.,1.));
#70163=DIRECTION('ref_axis',(-0.935644460865676,-0.35294396559706,0.));
#70164=DIRECTION('center_axis',(0.,0.,-1.));
#70165=DIRECTION('ref_axis',(-0.935644460865676,-0.35294396559706,0.));
#70166=DIRECTION('',(0.,0.,-1.));
#70167=DIRECTION('center_axis',(0.,0.,1.));
#70168=DIRECTION('ref_axis',(0.38268343236509,-0.923879532511287,0.));
#70169=DIRECTION('center_axis',(0.107868863184986,-0.994165131331399,0.));
#70170=DIRECTION('ref_axis',(-0.994165131331399,-0.107868863184986,0.));
#70171=DIRECTION('',(0.994165131331399,0.107868863184986,0.));
#70172=DIRECTION('',(0.,0.,-1.));
#70173=DIRECTION('',(-0.994165131331399,-0.107868863184986,0.));
#70174=DIRECTION('center_axis',(0.107868863184987,0.994165131331399,0.));
#70175=DIRECTION('ref_axis',(0.994165131331399,-0.107868863184987,0.));
#70176=DIRECTION('',(0.994165131331399,-0.107868863184987,0.));
#70177=DIRECTION('',(0.,0.,-1.));
#70178=DIRECTION('',(-0.994165131331399,0.107868863184987,0.));
#70179=DIRECTION('',(0.,0.,-1.));
#70180=DIRECTION('center_axis',(0.,0.,-1.));
#70181=DIRECTION('ref_axis',(-0.999488575288585,0.0319779278189696,0.));
#70182=DIRECTION('center_axis',(0.,0.,1.));
#70183=DIRECTION('ref_axis',(-0.999488575288585,0.0319779278189696,0.));
#70184=DIRECTION('center_axis',(0.,0.,-1.));
#70185=DIRECTION('ref_axis',(-0.999488575288585,0.0319779278189696,0.));
#70186=DIRECTION('',(0.,0.,-1.));
#70187=DIRECTION('center_axis',(0.,0.,1.));
#70188=DIRECTION('ref_axis',(-1.83697019872103E-16,-1.,0.));
#70189=DIRECTION('center_axis',(-0.280792689903722,-0.959768443582426,0.));
#70190=DIRECTION('ref_axis',(-0.959768443582426,0.280792689903722,0.));
#70191=DIRECTION('',(0.959768443582426,-0.280792689903722,0.));
#70192=DIRECTION('',(0.,0.,-1.));
#70193=DIRECTION('',(-0.959768443582426,0.280792689903722,0.));
#70194=DIRECTION('center_axis',(0.48010835968746,0.877209189964524,0.));
#70195=DIRECTION('ref_axis',(0.877209189964524,-0.48010835968746,0.));
#70196=DIRECTION('',(0.877209189964524,-0.48010835968746,0.));
#70197=DIRECTION('',(0.,0.,-1.));
#70198=DIRECTION('',(-0.877209189964524,0.48010835968746,0.));
#70199=DIRECTION('',(0.,0.,-1.));
#70200=DIRECTION('center_axis',(0.,0.,-1.));
#70201=DIRECTION('ref_axis',(-0.911169614510303,0.412031471605199,0.));
#70202=DIRECTION('center_axis',(0.,0.,1.));
#70203=DIRECTION('ref_axis',(-0.911169614510303,0.412031471605199,0.));
#70204=DIRECTION('center_axis',(0.,0.,-1.));
#70205=DIRECTION('ref_axis',(-0.911169614510303,0.412031471605199,0.));
#70206=DIRECTION('',(0.,0.,-1.));
#70207=DIRECTION('center_axis',(0.,0.,1.));
#70208=DIRECTION('ref_axis',(-0.38268343236509,-0.923879532511286,0.));
#70209=DIRECTION('center_axis',(-0.626706101346659,-0.779255710620635,0.));
#70210=DIRECTION('ref_axis',(-0.779255710620635,0.626706101346659,0.));
#70211=DIRECTION('',(0.779255710620635,-0.626706101346659,0.));
#70212=DIRECTION('',(0.,0.,-1.));
#70213=DIRECTION('',(-0.779255710620635,0.626706101346659,0.));
#70214=DIRECTION('center_axis',(0.779255710620635,0.626706101346659,0.));
#70215=DIRECTION('ref_axis',(0.626706101346659,-0.779255710620635,0.));
#70216=DIRECTION('',(0.626706101346659,-0.779255710620635,0.));
#70217=DIRECTION('',(0.,0.,-1.));
#70218=DIRECTION('',(-0.626706101346659,0.779255710620635,0.));
#70219=DIRECTION('',(0.,0.,-1.));
#70220=DIRECTION('center_axis',(0.,0.,-1.));
#70221=DIRECTION('ref_axis',(-0.684133339695952,0.729356958914127,0.));
#70222=DIRECTION('center_axis',(0.,0.,1.));
#70223=DIRECTION('ref_axis',(-0.684133339695952,0.729356958914127,0.));
#70224=DIRECTION('center_axis',(0.,0.,-1.));
#70225=DIRECTION('ref_axis',(-0.684133339695952,0.729356958914127,0.));
#70226=DIRECTION('',(0.,0.,-1.));
#70227=DIRECTION('center_axis',(0.,0.,1.));
#70228=DIRECTION('ref_axis',(-0.707106781186548,-0.707106781186547,0.));
#70229=DIRECTION('center_axis',(-0.877209189964525,-0.480108359687459,0.));
#70230=DIRECTION('ref_axis',(-0.480108359687459,0.877209189964524,0.));
#70231=DIRECTION('',(0.480108359687459,-0.877209189964524,0.));
#70232=DIRECTION('',(0.,0.,-1.));
#70233=DIRECTION('',(-0.480108359687459,0.877209189964524,0.));
#70234=DIRECTION('center_axis',(0.959768443582426,0.280792689903721,0.));
#70235=DIRECTION('ref_axis',(0.280792689903721,-0.959768443582426,0.));
#70236=DIRECTION('',(0.280792689903721,-0.959768443582426,0.));
#70237=DIRECTION('',(0.,0.,-1.));
#70238=DIRECTION('',(-0.280792689903721,0.959768443582426,0.));
#70239=DIRECTION('',(0.,0.,-1.));
#70240=DIRECTION('center_axis',(0.,0.,-1.));
#70241=DIRECTION('ref_axis',(-0.35294396559706,0.935644460865676,0.));
#70242=DIRECTION('center_axis',(0.,0.,1.));
#70243=DIRECTION('ref_axis',(-0.35294396559706,0.935644460865676,0.));
#70244=DIRECTION('center_axis',(0.,0.,-1.));
#70245=DIRECTION('ref_axis',(-0.35294396559706,0.935644460865676,0.));
#70246=DIRECTION('',(0.,0.,-1.));
#70247=DIRECTION('center_axis',(0.,0.,1.));
#70248=DIRECTION('ref_axis',(-0.923879532511287,-0.38268343236509,0.));
#70249=DIRECTION('center_axis',(-0.994165131331399,-0.107868863184986,0.));
#70250=DIRECTION('ref_axis',(-0.107868863184986,0.994165131331399,0.));
#70251=DIRECTION('',(0.107868863184986,-0.994165131331399,0.));
#70252=DIRECTION('',(0.,0.,-1.));
#70253=DIRECTION('',(-0.107868863184986,0.994165131331399,0.));
#70254=DIRECTION('center_axis',(0.994165131331399,-0.107868863184987,0.));
#70255=DIRECTION('ref_axis',(-0.107868863184987,-0.994165131331399,0.));
#70256=DIRECTION('',(-0.107868863184987,-0.994165131331399,0.));
#70257=DIRECTION('',(0.,0.,-1.));
#70258=DIRECTION('',(0.107868863184987,0.994165131331399,0.));
#70259=DIRECTION('',(0.,0.,-1.));
#70260=DIRECTION('center_axis',(0.,0.,-1.));
#70261=DIRECTION('ref_axis',(0.0319779278189696,0.999488575288585,0.));
#70262=DIRECTION('center_axis',(0.,0.,1.));
#70263=DIRECTION('ref_axis',(0.0319779278189696,0.999488575288585,0.));
#70264=DIRECTION('center_axis',(0.,0.,-1.));
#70265=DIRECTION('ref_axis',(0.0319779278189696,0.999488575288585,0.));
#70266=DIRECTION('',(0.,0.,-1.));
#70267=DIRECTION('center_axis',(0.,0.,1.));
#70268=DIRECTION('ref_axis',(-1.,1.22464679914735E-16,0.));
#70269=DIRECTION('center_axis',(-0.959768443582426,0.280792689903721,0.));
#70270=DIRECTION('ref_axis',(0.280792689903721,0.959768443582426,0.));
#70271=DIRECTION('',(-0.280792689903721,-0.959768443582426,0.));
#70272=DIRECTION('',(0.,0.,-1.));
#70273=DIRECTION('',(0.280792689903721,0.959768443582426,0.));
#70274=DIRECTION('center_axis',(0.877209189964524,-0.48010835968746,0.));
#70275=DIRECTION('ref_axis',(-0.48010835968746,-0.877209189964524,0.));
#70276=DIRECTION('',(-0.48010835968746,-0.877209189964524,0.));
#70277=DIRECTION('',(0.,0.,-1.));
#70278=DIRECTION('',(0.48010835968746,0.877209189964524,0.));
#70279=DIRECTION('',(0.,0.,-1.));
#70280=DIRECTION('center_axis',(0.,0.,-1.));
#70281=DIRECTION('ref_axis',(0.412031471605198,0.911169614510303,0.));
#70282=DIRECTION('center_axis',(0.,0.,1.));
#70283=DIRECTION('ref_axis',(0.412031471605198,0.911169614510303,0.));
#70284=DIRECTION('center_axis',(0.,0.,-1.));
#70285=DIRECTION('ref_axis',(0.412031471605198,0.911169614510303,0.));
#70286=DIRECTION('',(0.,0.,-1.));
#70287=DIRECTION('center_axis',(0.,0.,1.));
#70288=DIRECTION('ref_axis',(-0.923879532511287,0.38268343236509,0.));
#70289=DIRECTION('center_axis',(-0.779255710620635,0.626706101346659,0.));
#70290=DIRECTION('ref_axis',(0.626706101346659,0.779255710620635,0.));
#70291=DIRECTION('',(-0.626706101346659,-0.779255710620635,0.));
#70292=DIRECTION('',(0.,0.,-1.));
#70293=DIRECTION('',(0.626706101346659,0.779255710620635,0.));
#70294=DIRECTION('center_axis',(0.626706101346659,-0.779255710620635,0.));
#70295=DIRECTION('ref_axis',(-0.779255710620635,-0.626706101346659,0.));
#70296=DIRECTION('',(-0.779255710620635,-0.626706101346659,0.));
#70297=DIRECTION('',(0.,0.,-1.));
#70298=DIRECTION('',(0.779255710620635,0.626706101346659,0.));
#70299=DIRECTION('',(0.,0.,-1.));
#70300=DIRECTION('center_axis',(0.,0.,-1.));
#70301=DIRECTION('ref_axis',(0.729356958914127,0.684133339695952,0.));
#70302=DIRECTION('center_axis',(0.,0.,1.));
#70303=DIRECTION('ref_axis',(0.729356958914127,0.684133339695952,0.));
#70304=DIRECTION('center_axis',(0.,0.,-1.));
#70305=DIRECTION('ref_axis',(0.729356958914127,0.684133339695952,0.));
#70306=DIRECTION('',(0.,0.,-1.));
#70307=DIRECTION('center_axis',(0.,0.,1.));
#70308=DIRECTION('ref_axis',(-0.707106781186547,0.707106781186548,0.));
#70309=DIRECTION('center_axis',(-0.480108359687459,0.877209189964524,0.));
#70310=DIRECTION('ref_axis',(0.877209189964524,0.480108359687459,0.));
#70311=DIRECTION('',(-0.877209189964524,-0.480108359687459,0.));
#70312=DIRECTION('',(0.,0.,-1.));
#70313=DIRECTION('',(0.877209189964524,0.480108359687459,0.));
#70314=DIRECTION('center_axis',(0.280792689903721,-0.959768443582426,0.));
#70315=DIRECTION('ref_axis',(-0.959768443582426,-0.280792689903721,0.));
#70316=DIRECTION('',(-0.959768443582426,-0.280792689903721,0.));
#70317=DIRECTION('',(0.,0.,-1.));
#70318=DIRECTION('',(0.959768443582426,0.280792689903721,0.));
#70319=DIRECTION('',(0.,0.,-1.));
#70320=DIRECTION('center_axis',(0.,0.,-1.));
#70321=DIRECTION('ref_axis',(0.935644460865676,0.35294396559706,0.));
#70322=DIRECTION('center_axis',(0.,0.,1.));
#70323=DIRECTION('ref_axis',(0.935644460865676,0.35294396559706,0.));
#70324=DIRECTION('center_axis',(0.,0.,-1.));
#70325=DIRECTION('ref_axis',(0.935644460865676,0.35294396559706,0.));
#70326=DIRECTION('',(0.,0.,-1.));
#70327=DIRECTION('center_axis',(0.,0.,1.));
#70328=DIRECTION('ref_axis',(-0.38268343236509,0.923879532511287,0.));
#70329=DIRECTION('center_axis',(-0.107868863184986,0.994165131331399,0.));
#70330=DIRECTION('ref_axis',(0.994165131331399,0.107868863184986,0.));
#70331=DIRECTION('',(-0.994165131331399,-0.107868863184986,0.));
#70332=DIRECTION('',(0.,0.,-1.));
#70333=DIRECTION('',(0.994165131331399,0.107868863184986,0.));
#70334=DIRECTION('center_axis',(-0.107868863184987,-0.994165131331399,0.));
#70335=DIRECTION('ref_axis',(-0.994165131331399,0.107868863184987,0.));
#70336=DIRECTION('',(-0.994165131331399,0.107868863184987,0.));
#70337=DIRECTION('',(0.,0.,-1.));
#70338=DIRECTION('',(0.994165131331399,-0.107868863184987,0.));
#70339=DIRECTION('',(0.,0.,-1.));
#70340=DIRECTION('center_axis',(0.,0.,-1.));
#70341=DIRECTION('ref_axis',(0.999488575288585,-0.0319779278189695,0.));
#70342=DIRECTION('center_axis',(0.,0.,1.));
#70343=DIRECTION('ref_axis',(0.999488575288585,-0.0319779278189695,0.));
#70344=DIRECTION('center_axis',(0.,0.,-1.));
#70345=DIRECTION('ref_axis',(0.999488575288585,-0.0319779278189695,0.));
#70346=DIRECTION('',(0.,0.,-1.));
#70347=DIRECTION('center_axis',(0.,0.,1.));
#70348=DIRECTION('ref_axis',(6.12323399573677E-17,1.,0.));
#70349=DIRECTION('center_axis',(0.280792689903721,0.959768443582426,0.));
#70350=DIRECTION('ref_axis',(0.959768443582426,-0.280792689903721,0.));
#70351=DIRECTION('',(-0.959768443582426,0.280792689903721,0.));
#70352=DIRECTION('',(0.,0.,-1.));
#70353=DIRECTION('',(0.959768443582426,-0.280792689903721,0.));
#70354=DIRECTION('center_axis',(-0.48010835968746,-0.877209189964524,0.));
#70355=DIRECTION('ref_axis',(-0.877209189964524,0.480108359687459,0.));
#70356=DIRECTION('',(-0.877209189964524,0.480108359687459,0.));
#70357=DIRECTION('',(0.,0.,-1.));
#70358=DIRECTION('',(0.877209189964524,-0.480108359687459,0.));
#70359=DIRECTION('',(0.,0.,-1.));
#70360=DIRECTION('center_axis',(0.,0.,-1.));
#70361=DIRECTION('ref_axis',(0.911169614510303,-0.412031471605198,0.));
#70362=DIRECTION('center_axis',(0.,0.,1.));
#70363=DIRECTION('ref_axis',(0.911169614510303,-0.412031471605198,0.));
#70364=DIRECTION('center_axis',(0.,0.,-1.));
#70365=DIRECTION('ref_axis',(0.911169614510303,-0.412031471605198,0.));
#70366=DIRECTION('',(0.,0.,-1.));
#70367=DIRECTION('center_axis',(0.,0.,1.));
#70368=DIRECTION('ref_axis',(0.38268343236509,0.923879532511287,0.));
#70369=DIRECTION('center_axis',(0.626706101346659,0.779255710620635,0.));
#70370=DIRECTION('ref_axis',(0.779255710620635,-0.626706101346659,0.));
#70371=DIRECTION('',(-0.779255710620635,0.626706101346659,0.));
#70372=DIRECTION('',(0.,0.,-1.));
#70373=DIRECTION('',(0.779255710620635,-0.626706101346659,0.));
#70374=DIRECTION('center_axis',(-0.779255710620635,-0.626706101346659,0.));
#70375=DIRECTION('ref_axis',(-0.626706101346659,0.779255710620635,0.));
#70376=DIRECTION('',(-0.626706101346659,0.779255710620635,0.));
#70377=DIRECTION('',(0.,0.,-1.));
#70378=DIRECTION('',(0.626706101346659,-0.779255710620635,0.));
#70379=DIRECTION('',(0.,0.,-1.));
#70380=DIRECTION('center_axis',(0.,0.,-1.));
#70381=DIRECTION('ref_axis',(0.684133339695952,-0.729356958914127,0.));
#70382=DIRECTION('center_axis',(0.,0.,1.));
#70383=DIRECTION('ref_axis',(0.684133339695952,-0.729356958914127,0.));
#70384=DIRECTION('center_axis',(0.,0.,-1.));
#70385=DIRECTION('ref_axis',(0.684133339695952,-0.729356958914127,0.));
#70386=DIRECTION('',(0.,0.,-1.));
#70387=DIRECTION('center_axis',(0.,0.,1.));
#70388=DIRECTION('ref_axis',(0.707106781186548,0.707106781186548,0.));
#70389=DIRECTION('center_axis',(0.877209189964524,0.480108359687459,0.));
#70390=DIRECTION('ref_axis',(0.480108359687459,-0.877209189964524,0.));
#70391=DIRECTION('',(-0.480108359687459,0.877209189964524,0.));
#70392=DIRECTION('',(0.,0.,-1.));
#70393=DIRECTION('',(0.480108359687459,-0.877209189964524,0.));
#70394=DIRECTION('center_axis',(-0.959768443582426,-0.280792689903721,0.));
#70395=DIRECTION('ref_axis',(-0.280792689903721,0.959768443582426,0.));
#70396=DIRECTION('',(-0.280792689903721,0.959768443582426,0.));
#70397=DIRECTION('',(0.,0.,-1.));
#70398=DIRECTION('',(0.280792689903721,-0.959768443582426,0.));
#70399=DIRECTION('',(0.,0.,-1.));
#70400=DIRECTION('center_axis',(0.,0.,-1.));
#70401=DIRECTION('ref_axis',(0.35294396559706,-0.935644460865676,0.));
#70402=DIRECTION('center_axis',(0.,0.,1.));
#70403=DIRECTION('ref_axis',(0.35294396559706,-0.935644460865676,0.));
#70404=DIRECTION('center_axis',(0.,0.,-1.));
#70405=DIRECTION('ref_axis',(0.35294396559706,-0.935644460865676,0.));
#70406=DIRECTION('',(0.,0.,-1.));
#70407=DIRECTION('center_axis',(0.,0.,1.));
#70408=DIRECTION('ref_axis',(0.923879532511287,0.38268343236509,0.));
#70409=DIRECTION('center_axis',(-0.994165131331399,0.107868863184986,0.));
#70410=DIRECTION('ref_axis',(0.107868863184986,0.994165131331399,0.));
#70411=DIRECTION('',(0.107868863184986,0.994165131331399,0.));
#70412=DIRECTION('',(0.,0.,-1.));
#70413=DIRECTION('',(-0.107868863184986,-0.994165131331399,0.));
#70414=DIRECTION('',(0.,0.,-1.));
#70415=DIRECTION('center_axis',(0.,0.,-1.));
#70416=DIRECTION('ref_axis',(-0.0319779278189694,-0.999488575288585,0.));
#70417=DIRECTION('center_axis',(0.,0.,1.));
#70418=DIRECTION('ref_axis',(-0.0319779278189694,-0.999488575288585,0.));
#70419=DIRECTION('center_axis',(0.,0.,-1.));
#70420=DIRECTION('ref_axis',(-0.0319779278189694,-0.999488575288585,0.));
#70421=DIRECTION('',(0.,0.,-1.));
#70422=DIRECTION('',(0.,0.,-1.));
#70423=DIRECTION('center_axis',(0.994165131331399,0.107868863184986,0.));
#70424=DIRECTION('ref_axis',(0.107868863184986,-0.994165131331399,0.));
#70425=DIRECTION('',(-0.107868863184986,0.994165131331399,0.));
#70426=DIRECTION('',(0.107868863184986,-0.994165131331399,0.));
#70427=DIRECTION('center_axis',(0.,0.,1.));
#70428=DIRECTION('ref_axis',(1.,0.,0.));
#70429=DIRECTION('center_axis',(0.,0.,1.));
#70430=DIRECTION('ref_axis',(1.,0.,0.));
#70431=DIRECTION('center_axis',(0.,0.,1.));
#70432=DIRECTION('ref_axis',(1.,0.,0.));
#70433=DIRECTION('',(0.,0.,-1.));
#70434=DIRECTION('center_axis',(0.,0.,1.));
#70435=DIRECTION('ref_axis',(1.,0.,0.));
#70436=DIRECTION('center_axis',(0.,0.,-1.));
#70437=DIRECTION('ref_axis',(-1.,0.,0.));
#70438=DIRECTION('center_axis',(0.,0.,-1.));
#70439=DIRECTION('ref_axis',(-1.,0.,0.));
#70440=DIRECTION('center_axis',(0.,0.,1.));
#70441=DIRECTION('ref_axis',(1.,0.,0.));
#70442=DIRECTION('center_axis',(0.,0.,1.));
#70443=DIRECTION('ref_axis',(1.,0.,0.));
#70444=DIRECTION('center_axis',(0.,0.,1.));
#70445=DIRECTION('ref_axis',(1.,0.,0.));
#70446=DIRECTION('',(0.,0.,-1.));
#70447=DIRECTION('center_axis',(0.,0.,-1.));
#70448=DIRECTION('ref_axis',(1.,0.,0.));
#70449=DIRECTION('center_axis',(0.,0.,1.));
#70450=DIRECTION('ref_axis',(1.,0.,0.));
#70451=DIRECTION('',(-0.707106781186547,-8.65956056235493E-17,-0.707106781186547));
#70452=DIRECTION('center_axis',(0.,0.,1.));
#70453=DIRECTION('ref_axis',(1.,0.,0.));
#70454=DIRECTION('axis',(0.,0.,1.));
#70455=DIRECTION('refdir',(1.,0.,0.));
#70456=DIRECTION('center_axis',(0.,1.,0.));
#70457=DIRECTION('ref_axis',(1.,0.,0.));
#70458=DIRECTION('',(0.,0.,1.));
#70459=DIRECTION('center_axis',(0.,-1.,0.));
#70460=DIRECTION('ref_axis',(1.,0.,0.));
#70461=DIRECTION('center_axis',(0.,-1.,0.));
#70462=DIRECTION('ref_axis',(1.,0.,0.));
#70463=DIRECTION('center_axis',(0.,-1.,0.));
#70464=DIRECTION('ref_axis',(1.,0.,0.));
#70465=DIRECTION('',(0.,-1.,0.));
#70466=DIRECTION('center_axis',(0.,-1.,0.));
#70467=DIRECTION('ref_axis',(1.,0.,0.));
#70468=DIRECTION('center_axis',(0.,1.,0.));
#70469=DIRECTION('ref_axis',(1.,0.,0.));
#70470=DIRECTION('',(0.,0.,-1.));
#70471=DIRECTION('center_axis',(-0.402510663229762,0.915415297002588,0.));
#70472=DIRECTION('ref_axis',(0.915415297002588,0.402510663229762,0.));
#70473=DIRECTION('',(0.,0.,-1.));
#70474=DIRECTION('',(0.,0.,-1.));
#70475=DIRECTION('center_axis',(-0.66568927282754,-0.746229047975447,0.));
#70476=DIRECTION('ref_axis',(-0.746229047975447,0.66568927282754,0.));
#70477=DIRECTION('',(0.,0.,1.));
#70478=DIRECTION('center_axis',(0.,0.,1.));
#70479=DIRECTION('ref_axis',(1.,0.,0.));
#70480=DIRECTION('center_axis',(0.,0.,1.));
#70481=DIRECTION('ref_axis',(1.,0.,0.));
#70482=DIRECTION('center_axis',(0.,0.,1.));
#70483=DIRECTION('ref_axis',(1.,0.,0.));
#70484=DIRECTION('center_axis',(0.,0.,1.));
#70485=DIRECTION('ref_axis',(1.,0.,0.));
#70486=DIRECTION('center_axis',(0.,0.,1.));
#70487=DIRECTION('ref_axis',(1.,0.,0.));
#70488=DIRECTION('center_axis',(0.,0.,1.));
#70489=DIRECTION('ref_axis',(1.,0.,0.));
#70490=DIRECTION('center_axis',(0.,0.,1.));
#70491=DIRECTION('ref_axis',(1.,0.,0.));
#70492=DIRECTION('center_axis',(0.,0.,1.));
#70493=DIRECTION('ref_axis',(1.,0.,0.));
#70494=DIRECTION('center_axis',(0.,0.,1.));
#70495=DIRECTION('ref_axis',(1.,0.,0.));
#70496=DIRECTION('center_axis',(0.,0.,1.));
#70497=DIRECTION('ref_axis',(1.,0.,0.));
#70498=DIRECTION('center_axis',(0.,0.,1.));
#70499=DIRECTION('ref_axis',(1.,0.,0.));
#70500=DIRECTION('center_axis',(0.,0.,1.));
#70501=DIRECTION('ref_axis',(1.,0.,0.));
#70502=DIRECTION('center_axis',(0.,0.,1.));
#70503=DIRECTION('ref_axis',(1.,0.,0.));
#70504=DIRECTION('center_axis',(0.,0.,1.));
#70505=DIRECTION('ref_axis',(1.,0.,0.));
#70506=DIRECTION('center_axis',(0.,0.,1.));
#70507=DIRECTION('ref_axis',(1.,0.,0.));
#70508=DIRECTION('center_axis',(0.,0.,1.));
#70509=DIRECTION('ref_axis',(1.,0.,0.));
#70510=DIRECTION('center_axis',(0.,0.,1.));
#70511=DIRECTION('ref_axis',(1.,0.,0.));
#70512=DIRECTION('center_axis',(0.,0.,1.));
#70513=DIRECTION('ref_axis',(1.,0.,0.));
#70514=DIRECTION('center_axis',(0.,0.,1.));
#70515=DIRECTION('ref_axis',(1.,0.,0.));
#70516=DIRECTION('center_axis',(0.,0.,1.));
#70517=DIRECTION('ref_axis',(1.,0.,0.));
#70518=DIRECTION('',(0.707106781186547,8.65956056235493E-17,-0.707106781186547));
#70519=DIRECTION('center_axis',(0.,0.,1.));
#70520=DIRECTION('ref_axis',(1.,0.,0.));
#70521=DIRECTION('center_axis',(0.,0.,1.));
#70522=DIRECTION('ref_axis',(1.,0.,0.));
#70523=DIRECTION('center_axis',(0.,0.,1.));
#70524=DIRECTION('ref_axis',(1.,0.,0.));
#70525=DIRECTION('center_axis',(0.,0.,1.));
#70526=DIRECTION('ref_axis',(1.,0.,0.));
#70527=DIRECTION('center_axis',(0.,0.,1.));
#70528=DIRECTION('ref_axis',(1.,0.,0.));
#70529=DIRECTION('center_axis',(0.,0.,1.));
#70530=DIRECTION('ref_axis',(1.,0.,0.));
#70531=DIRECTION('center_axis',(0.,0.,1.));
#70532=DIRECTION('ref_axis',(1.,0.,0.));
#70533=DIRECTION('center_axis',(0.,0.,1.));
#70534=DIRECTION('ref_axis',(1.,0.,0.));
#70535=DIRECTION('center_axis',(0.,0.,1.));
#70536=DIRECTION('ref_axis',(1.,0.,0.));
#70537=DIRECTION('center_axis',(0.,0.,1.));
#70538=DIRECTION('ref_axis',(1.,0.,0.));
#70539=DIRECTION('center_axis',(0.,0.,1.));
#70540=DIRECTION('ref_axis',(1.,0.,0.));
#70541=DIRECTION('center_axis',(0.,0.,1.));
#70542=DIRECTION('ref_axis',(1.,0.,0.));
#70543=DIRECTION('center_axis',(0.,0.,1.));
#70544=DIRECTION('ref_axis',(1.,0.,0.));
#70545=DIRECTION('center_axis',(0.,0.,1.));
#70546=DIRECTION('ref_axis',(1.,0.,0.));
#70547=DIRECTION('center_axis',(0.,0.,1.));
#70548=DIRECTION('ref_axis',(1.,0.,0.));
#70549=DIRECTION('center_axis',(0.,0.,1.));
#70550=DIRECTION('ref_axis',(1.,0.,0.));
#70551=DIRECTION('center_axis',(0.,0.,1.));
#70552=DIRECTION('ref_axis',(1.,0.,0.));
#70553=DIRECTION('center_axis',(0.,0.,1.));
#70554=DIRECTION('ref_axis',(1.,0.,0.));
#70555=DIRECTION('center_axis',(0.,0.,1.));
#70556=DIRECTION('ref_axis',(1.,0.,0.));
#70557=DIRECTION('center_axis',(0.,0.,1.));
#70558=DIRECTION('ref_axis',(1.,0.,0.));
#70559=DIRECTION('center_axis',(0.,0.,1.));
#70560=DIRECTION('ref_axis',(1.,0.,0.));
#70561=DIRECTION('center_axis',(0.,0.,1.));
#70562=DIRECTION('ref_axis',(1.,0.,0.));
#70563=DIRECTION('center_axis',(0.,0.,1.));
#70564=DIRECTION('ref_axis',(1.,0.,0.));
#70565=DIRECTION('center_axis',(0.,0.,1.));
#70566=DIRECTION('ref_axis',(1.,0.,0.));
#70567=DIRECTION('',(0.,0.,-1.));
#70568=DIRECTION('center_axis',(0.,0.,1.));
#70569=DIRECTION('ref_axis',(1.,0.,0.));
#70570=DIRECTION('',(0.,0.,1.));
#70571=DIRECTION('center_axis',(0.,0.,1.));
#70572=DIRECTION('ref_axis',(1.,0.,0.));
#70573=DIRECTION('center_axis',(-0.774229475148536,-0.632904984820962,0.));
#70574=DIRECTION('ref_axis',(-0.632904984820962,0.774229475148536,0.));
#70575=DIRECTION('',(0.,0.,-1.));
#70576=DIRECTION('',(0.,0.,1.));
#70577=DIRECTION('center_axis',(-0.254352586761008,0.967111555927228,0.));
#70578=DIRECTION('ref_axis',(0.967111555927228,0.254352586761008,0.));
#70579=DIRECTION('center_axis',(0.,0.,1.));
#70580=DIRECTION('ref_axis',(1.,0.,0.));
#70581=DIRECTION('center_axis',(0.,0.,1.));
#70582=DIRECTION('ref_axis',(1.,0.,0.));
#70583=DIRECTION('',(0.,0.,-1.));
#70584=DIRECTION('center_axis',(0.,0.,-1.));
#70585=DIRECTION('ref_axis',(1.,0.,0.));
#70586=DIRECTION('center_axis',(0.,0.,1.));
#70587=DIRECTION('ref_axis',(1.,0.,0.));
#70588=DIRECTION('',(-0.707106781186547,-8.65956056235493E-17,-0.707106781186547));
#70589=DIRECTION('center_axis',(0.,0.,1.));
#70590=DIRECTION('ref_axis',(1.,0.,0.));
#70591=DIRECTION('center_axis',(0.,0.,1.));
#70592=DIRECTION('ref_axis',(1.,0.,0.));
#70593=DIRECTION('center_axis',(0.,0.,1.));
#70594=DIRECTION('ref_axis',(1.,0.,0.));
#70595=DIRECTION('center_axis',(0.,0.,1.));
#70596=DIRECTION('ref_axis',(1.,0.,0.));
#70597=DIRECTION('center_axis',(0.,0.,1.));
#70598=DIRECTION('ref_axis',(1.,0.,0.));
#70599=DIRECTION('center_axis',(0.,0.,1.));
#70600=DIRECTION('ref_axis',(1.,0.,0.));
#70601=DIRECTION('center_axis',(0.,0.,1.));
#70602=DIRECTION('ref_axis',(1.,0.,0.));
#70603=DIRECTION('center_axis',(0.,0.,1.));
#70604=DIRECTION('ref_axis',(1.,0.,0.));
#70605=DIRECTION('center_axis',(0.,0.,1.));
#70606=DIRECTION('ref_axis',(1.,0.,0.));
#70607=DIRECTION('center_axis',(0.,0.,1.));
#70608=DIRECTION('ref_axis',(1.,0.,0.));
#70609=DIRECTION('center_axis',(0.,0.,1.));
#70610=DIRECTION('ref_axis',(1.,0.,0.));
#70611=DIRECTION('center_axis',(0.,0.,1.));
#70612=DIRECTION('ref_axis',(1.,0.,0.));
#70613=DIRECTION('center_axis',(0.,0.,1.));
#70614=DIRECTION('ref_axis',(1.,0.,0.));
#70615=DIRECTION('center_axis',(0.,0.,1.));
#70616=DIRECTION('ref_axis',(1.,0.,0.));
#70617=DIRECTION('center_axis',(0.,0.,1.));
#70618=DIRECTION('ref_axis',(1.,0.,0.));
#70619=DIRECTION('center_axis',(0.,0.,1.));
#70620=DIRECTION('ref_axis',(1.,0.,0.));
#70621=DIRECTION('center_axis',(0.,0.,1.));
#70622=DIRECTION('ref_axis',(1.,0.,0.));
#70623=DIRECTION('center_axis',(0.,0.,1.));
#70624=DIRECTION('ref_axis',(1.,0.,0.));
#70625=DIRECTION('center_axis',(0.,0.,1.));
#70626=DIRECTION('ref_axis',(1.,0.,0.));
#70627=DIRECTION('center_axis',(0.,0.,1.));
#70628=DIRECTION('ref_axis',(1.,0.,0.));
#70629=DIRECTION('center_axis',(0.,0.,1.));
#70630=DIRECTION('ref_axis',(1.,0.,0.));
#70631=DIRECTION('center_axis',(0.,0.,1.));
#70632=DIRECTION('ref_axis',(1.,0.,0.));
#70633=DIRECTION('center_axis',(0.,0.,1.));
#70634=DIRECTION('ref_axis',(1.,0.,0.));
#70635=DIRECTION('center_axis',(0.,0.,1.));
#70636=DIRECTION('ref_axis',(1.,0.,0.));
#70637=DIRECTION('center_axis',(0.,0.,1.));
#70638=DIRECTION('ref_axis',(1.,0.,0.));
#70639=DIRECTION('center_axis',(0.,0.,1.));
#70640=DIRECTION('ref_axis',(1.,0.,0.));
#70641=DIRECTION('center_axis',(0.,0.,1.));
#70642=DIRECTION('ref_axis',(1.,0.,0.));
#70643=DIRECTION('center_axis',(0.,0.,1.));
#70644=DIRECTION('ref_axis',(1.,0.,0.));
#70645=DIRECTION('center_axis',(0.,0.,1.));
#70646=DIRECTION('ref_axis',(1.,0.,0.));
#70647=DIRECTION('center_axis',(0.,0.,1.));
#70648=DIRECTION('ref_axis',(1.,0.,0.));
#70649=DIRECTION('center_axis',(0.,0.,1.));
#70650=DIRECTION('ref_axis',(1.,0.,0.));
#70651=DIRECTION('center_axis',(0.,0.,1.));
#70652=DIRECTION('ref_axis',(1.,0.,0.));
#70653=DIRECTION('center_axis',(0.,0.,1.));
#70654=DIRECTION('ref_axis',(1.,0.,0.));
#70655=DIRECTION('center_axis',(0.,0.,1.));
#70656=DIRECTION('ref_axis',(1.,0.,0.));
#70657=DIRECTION('center_axis',(0.,0.,1.));
#70658=DIRECTION('ref_axis',(1.,0.,0.));
#70659=DIRECTION('center_axis',(0.,0.,1.));
#70660=DIRECTION('ref_axis',(1.,0.,0.));
#70661=DIRECTION('center_axis',(0.,0.,1.));
#70662=DIRECTION('ref_axis',(1.,0.,0.));
#70663=DIRECTION('center_axis',(-0.09993150545836,0.994994318685703,0.));
#70664=DIRECTION('ref_axis',(0.994994318685703,0.09993150545836,0.));
#70665=DIRECTION('',(0.,0.,-1.));
#70666=DIRECTION('center_axis',(-0.863705578271065,-0.503996700448967,0.));
#70667=DIRECTION('ref_axis',(-0.503996700448967,0.863705578271065,0.));
#70668=DIRECTION('',(0.,0.,1.));
#70669=DIRECTION('center_axis',(0.0569502211623254,0.998377019121315,0.));
#70670=DIRECTION('ref_axis',(0.998377019121315,-0.0569502211623254,0.));
#70671=DIRECTION('',(0.,0.,-1.));
#70672=DIRECTION('',(0.,0.,-1.));
#70673=DIRECTION('center_axis',(-0.931914383582088,-0.362678344642767,0.));
#70674=DIRECTION('ref_axis',(-0.362678344642767,0.931914383582087,0.));
#70675=DIRECTION('',(0.,0.,1.));
#70676=DIRECTION('center_axis',(0.,0.,1.));
#70677=DIRECTION('ref_axis',(1.,0.,0.));
#70678=DIRECTION('',(0.,0.,-1.));
#70679=DIRECTION('center_axis',(0.,0.,1.));
#70680=DIRECTION('ref_axis',(1.,0.,0.));
#70681=DIRECTION('center_axis',(-0.9771763639228,-0.212429644331046,0.));
#70682=DIRECTION('ref_axis',(-0.212429644331046,0.9771763639228,0.));
#70683=DIRECTION('',(0.,0.,-1.));
#70684=DIRECTION('',(0.,0.,1.));
#70685=DIRECTION('center_axis',(0.212429644331046,0.9771763639228,0.));
#70686=DIRECTION('ref_axis',(0.9771763639228,-0.212429644331046,0.));
#70687=DIRECTION('center_axis',(0.,0.,1.));
#70688=DIRECTION('ref_axis',(1.,0.,0.));
#70689=DIRECTION('',(0.,0.,-1.));
#70690=DIRECTION('center_axis',(0.362678344642768,0.931914383582087,0.));
#70691=DIRECTION('ref_axis',(0.931914383582087,-0.362678344642768,0.));
#70692=DIRECTION('',(0.,0.,-1.));
#70693=DIRECTION('center_axis',(-0.998377019121315,-0.0569502211623249,
0.));
#70694=DIRECTION('ref_axis',(-0.0569502211623248,0.998377019121315,0.));
#70695=DIRECTION('',(0.,0.,1.));
#70696=DIRECTION('center_axis',(0.503996700448967,0.863705578271065,0.));
#70697=DIRECTION('ref_axis',(0.863705578271065,-0.503996700448967,0.));
#70698=DIRECTION('',(0.,0.,-1.));
#70699=DIRECTION('',(0.,0.,-1.));
#70700=DIRECTION('center_axis',(-0.994994318685703,0.0999315054583604,0.));
#70701=DIRECTION('ref_axis',(0.0999315054583604,0.994994318685703,0.));
#70702=DIRECTION('',(0.,0.,1.));
#70703=DIRECTION('center_axis',(0.,0.,1.));
#70704=DIRECTION('ref_axis',(1.,0.,0.));
#70705=DIRECTION('',(0.,0.,-1.));
#70706=DIRECTION('center_axis',(0.,0.,1.));
#70707=DIRECTION('ref_axis',(1.,0.,0.));
#70708=DIRECTION('center_axis',(-0.967111555927228,0.254352586761009,0.));
#70709=DIRECTION('ref_axis',(0.254352586761009,0.967111555927228,0.));
#70710=DIRECTION('',(0.,0.,-1.));
#70711=DIRECTION('',(0.,0.,1.));
#70712=DIRECTION('center_axis',(0.632904984820962,0.774229475148536,0.));
#70713=DIRECTION('ref_axis',(0.774229475148536,-0.632904984820962,0.));
#70714=DIRECTION('center_axis',(0.,0.,1.));
#70715=DIRECTION('ref_axis',(1.,0.,0.));
#70716=DIRECTION('',(0.,0.,-1.));
#70717=DIRECTION('center_axis',(0.746229047975447,0.665689272827539,0.));
#70718=DIRECTION('ref_axis',(0.665689272827539,-0.746229047975447,0.));
#70719=DIRECTION('',(0.,0.,-1.));
#70720=DIRECTION('center_axis',(-0.915415297002588,0.402510663229763,0.));
#70721=DIRECTION('ref_axis',(0.402510663229763,0.915415297002588,0.));
#70722=DIRECTION('',(0.,0.,1.));
#70723=DIRECTION('center_axis',(0.841178475376555,0.540757591313496,0.));
#70724=DIRECTION('ref_axis',(0.540757591313496,-0.841178475376555,0.));
#70725=DIRECTION('',(0.,0.,-1.));
#70726=DIRECTION('',(0.,0.,-1.));
#70727=DIRECTION('center_axis',(-0.841178475376555,0.540757591313497,0.));
#70728=DIRECTION('ref_axis',(0.540757591313497,0.841178475376555,0.));
#70729=DIRECTION('',(0.,0.,1.));
#70730=DIRECTION('center_axis',(0.,0.,1.));
#70731=DIRECTION('ref_axis',(1.,0.,0.));
#70732=DIRECTION('',(0.,0.,-1.));
#70733=DIRECTION('center_axis',(0.,0.,1.));
#70734=DIRECTION('ref_axis',(1.,0.,0.));
#70735=DIRECTION('center_axis',(-0.746229047975447,0.66568927282754,0.));
#70736=DIRECTION('ref_axis',(0.66568927282754,0.746229047975447,0.));
#70737=DIRECTION('',(0.,0.,-1.));
#70738=DIRECTION('',(0.,0.,1.));
#70739=DIRECTION('center_axis',(0.915415297002588,0.402510663229763,0.));
#70740=DIRECTION('ref_axis',(0.402510663229763,-0.915415297002588,0.));
#70741=DIRECTION('center_axis',(0.,0.,1.));
#70742=DIRECTION('ref_axis',(1.,0.,0.));
#70743=DIRECTION('',(0.,0.,-1.));
#70744=DIRECTION('center_axis',(0.967111555927228,0.254352586761009,0.));
#70745=DIRECTION('ref_axis',(0.254352586761008,-0.967111555927228,0.));
#70746=DIRECTION('',(0.,0.,-1.));
#70747=DIRECTION('center_axis',(-0.632904984820962,0.774229475148536,0.));
#70748=DIRECTION('ref_axis',(0.774229475148536,0.632904984820962,0.));
#70749=DIRECTION('',(0.,0.,1.));
#70750=DIRECTION('center_axis',(0.994994318685703,0.0999315054583601,0.));
#70751=DIRECTION('ref_axis',(0.0999315054583601,-0.994994318685703,0.));
#70752=DIRECTION('',(0.,0.,-1.));
#70753=DIRECTION('',(0.,0.,-1.));
#70754=DIRECTION('center_axis',(-0.503996700448967,0.863705578271065,0.));
#70755=DIRECTION('ref_axis',(0.863705578271065,0.503996700448967,0.));
#70756=DIRECTION('',(0.,0.,1.));
#70757=DIRECTION('center_axis',(0.,0.,1.));
#70758=DIRECTION('ref_axis',(1.,0.,0.));
#70759=DIRECTION('',(0.,0.,-1.));
#70760=DIRECTION('center_axis',(0.,0.,1.));
#70761=DIRECTION('ref_axis',(1.,0.,0.));
#70762=DIRECTION('center_axis',(-0.362678344642767,0.931914383582087,0.));
#70763=DIRECTION('ref_axis',(0.931914383582087,0.362678344642767,0.));
#70764=DIRECTION('',(0.,0.,-1.));
#70765=DIRECTION('',(0.,0.,1.));
#70766=DIRECTION('center_axis',(0.998377019121315,-0.0569502211623253,0.));
#70767=DIRECTION('ref_axis',(-0.0569502211623253,-0.998377019121315,0.));
#70768=DIRECTION('center_axis',(0.,0.,1.));
#70769=DIRECTION('ref_axis',(1.,0.,0.));
#70770=DIRECTION('',(0.,0.,-1.));
#70771=DIRECTION('center_axis',(0.9771763639228,-0.212429644331046,0.));
#70772=DIRECTION('ref_axis',(-0.212429644331046,-0.9771763639228,0.));
#70773=DIRECTION('',(0.,0.,-1.));
#70774=DIRECTION('center_axis',(-0.212429644331046,0.9771763639228,0.));
#70775=DIRECTION('ref_axis',(0.9771763639228,0.212429644331046,0.));
#70776=DIRECTION('',(0.,0.,1.));
#70777=DIRECTION('center_axis',(0.931914383582087,-0.362678344642768,0.));
#70778=DIRECTION('ref_axis',(-0.362678344642768,-0.931914383582087,0.));
#70779=DIRECTION('',(0.,0.,-1.));
#70780=DIRECTION('',(0.,0.,-1.));
#70781=DIRECTION('center_axis',(-0.056950221162325,0.998377019121315,0.));
#70782=DIRECTION('ref_axis',(0.998377019121315,0.056950221162325,0.));
#70783=DIRECTION('',(0.,0.,1.));
#70784=DIRECTION('center_axis',(0.,0.,1.));
#70785=DIRECTION('ref_axis',(1.,0.,0.));
#70786=DIRECTION('',(0.,0.,-1.));
#70787=DIRECTION('center_axis',(0.,0.,1.));
#70788=DIRECTION('ref_axis',(1.,0.,0.));
#70789=DIRECTION('center_axis',(0.0999315054583604,0.994994318685703,0.));
#70790=DIRECTION('ref_axis',(0.994994318685703,-0.0999315054583604,0.));
#70791=DIRECTION('',(0.,0.,-1.));
#70792=DIRECTION('',(0.,0.,1.));
#70793=DIRECTION('center_axis',(0.863705578271065,-0.503996700448967,0.));
#70794=DIRECTION('ref_axis',(-0.503996700448967,-0.863705578271065,0.));
#70795=DIRECTION('center_axis',(0.,0.,1.));
#70796=DIRECTION('ref_axis',(1.,0.,0.));
#70797=DIRECTION('',(0.,0.,-1.));
#70798=DIRECTION('center_axis',(0.774229475148536,-0.632904984820962,0.));
#70799=DIRECTION('ref_axis',(-0.632904984820962,-0.774229475148536,0.));
#70800=DIRECTION('',(0.,0.,-1.));
#70801=DIRECTION('center_axis',(0.254352586761009,0.967111555927228,0.));
#70802=DIRECTION('ref_axis',(0.967111555927228,-0.254352586761009,0.));
#70803=DIRECTION('',(0.,0.,1.));
#70804=DIRECTION('center_axis',(0.665689272827539,-0.746229047975447,0.));
#70805=DIRECTION('ref_axis',(-0.746229047975447,-0.665689272827539,0.));
#70806=DIRECTION('',(0.,0.,-1.));
#70807=DIRECTION('',(0.,0.,-1.));
#70808=DIRECTION('center_axis',(0.402510663229763,0.915415297002588,0.));
#70809=DIRECTION('ref_axis',(0.915415297002588,-0.402510663229763,0.));
#70810=DIRECTION('',(0.,0.,1.));
#70811=DIRECTION('center_axis',(0.,0.,1.));
#70812=DIRECTION('ref_axis',(1.,0.,0.));
#70813=DIRECTION('',(0.,0.,-1.));
#70814=DIRECTION('center_axis',(0.,0.,1.));
#70815=DIRECTION('ref_axis',(1.,0.,0.));
#70816=DIRECTION('center_axis',(0.540757591313497,0.841178475376555,0.));
#70817=DIRECTION('ref_axis',(0.841178475376555,-0.540757591313497,0.));
#70818=DIRECTION('',(0.,0.,-1.));
#70819=DIRECTION('',(0.,0.,1.));
#70820=DIRECTION('center_axis',(0.540757591313496,-0.841178475376555,0.));
#70821=DIRECTION('ref_axis',(-0.841178475376555,-0.540757591313496,0.));
#70822=DIRECTION('center_axis',(0.,0.,1.));
#70823=DIRECTION('ref_axis',(1.,0.,0.));
#70824=DIRECTION('',(0.,0.,-1.));
#70825=DIRECTION('center_axis',(0.402510663229763,-0.915415297002588,0.));
#70826=DIRECTION('ref_axis',(-0.915415297002588,-0.402510663229763,0.));
#70827=DIRECTION('',(0.,0.,-1.));
#70828=DIRECTION('center_axis',(0.66568927282754,0.746229047975447,0.));
#70829=DIRECTION('ref_axis',(0.746229047975447,-0.66568927282754,0.));
#70830=DIRECTION('',(0.,0.,1.));
#70831=DIRECTION('center_axis',(0.254352586761009,-0.967111555927228,0.));
#70832=DIRECTION('ref_axis',(-0.967111555927228,-0.254352586761009,0.));
#70833=DIRECTION('',(0.,0.,-1.));
#70834=DIRECTION('',(0.,0.,-1.));
#70835=DIRECTION('center_axis',(0.774229475148536,0.632904984820962,0.));
#70836=DIRECTION('ref_axis',(0.632904984820962,-0.774229475148536,0.));
#70837=DIRECTION('',(0.,0.,1.));
#70838=DIRECTION('center_axis',(0.,0.,1.));
#70839=DIRECTION('ref_axis',(1.,0.,0.));
#70840=DIRECTION('',(0.,0.,-1.));
#70841=DIRECTION('center_axis',(0.,0.,1.));
#70842=DIRECTION('ref_axis',(1.,0.,0.));
#70843=DIRECTION('center_axis',(0.863705578271065,0.503996700448967,0.));
#70844=DIRECTION('ref_axis',(0.503996700448967,-0.863705578271065,0.));
#70845=DIRECTION('',(0.,0.,-1.));
#70846=DIRECTION('',(0.,0.,1.));
#70847=DIRECTION('center_axis',(0.0999315054583602,-0.994994318685703,0.));
#70848=DIRECTION('ref_axis',(-0.994994318685703,-0.0999315054583602,0.));
#70849=DIRECTION('center_axis',(0.,0.,1.));
#70850=DIRECTION('ref_axis',(1.,0.,0.));
#70851=DIRECTION('',(0.,0.,-1.));
#70852=DIRECTION('center_axis',(-0.0569502211623253,-0.998377019121315,
0.));
#70853=DIRECTION('ref_axis',(-0.998377019121315,0.0569502211623253,0.));
#70854=DIRECTION('',(0.,0.,-1.));
#70855=DIRECTION('center_axis',(0.931914383582087,0.362678344642767,0.));
#70856=DIRECTION('ref_axis',(0.362678344642767,-0.931914383582087,0.));
#70857=DIRECTION('',(0.,0.,1.));
#70858=DIRECTION('center_axis',(-0.212429644331046,-0.9771763639228,0.));
#70859=DIRECTION('ref_axis',(-0.9771763639228,0.212429644331046,0.));
#70860=DIRECTION('',(0.,0.,-1.));
#70861=DIRECTION('',(0.,0.,-1.));
#70862=DIRECTION('center_axis',(0.9771763639228,0.212429644331046,0.));
#70863=DIRECTION('ref_axis',(0.212429644331046,-0.9771763639228,0.));
#70864=DIRECTION('',(0.,0.,1.));
#70865=DIRECTION('center_axis',(0.,0.,1.));
#70866=DIRECTION('ref_axis',(1.,0.,0.));
#70867=DIRECTION('',(0.,0.,-1.));
#70868=DIRECTION('center_axis',(0.,0.,1.));
#70869=DIRECTION('ref_axis',(1.,0.,0.));
#70870=DIRECTION('center_axis',(0.998377019121315,0.056950221162325,0.));
#70871=DIRECTION('ref_axis',(0.056950221162325,-0.998377019121315,0.));
#70872=DIRECTION('',(0.,0.,-1.));
#70873=DIRECTION('',(0.,0.,1.));
#70874=DIRECTION('center_axis',(-0.362678344642768,-0.931914383582087,0.));
#70875=DIRECTION('ref_axis',(-0.931914383582087,0.362678344642768,0.));
#70876=DIRECTION('center_axis',(0.,0.,1.));
#70877=DIRECTION('ref_axis',(1.,0.,0.));
#70878=DIRECTION('',(0.,0.,-1.));
#70879=DIRECTION('center_axis',(-0.503996700448967,-0.863705578271065,0.));
#70880=DIRECTION('ref_axis',(-0.863705578271065,0.503996700448967,0.));
#70881=DIRECTION('',(0.,0.,-1.));
#70882=DIRECTION('center_axis',(0.994994318685703,-0.0999315054583603,0.));
#70883=DIRECTION('ref_axis',(-0.0999315054583603,-0.994994318685703,0.));
#70884=DIRECTION('',(0.,0.,1.));
#70885=DIRECTION('center_axis',(-0.632904984820962,-0.774229475148536,0.));
#70886=DIRECTION('ref_axis',(-0.774229475148536,0.632904984820962,0.));
#70887=DIRECTION('',(0.,0.,-1.));
#70888=DIRECTION('',(0.,0.,-1.));
#70889=DIRECTION('center_axis',(0.967111555927228,-0.254352586761009,0.));
#70890=DIRECTION('ref_axis',(-0.254352586761009,-0.967111555927228,0.));
#70891=DIRECTION('',(0.,0.,1.));
#70892=DIRECTION('center_axis',(0.,0.,1.));
#70893=DIRECTION('ref_axis',(1.,0.,0.));
#70894=DIRECTION('',(0.,0.,-1.));
#70895=DIRECTION('center_axis',(0.,0.,1.));
#70896=DIRECTION('ref_axis',(1.,0.,0.));
#70897=DIRECTION('center_axis',(0.915415297002588,-0.402510663229763,0.));
#70898=DIRECTION('ref_axis',(-0.402510663229763,-0.915415297002588,0.));
#70899=DIRECTION('',(0.,0.,-1.));
#70900=DIRECTION('',(0.,0.,1.));
#70901=DIRECTION('center_axis',(-0.746229047975447,-0.665689272827539,0.));
#70902=DIRECTION('ref_axis',(-0.665689272827539,0.746229047975447,0.));
#70903=DIRECTION('center_axis',(0.,0.,1.));
#70904=DIRECTION('ref_axis',(1.,0.,0.));
#70905=DIRECTION('',(0.,0.,-1.));
#70906=DIRECTION('center_axis',(-0.841178475376555,-0.540757591313497,0.));
#70907=DIRECTION('ref_axis',(-0.540757591313497,0.841178475376555,0.));
#70908=DIRECTION('',(0.,0.,-1.));
#70909=DIRECTION('center_axis',(0.841178475376555,-0.540757591313497,0.));
#70910=DIRECTION('ref_axis',(-0.540757591313497,-0.841178475376555,0.));
#70911=DIRECTION('',(0.,0.,1.));
#70912=DIRECTION('center_axis',(-0.915415297002588,-0.402510663229763,0.));
#70913=DIRECTION('ref_axis',(-0.402510663229763,0.915415297002588,0.));
#70914=DIRECTION('',(0.,0.,-1.));
#70915=DIRECTION('',(0.,0.,-1.));
#70916=DIRECTION('center_axis',(0.746229047975447,-0.66568927282754,0.));
#70917=DIRECTION('ref_axis',(-0.66568927282754,-0.746229047975447,0.));
#70918=DIRECTION('',(0.,0.,1.));
#70919=DIRECTION('center_axis',(0.,0.,1.));
#70920=DIRECTION('ref_axis',(1.,0.,0.));
#70921=DIRECTION('',(0.,0.,-1.));
#70922=DIRECTION('center_axis',(0.,0.,1.));
#70923=DIRECTION('ref_axis',(1.,0.,0.));
#70924=DIRECTION('center_axis',(0.632904984820962,-0.774229475148536,0.));
#70925=DIRECTION('ref_axis',(-0.774229475148536,-0.632904984820962,0.));
#70926=DIRECTION('',(0.,0.,-1.));
#70927=DIRECTION('',(0.,0.,1.));
#70928=DIRECTION('center_axis',(-0.967111555927228,-0.254352586761009,0.));
#70929=DIRECTION('ref_axis',(-0.254352586761009,0.967111555927228,0.));
#70930=DIRECTION('center_axis',(0.,0.,1.));
#70931=DIRECTION('ref_axis',(1.,0.,0.));
#70932=DIRECTION('',(0.,0.,-1.));
#70933=DIRECTION('center_axis',(-0.994994318685703,-0.0999315054583602,
0.));
#70934=DIRECTION('ref_axis',(-0.0999315054583602,0.994994318685703,0.));
#70935=DIRECTION('',(0.,0.,-1.));
#70936=DIRECTION('center_axis',(0.503996700448967,-0.863705578271065,0.));
#70937=DIRECTION('ref_axis',(-0.863705578271065,-0.503996700448967,0.));
#70938=DIRECTION('',(0.,0.,1.));
#70939=DIRECTION('center_axis',(-0.998377019121315,0.0569502211623251,0.));
#70940=DIRECTION('ref_axis',(0.0569502211623251,0.998377019121315,0.));
#70941=DIRECTION('',(0.,0.,-1.));
#70942=DIRECTION('',(0.,0.,-1.));
#70943=DIRECTION('center_axis',(0.362678344642768,-0.931914383582087,0.));
#70944=DIRECTION('ref_axis',(-0.931914383582087,-0.362678344642768,0.));
#70945=DIRECTION('',(0.,0.,1.));
#70946=DIRECTION('center_axis',(0.,0.,1.));
#70947=DIRECTION('ref_axis',(1.,0.,0.));
#70948=DIRECTION('',(0.,0.,-1.));
#70949=DIRECTION('center_axis',(0.,0.,1.));
#70950=DIRECTION('ref_axis',(1.,0.,0.));
#70951=DIRECTION('center_axis',(0.212429644331046,-0.9771763639228,0.));
#70952=DIRECTION('ref_axis',(-0.9771763639228,-0.212429644331046,0.));
#70953=DIRECTION('',(0.,0.,-1.));
#70954=DIRECTION('',(0.,0.,1.));
#70955=DIRECTION('center_axis',(-0.9771763639228,0.212429644331046,0.));
#70956=DIRECTION('ref_axis',(0.212429644331046,0.9771763639228,0.));
#70957=DIRECTION('center_axis',(0.,0.,1.));
#70958=DIRECTION('ref_axis',(1.,0.,0.));
#70959=DIRECTION('',(0.,0.,-1.));
#70960=DIRECTION('center_axis',(-0.931914383582087,0.362678344642768,0.));
#70961=DIRECTION('ref_axis',(0.362678344642768,0.931914383582087,0.));
#70962=DIRECTION('',(0.,0.,-1.));
#70963=DIRECTION('center_axis',(0.0569502211623251,-0.998377019121315,0.));
#70964=DIRECTION('ref_axis',(-0.998377019121315,-0.0569502211623251,0.));
#70965=DIRECTION('',(0.,0.,1.));
#70966=DIRECTION('center_axis',(-0.863705578271065,0.503996700448967,0.));
#70967=DIRECTION('ref_axis',(0.503996700448967,0.863705578271065,0.));
#70968=DIRECTION('',(0.,0.,-1.));
#70969=DIRECTION('',(0.,0.,-1.));
#70970=DIRECTION('center_axis',(-0.0999315054583603,-0.994994318685703,
0.));
#70971=DIRECTION('ref_axis',(-0.994994318685703,0.0999315054583603,0.));
#70972=DIRECTION('',(0.,0.,1.));
#70973=DIRECTION('center_axis',(0.,0.,1.));
#70974=DIRECTION('ref_axis',(1.,0.,0.));
#70975=DIRECTION('',(0.,0.,-1.));
#70976=DIRECTION('center_axis',(0.,0.,1.));
#70977=DIRECTION('ref_axis',(1.,0.,0.));
#70978=DIRECTION('center_axis',(-0.254352586761009,-0.967111555927228,0.));
#70979=DIRECTION('ref_axis',(-0.967111555927228,0.254352586761009,0.));
#70980=DIRECTION('',(0.,0.,-1.));
#70981=DIRECTION('',(0.,0.,1.));
#70982=DIRECTION('center_axis',(-0.774229475148536,0.632904984820962,0.));
#70983=DIRECTION('ref_axis',(0.632904984820962,0.774229475148536,0.));
#70984=DIRECTION('center_axis',(0.,0.,1.));
#70985=DIRECTION('ref_axis',(1.,0.,0.));
#70986=DIRECTION('',(0.,0.,-1.));
#70987=DIRECTION('center_axis',(-0.665689272827539,0.746229047975447,0.));
#70988=DIRECTION('ref_axis',(0.746229047975447,0.665689272827539,0.));
#70989=DIRECTION('',(0.,0.,-1.));
#70990=DIRECTION('center_axis',(-0.402510663229763,-0.915415297002588,0.));
#70991=DIRECTION('ref_axis',(-0.915415297002588,0.402510663229763,0.));
#70992=DIRECTION('',(0.,0.,1.));
#70993=DIRECTION('center_axis',(-0.540757591313497,0.841178475376555,0.));
#70994=DIRECTION('ref_axis',(0.841178475376555,0.540757591313497,0.));
#70995=DIRECTION('',(0.,0.,-1.));
#70996=DIRECTION('',(0.,0.,-1.));
#70997=DIRECTION('center_axis',(-0.540757591313497,-0.841178475376555,0.));
#70998=DIRECTION('ref_axis',(-0.841178475376555,0.540757591313497,0.));
#70999=DIRECTION('center_axis',(0.,0.,-1.));
#71000=DIRECTION('ref_axis',(1.,0.,0.));
#71001=DIRECTION('center_axis',(0.,0.,1.));
#71002=DIRECTION('ref_axis',(1.,0.,0.));
#71003=DIRECTION('',(-0.707106781186547,-8.65956056235493E-17,-0.707106781186547));
#71004=DIRECTION('center_axis',(0.,0.,1.));
#71005=DIRECTION('ref_axis',(1.,0.,0.));
#71006=DIRECTION('center_axis',(0.,0.,-1.));
#71007=DIRECTION('ref_axis',(-1.,0.,0.));
#71008=DIRECTION('center_axis',(0.,0.,1.));
#71009=DIRECTION('ref_axis',(1.,0.,0.));
#71010=DIRECTION('center_axis',(0.,0.,1.));
#71011=DIRECTION('ref_axis',(1.,0.,0.));
#71012=DIRECTION('center_axis',(0.,0.,1.));
#71013=DIRECTION('ref_axis',(1.,0.,0.));
#71014=DIRECTION('',(0.707106781186548,8.65956056235493E-17,-0.707106781186548));
#71015=DIRECTION('center_axis',(0.,0.,1.));
#71016=DIRECTION('ref_axis',(1.,0.,0.));
#71017=DIRECTION('center_axis',(0.,0.,1.));
#71018=DIRECTION('ref_axis',(1.,0.,0.));
#71019=DIRECTION('',(0.,0.,-1.));
#71020=DIRECTION('center_axis',(0.,0.,1.));
#71021=DIRECTION('ref_axis',(1.,0.,0.));
#71022=DIRECTION('center_axis',(0.,0.,1.));
#71023=DIRECTION('ref_axis',(1.,0.,0.));
#71024=DIRECTION('',(0.707106781186555,8.65956056235503E-17,-0.70710678118654));
#71025=DIRECTION('center_axis',(0.,0.,-1.));
#71026=DIRECTION('ref_axis',(-1.,0.,0.));
#71027=DIRECTION('center_axis',(0.,0.,1.));
#71028=DIRECTION('ref_axis',(1.,0.,0.));
#71029=DIRECTION('center_axis',(0.,0.,1.));
#71030=DIRECTION('ref_axis',(1.,0.,0.));
#71031=DIRECTION('center_axis',(0.,0.,1.));
#71032=DIRECTION('ref_axis',(1.,0.,0.));
#71033=DIRECTION('',(0.,0.,-1.));
#71034=DIRECTION('center_axis',(0.,0.,1.));
#71035=DIRECTION('ref_axis',(1.,0.,0.));
#71036=DIRECTION('center_axis',(0.,0.,1.));
#71037=DIRECTION('ref_axis',(1.,0.,0.));
#71038=DIRECTION('',(0.707106781186555,8.65956056235503E-17,-0.70710678118654));
#71039=DIRECTION('center_axis',(0.,0.,-1.));
#71040=DIRECTION('ref_axis',(-1.,0.,0.));
#71041=DIRECTION('center_axis',(0.,0.,1.));
#71042=DIRECTION('ref_axis',(1.,0.,0.));
#71043=DIRECTION('center_axis',(0.,0.,1.));
#71044=DIRECTION('ref_axis',(1.,0.,0.));
#71045=DIRECTION('center_axis',(0.,0.,1.));
#71046=DIRECTION('ref_axis',(1.,0.,0.));
#71047=DIRECTION('center_axis',(0.,0.,1.));
#71048=DIRECTION('ref_axis',(1.,0.,0.));
#71049=DIRECTION('',(0.707106781186547,8.65956056235494E-17,-0.707106781186547));
#71050=DIRECTION('center_axis',(0.,0.,1.));
#71051=DIRECTION('ref_axis',(1.,0.,0.));
#71052=DIRECTION('center_axis',(0.,0.,1.));
#71053=DIRECTION('ref_axis',(1.,0.,0.));
#71054=DIRECTION('center_axis',(0.,0.,-1.));
#71055=DIRECTION('ref_axis',(1.,0.,0.));
#71056=DIRECTION('',(-0.8583968680612,-1.05123297686926E-16,-0.512986176132187));
#71057=DIRECTION('center_axis',(0.,0.,1.));
#71058=DIRECTION('ref_axis',(1.,0.,0.));
#71059=DIRECTION('center_axis',(0.,0.,1.));
#71060=DIRECTION('ref_axis',(1.,0.,0.));
#71061=DIRECTION('',(0.,0.,-1.));
#71062=DIRECTION('axis',(0.,0.,1.));
#71063=DIRECTION('refdir',(1.,0.,0.));
#71064=DIRECTION('center_axis',(0.,0.,-1.));
#71065=DIRECTION('ref_axis',(1.,0.,0.));
#71066=DIRECTION('center_axis',(0.,0.,1.));
#71067=DIRECTION('ref_axis',(1.,0.,0.));
#71068=DIRECTION('',(-0.707106781186537,-8.6595605623548E-17,-0.707106781186558));
#71069=DIRECTION('center_axis',(0.,0.,1.));
#71070=DIRECTION('ref_axis',(1.,0.,0.));
#71071=DIRECTION('center_axis',(0.,0.,-1.));
#71072=DIRECTION('ref_axis',(-1.,0.,0.));
#71073=DIRECTION('center_axis',(0.,0.,1.));
#71074=DIRECTION('ref_axis',(1.,0.,0.));
#71075=DIRECTION('center_axis',(0.,0.,1.));
#71076=DIRECTION('ref_axis',(1.,0.,0.));
#71077=DIRECTION('center_axis',(0.,0.,1.));
#71078=DIRECTION('ref_axis',(1.,0.,0.));
#71079=DIRECTION('',(0.707106781186558,8.65956056235506E-17,-0.707106781186537));
#71080=DIRECTION('center_axis',(0.,0.,1.));
#71081=DIRECTION('ref_axis',(1.,0.,0.));
#71082=DIRECTION('center_axis',(0.,0.,1.));
#71083=DIRECTION('ref_axis',(1.,0.,0.));
#71084=DIRECTION('',(0.,0.,-1.));
#71085=DIRECTION('center_axis',(0.,0.,-1.));
#71086=DIRECTION('ref_axis',(-1.,0.,0.));
#71087=DIRECTION('center_axis',(0.,0.,1.));
#71088=DIRECTION('ref_axis',(1.,0.,0.));
#71089=DIRECTION('center_axis',(0.,0.,1.));
#71090=DIRECTION('ref_axis',(1.,0.,0.));
#71091=DIRECTION('center_axis',(0.,0.,1.));
#71092=DIRECTION('ref_axis',(1.,0.,0.));
#71093=DIRECTION('',(0.707106781186537,8.6595605623548E-17,-0.707106781186558));
#71094=DIRECTION('center_axis',(0.,0.,1.));
#71095=DIRECTION('ref_axis',(1.,0.,0.));
#71096=DIRECTION('center_axis',(0.,0.,1.));
#71097=DIRECTION('ref_axis',(1.,0.,0.));
#71098=DIRECTION('',(0.,0.,-1.));
#71099=DIRECTION('center_axis',(0.,0.,1.));
#71100=DIRECTION('ref_axis',(1.,0.,0.));
#71101=DIRECTION('center_axis',(0.,0.,1.));
#71102=DIRECTION('ref_axis',(1.,0.,0.));
#71103=DIRECTION('center_axis',(0.,0.,1.));
#71104=DIRECTION('ref_axis',(1.,0.,0.));
#71105=DIRECTION('',(0.707106781186537,8.6595605623548E-17,-0.707106781186558));
#71106=DIRECTION('center_axis',(0.,0.,1.));
#71107=DIRECTION('ref_axis',(1.,0.,0.));
#71108=DIRECTION('center_axis',(0.,0.,1.));
#71109=DIRECTION('ref_axis',(1.,0.,0.));
#71110=DIRECTION('',(0.,0.,-1.));
#71111=DIRECTION('axis',(0.,0.,1.));
#71112=DIRECTION('refdir',(1.,0.,0.));
#71113=DIRECTION('center_axis',(0.,1.,0.));
#71114=DIRECTION('ref_axis',(1.,0.,0.));
#71115=DIRECTION('center_axis',(0.,1.,0.));
#71116=DIRECTION('ref_axis',(1.,0.,0.));
#71117=DIRECTION('',(0.707106781186561,-0.707106781186534,-8.65956056235509E-17));
#71118=DIRECTION('center_axis',(0.,-1.,0.));
#71119=DIRECTION('ref_axis',(1.,0.,0.));
#71120=DIRECTION('center_axis',(0.,-1.,0.));
#71121=DIRECTION('ref_axis',(1.,0.,0.));
#71122=DIRECTION('',(0.,-1.,0.));
#71123=DIRECTION('center_axis',(0.,-1.,0.));
#71124=DIRECTION('ref_axis',(1.,0.,0.));
#71125=DIRECTION('center_axis',(0.,1.,0.));
#71126=DIRECTION('ref_axis',(-1.,0.,0.));
#71127=DIRECTION('',(-1.,0.,0.));
#71128=DIRECTION('',(0.,0.,1.));
#71129=DIRECTION('',(-1.,0.,0.));
#71130=DIRECTION('',(0.,0.,1.));
#71131=DIRECTION('center_axis',(0.,1.,0.));
#71132=DIRECTION('ref_axis',(1.,0.,0.));
#71133=DIRECTION('center_axis',(0.,1.,0.));
#71134=DIRECTION('ref_axis',(1.,0.,0.));
#71135=DIRECTION('',(0.707106781186548,-0.707106781186548,-8.65956056235493E-17));
#71136=DIRECTION('center_axis',(0.,-1.,0.));
#71137=DIRECTION('ref_axis',(1.,0.,0.));
#71138=DIRECTION('center_axis',(0.,-1.,0.));
#71139=DIRECTION('ref_axis',(1.,0.,0.));
#71140=DIRECTION('',(0.,-1.,0.));
#71141=DIRECTION('center_axis',(0.,-1.,0.));
#71142=DIRECTION('ref_axis',(1.,0.,0.));
#71143=DIRECTION('center_axis',(0.,1.,0.));
#71144=DIRECTION('ref_axis',(-1.,0.,0.));
#71145=DIRECTION('',(-1.,0.,0.));
#71146=DIRECTION('',(0.,0.,1.));
#71147=DIRECTION('',(-1.,0.,0.));
#71148=DIRECTION('',(0.,0.,1.));
#71149=DIRECTION('center_axis',(0.,1.,0.));
#71150=DIRECTION('ref_axis',(1.,0.,0.));
#71151=DIRECTION('center_axis',(0.,1.,0.));
#71152=DIRECTION('ref_axis',(1.,0.,0.));
#71153=DIRECTION('center_axis',(0.,1.,0.));
#71154=DIRECTION('ref_axis',(1.,0.,0.));
#71155=DIRECTION('center_axis',(0.,1.,0.));
#71156=DIRECTION('ref_axis',(1.,0.,0.));
#71157=DIRECTION('center_axis',(0.,-1.,0.));
#71158=DIRECTION('ref_axis',(1.,0.,0.));
#71159=DIRECTION('',(0.,-1.,0.));
#71160=DIRECTION('center_axis',(0.,1.,0.));
#71161=DIRECTION('ref_axis',(1.,0.,0.));
#71162=DIRECTION('center_axis',(0.,-1.,0.));
#71163=DIRECTION('ref_axis',(1.,0.,0.));
#71164=DIRECTION('',(0.,-1.,0.));
#71165=DIRECTION('center_axis',(0.,1.,0.));
#71166=DIRECTION('ref_axis',(1.,0.,0.));
#71167=DIRECTION('center_axis',(0.,-0.707106781186545,0.70710678118655));
#71168=DIRECTION('ref_axis',(1.,0.,0.));
#71169=DIRECTION('',(0.,0.70710678118655,0.707106781186545));
#71170=DIRECTION('',(-1.,0.,0.));
#71171=DIRECTION('',(0.,-0.70710678118655,-0.707106781186545));
#71172=DIRECTION('',(1.,0.,0.));
#71173=DIRECTION('center_axis',(1.,0.,0.));
#71174=DIRECTION('ref_axis',(0.,1.,0.));
#71175=DIRECTION('',(0.,0.,1.));
#71176=DIRECTION('',(0.,-0.70710678118655,0.707106781186545));
#71177=DIRECTION('',(0.,1.,0.));
#71178=DIRECTION('',(0.,1.,0.));
#71179=DIRECTION('center_axis',(0.,-1.,0.));
#71180=DIRECTION('ref_axis',(1.,0.,0.));
#71181=DIRECTION('',(0.,0.,1.));
#71182=DIRECTION('',(-1.,0.,0.));
#71183=DIRECTION('center_axis',(0.,-0.707106781186545,-0.70710678118655));
#71184=DIRECTION('ref_axis',(-1.,0.,0.));
#71185=DIRECTION('',(0.,0.70710678118655,-0.707106781186545));
#71186=DIRECTION('',(1.,0.,0.));
#71187=DIRECTION('center_axis',(0.939692620785909,0.342020143325668,0.));
#71188=DIRECTION('ref_axis',(-0.342020143325668,0.939692620785909,0.));
#71189=DIRECTION('',(-0.342020143325668,0.939692620785909,0.));
#71190=DIRECTION('',(-0.342020143325668,0.939692620785909,0.));
#71191=DIRECTION('',(0.,0.,1.));
#71192=DIRECTION('center_axis',(0.,1.,0.));
#71193=DIRECTION('ref_axis',(-1.,0.,0.));
#71194=DIRECTION('',(-1.,0.,0.));
#71195=DIRECTION('',(-1.,0.,0.));
#71196=DIRECTION('',(0.,0.,1.));
#71197=DIRECTION('center_axis',(-0.939692620785909,0.342020143325668,0.));
#71198=DIRECTION('ref_axis',(-0.342020143325668,-0.939692620785909,0.));
#71199=DIRECTION('',(-0.342020143325668,-0.939692620785909,0.));
#71200=DIRECTION('',(-0.342020143325668,-0.939692620785909,0.));
#71201=DIRECTION('',(0.,0.,1.));
#71202=DIRECTION('center_axis',(0.,1.,0.));
#71203=DIRECTION('ref_axis',(-1.,0.,0.));
#71204=DIRECTION('',(-1.,0.,0.));
#71205=DIRECTION('',(-1.,0.,0.));
#71206=DIRECTION('',(0.,0.,1.));
#71207=DIRECTION('center_axis',(0.939692620785909,0.342020143325668,0.));
#71208=DIRECTION('ref_axis',(-0.342020143325668,0.939692620785909,0.));
#71209=DIRECTION('',(-0.342020143325668,0.939692620785909,0.));
#71210=DIRECTION('',(-0.342020143325668,0.939692620785909,0.));
#71211=DIRECTION('',(0.,0.,1.));
#71212=DIRECTION('center_axis',(0.,1.,0.));
#71213=DIRECTION('ref_axis',(-1.,0.,0.));
#71214=DIRECTION('',(-1.,0.,0.));
#71215=DIRECTION('',(-1.,0.,0.));
#71216=DIRECTION('',(0.,0.,1.));
#71217=DIRECTION('center_axis',(-0.939692620785909,0.342020143325668,0.));
#71218=DIRECTION('ref_axis',(-0.342020143325668,-0.939692620785909,0.));
#71219=DIRECTION('',(-0.342020143325668,-0.939692620785909,0.));
#71220=DIRECTION('',(-0.342020143325668,-0.939692620785909,0.));
#71221=DIRECTION('',(0.,0.,1.));
#71222=DIRECTION('center_axis',(0.,1.,0.));
#71223=DIRECTION('ref_axis',(-1.,0.,0.));
#71224=DIRECTION('',(-1.,0.,0.));
#71225=DIRECTION('',(-1.,0.,0.));
#71226=DIRECTION('',(0.,0.,1.));
#71227=DIRECTION('center_axis',(0.939692620785909,0.342020143325668,0.));
#71228=DIRECTION('ref_axis',(-0.342020143325668,0.939692620785909,0.));
#71229=DIRECTION('',(-0.342020143325668,0.939692620785909,0.));
#71230=DIRECTION('',(-0.342020143325668,0.939692620785909,0.));
#71231=DIRECTION('',(0.,0.,1.));
#71232=DIRECTION('center_axis',(0.,1.,0.));
#71233=DIRECTION('ref_axis',(-1.,0.,0.));
#71234=DIRECTION('',(-1.,0.,0.));
#71235=DIRECTION('',(-1.,0.,0.));
#71236=DIRECTION('',(0.,0.,1.));
#71237=DIRECTION('center_axis',(-0.939692620785909,0.342020143325668,0.));
#71238=DIRECTION('ref_axis',(-0.342020143325668,-0.939692620785909,0.));
#71239=DIRECTION('',(-0.342020143325668,-0.939692620785909,0.));
#71240=DIRECTION('',(-0.342020143325668,-0.939692620785909,0.));
#71241=DIRECTION('',(0.,0.,1.));
#71242=DIRECTION('center_axis',(0.,1.,0.));
#71243=DIRECTION('ref_axis',(-1.,0.,0.));
#71244=DIRECTION('',(-1.,0.,0.));
#71245=DIRECTION('',(-1.,0.,0.));
#71246=DIRECTION('',(0.,0.,1.));
#71247=DIRECTION('center_axis',(0.939692620785909,0.342020143325668,0.));
#71248=DIRECTION('ref_axis',(-0.342020143325668,0.939692620785909,0.));
#71249=DIRECTION('',(-0.342020143325668,0.939692620785909,0.));
#71250=DIRECTION('',(-0.342020143325668,0.939692620785909,0.));
#71251=DIRECTION('',(0.,0.,1.));
#71252=DIRECTION('center_axis',(0.,1.,0.));
#71253=DIRECTION('ref_axis',(-1.,0.,0.));
#71254=DIRECTION('',(-1.,0.,0.));
#71255=DIRECTION('',(-1.,0.,0.));
#71256=DIRECTION('',(0.,0.,1.));
#71257=DIRECTION('center_axis',(-0.939692620785909,0.342020143325668,0.));
#71258=DIRECTION('ref_axis',(-0.342020143325668,-0.939692620785909,0.));
#71259=DIRECTION('',(-0.342020143325668,-0.939692620785909,0.));
#71260=DIRECTION('',(-0.342020143325668,-0.939692620785909,0.));
#71261=DIRECTION('',(0.,0.,1.));
#71262=DIRECTION('center_axis',(0.,1.,0.));
#71263=DIRECTION('ref_axis',(-1.,0.,0.));
#71264=DIRECTION('',(-1.,0.,0.));
#71265=DIRECTION('',(-1.,0.,0.));
#71266=DIRECTION('',(0.,0.,1.));
#71267=DIRECTION('center_axis',(0.939692620785909,0.342020143325668,0.));
#71268=DIRECTION('ref_axis',(-0.342020143325668,0.939692620785909,0.));
#71269=DIRECTION('',(-0.342020143325668,0.939692620785909,0.));
#71270=DIRECTION('',(-0.342020143325668,0.939692620785909,0.));
#71271=DIRECTION('',(0.,0.,1.));
#71272=DIRECTION('center_axis',(0.,1.,0.));
#71273=DIRECTION('ref_axis',(-1.,0.,0.));
#71274=DIRECTION('',(-1.,0.,0.));
#71275=DIRECTION('',(-1.,0.,0.));
#71276=DIRECTION('',(0.,0.,1.));
#71277=DIRECTION('center_axis',(-0.939692620785909,0.342020143325668,0.));
#71278=DIRECTION('ref_axis',(-0.342020143325668,-0.939692620785909,0.));
#71279=DIRECTION('',(-0.342020143325668,-0.939692620785909,0.));
#71280=DIRECTION('',(-0.342020143325668,-0.939692620785909,0.));
#71281=DIRECTION('',(0.,0.,1.));
#71282=DIRECTION('center_axis',(0.,1.,0.));
#71283=DIRECTION('ref_axis',(-1.,0.,0.));
#71284=DIRECTION('',(-1.,0.,0.));
#71285=DIRECTION('',(-1.,0.,0.));
#71286=DIRECTION('',(0.,0.,1.));
#71287=DIRECTION('center_axis',(0.939692620785909,0.342020143325668,0.));
#71288=DIRECTION('ref_axis',(-0.342020143325668,0.939692620785909,0.));
#71289=DIRECTION('',(-0.342020143325668,0.939692620785909,0.));
#71290=DIRECTION('',(-0.342020143325668,0.939692620785909,0.));
#71291=DIRECTION('',(0.,0.,1.));
#71292=DIRECTION('center_axis',(0.,1.,0.));
#71293=DIRECTION('ref_axis',(-1.,0.,0.));
#71294=DIRECTION('',(-1.,0.,0.));
#71295=DIRECTION('',(-1.,0.,0.));
#71296=DIRECTION('',(0.,0.,1.));
#71297=DIRECTION('center_axis',(-0.939692620785909,0.342020143325668,0.));
#71298=DIRECTION('ref_axis',(-0.342020143325668,-0.939692620785909,0.));
#71299=DIRECTION('',(-0.342020143325668,-0.939692620785909,0.));
#71300=DIRECTION('',(-0.342020143325668,-0.939692620785909,0.));
#71301=DIRECTION('',(0.,0.,1.));
#71302=DIRECTION('center_axis',(0.,1.,0.));
#71303=DIRECTION('ref_axis',(-1.,0.,0.));
#71304=DIRECTION('',(-1.,0.,0.));
#71305=DIRECTION('',(-1.,0.,0.));
#71306=DIRECTION('',(0.,0.,1.));
#71307=DIRECTION('center_axis',(0.939692620785909,0.342020143325668,0.));
#71308=DIRECTION('ref_axis',(-0.342020143325668,0.939692620785909,0.));
#71309=DIRECTION('',(-0.342020143325668,0.939692620785909,0.));
#71310=DIRECTION('',(-0.342020143325668,0.939692620785909,0.));
#71311=DIRECTION('',(0.,0.,1.));
#71312=DIRECTION('center_axis',(0.,1.,0.));
#71313=DIRECTION('ref_axis',(-1.,0.,0.));
#71314=DIRECTION('',(-1.,0.,0.));
#71315=DIRECTION('',(-1.,0.,0.));
#71316=DIRECTION('',(0.,0.,1.));
#71317=DIRECTION('center_axis',(-0.939692620785909,0.342020143325668,0.));
#71318=DIRECTION('ref_axis',(-0.342020143325668,-0.939692620785909,0.));
#71319=DIRECTION('',(-0.342020143325668,-0.939692620785909,0.));
#71320=DIRECTION('',(-0.342020143325668,-0.939692620785909,0.));
#71321=DIRECTION('',(0.,0.,1.));
#71322=DIRECTION('center_axis',(0.,1.,0.));
#71323=DIRECTION('ref_axis',(-1.,0.,0.));
#71324=DIRECTION('',(-1.,0.,0.));
#71325=DIRECTION('',(-1.,0.,0.));
#71326=DIRECTION('',(0.,0.,1.));
#71327=DIRECTION('center_axis',(0.939692620785909,0.342020143325668,0.));
#71328=DIRECTION('ref_axis',(-0.342020143325668,0.939692620785909,0.));
#71329=DIRECTION('',(-0.342020143325668,0.939692620785909,0.));
#71330=DIRECTION('',(-0.342020143325668,0.939692620785909,0.));
#71331=DIRECTION('',(0.,0.,1.));
#71332=DIRECTION('center_axis',(0.,1.,0.));
#71333=DIRECTION('ref_axis',(-1.,0.,0.));
#71334=DIRECTION('',(-1.,0.,0.));
#71335=DIRECTION('',(-1.,0.,0.));
#71336=DIRECTION('',(0.,0.,1.));
#71337=DIRECTION('center_axis',(-0.939692620785909,0.342020143325668,0.));
#71338=DIRECTION('ref_axis',(-0.342020143325668,-0.939692620785909,0.));
#71339=DIRECTION('',(-0.342020143325668,-0.939692620785909,0.));
#71340=DIRECTION('',(-0.342020143325668,-0.939692620785909,0.));
#71341=DIRECTION('',(0.,0.,1.));
#71342=DIRECTION('center_axis',(0.,1.,0.));
#71343=DIRECTION('ref_axis',(-1.,0.,0.));
#71344=DIRECTION('',(-1.,0.,0.));
#71345=DIRECTION('',(-1.,0.,0.));
#71346=DIRECTION('',(0.,0.,1.));
#71347=DIRECTION('center_axis',(0.939692620785909,0.342020143325668,0.));
#71348=DIRECTION('ref_axis',(-0.342020143325668,0.939692620785909,0.));
#71349=DIRECTION('',(-0.342020143325668,0.939692620785909,0.));
#71350=DIRECTION('',(-0.342020143325668,0.939692620785909,0.));
#71351=DIRECTION('',(0.,0.,1.));
#71352=DIRECTION('center_axis',(0.,1.,0.));
#71353=DIRECTION('ref_axis',(-1.,0.,0.));
#71354=DIRECTION('',(-1.,0.,0.));
#71355=DIRECTION('',(-1.,0.,0.));
#71356=DIRECTION('',(0.,0.,1.));
#71357=DIRECTION('center_axis',(-0.939692620785909,0.342020143325668,0.));
#71358=DIRECTION('ref_axis',(-0.342020143325668,-0.939692620785909,0.));
#71359=DIRECTION('',(-0.342020143325668,-0.939692620785909,0.));
#71360=DIRECTION('',(-0.342020143325668,-0.939692620785909,0.));
#71361=DIRECTION('',(0.,0.,1.));
#71362=DIRECTION('center_axis',(0.,1.,0.));
#71363=DIRECTION('ref_axis',(-1.,0.,0.));
#71364=DIRECTION('',(-1.,0.,0.));
#71365=DIRECTION('',(-1.,0.,0.));
#71366=DIRECTION('',(0.,0.,1.));
#71367=DIRECTION('center_axis',(0.939692620785909,0.342020143325668,0.));
#71368=DIRECTION('ref_axis',(-0.342020143325668,0.939692620785909,0.));
#71369=DIRECTION('',(-0.342020143325668,0.939692620785909,0.));
#71370=DIRECTION('',(-0.342020143325668,0.939692620785909,0.));
#71371=DIRECTION('',(0.,0.,1.));
#71372=DIRECTION('center_axis',(0.,1.,0.));
#71373=DIRECTION('ref_axis',(-1.,0.,0.));
#71374=DIRECTION('',(-1.,0.,0.));
#71375=DIRECTION('',(-1.,0.,0.));
#71376=DIRECTION('',(0.,0.,1.));
#71377=DIRECTION('center_axis',(-0.939692620785909,0.342020143325668,0.));
#71378=DIRECTION('ref_axis',(-0.342020143325668,-0.939692620785909,0.));
#71379=DIRECTION('',(-0.342020143325668,-0.939692620785909,0.));
#71380=DIRECTION('',(-0.342020143325668,-0.939692620785909,0.));
#71381=DIRECTION('',(0.,0.,1.));
#71382=DIRECTION('center_axis',(0.,1.,0.));
#71383=DIRECTION('ref_axis',(-1.,0.,0.));
#71384=DIRECTION('',(-1.,0.,0.));
#71385=DIRECTION('',(-1.,0.,0.));
#71386=DIRECTION('',(0.,0.,1.));
#71387=DIRECTION('center_axis',(0.939692620785909,0.342020143325668,0.));
#71388=DIRECTION('ref_axis',(-0.342020143325668,0.939692620785909,0.));
#71389=DIRECTION('',(-0.342020143325668,0.939692620785909,0.));
#71390=DIRECTION('',(-0.342020143325668,0.939692620785909,0.));
#71391=DIRECTION('',(0.,0.,1.));
#71392=DIRECTION('center_axis',(0.,1.,0.));
#71393=DIRECTION('ref_axis',(-1.,0.,0.));
#71394=DIRECTION('',(-1.,0.,0.));
#71395=DIRECTION('',(-1.,0.,0.));
#71396=DIRECTION('',(0.,0.,1.));
#71397=DIRECTION('center_axis',(-0.939692620785909,0.342020143325668,0.));
#71398=DIRECTION('ref_axis',(-0.342020143325668,-0.939692620785909,0.));
#71399=DIRECTION('',(-0.342020143325668,-0.939692620785909,0.));
#71400=DIRECTION('',(-0.342020143325668,-0.939692620785909,0.));
#71401=DIRECTION('',(0.,0.,1.));
#71402=DIRECTION('center_axis',(0.,1.,0.));
#71403=DIRECTION('ref_axis',(-1.,0.,0.));
#71404=DIRECTION('',(-1.,0.,0.));
#71405=DIRECTION('',(-1.,0.,0.));
#71406=DIRECTION('',(0.,0.,1.));
#71407=DIRECTION('center_axis',(0.939692620785909,0.342020143325668,0.));
#71408=DIRECTION('ref_axis',(-0.342020143325668,0.939692620785909,0.));
#71409=DIRECTION('',(-0.342020143325668,0.939692620785909,0.));
#71410=DIRECTION('',(-0.342020143325668,0.939692620785909,0.));
#71411=DIRECTION('',(0.,0.,1.));
#71412=DIRECTION('center_axis',(0.,1.,0.));
#71413=DIRECTION('ref_axis',(-1.,0.,0.));
#71414=DIRECTION('',(-1.,0.,0.));
#71415=DIRECTION('',(-1.,0.,0.));
#71416=DIRECTION('',(0.,0.,1.));
#71417=DIRECTION('center_axis',(-0.939692620785909,0.342020143325668,0.));
#71418=DIRECTION('ref_axis',(-0.342020143325668,-0.939692620785909,0.));
#71419=DIRECTION('',(-0.342020143325668,-0.939692620785909,0.));
#71420=DIRECTION('',(-0.342020143325668,-0.939692620785909,0.));
#71421=DIRECTION('',(0.,0.,1.));
#71422=DIRECTION('center_axis',(0.,1.,0.));
#71423=DIRECTION('ref_axis',(-1.,0.,0.));
#71424=DIRECTION('',(-1.,0.,0.));
#71425=DIRECTION('',(-1.,0.,0.));
#71426=DIRECTION('',(0.,0.,1.));
#71427=DIRECTION('center_axis',(0.939692620785909,0.342020143325668,0.));
#71428=DIRECTION('ref_axis',(-0.342020143325668,0.939692620785909,0.));
#71429=DIRECTION('',(-0.342020143325668,0.939692620785909,0.));
#71430=DIRECTION('',(-0.342020143325668,0.939692620785909,0.));
#71431=DIRECTION('',(0.,0.,1.));
#71432=DIRECTION('center_axis',(0.,1.,0.));
#71433=DIRECTION('ref_axis',(-1.,0.,0.));
#71434=DIRECTION('',(-1.,0.,0.));
#71435=DIRECTION('',(-1.,0.,0.));
#71436=DIRECTION('',(0.,0.,1.));
#71437=DIRECTION('center_axis',(-0.939692620785909,0.342020143325668,0.));
#71438=DIRECTION('ref_axis',(-0.342020143325668,-0.939692620785909,0.));
#71439=DIRECTION('',(-0.342020143325668,-0.939692620785909,0.));
#71440=DIRECTION('',(-0.342020143325668,-0.939692620785909,0.));
#71441=DIRECTION('',(0.,0.,1.));
#71442=DIRECTION('center_axis',(0.,1.,0.));
#71443=DIRECTION('ref_axis',(-1.,0.,0.));
#71444=DIRECTION('',(-1.,0.,0.));
#71445=DIRECTION('',(-1.,0.,0.));
#71446=DIRECTION('',(0.,0.,1.));
#71447=DIRECTION('center_axis',(0.939692620785909,0.342020143325668,0.));
#71448=DIRECTION('ref_axis',(-0.342020143325668,0.939692620785909,0.));
#71449=DIRECTION('',(-0.342020143325668,0.939692620785909,0.));
#71450=DIRECTION('',(-0.342020143325668,0.939692620785909,0.));
#71451=DIRECTION('',(0.,0.,1.));
#71452=DIRECTION('center_axis',(0.,1.,0.));
#71453=DIRECTION('ref_axis',(-1.,0.,0.));
#71454=DIRECTION('',(-1.,0.,0.));
#71455=DIRECTION('',(-1.,0.,0.));
#71456=DIRECTION('',(0.,0.,1.));
#71457=DIRECTION('center_axis',(-0.939692620785909,0.342020143325668,0.));
#71458=DIRECTION('ref_axis',(-0.342020143325668,-0.939692620785909,0.));
#71459=DIRECTION('',(-0.342020143325668,-0.939692620785909,0.));
#71460=DIRECTION('',(-0.342020143325668,-0.939692620785909,0.));
#71461=DIRECTION('',(0.,0.,1.));
#71462=DIRECTION('center_axis',(0.,1.,0.));
#71463=DIRECTION('ref_axis',(-1.,0.,0.));
#71464=DIRECTION('',(-1.,0.,0.));
#71465=DIRECTION('',(-1.,0.,0.));
#71466=DIRECTION('',(0.,0.,1.));
#71467=DIRECTION('center_axis',(0.939692620785909,0.342020143325668,0.));
#71468=DIRECTION('ref_axis',(-0.342020143325668,0.939692620785909,0.));
#71469=DIRECTION('',(-0.342020143325668,0.939692620785909,0.));
#71470=DIRECTION('',(-0.342020143325668,0.939692620785909,0.));
#71471=DIRECTION('',(0.,0.,1.));
#71472=DIRECTION('center_axis',(0.,1.,0.));
#71473=DIRECTION('ref_axis',(-1.,0.,0.));
#71474=DIRECTION('',(-1.,0.,0.));
#71475=DIRECTION('',(-1.,0.,0.));
#71476=DIRECTION('',(0.,0.,1.));
#71477=DIRECTION('center_axis',(-0.939692620785909,0.342020143325668,0.));
#71478=DIRECTION('ref_axis',(-0.342020143325668,-0.939692620785909,0.));
#71479=DIRECTION('',(-0.342020143325668,-0.939692620785909,0.));
#71480=DIRECTION('',(-0.342020143325668,-0.939692620785909,0.));
#71481=DIRECTION('',(0.,0.,1.));
#71482=DIRECTION('center_axis',(0.,1.,0.));
#71483=DIRECTION('ref_axis',(-1.,0.,0.));
#71484=DIRECTION('',(-1.,0.,0.));
#71485=DIRECTION('',(-1.,0.,0.));
#71486=DIRECTION('',(0.,0.,1.));
#71487=DIRECTION('center_axis',(0.939692620785909,0.342020143325668,0.));
#71488=DIRECTION('ref_axis',(-0.342020143325668,0.939692620785909,0.));
#71489=DIRECTION('',(-0.342020143325668,0.939692620785909,0.));
#71490=DIRECTION('',(-0.342020143325668,0.939692620785909,0.));
#71491=DIRECTION('',(0.,0.,1.));
#71492=DIRECTION('center_axis',(0.,1.,0.));
#71493=DIRECTION('ref_axis',(-1.,0.,0.));
#71494=DIRECTION('',(-1.,0.,0.));
#71495=DIRECTION('',(-1.,0.,0.));
#71496=DIRECTION('',(0.,0.,1.));
#71497=DIRECTION('center_axis',(-0.939692620785909,0.342020143325668,0.));
#71498=DIRECTION('ref_axis',(-0.342020143325668,-0.939692620785909,0.));
#71499=DIRECTION('',(-0.342020143325668,-0.939692620785909,0.));
#71500=DIRECTION('',(-0.342020143325668,-0.939692620785909,0.));
#71501=DIRECTION('',(0.,0.,1.));
#71502=DIRECTION('center_axis',(0.,1.,0.));
#71503=DIRECTION('ref_axis',(-1.,0.,0.));
#71504=DIRECTION('',(-1.,0.,0.));
#71505=DIRECTION('',(-1.,0.,0.));
#71506=DIRECTION('',(0.,0.,1.));
#71507=DIRECTION('center_axis',(0.939692620785909,0.342020143325668,0.));
#71508=DIRECTION('ref_axis',(-0.342020143325668,0.939692620785909,0.));
#71509=DIRECTION('',(-0.342020143325668,0.939692620785909,0.));
#71510=DIRECTION('',(-0.342020143325668,0.939692620785909,0.));
#71511=DIRECTION('',(0.,0.,1.));
#71512=DIRECTION('center_axis',(0.,1.,0.));
#71513=DIRECTION('ref_axis',(-1.,0.,0.));
#71514=DIRECTION('',(-1.,0.,0.));
#71515=DIRECTION('',(-1.,0.,0.));
#71516=DIRECTION('',(0.,0.,1.));
#71517=DIRECTION('center_axis',(-0.939692620785909,0.342020143325668,0.));
#71518=DIRECTION('ref_axis',(-0.342020143325668,-0.939692620785909,0.));
#71519=DIRECTION('',(-0.342020143325668,-0.939692620785909,0.));
#71520=DIRECTION('',(-0.342020143325668,-0.939692620785909,0.));
#71521=DIRECTION('',(0.,0.,1.));
#71522=DIRECTION('center_axis',(0.,1.,0.));
#71523=DIRECTION('ref_axis',(-1.,0.,0.));
#71524=DIRECTION('',(-1.,0.,0.));
#71525=DIRECTION('',(-1.,0.,0.));
#71526=DIRECTION('',(0.,0.,1.));
#71527=DIRECTION('center_axis',(0.939692620785909,0.342020143325668,0.));
#71528=DIRECTION('ref_axis',(-0.342020143325668,0.939692620785909,0.));
#71529=DIRECTION('',(-0.342020143325668,0.939692620785909,0.));
#71530=DIRECTION('',(-0.342020143325668,0.939692620785909,0.));
#71531=DIRECTION('',(0.,0.,1.));
#71532=DIRECTION('center_axis',(0.,1.,0.));
#71533=DIRECTION('ref_axis',(-1.,0.,0.));
#71534=DIRECTION('',(-1.,0.,0.));
#71535=DIRECTION('',(-1.,0.,0.));
#71536=DIRECTION('',(0.,0.,1.));
#71537=DIRECTION('center_axis',(-0.939692620785909,0.342020143325668,0.));
#71538=DIRECTION('ref_axis',(-0.342020143325668,-0.939692620785909,0.));
#71539=DIRECTION('',(-0.342020143325668,-0.939692620785909,0.));
#71540=DIRECTION('',(-0.342020143325668,-0.939692620785909,0.));
#71541=DIRECTION('',(0.,0.,1.));
#71542=DIRECTION('center_axis',(0.,1.,0.));
#71543=DIRECTION('ref_axis',(-1.,0.,0.));
#71544=DIRECTION('',(-1.,0.,0.));
#71545=DIRECTION('',(-1.,0.,0.));
#71546=DIRECTION('',(0.,0.,1.));
#71547=DIRECTION('center_axis',(0.939692620785909,0.342020143325668,0.));
#71548=DIRECTION('ref_axis',(-0.342020143325668,0.939692620785909,0.));
#71549=DIRECTION('',(-0.342020143325668,0.939692620785909,0.));
#71550=DIRECTION('',(-0.342020143325668,0.939692620785909,0.));
#71551=DIRECTION('',(0.,0.,1.));
#71552=DIRECTION('center_axis',(0.,1.,0.));
#71553=DIRECTION('ref_axis',(-1.,0.,0.));
#71554=DIRECTION('',(-1.,0.,0.));
#71555=DIRECTION('',(-1.,0.,0.));
#71556=DIRECTION('',(0.,0.,1.));
#71557=DIRECTION('center_axis',(-0.939692620785909,0.342020143325668,0.));
#71558=DIRECTION('ref_axis',(-0.342020143325668,-0.939692620785909,0.));
#71559=DIRECTION('',(-0.342020143325668,-0.939692620785909,0.));
#71560=DIRECTION('',(-0.342020143325668,-0.939692620785909,0.));
#71561=DIRECTION('',(0.,0.,1.));
#71562=DIRECTION('center_axis',(0.,1.,0.));
#71563=DIRECTION('ref_axis',(-1.,0.,0.));
#71564=DIRECTION('',(-1.,0.,0.));
#71565=DIRECTION('',(-1.,0.,0.));
#71566=DIRECTION('',(0.,0.,1.));
#71567=DIRECTION('center_axis',(0.939692620785909,0.342020143325668,0.));
#71568=DIRECTION('ref_axis',(-0.342020143325668,0.939692620785909,0.));
#71569=DIRECTION('',(-0.342020143325668,0.939692620785909,0.));
#71570=DIRECTION('',(-0.342020143325668,0.939692620785909,0.));
#71571=DIRECTION('',(0.,0.,1.));
#71572=DIRECTION('center_axis',(0.,1.,0.));
#71573=DIRECTION('ref_axis',(-1.,0.,0.));
#71574=DIRECTION('',(-1.,0.,0.));
#71575=DIRECTION('',(-1.,0.,0.));
#71576=DIRECTION('',(0.,0.,1.));
#71577=DIRECTION('center_axis',(-0.939692620785909,0.342020143325668,0.));
#71578=DIRECTION('ref_axis',(-0.342020143325668,-0.939692620785909,0.));
#71579=DIRECTION('',(-0.342020143325668,-0.939692620785909,0.));
#71580=DIRECTION('',(-0.342020143325668,-0.939692620785909,0.));
#71581=DIRECTION('',(0.,0.,1.));
#71582=DIRECTION('center_axis',(0.,1.,0.));
#71583=DIRECTION('ref_axis',(-1.,0.,0.));
#71584=DIRECTION('',(-1.,0.,0.));
#71585=DIRECTION('',(-1.,0.,0.));
#71586=DIRECTION('',(0.,0.,1.));
#71587=DIRECTION('center_axis',(0.939692620785909,0.342020143325668,0.));
#71588=DIRECTION('ref_axis',(-0.342020143325668,0.939692620785909,0.));
#71589=DIRECTION('',(-0.342020143325668,0.939692620785909,0.));
#71590=DIRECTION('',(-0.342020143325668,0.939692620785909,0.));
#71591=DIRECTION('',(0.,0.,1.));
#71592=DIRECTION('center_axis',(0.,1.,0.));
#71593=DIRECTION('ref_axis',(-1.,0.,0.));
#71594=DIRECTION('',(-1.,0.,0.));
#71595=DIRECTION('',(-1.,0.,0.));
#71596=DIRECTION('',(0.,0.,1.));
#71597=DIRECTION('center_axis',(-0.939692620785909,0.342020143325668,0.));
#71598=DIRECTION('ref_axis',(-0.342020143325668,-0.939692620785909,0.));
#71599=DIRECTION('',(-0.342020143325668,-0.939692620785909,0.));
#71600=DIRECTION('',(-0.342020143325668,-0.939692620785909,0.));
#71601=DIRECTION('',(0.,0.,1.));
#71602=DIRECTION('center_axis',(0.,1.,0.));
#71603=DIRECTION('ref_axis',(-1.,0.,0.));
#71604=DIRECTION('',(-1.,0.,0.));
#71605=DIRECTION('',(-1.,0.,0.));
#71606=DIRECTION('',(0.,0.,1.));
#71607=DIRECTION('center_axis',(0.939692620785909,0.342020143325668,0.));
#71608=DIRECTION('ref_axis',(-0.342020143325668,0.939692620785909,0.));
#71609=DIRECTION('',(-0.342020143325668,0.939692620785909,0.));
#71610=DIRECTION('',(-0.342020143325668,0.939692620785909,0.));
#71611=DIRECTION('',(0.,0.,1.));
#71612=DIRECTION('center_axis',(0.,1.,0.));
#71613=DIRECTION('ref_axis',(-1.,0.,0.));
#71614=DIRECTION('',(-1.,0.,0.));
#71615=DIRECTION('',(-1.,0.,0.));
#71616=DIRECTION('',(0.,0.,1.));
#71617=DIRECTION('center_axis',(-0.939692620785909,0.342020143325668,0.));
#71618=DIRECTION('ref_axis',(-0.342020143325668,-0.939692620785909,0.));
#71619=DIRECTION('',(-0.342020143325668,-0.939692620785909,0.));
#71620=DIRECTION('',(-0.342020143325668,-0.939692620785909,0.));
#71621=DIRECTION('',(0.,0.,1.));
#71622=DIRECTION('center_axis',(0.,1.,0.));
#71623=DIRECTION('ref_axis',(-1.,0.,0.));
#71624=DIRECTION('',(-1.,0.,0.));
#71625=DIRECTION('',(-1.,0.,0.));
#71626=DIRECTION('',(0.,0.,1.));
#71627=DIRECTION('center_axis',(0.939692620785909,0.342020143325668,0.));
#71628=DIRECTION('ref_axis',(-0.342020143325668,0.939692620785909,0.));
#71629=DIRECTION('',(-0.342020143325668,0.939692620785909,0.));
#71630=DIRECTION('',(-0.342020143325668,0.939692620785909,0.));
#71631=DIRECTION('',(0.,0.,1.));
#71632=DIRECTION('center_axis',(0.,1.,0.));
#71633=DIRECTION('ref_axis',(-1.,0.,0.));
#71634=DIRECTION('',(-1.,0.,0.));
#71635=DIRECTION('',(-1.,0.,0.));
#71636=DIRECTION('',(0.,0.,1.));
#71637=DIRECTION('center_axis',(-0.939692620785909,0.342020143325668,0.));
#71638=DIRECTION('ref_axis',(-0.342020143325668,-0.939692620785909,0.));
#71639=DIRECTION('',(-0.342020143325668,-0.939692620785909,0.));
#71640=DIRECTION('',(-0.342020143325668,-0.939692620785909,0.));
#71641=DIRECTION('',(0.,0.,1.));
#71642=DIRECTION('center_axis',(0.,1.,0.));
#71643=DIRECTION('ref_axis',(-1.,0.,0.));
#71644=DIRECTION('',(-1.,0.,0.));
#71645=DIRECTION('',(-1.,0.,0.));
#71646=DIRECTION('',(0.,0.,1.));
#71647=DIRECTION('center_axis',(0.939692620785909,0.342020143325668,0.));
#71648=DIRECTION('ref_axis',(-0.342020143325668,0.939692620785909,0.));
#71649=DIRECTION('',(-0.342020143325668,0.939692620785909,0.));
#71650=DIRECTION('',(-0.342020143325668,0.939692620785909,0.));
#71651=DIRECTION('',(0.,0.,1.));
#71652=DIRECTION('center_axis',(0.,1.,0.));
#71653=DIRECTION('ref_axis',(-1.,0.,0.));
#71654=DIRECTION('',(-1.,0.,0.));
#71655=DIRECTION('',(-1.,0.,0.));
#71656=DIRECTION('',(0.,0.,1.));
#71657=DIRECTION('center_axis',(-0.939692620785909,0.342020143325668,0.));
#71658=DIRECTION('ref_axis',(-0.342020143325668,-0.939692620785909,0.));
#71659=DIRECTION('',(-0.342020143325668,-0.939692620785909,0.));
#71660=DIRECTION('',(-0.342020143325668,-0.939692620785909,0.));
#71661=DIRECTION('',(0.,0.,1.));
#71662=DIRECTION('center_axis',(0.,1.,0.));
#71663=DIRECTION('ref_axis',(-1.,0.,0.));
#71664=DIRECTION('',(-1.,0.,0.));
#71665=DIRECTION('',(-1.,0.,0.));
#71666=DIRECTION('',(0.,0.,1.));
#71667=DIRECTION('center_axis',(0.939692620785909,0.342020143325668,0.));
#71668=DIRECTION('ref_axis',(-0.342020143325668,0.939692620785909,0.));
#71669=DIRECTION('',(-0.342020143325668,0.939692620785909,0.));
#71670=DIRECTION('',(-0.342020143325668,0.939692620785909,0.));
#71671=DIRECTION('',(0.,0.,1.));
#71672=DIRECTION('center_axis',(0.,1.,0.));
#71673=DIRECTION('ref_axis',(-1.,0.,0.));
#71674=DIRECTION('',(-1.,0.,0.));
#71675=DIRECTION('',(-1.,0.,0.));
#71676=DIRECTION('',(0.,0.,1.));
#71677=DIRECTION('center_axis',(-0.939692620785909,0.342020143325668,0.));
#71678=DIRECTION('ref_axis',(-0.342020143325668,-0.939692620785909,0.));
#71679=DIRECTION('',(-0.342020143325668,-0.939692620785909,0.));
#71680=DIRECTION('',(-0.342020143325668,-0.939692620785909,0.));
#71681=DIRECTION('',(0.,0.,1.));
#71682=DIRECTION('center_axis',(0.,1.,0.));
#71683=DIRECTION('ref_axis',(-1.,0.,0.));
#71684=DIRECTION('',(-1.,0.,0.));
#71685=DIRECTION('',(-1.,0.,0.));
#71686=DIRECTION('',(0.,0.,1.));
#71687=DIRECTION('center_axis',(0.939692620785909,0.342020143325668,0.));
#71688=DIRECTION('ref_axis',(-0.342020143325668,0.939692620785909,0.));
#71689=DIRECTION('',(-0.342020143325668,0.939692620785909,0.));
#71690=DIRECTION('',(-0.342020143325668,0.939692620785909,0.));
#71691=DIRECTION('',(0.,0.,1.));
#71692=DIRECTION('center_axis',(0.,1.,0.));
#71693=DIRECTION('ref_axis',(-1.,0.,0.));
#71694=DIRECTION('',(-1.,0.,0.));
#71695=DIRECTION('',(-1.,0.,0.));
#71696=DIRECTION('',(0.,0.,1.));
#71697=DIRECTION('center_axis',(-0.939692620785909,0.342020143325668,0.));
#71698=DIRECTION('ref_axis',(-0.342020143325668,-0.939692620785909,0.));
#71699=DIRECTION('',(-0.342020143325668,-0.939692620785909,0.));
#71700=DIRECTION('',(-0.342020143325668,-0.939692620785909,0.));
#71701=DIRECTION('',(0.,0.,1.));
#71702=DIRECTION('center_axis',(0.,1.,0.));
#71703=DIRECTION('ref_axis',(-1.,0.,0.));
#71704=DIRECTION('',(-1.,0.,0.));
#71705=DIRECTION('',(-1.,0.,0.));
#71706=DIRECTION('',(0.,0.,1.));
#71707=DIRECTION('center_axis',(0.939692620785909,0.342020143325668,0.));
#71708=DIRECTION('ref_axis',(-0.342020143325668,0.939692620785909,0.));
#71709=DIRECTION('',(-0.342020143325668,0.939692620785909,0.));
#71710=DIRECTION('',(-0.342020143325668,0.939692620785909,0.));
#71711=DIRECTION('',(0.,0.,1.));
#71712=DIRECTION('center_axis',(0.,1.,0.));
#71713=DIRECTION('ref_axis',(-1.,0.,0.));
#71714=DIRECTION('',(-1.,0.,0.));
#71715=DIRECTION('',(-1.,0.,0.));
#71716=DIRECTION('',(0.,0.,1.));
#71717=DIRECTION('center_axis',(-0.939692620785909,0.342020143325668,0.));
#71718=DIRECTION('ref_axis',(-0.342020143325668,-0.939692620785909,0.));
#71719=DIRECTION('',(-0.342020143325668,-0.939692620785909,0.));
#71720=DIRECTION('',(-0.342020143325668,-0.939692620785909,0.));
#71721=DIRECTION('',(0.,0.,1.));
#71722=DIRECTION('center_axis',(0.,1.,0.));
#71723=DIRECTION('ref_axis',(-1.,0.,0.));
#71724=DIRECTION('',(-1.,0.,0.));
#71725=DIRECTION('',(-1.,0.,0.));
#71726=DIRECTION('',(0.,0.,1.));
#71727=DIRECTION('center_axis',(0.939692620785909,0.342020143325668,0.));
#71728=DIRECTION('ref_axis',(-0.342020143325668,0.939692620785909,0.));
#71729=DIRECTION('',(-0.342020143325668,0.939692620785909,0.));
#71730=DIRECTION('',(-0.342020143325668,0.939692620785909,0.));
#71731=DIRECTION('',(0.,0.,1.));
#71732=DIRECTION('center_axis',(0.,1.,0.));
#71733=DIRECTION('ref_axis',(-1.,0.,0.));
#71734=DIRECTION('',(-1.,0.,0.));
#71735=DIRECTION('',(-1.,0.,0.));
#71736=DIRECTION('',(0.,0.,1.));
#71737=DIRECTION('center_axis',(-0.939692620785909,0.342020143325668,0.));
#71738=DIRECTION('ref_axis',(-0.342020143325668,-0.939692620785909,0.));
#71739=DIRECTION('',(-0.342020143325668,-0.939692620785909,0.));
#71740=DIRECTION('',(-0.342020143325668,-0.939692620785909,0.));
#71741=DIRECTION('',(0.,0.,1.));
#71742=DIRECTION('center_axis',(0.,1.,0.));
#71743=DIRECTION('ref_axis',(-1.,0.,0.));
#71744=DIRECTION('',(-1.,0.,0.));
#71745=DIRECTION('',(-1.,0.,0.));
#71746=DIRECTION('',(0.,0.,1.));
#71747=DIRECTION('center_axis',(0.939692620785909,0.342020143325668,0.));
#71748=DIRECTION('ref_axis',(-0.342020143325668,0.939692620785909,0.));
#71749=DIRECTION('',(-0.342020143325668,0.939692620785909,0.));
#71750=DIRECTION('',(-0.342020143325668,0.939692620785909,0.));
#71751=DIRECTION('',(0.,0.,1.));
#71752=DIRECTION('center_axis',(0.,1.,0.));
#71753=DIRECTION('ref_axis',(-1.,0.,0.));
#71754=DIRECTION('',(-1.,0.,0.));
#71755=DIRECTION('',(-1.,0.,0.));
#71756=DIRECTION('',(0.,0.,1.));
#71757=DIRECTION('center_axis',(-0.939692620785909,0.342020143325668,0.));
#71758=DIRECTION('ref_axis',(-0.342020143325668,-0.939692620785909,0.));
#71759=DIRECTION('',(-0.342020143325668,-0.939692620785909,0.));
#71760=DIRECTION('',(-0.342020143325668,-0.939692620785909,0.));
#71761=DIRECTION('',(0.,0.,1.));
#71762=DIRECTION('center_axis',(0.,1.,0.));
#71763=DIRECTION('ref_axis',(-1.,0.,0.));
#71764=DIRECTION('',(-1.,0.,0.));
#71765=DIRECTION('',(-1.,0.,0.));
#71766=DIRECTION('',(0.,0.,1.));
#71767=DIRECTION('center_axis',(0.939692620785909,0.342020143325668,0.));
#71768=DIRECTION('ref_axis',(-0.342020143325668,0.939692620785909,0.));
#71769=DIRECTION('',(-0.342020143325668,0.939692620785909,0.));
#71770=DIRECTION('',(-0.342020143325668,0.939692620785909,0.));
#71771=DIRECTION('',(0.,0.,1.));
#71772=DIRECTION('center_axis',(0.,1.,0.));
#71773=DIRECTION('ref_axis',(-1.,0.,0.));
#71774=DIRECTION('',(-1.,0.,0.));
#71775=DIRECTION('',(-1.,0.,0.));
#71776=DIRECTION('',(0.,0.,1.));
#71777=DIRECTION('center_axis',(-0.939692620785909,0.342020143325668,0.));
#71778=DIRECTION('ref_axis',(-0.342020143325668,-0.939692620785909,0.));
#71779=DIRECTION('',(-0.342020143325668,-0.939692620785909,0.));
#71780=DIRECTION('',(-0.342020143325668,-0.939692620785909,0.));
#71781=DIRECTION('',(0.,0.,1.));
#71782=DIRECTION('center_axis',(0.,1.,0.));
#71783=DIRECTION('ref_axis',(-1.,0.,0.));
#71784=DIRECTION('',(-1.,0.,0.));
#71785=DIRECTION('',(-1.,0.,0.));
#71786=DIRECTION('',(0.,0.,1.));
#71787=DIRECTION('center_axis',(0.939692620785909,0.342020143325668,0.));
#71788=DIRECTION('ref_axis',(-0.342020143325668,0.939692620785909,0.));
#71789=DIRECTION('',(-0.342020143325668,0.939692620785909,0.));
#71790=DIRECTION('',(-0.342020143325668,0.939692620785909,0.));
#71791=DIRECTION('',(0.,0.,1.));
#71792=DIRECTION('center_axis',(0.,1.,0.));
#71793=DIRECTION('ref_axis',(-1.,0.,0.));
#71794=DIRECTION('',(-1.,0.,0.));
#71795=DIRECTION('',(-1.,0.,0.));
#71796=DIRECTION('',(0.,0.,1.));
#71797=DIRECTION('center_axis',(-0.939692620785909,0.342020143325668,0.));
#71798=DIRECTION('ref_axis',(-0.342020143325668,-0.939692620785909,0.));
#71799=DIRECTION('',(-0.342020143325668,-0.939692620785909,0.));
#71800=DIRECTION('',(-0.342020143325668,-0.939692620785909,0.));
#71801=DIRECTION('',(0.,0.,1.));
#71802=DIRECTION('center_axis',(0.,1.,0.));
#71803=DIRECTION('ref_axis',(-1.,0.,0.));
#71804=DIRECTION('',(-1.,0.,0.));
#71805=DIRECTION('',(-1.,0.,0.));
#71806=DIRECTION('',(0.,0.,1.));
#71807=DIRECTION('center_axis',(0.939692620785909,0.342020143325668,0.));
#71808=DIRECTION('ref_axis',(-0.342020143325668,0.939692620785909,0.));
#71809=DIRECTION('',(-0.342020143325668,0.939692620785909,0.));
#71810=DIRECTION('',(-0.342020143325668,0.939692620785909,0.));
#71811=DIRECTION('',(0.,0.,1.));
#71812=DIRECTION('center_axis',(0.,1.,0.));
#71813=DIRECTION('ref_axis',(-1.,0.,0.));
#71814=DIRECTION('',(-1.,0.,0.));
#71815=DIRECTION('',(-1.,0.,0.));
#71816=DIRECTION('',(0.,0.,1.));
#71817=DIRECTION('center_axis',(-0.939692620785909,0.342020143325668,0.));
#71818=DIRECTION('ref_axis',(-0.342020143325668,-0.939692620785909,0.));
#71819=DIRECTION('',(-0.342020143325668,-0.939692620785909,0.));
#71820=DIRECTION('',(-0.342020143325668,-0.939692620785909,0.));
#71821=DIRECTION('',(0.,0.,1.));
#71822=DIRECTION('center_axis',(0.,1.,0.));
#71823=DIRECTION('ref_axis',(-1.,0.,0.));
#71824=DIRECTION('',(-1.,0.,0.));
#71825=DIRECTION('',(-1.,0.,0.));
#71826=DIRECTION('',(0.,0.,1.));
#71827=DIRECTION('center_axis',(0.939692620785909,0.342020143325668,0.));
#71828=DIRECTION('ref_axis',(-0.342020143325668,0.939692620785909,0.));
#71829=DIRECTION('',(-0.342020143325668,0.939692620785909,0.));
#71830=DIRECTION('',(-0.342020143325668,0.939692620785909,0.));
#71831=DIRECTION('',(0.,0.,1.));
#71832=DIRECTION('center_axis',(0.,1.,0.));
#71833=DIRECTION('ref_axis',(-1.,0.,0.));
#71834=DIRECTION('',(-1.,0.,0.));
#71835=DIRECTION('',(-1.,0.,0.));
#71836=DIRECTION('',(0.,0.,1.));
#71837=DIRECTION('center_axis',(-0.939692620785909,0.342020143325668,0.));
#71838=DIRECTION('ref_axis',(-0.342020143325668,-0.939692620785909,0.));
#71839=DIRECTION('',(-0.342020143325668,-0.939692620785909,0.));
#71840=DIRECTION('',(-0.342020143325668,-0.939692620785909,0.));
#71841=DIRECTION('',(0.,0.,1.));
#71842=DIRECTION('center_axis',(0.,1.,0.));
#71843=DIRECTION('ref_axis',(-1.,0.,0.));
#71844=DIRECTION('',(-1.,0.,0.));
#71845=DIRECTION('',(-1.,0.,0.));
#71846=DIRECTION('',(0.,0.,1.));
#71847=DIRECTION('center_axis',(0.939692620785909,0.342020143325668,0.));
#71848=DIRECTION('ref_axis',(-0.342020143325668,0.939692620785909,0.));
#71849=DIRECTION('',(-0.342020143325668,0.939692620785909,0.));
#71850=DIRECTION('',(-0.342020143325668,0.939692620785909,0.));
#71851=DIRECTION('',(0.,0.,1.));
#71852=DIRECTION('center_axis',(0.,1.,0.));
#71853=DIRECTION('ref_axis',(-1.,0.,0.));
#71854=DIRECTION('',(-1.,0.,0.));
#71855=DIRECTION('',(-1.,0.,0.));
#71856=DIRECTION('',(0.,0.,1.));
#71857=DIRECTION('center_axis',(-0.939692620785909,0.342020143325668,0.));
#71858=DIRECTION('ref_axis',(-0.342020143325668,-0.939692620785909,0.));
#71859=DIRECTION('',(-0.342020143325668,-0.939692620785909,0.));
#71860=DIRECTION('',(-0.342020143325668,-0.939692620785909,0.));
#71861=DIRECTION('',(0.,0.,1.));
#71862=DIRECTION('center_axis',(0.,1.,0.));
#71863=DIRECTION('ref_axis',(-1.,0.,0.));
#71864=DIRECTION('',(-1.,0.,0.));
#71865=DIRECTION('',(-1.,0.,0.));
#71866=DIRECTION('',(0.,0.,1.));
#71867=DIRECTION('center_axis',(0.939692620785909,0.342020143325668,0.));
#71868=DIRECTION('ref_axis',(-0.342020143325668,0.939692620785909,0.));
#71869=DIRECTION('',(-0.342020143325668,0.939692620785909,0.));
#71870=DIRECTION('',(-0.342020143325668,0.939692620785909,0.));
#71871=DIRECTION('',(0.,0.,1.));
#71872=DIRECTION('center_axis',(0.,1.,0.));
#71873=DIRECTION('ref_axis',(-1.,0.,0.));
#71874=DIRECTION('',(-1.,0.,0.));
#71875=DIRECTION('',(-1.,0.,0.));
#71876=DIRECTION('',(0.,0.,1.));
#71877=DIRECTION('center_axis',(-0.939692620785909,0.342020143325668,0.));
#71878=DIRECTION('ref_axis',(-0.342020143325668,-0.939692620785909,0.));
#71879=DIRECTION('',(-0.342020143325668,-0.939692620785909,0.));
#71880=DIRECTION('',(-0.342020143325668,-0.939692620785909,0.));
#71881=DIRECTION('',(0.,0.,1.));
#71882=DIRECTION('center_axis',(0.,1.,0.));
#71883=DIRECTION('ref_axis',(-1.,0.,0.));
#71884=DIRECTION('',(-1.,0.,0.));
#71885=DIRECTION('',(-1.,0.,0.));
#71886=DIRECTION('',(0.,0.,1.));
#71887=DIRECTION('center_axis',(0.939692620785909,0.342020143325668,0.));
#71888=DIRECTION('ref_axis',(-0.342020143325668,0.939692620785909,0.));
#71889=DIRECTION('',(-0.342020143325668,0.939692620785909,0.));
#71890=DIRECTION('',(-0.342020143325668,0.939692620785909,0.));
#71891=DIRECTION('',(0.,0.,1.));
#71892=DIRECTION('center_axis',(0.,1.,0.));
#71893=DIRECTION('ref_axis',(-1.,0.,0.));
#71894=DIRECTION('',(-1.,0.,0.));
#71895=DIRECTION('',(-1.,0.,0.));
#71896=DIRECTION('',(0.,0.,1.));
#71897=DIRECTION('center_axis',(-0.939692620785909,0.342020143325668,0.));
#71898=DIRECTION('ref_axis',(-0.342020143325668,-0.939692620785909,0.));
#71899=DIRECTION('',(-0.342020143325668,-0.939692620785909,0.));
#71900=DIRECTION('',(-0.342020143325668,-0.939692620785909,0.));
#71901=DIRECTION('',(0.,0.,1.));
#71902=DIRECTION('center_axis',(0.,1.,0.));
#71903=DIRECTION('ref_axis',(-1.,0.,0.));
#71904=DIRECTION('',(-1.,0.,0.));
#71905=DIRECTION('',(-1.,0.,0.));
#71906=DIRECTION('',(0.,0.,1.));
#71907=DIRECTION('center_axis',(0.939692620785909,0.342020143325668,0.));
#71908=DIRECTION('ref_axis',(-0.342020143325668,0.939692620785909,0.));
#71909=DIRECTION('',(-0.342020143325668,0.939692620785909,0.));
#71910=DIRECTION('',(-0.342020143325668,0.939692620785909,0.));
#71911=DIRECTION('',(0.,0.,1.));
#71912=DIRECTION('center_axis',(0.,1.,0.));
#71913=DIRECTION('ref_axis',(-1.,0.,0.));
#71914=DIRECTION('',(-1.,0.,0.));
#71915=DIRECTION('',(-1.,0.,0.));
#71916=DIRECTION('',(0.,0.,1.));
#71917=DIRECTION('center_axis',(-0.939692620785909,0.342020143325668,0.));
#71918=DIRECTION('ref_axis',(-0.342020143325668,-0.939692620785909,0.));
#71919=DIRECTION('',(-0.342020143325668,-0.939692620785909,0.));
#71920=DIRECTION('',(-0.342020143325668,-0.939692620785909,0.));
#71921=DIRECTION('',(0.,0.,1.));
#71922=DIRECTION('center_axis',(0.,1.,0.));
#71923=DIRECTION('ref_axis',(-1.,0.,0.));
#71924=DIRECTION('',(-1.,0.,0.));
#71925=DIRECTION('',(-1.,0.,0.));
#71926=DIRECTION('',(0.,0.,1.));
#71927=DIRECTION('center_axis',(0.939692620785909,0.342020143325668,0.));
#71928=DIRECTION('ref_axis',(-0.342020143325668,0.939692620785909,0.));
#71929=DIRECTION('',(-0.342020143325668,0.939692620785909,0.));
#71930=DIRECTION('',(-0.342020143325668,0.939692620785909,0.));
#71931=DIRECTION('',(0.,0.,1.));
#71932=DIRECTION('center_axis',(0.,1.,0.));
#71933=DIRECTION('ref_axis',(-1.,0.,0.));
#71934=DIRECTION('',(-1.,0.,0.));
#71935=DIRECTION('',(-1.,0.,0.));
#71936=DIRECTION('',(0.,0.,1.));
#71937=DIRECTION('center_axis',(-0.939692620785909,0.342020143325668,0.));
#71938=DIRECTION('ref_axis',(-0.342020143325668,-0.939692620785909,0.));
#71939=DIRECTION('',(-0.342020143325668,-0.939692620785909,0.));
#71940=DIRECTION('',(-0.342020143325668,-0.939692620785909,0.));
#71941=DIRECTION('',(0.,0.,1.));
#71942=DIRECTION('center_axis',(0.,1.,0.));
#71943=DIRECTION('ref_axis',(-1.,0.,0.));
#71944=DIRECTION('',(-1.,0.,0.));
#71945=DIRECTION('',(-1.,0.,0.));
#71946=DIRECTION('',(0.,0.,1.));
#71947=DIRECTION('center_axis',(0.939692620785909,0.342020143325668,0.));
#71948=DIRECTION('ref_axis',(-0.342020143325668,0.939692620785909,0.));
#71949=DIRECTION('',(-0.342020143325668,0.939692620785909,0.));
#71950=DIRECTION('',(-0.342020143325668,0.939692620785909,0.));
#71951=DIRECTION('',(0.,0.,1.));
#71952=DIRECTION('center_axis',(0.,1.,0.));
#71953=DIRECTION('ref_axis',(-1.,0.,0.));
#71954=DIRECTION('',(-1.,0.,0.));
#71955=DIRECTION('',(-1.,0.,0.));
#71956=DIRECTION('',(0.,0.,1.));
#71957=DIRECTION('center_axis',(-0.939692620785909,0.342020143325668,0.));
#71958=DIRECTION('ref_axis',(-0.342020143325668,-0.939692620785909,0.));
#71959=DIRECTION('',(-0.342020143325668,-0.939692620785909,0.));
#71960=DIRECTION('',(-0.342020143325668,-0.939692620785909,0.));
#71961=DIRECTION('',(0.,0.,1.));
#71962=DIRECTION('center_axis',(0.,1.,0.));
#71963=DIRECTION('ref_axis',(-1.,0.,0.));
#71964=DIRECTION('',(-1.,0.,0.));
#71965=DIRECTION('',(-1.,0.,0.));
#71966=DIRECTION('',(0.,0.,1.));
#71967=DIRECTION('center_axis',(0.939692620785909,0.342020143325668,0.));
#71968=DIRECTION('ref_axis',(-0.342020143325668,0.939692620785909,0.));
#71969=DIRECTION('',(-0.342020143325668,0.939692620785909,0.));
#71970=DIRECTION('',(-0.342020143325668,0.939692620785909,0.));
#71971=DIRECTION('',(0.,0.,1.));
#71972=DIRECTION('center_axis',(0.,1.,0.));
#71973=DIRECTION('ref_axis',(-1.,0.,0.));
#71974=DIRECTION('',(-1.,0.,0.));
#71975=DIRECTION('',(-1.,0.,0.));
#71976=DIRECTION('',(0.,0.,1.));
#71977=DIRECTION('center_axis',(-0.939692620785909,0.342020143325668,0.));
#71978=DIRECTION('ref_axis',(-0.342020143325668,-0.939692620785909,0.));
#71979=DIRECTION('',(-0.342020143325668,-0.939692620785909,0.));
#71980=DIRECTION('',(-0.342020143325668,-0.939692620785909,0.));
#71981=DIRECTION('',(0.,0.,1.));
#71982=DIRECTION('center_axis',(0.,1.,0.));
#71983=DIRECTION('ref_axis',(-1.,0.,0.));
#71984=DIRECTION('',(-1.,0.,0.));
#71985=DIRECTION('',(-1.,0.,0.));
#71986=DIRECTION('',(0.,0.,1.));
#71987=DIRECTION('center_axis',(0.939692620785909,0.342020143325668,0.));
#71988=DIRECTION('ref_axis',(-0.342020143325668,0.939692620785909,0.));
#71989=DIRECTION('',(-0.342020143325668,0.939692620785909,0.));
#71990=DIRECTION('',(-0.342020143325668,0.939692620785909,0.));
#71991=DIRECTION('',(0.,0.,1.));
#71992=DIRECTION('center_axis',(0.,1.,0.));
#71993=DIRECTION('ref_axis',(-1.,0.,0.));
#71994=DIRECTION('',(-1.,0.,0.));
#71995=DIRECTION('',(-1.,0.,0.));
#71996=DIRECTION('',(0.,0.,1.));
#71997=DIRECTION('center_axis',(-0.939692620785909,0.342020143325668,0.));
#71998=DIRECTION('ref_axis',(-0.342020143325668,-0.939692620785909,0.));
#71999=DIRECTION('',(-0.342020143325668,-0.939692620785909,0.));
#72000=DIRECTION('',(-0.342020143325668,-0.939692620785909,0.));
#72001=DIRECTION('',(0.,0.,1.));
#72002=DIRECTION('center_axis',(0.,1.,0.));
#72003=DIRECTION('ref_axis',(-1.,0.,0.));
#72004=DIRECTION('',(-1.,0.,0.));
#72005=DIRECTION('',(-1.,0.,0.));
#72006=DIRECTION('',(0.,0.,1.));
#72007=DIRECTION('center_axis',(0.939692620785909,0.342020143325668,0.));
#72008=DIRECTION('ref_axis',(-0.342020143325668,0.939692620785909,0.));
#72009=DIRECTION('',(-0.342020143325668,0.939692620785909,0.));
#72010=DIRECTION('',(-0.342020143325668,0.939692620785909,0.));
#72011=DIRECTION('',(0.,0.,1.));
#72012=DIRECTION('center_axis',(0.,1.,0.));
#72013=DIRECTION('ref_axis',(-1.,0.,0.));
#72014=DIRECTION('',(-1.,0.,0.));
#72015=DIRECTION('',(-1.,0.,0.));
#72016=DIRECTION('',(0.,0.,1.));
#72017=DIRECTION('center_axis',(-0.939692620785909,0.342020143325668,0.));
#72018=DIRECTION('ref_axis',(-0.342020143325668,-0.939692620785909,0.));
#72019=DIRECTION('',(-0.342020143325668,-0.939692620785909,0.));
#72020=DIRECTION('',(-0.342020143325668,-0.939692620785909,0.));
#72021=DIRECTION('',(0.,0.,1.));
#72022=DIRECTION('center_axis',(0.,1.,0.));
#72023=DIRECTION('ref_axis',(-1.,0.,0.));
#72024=DIRECTION('',(-1.,0.,0.));
#72025=DIRECTION('',(-1.,0.,0.));
#72026=DIRECTION('',(0.,0.,1.));
#72027=DIRECTION('center_axis',(0.939692620785909,0.342020143325668,0.));
#72028=DIRECTION('ref_axis',(-0.342020143325668,0.939692620785909,0.));
#72029=DIRECTION('',(-0.342020143325668,0.939692620785909,0.));
#72030=DIRECTION('',(-0.342020143325668,0.939692620785909,0.));
#72031=DIRECTION('',(0.,0.,1.));
#72032=DIRECTION('center_axis',(0.,1.,0.));
#72033=DIRECTION('ref_axis',(-1.,0.,0.));
#72034=DIRECTION('',(-1.,0.,0.));
#72035=DIRECTION('',(-1.,0.,0.));
#72036=DIRECTION('',(0.,0.,1.));
#72037=DIRECTION('center_axis',(-0.939692620785909,0.342020143325668,0.));
#72038=DIRECTION('ref_axis',(-0.342020143325668,-0.939692620785909,0.));
#72039=DIRECTION('',(-0.342020143325668,-0.939692620785909,0.));
#72040=DIRECTION('',(-0.342020143325668,-0.939692620785909,0.));
#72041=DIRECTION('',(0.,0.,1.));
#72042=DIRECTION('center_axis',(0.,1.,0.));
#72043=DIRECTION('ref_axis',(-1.,0.,0.));
#72044=DIRECTION('',(-1.,0.,0.));
#72045=DIRECTION('',(-1.,0.,0.));
#72046=DIRECTION('',(0.,0.,1.));
#72047=DIRECTION('center_axis',(0.939692620785909,0.342020143325668,0.));
#72048=DIRECTION('ref_axis',(-0.342020143325668,0.939692620785909,0.));
#72049=DIRECTION('',(-0.342020143325668,0.939692620785909,0.));
#72050=DIRECTION('',(-0.342020143325668,0.939692620785909,0.));
#72051=DIRECTION('',(0.,0.,1.));
#72052=DIRECTION('center_axis',(0.,1.,0.));
#72053=DIRECTION('ref_axis',(-1.,0.,0.));
#72054=DIRECTION('',(-1.,0.,0.));
#72055=DIRECTION('',(-1.,0.,0.));
#72056=DIRECTION('',(0.,0.,1.));
#72057=DIRECTION('center_axis',(-0.939692620785909,0.342020143325668,0.));
#72058=DIRECTION('ref_axis',(-0.342020143325668,-0.939692620785909,0.));
#72059=DIRECTION('',(-0.342020143325668,-0.939692620785909,0.));
#72060=DIRECTION('',(-0.342020143325668,-0.939692620785909,0.));
#72061=DIRECTION('',(0.,0.,1.));
#72062=DIRECTION('center_axis',(0.,1.,0.));
#72063=DIRECTION('ref_axis',(-1.,0.,0.));
#72064=DIRECTION('',(-1.,0.,0.));
#72065=DIRECTION('',(-1.,0.,0.));
#72066=DIRECTION('',(0.,0.,1.));
#72067=DIRECTION('center_axis',(0.939692620785909,0.342020143325668,0.));
#72068=DIRECTION('ref_axis',(-0.342020143325668,0.939692620785909,0.));
#72069=DIRECTION('',(-0.342020143325668,0.939692620785909,0.));
#72070=DIRECTION('',(-0.342020143325668,0.939692620785909,0.));
#72071=DIRECTION('',(0.,0.,1.));
#72072=DIRECTION('center_axis',(0.,1.,0.));
#72073=DIRECTION('ref_axis',(-1.,0.,0.));
#72074=DIRECTION('',(-1.,0.,0.));
#72075=DIRECTION('',(-1.,0.,0.));
#72076=DIRECTION('',(0.,0.,1.));
#72077=DIRECTION('center_axis',(-0.939692620785909,0.342020143325668,0.));
#72078=DIRECTION('ref_axis',(-0.342020143325668,-0.939692620785909,0.));
#72079=DIRECTION('',(-0.342020143325668,-0.939692620785909,0.));
#72080=DIRECTION('',(-0.342020143325668,-0.939692620785909,0.));
#72081=DIRECTION('',(0.,0.,1.));
#72082=DIRECTION('center_axis',(0.,1.,0.));
#72083=DIRECTION('ref_axis',(-1.,0.,0.));
#72084=DIRECTION('',(-1.,0.,0.));
#72085=DIRECTION('',(-1.,0.,0.));
#72086=DIRECTION('',(0.,0.,1.));
#72087=DIRECTION('center_axis',(0.939692620785909,0.342020143325668,0.));
#72088=DIRECTION('ref_axis',(-0.342020143325668,0.939692620785909,0.));
#72089=DIRECTION('',(-0.342020143325668,0.939692620785909,0.));
#72090=DIRECTION('',(-0.342020143325668,0.939692620785909,0.));
#72091=DIRECTION('',(0.,0.,1.));
#72092=DIRECTION('center_axis',(0.,1.,0.));
#72093=DIRECTION('ref_axis',(-1.,0.,0.));
#72094=DIRECTION('',(-1.,0.,0.));
#72095=DIRECTION('',(-1.,0.,0.));
#72096=DIRECTION('',(0.,0.,1.));
#72097=DIRECTION('center_axis',(-0.939692620785909,0.342020143325668,0.));
#72098=DIRECTION('ref_axis',(-0.342020143325668,-0.939692620785909,0.));
#72099=DIRECTION('',(-0.342020143325668,-0.939692620785909,0.));
#72100=DIRECTION('',(-0.342020143325668,-0.939692620785909,0.));
#72101=DIRECTION('',(0.,0.,1.));
#72102=DIRECTION('center_axis',(0.,1.,0.));
#72103=DIRECTION('ref_axis',(-1.,0.,0.));
#72104=DIRECTION('',(-1.,0.,0.));
#72105=DIRECTION('',(-1.,0.,0.));
#72106=DIRECTION('',(0.,0.,1.));
#72107=DIRECTION('center_axis',(0.939692620785909,0.342020143325668,0.));
#72108=DIRECTION('ref_axis',(-0.342020143325668,0.939692620785909,0.));
#72109=DIRECTION('',(-0.342020143325668,0.939692620785909,0.));
#72110=DIRECTION('',(-0.342020143325668,0.939692620785909,0.));
#72111=DIRECTION('',(0.,0.,1.));
#72112=DIRECTION('center_axis',(0.,1.,0.));
#72113=DIRECTION('ref_axis',(-1.,0.,0.));
#72114=DIRECTION('',(-1.,0.,0.));
#72115=DIRECTION('',(-1.,0.,0.));
#72116=DIRECTION('',(0.,0.,1.));
#72117=DIRECTION('center_axis',(-0.939692620785909,0.342020143325668,0.));
#72118=DIRECTION('ref_axis',(-0.342020143325668,-0.939692620785909,0.));
#72119=DIRECTION('',(-0.342020143325668,-0.939692620785909,0.));
#72120=DIRECTION('',(-0.342020143325668,-0.939692620785909,0.));
#72121=DIRECTION('',(0.,0.,1.));
#72122=DIRECTION('center_axis',(0.,1.,0.));
#72123=DIRECTION('ref_axis',(-1.,0.,0.));
#72124=DIRECTION('',(-1.,0.,0.));
#72125=DIRECTION('',(-1.,0.,0.));
#72126=DIRECTION('',(0.,0.,1.));
#72127=DIRECTION('center_axis',(0.939692620785909,0.342020143325668,0.));
#72128=DIRECTION('ref_axis',(-0.342020143325668,0.939692620785909,0.));
#72129=DIRECTION('',(-0.342020143325668,0.939692620785909,0.));
#72130=DIRECTION('',(-0.342020143325668,0.939692620785909,0.));
#72131=DIRECTION('',(0.,0.,1.));
#72132=DIRECTION('center_axis',(0.,1.,0.));
#72133=DIRECTION('ref_axis',(-1.,0.,0.));
#72134=DIRECTION('',(-1.,0.,0.));
#72135=DIRECTION('',(-1.,0.,0.));
#72136=DIRECTION('',(0.,0.,1.));
#72137=DIRECTION('center_axis',(-0.939692620785909,0.342020143325668,0.));
#72138=DIRECTION('ref_axis',(-0.342020143325668,-0.939692620785909,0.));
#72139=DIRECTION('',(-0.342020143325668,-0.939692620785909,0.));
#72140=DIRECTION('',(-0.342020143325668,-0.939692620785909,0.));
#72141=DIRECTION('',(0.,0.,1.));
#72142=DIRECTION('center_axis',(0.,1.,0.));
#72143=DIRECTION('ref_axis',(-1.,0.,0.));
#72144=DIRECTION('',(-1.,0.,0.));
#72145=DIRECTION('',(-1.,0.,0.));
#72146=DIRECTION('',(0.,0.,1.));
#72147=DIRECTION('center_axis',(0.939692620785909,0.342020143325668,0.));
#72148=DIRECTION('ref_axis',(-0.342020143325668,0.939692620785909,0.));
#72149=DIRECTION('',(-0.342020143325668,0.939692620785909,0.));
#72150=DIRECTION('',(-0.342020143325668,0.939692620785909,0.));
#72151=DIRECTION('',(0.,0.,1.));
#72152=DIRECTION('center_axis',(0.,1.,0.));
#72153=DIRECTION('ref_axis',(-1.,0.,0.));
#72154=DIRECTION('',(-1.,0.,0.));
#72155=DIRECTION('',(-1.,0.,0.));
#72156=DIRECTION('',(0.,0.,1.));
#72157=DIRECTION('center_axis',(-0.939692620785909,0.342020143325668,0.));
#72158=DIRECTION('ref_axis',(-0.342020143325668,-0.939692620785909,0.));
#72159=DIRECTION('',(-0.342020143325668,-0.939692620785909,0.));
#72160=DIRECTION('',(-0.342020143325668,-0.939692620785909,0.));
#72161=DIRECTION('',(0.,0.,1.));
#72162=DIRECTION('center_axis',(0.,1.,0.));
#72163=DIRECTION('ref_axis',(-1.,0.,0.));
#72164=DIRECTION('',(-1.,0.,0.));
#72165=DIRECTION('',(-1.,0.,0.));
#72166=DIRECTION('',(0.,0.,1.));
#72167=DIRECTION('center_axis',(0.939692620785909,0.342020143325668,0.));
#72168=DIRECTION('ref_axis',(-0.342020143325668,0.939692620785909,0.));
#72169=DIRECTION('',(-0.342020143325668,0.939692620785909,0.));
#72170=DIRECTION('',(-0.342020143325668,0.939692620785909,0.));
#72171=DIRECTION('',(0.,0.,1.));
#72172=DIRECTION('center_axis',(0.,1.,0.));
#72173=DIRECTION('ref_axis',(-1.,0.,0.));
#72174=DIRECTION('',(-1.,0.,0.));
#72175=DIRECTION('',(-1.,0.,0.));
#72176=DIRECTION('',(0.,0.,1.));
#72177=DIRECTION('center_axis',(-0.939692620785909,0.342020143325668,0.));
#72178=DIRECTION('ref_axis',(-0.342020143325668,-0.939692620785909,0.));
#72179=DIRECTION('',(-0.342020143325668,-0.939692620785909,0.));
#72180=DIRECTION('',(-0.342020143325668,-0.939692620785909,0.));
#72181=DIRECTION('',(0.,0.,1.));
#72182=DIRECTION('center_axis',(0.,1.,0.));
#72183=DIRECTION('ref_axis',(-1.,0.,0.));
#72184=DIRECTION('',(-1.,0.,0.));
#72185=DIRECTION('',(-1.,0.,0.));
#72186=DIRECTION('',(0.,0.,1.));
#72187=DIRECTION('center_axis',(0.939692620785909,0.342020143325668,0.));
#72188=DIRECTION('ref_axis',(-0.342020143325668,0.939692620785909,0.));
#72189=DIRECTION('',(-0.342020143325668,0.939692620785909,0.));
#72190=DIRECTION('',(-0.342020143325668,0.939692620785909,0.));
#72191=DIRECTION('',(0.,0.,1.));
#72192=DIRECTION('center_axis',(0.,1.,0.));
#72193=DIRECTION('ref_axis',(-1.,0.,0.));
#72194=DIRECTION('',(-1.,0.,0.));
#72195=DIRECTION('',(-1.,0.,0.));
#72196=DIRECTION('',(0.,0.,1.));
#72197=DIRECTION('center_axis',(-0.939692620785909,0.342020143325668,0.));
#72198=DIRECTION('ref_axis',(-0.342020143325668,-0.939692620785909,0.));
#72199=DIRECTION('',(-0.342020143325668,-0.939692620785909,0.));
#72200=DIRECTION('',(-0.342020143325668,-0.939692620785909,0.));
#72201=DIRECTION('',(0.,0.,1.));
#72202=DIRECTION('center_axis',(0.,1.,0.));
#72203=DIRECTION('ref_axis',(-1.,0.,0.));
#72204=DIRECTION('',(-1.,0.,0.));
#72205=DIRECTION('',(-1.,0.,0.));
#72206=DIRECTION('',(0.,0.,1.));
#72207=DIRECTION('center_axis',(0.939692620785909,0.342020143325668,0.));
#72208=DIRECTION('ref_axis',(-0.342020143325668,0.939692620785909,0.));
#72209=DIRECTION('',(-0.342020143325668,0.939692620785909,0.));
#72210=DIRECTION('',(-0.342020143325668,0.939692620785909,0.));
#72211=DIRECTION('',(0.,0.,1.));
#72212=DIRECTION('center_axis',(0.,1.,0.));
#72213=DIRECTION('ref_axis',(-1.,0.,0.));
#72214=DIRECTION('',(-1.,0.,0.));
#72215=DIRECTION('',(-1.,0.,0.));
#72216=DIRECTION('',(0.,0.,1.));
#72217=DIRECTION('center_axis',(-0.939692620785909,0.342020143325668,0.));
#72218=DIRECTION('ref_axis',(-0.342020143325668,-0.939692620785909,0.));
#72219=DIRECTION('',(-0.342020143325668,-0.939692620785909,0.));
#72220=DIRECTION('',(-0.342020143325668,-0.939692620785909,0.));
#72221=DIRECTION('',(0.,0.,1.));
#72222=DIRECTION('center_axis',(0.,1.,0.));
#72223=DIRECTION('ref_axis',(-1.,0.,0.));
#72224=DIRECTION('',(-1.,0.,0.));
#72225=DIRECTION('',(-1.,0.,0.));
#72226=DIRECTION('',(0.,0.,1.));
#72227=DIRECTION('center_axis',(0.939692620785909,0.342020143325668,0.));
#72228=DIRECTION('ref_axis',(-0.342020143325668,0.939692620785909,0.));
#72229=DIRECTION('',(-0.342020143325668,0.939692620785909,0.));
#72230=DIRECTION('',(-0.342020143325668,0.939692620785909,0.));
#72231=DIRECTION('',(0.,0.,1.));
#72232=DIRECTION('center_axis',(0.,1.,0.));
#72233=DIRECTION('ref_axis',(-1.,0.,0.));
#72234=DIRECTION('',(-1.,0.,0.));
#72235=DIRECTION('',(-1.,0.,0.));
#72236=DIRECTION('',(0.,0.,1.));
#72237=DIRECTION('center_axis',(-0.939692620785909,0.342020143325668,0.));
#72238=DIRECTION('ref_axis',(-0.342020143325668,-0.939692620785909,0.));
#72239=DIRECTION('',(-0.342020143325668,-0.939692620785909,0.));
#72240=DIRECTION('',(-0.342020143325668,-0.939692620785909,0.));
#72241=DIRECTION('',(0.,0.,1.));
#72242=DIRECTION('center_axis',(0.,1.,0.));
#72243=DIRECTION('ref_axis',(-1.,0.,0.));
#72244=DIRECTION('',(-1.,0.,0.));
#72245=DIRECTION('',(-1.,0.,0.));
#72246=DIRECTION('',(0.,0.,1.));
#72247=DIRECTION('center_axis',(0.939692620785909,0.342020143325668,0.));
#72248=DIRECTION('ref_axis',(-0.342020143325668,0.939692620785909,0.));
#72249=DIRECTION('',(-0.342020143325668,0.939692620785909,0.));
#72250=DIRECTION('',(-0.342020143325668,0.939692620785909,0.));
#72251=DIRECTION('',(0.,0.,1.));
#72252=DIRECTION('center_axis',(0.,1.,0.));
#72253=DIRECTION('ref_axis',(-1.,0.,0.));
#72254=DIRECTION('',(-1.,0.,0.));
#72255=DIRECTION('',(-1.,0.,0.));
#72256=DIRECTION('',(0.,0.,1.));
#72257=DIRECTION('center_axis',(-0.939692620785909,0.342020143325668,0.));
#72258=DIRECTION('ref_axis',(-0.342020143325668,-0.939692620785909,0.));
#72259=DIRECTION('',(-0.342020143325668,-0.939692620785909,0.));
#72260=DIRECTION('',(-0.342020143325668,-0.939692620785909,0.));
#72261=DIRECTION('',(0.,0.,1.));
#72262=DIRECTION('center_axis',(0.,1.,0.));
#72263=DIRECTION('ref_axis',(-1.,0.,0.));
#72264=DIRECTION('',(-1.,0.,0.));
#72265=DIRECTION('',(-1.,0.,0.));
#72266=DIRECTION('',(0.,0.,1.));
#72267=DIRECTION('center_axis',(0.939692620785909,0.342020143325668,0.));
#72268=DIRECTION('ref_axis',(-0.342020143325668,0.939692620785909,0.));
#72269=DIRECTION('',(-0.342020143325668,0.939692620785909,0.));
#72270=DIRECTION('',(-0.342020143325668,0.939692620785909,0.));
#72271=DIRECTION('',(0.,0.,1.));
#72272=DIRECTION('center_axis',(0.,1.,0.));
#72273=DIRECTION('ref_axis',(-1.,0.,0.));
#72274=DIRECTION('',(-1.,0.,0.));
#72275=DIRECTION('',(-1.,0.,0.));
#72276=DIRECTION('',(0.,0.,1.));
#72277=DIRECTION('center_axis',(-0.939692620785909,0.342020143325668,0.));
#72278=DIRECTION('ref_axis',(-0.342020143325668,-0.939692620785909,0.));
#72279=DIRECTION('',(-0.342020143325668,-0.939692620785909,0.));
#72280=DIRECTION('',(-0.342020143325668,-0.939692620785909,0.));
#72281=DIRECTION('',(0.,0.,1.));
#72282=DIRECTION('center_axis',(0.,1.,0.));
#72283=DIRECTION('ref_axis',(-1.,0.,0.));
#72284=DIRECTION('',(-1.,0.,0.));
#72285=DIRECTION('',(-1.,0.,0.));
#72286=DIRECTION('',(0.,0.,1.));
#72287=DIRECTION('center_axis',(0.939692620785909,0.342020143325668,0.));
#72288=DIRECTION('ref_axis',(-0.342020143325668,0.939692620785909,0.));
#72289=DIRECTION('',(-0.342020143325668,0.939692620785909,0.));
#72290=DIRECTION('',(-0.342020143325668,0.939692620785909,0.));
#72291=DIRECTION('',(0.,0.,1.));
#72292=DIRECTION('center_axis',(0.,1.,0.));
#72293=DIRECTION('ref_axis',(-1.,0.,0.));
#72294=DIRECTION('',(-1.,0.,0.));
#72295=DIRECTION('',(-1.,0.,0.));
#72296=DIRECTION('',(0.,0.,1.));
#72297=DIRECTION('center_axis',(-0.939692620785909,0.342020143325668,0.));
#72298=DIRECTION('ref_axis',(-0.342020143325668,-0.939692620785909,0.));
#72299=DIRECTION('',(-0.342020143325668,-0.939692620785909,0.));
#72300=DIRECTION('',(-0.342020143325668,-0.939692620785909,0.));
#72301=DIRECTION('',(0.,0.,1.));
#72302=DIRECTION('center_axis',(0.,1.,0.));
#72303=DIRECTION('ref_axis',(-1.,0.,0.));
#72304=DIRECTION('',(-1.,0.,0.));
#72305=DIRECTION('',(-1.,0.,0.));
#72306=DIRECTION('',(0.,0.,1.));
#72307=DIRECTION('center_axis',(0.939692620785909,0.342020143325668,0.));
#72308=DIRECTION('ref_axis',(-0.342020143325668,0.939692620785909,0.));
#72309=DIRECTION('',(-0.342020143325668,0.939692620785909,0.));
#72310=DIRECTION('',(-0.342020143325668,0.939692620785909,0.));
#72311=DIRECTION('',(0.,0.,1.));
#72312=DIRECTION('center_axis',(0.,1.,0.));
#72313=DIRECTION('ref_axis',(-1.,0.,0.));
#72314=DIRECTION('',(-1.,0.,0.));
#72315=DIRECTION('',(-1.,0.,0.));
#72316=DIRECTION('',(0.,0.,1.));
#72317=DIRECTION('center_axis',(-0.939692620785909,0.342020143325668,0.));
#72318=DIRECTION('ref_axis',(-0.342020143325668,-0.939692620785909,0.));
#72319=DIRECTION('',(-0.342020143325668,-0.939692620785909,0.));
#72320=DIRECTION('',(-0.342020143325668,-0.939692620785909,0.));
#72321=DIRECTION('',(0.,0.,1.));
#72322=DIRECTION('center_axis',(0.,1.,0.));
#72323=DIRECTION('ref_axis',(-1.,0.,0.));
#72324=DIRECTION('',(-1.,0.,0.));
#72325=DIRECTION('',(-1.,0.,0.));
#72326=DIRECTION('',(0.,0.,1.));
#72327=DIRECTION('center_axis',(0.939692620785909,0.342020143325668,0.));
#72328=DIRECTION('ref_axis',(-0.342020143325668,0.939692620785909,0.));
#72329=DIRECTION('',(-0.342020143325668,0.939692620785909,0.));
#72330=DIRECTION('',(-0.342020143325668,0.939692620785909,0.));
#72331=DIRECTION('',(0.,0.,1.));
#72332=DIRECTION('center_axis',(0.,1.,0.));
#72333=DIRECTION('ref_axis',(-1.,0.,0.));
#72334=DIRECTION('',(-1.,0.,0.));
#72335=DIRECTION('',(-1.,0.,0.));
#72336=DIRECTION('',(0.,0.,1.));
#72337=DIRECTION('center_axis',(-0.939692620785909,0.342020143325668,0.));
#72338=DIRECTION('ref_axis',(-0.342020143325668,-0.939692620785909,0.));
#72339=DIRECTION('',(-0.342020143325668,-0.939692620785909,0.));
#72340=DIRECTION('',(-0.342020143325668,-0.939692620785909,0.));
#72341=DIRECTION('',(0.,0.,1.));
#72342=DIRECTION('center_axis',(0.,1.,0.));
#72343=DIRECTION('ref_axis',(-1.,0.,0.));
#72344=DIRECTION('',(-1.,0.,0.));
#72345=DIRECTION('',(-1.,0.,0.));
#72346=DIRECTION('',(0.,0.,1.));
#72347=DIRECTION('center_axis',(0.939692620785909,0.342020143325668,0.));
#72348=DIRECTION('ref_axis',(-0.342020143325668,0.939692620785909,0.));
#72349=DIRECTION('',(-0.342020143325668,0.939692620785909,0.));
#72350=DIRECTION('',(-0.342020143325668,0.939692620785909,0.));
#72351=DIRECTION('',(0.,0.,1.));
#72352=DIRECTION('center_axis',(0.,1.,0.));
#72353=DIRECTION('ref_axis',(-1.,0.,0.));
#72354=DIRECTION('',(-1.,0.,0.));
#72355=DIRECTION('',(-1.,0.,0.));
#72356=DIRECTION('',(0.,0.,1.));
#72357=DIRECTION('center_axis',(-0.939692620785909,0.342020143325668,0.));
#72358=DIRECTION('ref_axis',(-0.342020143325668,-0.939692620785909,0.));
#72359=DIRECTION('',(-0.342020143325668,-0.939692620785909,0.));
#72360=DIRECTION('',(-0.342020143325668,-0.939692620785909,0.));
#72361=DIRECTION('',(0.,0.,1.));
#72362=DIRECTION('center_axis',(0.,1.,0.));
#72363=DIRECTION('ref_axis',(-1.,0.,0.));
#72364=DIRECTION('',(-1.,0.,0.));
#72365=DIRECTION('',(-1.,0.,0.));
#72366=DIRECTION('',(0.,0.,1.));
#72367=DIRECTION('center_axis',(0.939692620785909,0.342020143325668,0.));
#72368=DIRECTION('ref_axis',(-0.342020143325668,0.939692620785909,0.));
#72369=DIRECTION('',(-0.342020143325668,0.939692620785909,0.));
#72370=DIRECTION('',(-0.342020143325668,0.939692620785909,0.));
#72371=DIRECTION('',(0.,0.,1.));
#72372=DIRECTION('center_axis',(0.,1.,0.));
#72373=DIRECTION('ref_axis',(-1.,0.,0.));
#72374=DIRECTION('',(-1.,0.,0.));
#72375=DIRECTION('',(-1.,0.,0.));
#72376=DIRECTION('',(0.,0.,1.));
#72377=DIRECTION('center_axis',(-0.939692620785909,0.342020143325668,0.));
#72378=DIRECTION('ref_axis',(-0.342020143325668,-0.939692620785909,0.));
#72379=DIRECTION('',(-0.342020143325668,-0.939692620785909,0.));
#72380=DIRECTION('',(-0.342020143325668,-0.939692620785909,0.));
#72381=DIRECTION('',(0.,0.,1.));
#72382=DIRECTION('center_axis',(0.,1.,0.));
#72383=DIRECTION('ref_axis',(-1.,0.,0.));
#72384=DIRECTION('',(-1.,0.,0.));
#72385=DIRECTION('',(-1.,0.,0.));
#72386=DIRECTION('',(0.,0.,1.));
#72387=DIRECTION('center_axis',(0.939692620785909,0.342020143325668,0.));
#72388=DIRECTION('ref_axis',(-0.342020143325668,0.939692620785909,0.));
#72389=DIRECTION('',(-0.342020143325668,0.939692620785909,0.));
#72390=DIRECTION('',(-0.342020143325668,0.939692620785909,0.));
#72391=DIRECTION('',(0.,0.,1.));
#72392=DIRECTION('center_axis',(0.,1.,0.));
#72393=DIRECTION('ref_axis',(-1.,0.,0.));
#72394=DIRECTION('',(-1.,0.,0.));
#72395=DIRECTION('',(-1.,0.,0.));
#72396=DIRECTION('',(0.,0.,1.));
#72397=DIRECTION('center_axis',(-0.939692620785909,0.342020143325668,0.));
#72398=DIRECTION('ref_axis',(-0.342020143325668,-0.939692620785909,0.));
#72399=DIRECTION('',(-0.342020143325668,-0.939692620785909,0.));
#72400=DIRECTION('',(-0.342020143325668,-0.939692620785909,0.));
#72401=DIRECTION('',(0.,0.,1.));
#72402=DIRECTION('center_axis',(0.,1.,0.));
#72403=DIRECTION('ref_axis',(-1.,0.,0.));
#72404=DIRECTION('',(-1.,0.,0.));
#72405=DIRECTION('',(-1.,0.,0.));
#72406=DIRECTION('',(0.,0.,1.));
#72407=DIRECTION('center_axis',(0.939692620785909,0.342020143325668,0.));
#72408=DIRECTION('ref_axis',(-0.342020143325668,0.939692620785909,0.));
#72409=DIRECTION('',(-0.342020143325668,0.939692620785909,0.));
#72410=DIRECTION('',(-0.342020143325668,0.939692620785909,0.));
#72411=DIRECTION('',(0.,0.,1.));
#72412=DIRECTION('center_axis',(0.,1.,0.));
#72413=DIRECTION('ref_axis',(-1.,0.,0.));
#72414=DIRECTION('',(-1.,0.,0.));
#72415=DIRECTION('',(-1.,0.,0.));
#72416=DIRECTION('',(0.,0.,1.));
#72417=DIRECTION('center_axis',(-0.939692620785909,0.342020143325668,0.));
#72418=DIRECTION('ref_axis',(-0.342020143325668,-0.939692620785909,0.));
#72419=DIRECTION('',(-0.342020143325668,-0.939692620785909,0.));
#72420=DIRECTION('',(-0.342020143325668,-0.939692620785909,0.));
#72421=DIRECTION('',(0.,0.,1.));
#72422=DIRECTION('center_axis',(0.,1.,0.));
#72423=DIRECTION('ref_axis',(-1.,0.,0.));
#72424=DIRECTION('',(-1.,0.,0.));
#72425=DIRECTION('',(-1.,0.,0.));
#72426=DIRECTION('',(0.,0.,1.));
#72427=DIRECTION('center_axis',(0.939692620785909,0.342020143325668,0.));
#72428=DIRECTION('ref_axis',(-0.342020143325668,0.939692620785909,0.));
#72429=DIRECTION('',(-0.342020143325668,0.939692620785909,0.));
#72430=DIRECTION('',(-0.342020143325668,0.939692620785909,0.));
#72431=DIRECTION('',(0.,0.,1.));
#72432=DIRECTION('center_axis',(0.,1.,0.));
#72433=DIRECTION('ref_axis',(-1.,0.,0.));
#72434=DIRECTION('',(-1.,0.,0.));
#72435=DIRECTION('',(-1.,0.,0.));
#72436=DIRECTION('',(0.,0.,1.));
#72437=DIRECTION('center_axis',(-0.939692620785909,0.342020143325668,0.));
#72438=DIRECTION('ref_axis',(-0.342020143325668,-0.939692620785909,0.));
#72439=DIRECTION('',(-0.342020143325668,-0.939692620785909,0.));
#72440=DIRECTION('',(-0.342020143325668,-0.939692620785909,0.));
#72441=DIRECTION('',(0.,0.,1.));
#72442=DIRECTION('center_axis',(0.,1.,0.));
#72443=DIRECTION('ref_axis',(-1.,0.,0.));
#72444=DIRECTION('',(-1.,0.,0.));
#72445=DIRECTION('',(-1.,0.,0.));
#72446=DIRECTION('',(0.,0.,1.));
#72447=DIRECTION('center_axis',(0.939692620785909,0.342020143325668,0.));
#72448=DIRECTION('ref_axis',(-0.342020143325668,0.939692620785909,0.));
#72449=DIRECTION('',(-0.342020143325668,0.939692620785909,0.));
#72450=DIRECTION('',(-0.342020143325668,0.939692620785909,0.));
#72451=DIRECTION('',(0.,0.,1.));
#72452=DIRECTION('center_axis',(0.,1.,0.));
#72453=DIRECTION('ref_axis',(-1.,0.,0.));
#72454=DIRECTION('',(-1.,0.,0.));
#72455=DIRECTION('',(-1.,0.,0.));
#72456=DIRECTION('',(0.,0.,1.));
#72457=DIRECTION('center_axis',(-0.939692620785909,0.342020143325668,0.));
#72458=DIRECTION('ref_axis',(-0.342020143325668,-0.939692620785909,0.));
#72459=DIRECTION('',(-0.342020143325668,-0.939692620785909,0.));
#72460=DIRECTION('',(-0.342020143325668,-0.939692620785909,0.));
#72461=DIRECTION('',(0.,0.,1.));
#72462=DIRECTION('center_axis',(0.,1.,0.));
#72463=DIRECTION('ref_axis',(-1.,0.,0.));
#72464=DIRECTION('',(-1.,0.,0.));
#72465=DIRECTION('',(-1.,0.,0.));
#72466=DIRECTION('',(0.,0.,1.));
#72467=DIRECTION('center_axis',(0.939692620785909,0.342020143325668,0.));
#72468=DIRECTION('ref_axis',(-0.342020143325668,0.939692620785909,0.));
#72469=DIRECTION('',(-0.342020143325668,0.939692620785909,0.));
#72470=DIRECTION('',(-0.342020143325668,0.939692620785909,0.));
#72471=DIRECTION('',(0.,0.,1.));
#72472=DIRECTION('center_axis',(0.,1.,0.));
#72473=DIRECTION('ref_axis',(-1.,0.,0.));
#72474=DIRECTION('',(-1.,0.,0.));
#72475=DIRECTION('',(-1.,0.,0.));
#72476=DIRECTION('',(0.,0.,1.));
#72477=DIRECTION('center_axis',(-0.939692620785909,0.342020143325668,0.));
#72478=DIRECTION('ref_axis',(-0.342020143325668,-0.939692620785909,0.));
#72479=DIRECTION('',(-0.342020143325668,-0.939692620785909,0.));
#72480=DIRECTION('',(-0.342020143325668,-0.939692620785909,0.));
#72481=DIRECTION('',(0.,0.,1.));
#72482=DIRECTION('center_axis',(0.,1.,0.));
#72483=DIRECTION('ref_axis',(-1.,0.,0.));
#72484=DIRECTION('',(-1.,0.,0.));
#72485=DIRECTION('',(-1.,0.,0.));
#72486=DIRECTION('',(0.,0.,1.));
#72487=DIRECTION('center_axis',(0.939692620785909,0.342020143325668,0.));
#72488=DIRECTION('ref_axis',(-0.342020143325668,0.939692620785909,0.));
#72489=DIRECTION('',(-0.342020143325668,0.939692620785909,0.));
#72490=DIRECTION('',(-0.342020143325668,0.939692620785909,0.));
#72491=DIRECTION('',(0.,0.,1.));
#72492=DIRECTION('center_axis',(0.,1.,0.));
#72493=DIRECTION('ref_axis',(-1.,0.,0.));
#72494=DIRECTION('',(-1.,0.,0.));
#72495=DIRECTION('',(-1.,0.,0.));
#72496=DIRECTION('',(0.,0.,1.));
#72497=DIRECTION('center_axis',(-0.939692620785909,0.342020143325668,0.));
#72498=DIRECTION('ref_axis',(-0.342020143325668,-0.939692620785909,0.));
#72499=DIRECTION('',(-0.342020143325668,-0.939692620785909,0.));
#72500=DIRECTION('',(-0.342020143325668,-0.939692620785909,0.));
#72501=DIRECTION('',(0.,0.,1.));
#72502=DIRECTION('center_axis',(0.,1.,0.));
#72503=DIRECTION('ref_axis',(-1.,0.,0.));
#72504=DIRECTION('',(-1.,0.,0.));
#72505=DIRECTION('',(-1.,0.,0.));
#72506=DIRECTION('',(0.,0.,1.));
#72507=DIRECTION('center_axis',(0.939692620785909,0.342020143325668,0.));
#72508=DIRECTION('ref_axis',(-0.342020143325668,0.939692620785909,0.));
#72509=DIRECTION('',(-0.342020143325668,0.939692620785909,0.));
#72510=DIRECTION('',(-0.342020143325668,0.939692620785909,0.));
#72511=DIRECTION('',(0.,0.,1.));
#72512=DIRECTION('center_axis',(0.,1.,0.));
#72513=DIRECTION('ref_axis',(-1.,0.,0.));
#72514=DIRECTION('',(-1.,0.,0.));
#72515=DIRECTION('',(-1.,0.,0.));
#72516=DIRECTION('',(0.,0.,1.));
#72517=DIRECTION('center_axis',(-0.939692620785909,0.342020143325668,0.));
#72518=DIRECTION('ref_axis',(-0.342020143325668,-0.939692620785909,0.));
#72519=DIRECTION('',(-0.342020143325668,-0.939692620785909,0.));
#72520=DIRECTION('',(-0.342020143325668,-0.939692620785909,0.));
#72521=DIRECTION('',(0.,0.,1.));
#72522=DIRECTION('center_axis',(0.,1.,0.));
#72523=DIRECTION('ref_axis',(-1.,0.,0.));
#72524=DIRECTION('',(-1.,0.,0.));
#72525=DIRECTION('',(-1.,0.,0.));
#72526=DIRECTION('',(0.,0.,1.));
#72527=DIRECTION('center_axis',(0.939692620785909,0.342020143325668,0.));
#72528=DIRECTION('ref_axis',(-0.342020143325668,0.939692620785909,0.));
#72529=DIRECTION('',(-0.342020143325668,0.939692620785909,0.));
#72530=DIRECTION('',(-0.342020143325668,0.939692620785909,0.));
#72531=DIRECTION('',(0.,0.,1.));
#72532=DIRECTION('center_axis',(0.,1.,0.));
#72533=DIRECTION('ref_axis',(-1.,0.,0.));
#72534=DIRECTION('',(-1.,0.,0.));
#72535=DIRECTION('',(-1.,0.,0.));
#72536=DIRECTION('',(0.,0.,1.));
#72537=DIRECTION('center_axis',(-0.939692620785909,0.342020143325668,0.));
#72538=DIRECTION('ref_axis',(-0.342020143325668,-0.939692620785909,0.));
#72539=DIRECTION('',(-0.342020143325668,-0.939692620785909,0.));
#72540=DIRECTION('',(-0.342020143325668,-0.939692620785909,0.));
#72541=DIRECTION('',(0.,0.,1.));
#72542=DIRECTION('center_axis',(0.,1.,0.));
#72543=DIRECTION('ref_axis',(-1.,0.,0.));
#72544=DIRECTION('',(-1.,0.,0.));
#72545=DIRECTION('',(-1.,0.,0.));
#72546=DIRECTION('',(0.,0.,1.));
#72547=DIRECTION('center_axis',(0.939692620785909,0.342020143325668,0.));
#72548=DIRECTION('ref_axis',(-0.342020143325668,0.939692620785909,0.));
#72549=DIRECTION('',(-0.342020143325668,0.939692620785909,0.));
#72550=DIRECTION('',(-0.342020143325668,0.939692620785909,0.));
#72551=DIRECTION('',(0.,0.,1.));
#72552=DIRECTION('center_axis',(0.,1.,0.));
#72553=DIRECTION('ref_axis',(-1.,0.,0.));
#72554=DIRECTION('',(-1.,0.,0.));
#72555=DIRECTION('',(-1.,0.,0.));
#72556=DIRECTION('',(0.,0.,1.));
#72557=DIRECTION('center_axis',(-0.939692620785909,0.342020143325668,0.));
#72558=DIRECTION('ref_axis',(-0.342020143325668,-0.939692620785909,0.));
#72559=DIRECTION('',(-0.342020143325668,-0.939692620785909,0.));
#72560=DIRECTION('',(-0.342020143325668,-0.939692620785909,0.));
#72561=DIRECTION('',(0.,0.,1.));
#72562=DIRECTION('center_axis',(0.,1.,0.));
#72563=DIRECTION('ref_axis',(-1.,0.,0.));
#72564=DIRECTION('',(-1.,0.,0.));
#72565=DIRECTION('',(-1.,0.,0.));
#72566=DIRECTION('',(0.,0.,1.));
#72567=DIRECTION('center_axis',(0.939692620785909,0.342020143325668,0.));
#72568=DIRECTION('ref_axis',(-0.342020143325668,0.939692620785909,0.));
#72569=DIRECTION('',(-0.342020143325668,0.939692620785909,0.));
#72570=DIRECTION('',(-0.342020143325668,0.939692620785909,0.));
#72571=DIRECTION('',(0.,0.,1.));
#72572=DIRECTION('center_axis',(0.,1.,0.));
#72573=DIRECTION('ref_axis',(-1.,0.,0.));
#72574=DIRECTION('',(-1.,0.,0.));
#72575=DIRECTION('',(-1.,0.,0.));
#72576=DIRECTION('',(0.,0.,1.));
#72577=DIRECTION('center_axis',(-0.939692620785909,0.342020143325668,0.));
#72578=DIRECTION('ref_axis',(-0.342020143325668,-0.939692620785909,0.));
#72579=DIRECTION('',(-0.342020143325668,-0.939692620785909,0.));
#72580=DIRECTION('',(-0.342020143325668,-0.939692620785909,0.));
#72581=DIRECTION('',(0.,0.,1.));
#72582=DIRECTION('center_axis',(0.,1.,0.));
#72583=DIRECTION('ref_axis',(-1.,0.,0.));
#72584=DIRECTION('',(-1.,0.,0.));
#72585=DIRECTION('',(-1.,0.,0.));
#72586=DIRECTION('',(0.,0.,1.));
#72587=DIRECTION('center_axis',(0.939692620785909,0.342020143325668,0.));
#72588=DIRECTION('ref_axis',(-0.342020143325668,0.939692620785909,0.));
#72589=DIRECTION('',(-0.342020143325668,0.939692620785909,0.));
#72590=DIRECTION('',(-0.342020143325668,0.939692620785909,0.));
#72591=DIRECTION('',(0.,0.,1.));
#72592=DIRECTION('center_axis',(0.,1.,0.));
#72593=DIRECTION('ref_axis',(-1.,0.,0.));
#72594=DIRECTION('',(-1.,0.,0.));
#72595=DIRECTION('',(-1.,0.,0.));
#72596=DIRECTION('',(0.,0.,1.));
#72597=DIRECTION('center_axis',(-0.939692620785909,0.342020143325668,0.));
#72598=DIRECTION('ref_axis',(-0.342020143325668,-0.939692620785909,0.));
#72599=DIRECTION('',(-0.342020143325668,-0.939692620785909,0.));
#72600=DIRECTION('',(-0.342020143325668,-0.939692620785909,0.));
#72601=DIRECTION('',(0.,0.,1.));
#72602=DIRECTION('center_axis',(0.,1.,0.));
#72603=DIRECTION('ref_axis',(-1.,0.,0.));
#72604=DIRECTION('',(-1.,0.,0.));
#72605=DIRECTION('',(-1.,0.,0.));
#72606=DIRECTION('',(0.,0.,1.));
#72607=DIRECTION('center_axis',(0.939692620785909,0.342020143325668,0.));
#72608=DIRECTION('ref_axis',(-0.342020143325668,0.939692620785909,0.));
#72609=DIRECTION('',(-0.342020143325668,0.939692620785909,0.));
#72610=DIRECTION('',(-0.342020143325668,0.939692620785909,0.));
#72611=DIRECTION('',(0.,0.,1.));
#72612=DIRECTION('center_axis',(0.,1.,0.));
#72613=DIRECTION('ref_axis',(-1.,0.,0.));
#72614=DIRECTION('',(-1.,0.,0.));
#72615=DIRECTION('',(-1.,0.,0.));
#72616=DIRECTION('',(0.,0.,1.));
#72617=DIRECTION('center_axis',(-0.939692620785909,0.342020143325668,0.));
#72618=DIRECTION('ref_axis',(-0.342020143325668,-0.939692620785909,0.));
#72619=DIRECTION('',(-0.342020143325668,-0.939692620785909,0.));
#72620=DIRECTION('',(-0.342020143325668,-0.939692620785909,0.));
#72621=DIRECTION('',(0.,0.,1.));
#72622=DIRECTION('center_axis',(0.,1.,0.));
#72623=DIRECTION('ref_axis',(-1.,0.,0.));
#72624=DIRECTION('',(-1.,0.,0.));
#72625=DIRECTION('',(-1.,0.,0.));
#72626=DIRECTION('',(0.,0.,1.));
#72627=DIRECTION('center_axis',(0.939692620785909,0.342020143325668,0.));
#72628=DIRECTION('ref_axis',(-0.342020143325668,0.939692620785909,0.));
#72629=DIRECTION('',(-0.342020143325668,0.939692620785909,0.));
#72630=DIRECTION('',(-0.342020143325668,0.939692620785909,0.));
#72631=DIRECTION('',(0.,0.,1.));
#72632=DIRECTION('center_axis',(0.,1.,0.));
#72633=DIRECTION('ref_axis',(-1.,0.,0.));
#72634=DIRECTION('',(-1.,0.,0.));
#72635=DIRECTION('',(-1.,0.,0.));
#72636=DIRECTION('',(0.,0.,1.));
#72637=DIRECTION('center_axis',(-0.939692620785909,0.342020143325668,0.));
#72638=DIRECTION('ref_axis',(-0.342020143325668,-0.939692620785909,0.));
#72639=DIRECTION('',(-0.342020143325668,-0.939692620785909,0.));
#72640=DIRECTION('',(-0.342020143325668,-0.939692620785909,0.));
#72641=DIRECTION('',(0.,0.,1.));
#72642=DIRECTION('center_axis',(0.,1.,0.));
#72643=DIRECTION('ref_axis',(-1.,0.,0.));
#72644=DIRECTION('',(-1.,0.,0.));
#72645=DIRECTION('',(-1.,0.,0.));
#72646=DIRECTION('',(0.,0.,1.));
#72647=DIRECTION('center_axis',(0.939692620785909,0.342020143325668,0.));
#72648=DIRECTION('ref_axis',(-0.342020143325668,0.939692620785909,0.));
#72649=DIRECTION('',(-0.342020143325668,0.939692620785909,0.));
#72650=DIRECTION('',(-0.342020143325668,0.939692620785909,0.));
#72651=DIRECTION('',(0.,0.,1.));
#72652=DIRECTION('center_axis',(0.,1.,0.));
#72653=DIRECTION('ref_axis',(-1.,0.,0.));
#72654=DIRECTION('',(-1.,0.,0.));
#72655=DIRECTION('',(-1.,0.,0.));
#72656=DIRECTION('',(0.,0.,1.));
#72657=DIRECTION('center_axis',(-0.939692620785909,0.342020143325668,0.));
#72658=DIRECTION('ref_axis',(-0.342020143325668,-0.939692620785909,0.));
#72659=DIRECTION('',(-0.342020143325668,-0.939692620785909,0.));
#72660=DIRECTION('',(-0.342020143325668,-0.939692620785909,0.));
#72661=DIRECTION('',(0.,0.,1.));
#72662=DIRECTION('center_axis',(0.,1.,0.));
#72663=DIRECTION('ref_axis',(-1.,0.,0.));
#72664=DIRECTION('',(-1.,0.,0.));
#72665=DIRECTION('',(-1.,0.,0.));
#72666=DIRECTION('',(0.,0.,1.));
#72667=DIRECTION('center_axis',(0.939692620785914,0.342020143325655,0.));
#72668=DIRECTION('ref_axis',(-0.342020143325655,0.939692620785914,0.));
#72669=DIRECTION('',(-0.342020143325655,0.939692620785914,0.));
#72670=DIRECTION('',(-0.342020143325655,0.939692620785914,0.));
#72671=DIRECTION('',(0.,0.,1.));
#72672=DIRECTION('center_axis',(0.,1.,0.));
#72673=DIRECTION('ref_axis',(-1.,0.,0.));
#72674=DIRECTION('',(-1.,0.,0.));
#72675=DIRECTION('',(-1.,0.,0.));
#72676=DIRECTION('',(0.,0.,1.));
#72677=DIRECTION('center_axis',(-0.939692620785909,0.342020143325668,0.));
#72678=DIRECTION('ref_axis',(-0.342020143325668,-0.939692620785909,0.));
#72679=DIRECTION('',(-0.342020143325668,-0.939692620785909,0.));
#72680=DIRECTION('',(-0.342020143325668,-0.939692620785909,0.));
#72681=DIRECTION('',(0.,0.,1.));
#72682=DIRECTION('center_axis',(0.,1.,0.));
#72683=DIRECTION('ref_axis',(-1.,0.,0.));
#72684=DIRECTION('',(-1.,0.,0.));
#72685=DIRECTION('',(-1.,0.,0.));
#72686=DIRECTION('',(0.,0.,1.));
#72687=DIRECTION('center_axis',(0.939692620785914,0.342020143325655,0.));
#72688=DIRECTION('ref_axis',(-0.342020143325655,0.939692620785914,0.));
#72689=DIRECTION('',(-0.342020143325655,0.939692620785914,0.));
#72690=DIRECTION('',(-0.342020143325655,0.939692620785914,0.));
#72691=DIRECTION('',(0.,0.,1.));
#72692=DIRECTION('center_axis',(0.,1.,0.));
#72693=DIRECTION('ref_axis',(-1.,0.,0.));
#72694=DIRECTION('',(-1.,0.,0.));
#72695=DIRECTION('',(-1.,0.,0.));
#72696=DIRECTION('',(0.,0.,1.));
#72697=DIRECTION('center_axis',(-0.939692620785914,0.342020143325655,0.));
#72698=DIRECTION('ref_axis',(-0.342020143325655,-0.939692620785914,0.));
#72699=DIRECTION('',(-0.342020143325655,-0.939692620785914,0.));
#72700=DIRECTION('',(-0.342020143325655,-0.939692620785914,0.));
#72701=DIRECTION('',(0.,0.,1.));
#72702=DIRECTION('center_axis',(0.,1.,0.));
#72703=DIRECTION('ref_axis',(-1.,0.,0.));
#72704=DIRECTION('',(-1.,0.,0.));
#72705=DIRECTION('',(-1.,0.,0.));
#72706=DIRECTION('',(0.,0.,1.));
#72707=DIRECTION('center_axis',(0.939692620785914,0.342020143325655,0.));
#72708=DIRECTION('ref_axis',(-0.342020143325655,0.939692620785914,0.));
#72709=DIRECTION('',(-0.342020143325655,0.939692620785914,0.));
#72710=DIRECTION('',(-0.342020143325655,0.939692620785914,0.));
#72711=DIRECTION('',(0.,0.,1.));
#72712=DIRECTION('center_axis',(0.,1.,0.));
#72713=DIRECTION('ref_axis',(-1.,0.,0.));
#72714=DIRECTION('',(-1.,0.,0.));
#72715=DIRECTION('',(-1.,0.,0.));
#72716=DIRECTION('',(0.,0.,1.));
#72717=DIRECTION('center_axis',(-0.939692620785909,0.342020143325668,0.));
#72718=DIRECTION('ref_axis',(-0.342020143325668,-0.939692620785909,0.));
#72719=DIRECTION('',(-0.342020143325668,-0.939692620785909,0.));
#72720=DIRECTION('',(-0.342020143325668,-0.939692620785909,0.));
#72721=DIRECTION('',(0.,0.,1.));
#72722=DIRECTION('center_axis',(0.,1.,0.));
#72723=DIRECTION('ref_axis',(-1.,0.,0.));
#72724=DIRECTION('',(-1.,0.,0.));
#72725=DIRECTION('',(-1.,0.,0.));
#72726=DIRECTION('',(0.,0.,1.));
#72727=DIRECTION('center_axis',(0.939692620785914,0.342020143325655,0.));
#72728=DIRECTION('ref_axis',(-0.342020143325655,0.939692620785914,0.));
#72729=DIRECTION('',(-0.342020143325655,0.939692620785914,0.));
#72730=DIRECTION('',(-0.342020143325655,0.939692620785914,0.));
#72731=DIRECTION('',(0.,0.,1.));
#72732=DIRECTION('center_axis',(0.,1.,0.));
#72733=DIRECTION('ref_axis',(-1.,0.,0.));
#72734=DIRECTION('',(-1.,0.,0.));
#72735=DIRECTION('',(-1.,0.,0.));
#72736=DIRECTION('',(0.,0.,1.));
#72737=DIRECTION('center_axis',(-0.939692620785914,0.342020143325655,0.));
#72738=DIRECTION('ref_axis',(-0.342020143325655,-0.939692620785914,0.));
#72739=DIRECTION('',(-0.342020143325655,-0.939692620785914,0.));
#72740=DIRECTION('',(-0.342020143325655,-0.939692620785914,0.));
#72741=DIRECTION('',(0.,0.,1.));
#72742=DIRECTION('center_axis',(0.,1.,0.));
#72743=DIRECTION('ref_axis',(-1.,0.,0.));
#72744=DIRECTION('',(-1.,0.,0.));
#72745=DIRECTION('',(-1.,0.,0.));
#72746=DIRECTION('',(0.,0.,1.));
#72747=DIRECTION('center_axis',(0.939692620785914,0.342020143325655,0.));
#72748=DIRECTION('ref_axis',(-0.342020143325655,0.939692620785914,0.));
#72749=DIRECTION('',(-0.342020143325655,0.939692620785914,0.));
#72750=DIRECTION('',(-0.342020143325655,0.939692620785914,0.));
#72751=DIRECTION('',(0.,0.,1.));
#72752=DIRECTION('center_axis',(0.,1.,0.));
#72753=DIRECTION('ref_axis',(-1.,0.,0.));
#72754=DIRECTION('',(-1.,0.,0.));
#72755=DIRECTION('',(-1.,0.,0.));
#72756=DIRECTION('',(0.,0.,1.));
#72757=DIRECTION('center_axis',(-0.939692620785914,0.342020143325655,0.));
#72758=DIRECTION('ref_axis',(-0.342020143325655,-0.939692620785914,0.));
#72759=DIRECTION('',(-0.342020143325655,-0.939692620785914,0.));
#72760=DIRECTION('',(-0.342020143325655,-0.939692620785914,0.));
#72761=DIRECTION('',(0.,0.,1.));
#72762=DIRECTION('center_axis',(0.,1.,0.));
#72763=DIRECTION('ref_axis',(-1.,0.,0.));
#72764=DIRECTION('',(-1.,0.,0.));
#72765=DIRECTION('',(-1.,0.,0.));
#72766=DIRECTION('',(0.,0.,1.));
#72767=DIRECTION('center_axis',(0.939692620785914,0.342020143325655,0.));
#72768=DIRECTION('ref_axis',(-0.342020143325655,0.939692620785914,0.));
#72769=DIRECTION('',(-0.342020143325655,0.939692620785914,0.));
#72770=DIRECTION('',(-0.342020143325655,0.939692620785914,0.));
#72771=DIRECTION('',(0.,0.,1.));
#72772=DIRECTION('center_axis',(0.,1.,0.));
#72773=DIRECTION('ref_axis',(-1.,0.,0.));
#72774=DIRECTION('',(-1.,0.,0.));
#72775=DIRECTION('',(-1.,0.,0.));
#72776=DIRECTION('',(0.,0.,1.));
#72777=DIRECTION('center_axis',(-0.939692620785914,0.342020143325655,0.));
#72778=DIRECTION('ref_axis',(-0.342020143325655,-0.939692620785914,0.));
#72779=DIRECTION('',(-0.342020143325655,-0.939692620785914,0.));
#72780=DIRECTION('',(-0.342020143325655,-0.939692620785914,0.));
#72781=DIRECTION('',(0.,0.,1.));
#72782=DIRECTION('center_axis',(0.,1.,0.));
#72783=DIRECTION('ref_axis',(-1.,0.,0.));
#72784=DIRECTION('',(-1.,0.,0.));
#72785=DIRECTION('',(-1.,0.,0.));
#72786=DIRECTION('',(0.,0.,1.));
#72787=DIRECTION('center_axis',(0.939692620785909,0.342020143325668,0.));
#72788=DIRECTION('ref_axis',(-0.342020143325668,0.939692620785909,0.));
#72789=DIRECTION('',(-0.342020143325668,0.939692620785909,0.));
#72790=DIRECTION('',(-0.342020143325668,0.939692620785909,0.));
#72791=DIRECTION('',(0.,0.,1.));
#72792=DIRECTION('center_axis',(0.,1.,0.));
#72793=DIRECTION('ref_axis',(-1.,0.,0.));
#72794=DIRECTION('',(-1.,0.,0.));
#72795=DIRECTION('',(-1.,0.,0.));
#72796=DIRECTION('',(0.,0.,1.));
#72797=DIRECTION('center_axis',(-0.939692620785914,0.342020143325655,0.));
#72798=DIRECTION('ref_axis',(-0.342020143325655,-0.939692620785914,0.));
#72799=DIRECTION('',(-0.342020143325655,-0.939692620785914,0.));
#72800=DIRECTION('',(-0.342020143325655,-0.939692620785914,0.));
#72801=DIRECTION('',(0.,0.,1.));
#72802=DIRECTION('center_axis',(0.,1.,0.));
#72803=DIRECTION('ref_axis',(-1.,0.,0.));
#72804=DIRECTION('',(-1.,0.,0.));
#72805=DIRECTION('',(-1.,0.,0.));
#72806=DIRECTION('',(0.,0.,1.));
#72807=DIRECTION('center_axis',(0.939692620785914,0.342020143325655,0.));
#72808=DIRECTION('ref_axis',(-0.342020143325655,0.939692620785914,0.));
#72809=DIRECTION('',(-0.342020143325655,0.939692620785914,0.));
#72810=DIRECTION('',(-0.342020143325655,0.939692620785914,0.));
#72811=DIRECTION('',(0.,0.,1.));
#72812=DIRECTION('center_axis',(0.,1.,0.));
#72813=DIRECTION('ref_axis',(-1.,0.,0.));
#72814=DIRECTION('',(-1.,0.,0.));
#72815=DIRECTION('',(-1.,0.,0.));
#72816=DIRECTION('',(0.,0.,1.));
#72817=DIRECTION('center_axis',(-0.939692620785914,0.342020143325655,0.));
#72818=DIRECTION('ref_axis',(-0.342020143325655,-0.939692620785914,0.));
#72819=DIRECTION('',(-0.342020143325655,-0.939692620785914,0.));
#72820=DIRECTION('',(-0.342020143325655,-0.939692620785914,0.));
#72821=DIRECTION('',(0.,0.,1.));
#72822=DIRECTION('center_axis',(0.,1.,0.));
#72823=DIRECTION('ref_axis',(-1.,0.,0.));
#72824=DIRECTION('',(-1.,0.,0.));
#72825=DIRECTION('',(-1.,0.,0.));
#72826=DIRECTION('',(0.,0.,1.));
#72827=DIRECTION('center_axis',(0.939692620785909,0.342020143325668,0.));
#72828=DIRECTION('ref_axis',(-0.342020143325668,0.939692620785909,0.));
#72829=DIRECTION('',(-0.342020143325668,0.939692620785909,0.));
#72830=DIRECTION('',(-0.342020143325668,0.939692620785909,0.));
#72831=DIRECTION('',(0.,0.,1.));
#72832=DIRECTION('center_axis',(0.,1.,0.));
#72833=DIRECTION('ref_axis',(-1.,0.,0.));
#72834=DIRECTION('',(-1.,0.,0.));
#72835=DIRECTION('',(-1.,0.,0.));
#72836=DIRECTION('',(0.,0.,1.));
#72837=DIRECTION('center_axis',(-0.939692620785914,0.342020143325655,0.));
#72838=DIRECTION('ref_axis',(-0.342020143325655,-0.939692620785914,0.));
#72839=DIRECTION('',(-0.342020143325655,-0.939692620785914,0.));
#72840=DIRECTION('',(-0.342020143325655,-0.939692620785914,0.));
#72841=DIRECTION('',(0.,0.,1.));
#72842=DIRECTION('center_axis',(0.,1.,0.));
#72843=DIRECTION('ref_axis',(-1.,0.,0.));
#72844=DIRECTION('',(-1.,0.,0.));
#72845=DIRECTION('',(-1.,0.,0.));
#72846=DIRECTION('',(0.,0.,1.));
#72847=DIRECTION('center_axis',(0.939692620785914,0.342020143325655,0.));
#72848=DIRECTION('ref_axis',(-0.342020143325655,0.939692620785914,0.));
#72849=DIRECTION('',(-0.342020143325655,0.939692620785914,0.));
#72850=DIRECTION('',(-0.342020143325655,0.939692620785914,0.));
#72851=DIRECTION('',(0.,0.,1.));
#72852=DIRECTION('center_axis',(0.,1.,0.));
#72853=DIRECTION('ref_axis',(-1.,0.,0.));
#72854=DIRECTION('',(-1.,0.,0.));
#72855=DIRECTION('',(-1.,0.,0.));
#72856=DIRECTION('',(0.,0.,1.));
#72857=DIRECTION('center_axis',(-0.939692620785909,0.342020143325668,0.));
#72858=DIRECTION('ref_axis',(-0.342020143325668,-0.939692620785909,0.));
#72859=DIRECTION('',(-0.342020143325668,-0.939692620785909,0.));
#72860=DIRECTION('',(-0.342020143325668,-0.939692620785909,0.));
#72861=DIRECTION('',(0.,0.,1.));
#72862=DIRECTION('center_axis',(0.,1.,0.));
#72863=DIRECTION('ref_axis',(-1.,0.,0.));
#72864=DIRECTION('',(-1.,0.,0.));
#72865=DIRECTION('',(-1.,0.,0.));
#72866=DIRECTION('',(0.,0.,1.));
#72867=DIRECTION('center_axis',(0.939692620785914,0.342020143325655,0.));
#72868=DIRECTION('ref_axis',(-0.342020143325655,0.939692620785914,0.));
#72869=DIRECTION('',(-0.342020143325655,0.939692620785914,0.));
#72870=DIRECTION('',(-0.342020143325655,0.939692620785914,0.));
#72871=DIRECTION('',(0.,0.,1.));
#72872=DIRECTION('center_axis',(0.,1.,0.));
#72873=DIRECTION('ref_axis',(-1.,0.,0.));
#72874=DIRECTION('',(-1.,0.,0.));
#72875=DIRECTION('',(-1.,0.,0.));
#72876=DIRECTION('',(0.,0.,1.));
#72877=DIRECTION('center_axis',(-0.939692620785914,0.342020143325655,0.));
#72878=DIRECTION('ref_axis',(-0.342020143325655,-0.939692620785914,0.));
#72879=DIRECTION('',(-0.342020143325655,-0.939692620785914,0.));
#72880=DIRECTION('',(-0.342020143325655,-0.939692620785914,0.));
#72881=DIRECTION('',(0.,0.,1.));
#72882=DIRECTION('center_axis',(0.,1.,0.));
#72883=DIRECTION('ref_axis',(-1.,0.,0.));
#72884=DIRECTION('',(-1.,0.,0.));
#72885=DIRECTION('',(-1.,0.,0.));
#72886=DIRECTION('',(0.,0.,1.));
#72887=DIRECTION('center_axis',(0.939692620785914,0.342020143325655,0.));
#72888=DIRECTION('ref_axis',(-0.342020143325655,0.939692620785914,0.));
#72889=DIRECTION('',(-0.342020143325655,0.939692620785914,0.));
#72890=DIRECTION('',(-0.342020143325655,0.939692620785914,0.));
#72891=DIRECTION('',(0.,0.,1.));
#72892=DIRECTION('center_axis',(0.,1.,0.));
#72893=DIRECTION('ref_axis',(-1.,0.,0.));
#72894=DIRECTION('',(-1.,0.,0.));
#72895=DIRECTION('',(-1.,0.,0.));
#72896=DIRECTION('',(0.,0.,1.));
#72897=DIRECTION('center_axis',(-0.939692620785914,0.342020143325655,0.));
#72898=DIRECTION('ref_axis',(-0.342020143325655,-0.939692620785914,0.));
#72899=DIRECTION('',(-0.342020143325655,-0.939692620785914,0.));
#72900=DIRECTION('',(-0.342020143325655,-0.939692620785914,0.));
#72901=DIRECTION('',(0.,0.,1.));
#72902=DIRECTION('center_axis',(0.,1.,0.));
#72903=DIRECTION('ref_axis',(-1.,0.,0.));
#72904=DIRECTION('',(-1.,0.,0.));
#72905=DIRECTION('',(-1.,0.,0.));
#72906=DIRECTION('',(0.,0.,1.));
#72907=DIRECTION('center_axis',(0.939692620785914,0.342020143325655,0.));
#72908=DIRECTION('ref_axis',(-0.342020143325655,0.939692620785914,0.));
#72909=DIRECTION('',(-0.342020143325655,0.939692620785914,0.));
#72910=DIRECTION('',(-0.342020143325655,0.939692620785914,0.));
#72911=DIRECTION('',(0.,0.,1.));
#72912=DIRECTION('center_axis',(0.,1.,0.));
#72913=DIRECTION('ref_axis',(-1.,0.,0.));
#72914=DIRECTION('',(-1.,0.,0.));
#72915=DIRECTION('',(-1.,0.,0.));
#72916=DIRECTION('',(0.,0.,1.));
#72917=DIRECTION('center_axis',(-0.939692620785914,0.342020143325655,0.));
#72918=DIRECTION('ref_axis',(-0.342020143325655,-0.939692620785914,0.));
#72919=DIRECTION('',(-0.342020143325655,-0.939692620785914,0.));
#72920=DIRECTION('',(-0.342020143325655,-0.939692620785914,0.));
#72921=DIRECTION('',(0.,0.,1.));
#72922=DIRECTION('center_axis',(0.,1.,0.));
#72923=DIRECTION('ref_axis',(-1.,0.,0.));
#72924=DIRECTION('',(-1.,0.,0.));
#72925=DIRECTION('',(-1.,0.,0.));
#72926=DIRECTION('',(0.,0.,1.));
#72927=DIRECTION('center_axis',(0.939692620785914,0.342020143325655,0.));
#72928=DIRECTION('ref_axis',(-0.342020143325655,0.939692620785914,0.));
#72929=DIRECTION('',(-0.342020143325655,0.939692620785914,0.));
#72930=DIRECTION('',(-0.342020143325655,0.939692620785914,0.));
#72931=DIRECTION('',(0.,0.,1.));
#72932=DIRECTION('center_axis',(0.,1.,0.));
#72933=DIRECTION('ref_axis',(-1.,0.,0.));
#72934=DIRECTION('',(-1.,0.,0.));
#72935=DIRECTION('',(-1.,0.,0.));
#72936=DIRECTION('',(0.,0.,1.));
#72937=DIRECTION('center_axis',(-0.939692620785914,0.342020143325655,0.));
#72938=DIRECTION('ref_axis',(-0.342020143325655,-0.939692620785914,0.));
#72939=DIRECTION('',(-0.342020143325655,-0.939692620785914,0.));
#72940=DIRECTION('',(-0.342020143325655,-0.939692620785914,0.));
#72941=DIRECTION('',(0.,0.,1.));
#72942=DIRECTION('center_axis',(0.,1.,0.));
#72943=DIRECTION('ref_axis',(-1.,0.,0.));
#72944=DIRECTION('',(-1.,0.,0.));
#72945=DIRECTION('',(-1.,0.,0.));
#72946=DIRECTION('',(0.,0.,1.));
#72947=DIRECTION('center_axis',(0.939692620785914,0.342020143325655,0.));
#72948=DIRECTION('ref_axis',(-0.342020143325655,0.939692620785914,0.));
#72949=DIRECTION('',(-0.342020143325655,0.939692620785914,0.));
#72950=DIRECTION('',(-0.342020143325655,0.939692620785914,0.));
#72951=DIRECTION('',(0.,0.,1.));
#72952=DIRECTION('center_axis',(0.,1.,0.));
#72953=DIRECTION('ref_axis',(-1.,0.,0.));
#72954=DIRECTION('',(-1.,0.,0.));
#72955=DIRECTION('',(-1.,0.,0.));
#72956=DIRECTION('',(0.,0.,1.));
#72957=DIRECTION('center_axis',(-0.939692620785914,0.342020143325655,0.));
#72958=DIRECTION('ref_axis',(-0.342020143325655,-0.939692620785914,0.));
#72959=DIRECTION('',(-0.342020143325655,-0.939692620785914,0.));
#72960=DIRECTION('',(-0.342020143325655,-0.939692620785914,0.));
#72961=DIRECTION('',(0.,0.,1.));
#72962=DIRECTION('center_axis',(0.,1.,0.));
#72963=DIRECTION('ref_axis',(-1.,0.,0.));
#72964=DIRECTION('',(-1.,0.,0.));
#72965=DIRECTION('',(-1.,0.,0.));
#72966=DIRECTION('',(0.,0.,1.));
#72967=DIRECTION('center_axis',(0.939692620785909,0.342020143325668,0.));
#72968=DIRECTION('ref_axis',(-0.342020143325668,0.939692620785909,0.));
#72969=DIRECTION('',(-0.342020143325668,0.939692620785909,0.));
#72970=DIRECTION('',(-0.342020143325668,0.939692620785909,0.));
#72971=DIRECTION('',(0.,0.,1.));
#72972=DIRECTION('center_axis',(0.,1.,0.));
#72973=DIRECTION('ref_axis',(-1.,0.,0.));
#72974=DIRECTION('',(-1.,0.,0.));
#72975=DIRECTION('',(-1.,0.,0.));
#72976=DIRECTION('',(0.,0.,1.));
#72977=DIRECTION('center_axis',(-0.939692620785914,0.342020143325655,0.));
#72978=DIRECTION('ref_axis',(-0.342020143325655,-0.939692620785914,0.));
#72979=DIRECTION('',(-0.342020143325655,-0.939692620785914,0.));
#72980=DIRECTION('',(-0.342020143325655,-0.939692620785914,0.));
#72981=DIRECTION('',(0.,0.,1.));
#72982=DIRECTION('center_axis',(0.,1.,0.));
#72983=DIRECTION('ref_axis',(-1.,0.,0.));
#72984=DIRECTION('',(-1.,0.,0.));
#72985=DIRECTION('',(-1.,0.,0.));
#72986=DIRECTION('',(0.,0.,1.));
#72987=DIRECTION('center_axis',(0.939692620785914,0.342020143325655,0.));
#72988=DIRECTION('ref_axis',(-0.342020143325655,0.939692620785914,0.));
#72989=DIRECTION('',(-0.342020143325655,0.939692620785914,0.));
#72990=DIRECTION('',(-0.342020143325655,0.939692620785914,0.));
#72991=DIRECTION('',(0.,0.,1.));
#72992=DIRECTION('center_axis',(0.,1.,0.));
#72993=DIRECTION('ref_axis',(-1.,0.,0.));
#72994=DIRECTION('',(-1.,0.,0.));
#72995=DIRECTION('',(-1.,0.,0.));
#72996=DIRECTION('',(0.,0.,1.));
#72997=DIRECTION('center_axis',(-0.939692620785909,0.342020143325668,0.));
#72998=DIRECTION('ref_axis',(-0.342020143325668,-0.939692620785909,0.));
#72999=DIRECTION('',(-0.342020143325668,-0.939692620785909,0.));
#73000=DIRECTION('',(-0.342020143325668,-0.939692620785909,0.));
#73001=DIRECTION('',(0.,0.,1.));
#73002=DIRECTION('center_axis',(0.,1.,0.));
#73003=DIRECTION('ref_axis',(-1.,0.,0.));
#73004=DIRECTION('',(-1.,0.,0.));
#73005=DIRECTION('',(-1.,0.,0.));
#73006=DIRECTION('',(0.,0.,1.));
#73007=DIRECTION('center_axis',(0.939692620785909,0.342020143325668,0.));
#73008=DIRECTION('ref_axis',(-0.342020143325668,0.939692620785909,0.));
#73009=DIRECTION('',(-0.342020143325668,0.939692620785909,0.));
#73010=DIRECTION('',(-0.342020143325668,0.939692620785909,0.));
#73011=DIRECTION('',(0.,0.,1.));
#73012=DIRECTION('center_axis',(0.,1.,0.));
#73013=DIRECTION('ref_axis',(-1.,0.,0.));
#73014=DIRECTION('',(-1.,0.,0.));
#73015=DIRECTION('',(-1.,0.,0.));
#73016=DIRECTION('',(0.,0.,1.));
#73017=DIRECTION('center_axis',(-0.939692620785914,0.342020143325655,0.));
#73018=DIRECTION('ref_axis',(-0.342020143325655,-0.939692620785914,0.));
#73019=DIRECTION('',(-0.342020143325655,-0.939692620785914,0.));
#73020=DIRECTION('',(-0.342020143325655,-0.939692620785914,0.));
#73021=DIRECTION('',(0.,0.,1.));
#73022=DIRECTION('center_axis',(0.,1.,0.));
#73023=DIRECTION('ref_axis',(-1.,0.,0.));
#73024=DIRECTION('',(-1.,0.,0.));
#73025=DIRECTION('',(-1.,0.,0.));
#73026=DIRECTION('',(0.,0.,1.));
#73027=DIRECTION('center_axis',(0.939692620785914,0.342020143325655,0.));
#73028=DIRECTION('ref_axis',(-0.342020143325655,0.939692620785914,0.));
#73029=DIRECTION('',(-0.342020143325655,0.939692620785914,0.));
#73030=DIRECTION('',(-0.342020143325655,0.939692620785914,0.));
#73031=DIRECTION('',(0.,0.,1.));
#73032=DIRECTION('center_axis',(0.,1.,0.));
#73033=DIRECTION('ref_axis',(-1.,0.,0.));
#73034=DIRECTION('',(-1.,0.,0.));
#73035=DIRECTION('',(-1.,0.,0.));
#73036=DIRECTION('',(0.,0.,1.));
#73037=DIRECTION('center_axis',(-0.939692620785909,0.342020143325668,0.));
#73038=DIRECTION('ref_axis',(-0.342020143325668,-0.939692620785909,0.));
#73039=DIRECTION('',(-0.342020143325668,-0.939692620785909,0.));
#73040=DIRECTION('',(-0.342020143325668,-0.939692620785909,0.));
#73041=DIRECTION('',(0.,0.,1.));
#73042=DIRECTION('center_axis',(0.,1.,0.));
#73043=DIRECTION('ref_axis',(-1.,0.,0.));
#73044=DIRECTION('',(-1.,0.,0.));
#73045=DIRECTION('',(-1.,0.,0.));
#73046=DIRECTION('',(0.,0.,1.));
#73047=DIRECTION('center_axis',(0.939692620785914,0.342020143325655,0.));
#73048=DIRECTION('ref_axis',(-0.342020143325655,0.939692620785914,0.));
#73049=DIRECTION('',(-0.342020143325655,0.939692620785914,0.));
#73050=DIRECTION('',(-0.342020143325655,0.939692620785914,0.));
#73051=DIRECTION('',(0.,0.,1.));
#73052=DIRECTION('center_axis',(0.,1.,0.));
#73053=DIRECTION('ref_axis',(-1.,0.,0.));
#73054=DIRECTION('',(-1.,0.,0.));
#73055=DIRECTION('',(-1.,0.,0.));
#73056=DIRECTION('',(0.,0.,1.));
#73057=DIRECTION('center_axis',(-0.939692620785914,0.342020143325655,0.));
#73058=DIRECTION('ref_axis',(-0.342020143325655,-0.939692620785914,0.));
#73059=DIRECTION('',(-0.342020143325655,-0.939692620785914,0.));
#73060=DIRECTION('',(-0.342020143325655,-0.939692620785914,0.));
#73061=DIRECTION('',(0.,0.,1.));
#73062=DIRECTION('center_axis',(0.,1.,0.));
#73063=DIRECTION('ref_axis',(-1.,0.,0.));
#73064=DIRECTION('',(-1.,0.,0.));
#73065=DIRECTION('',(-1.,0.,0.));
#73066=DIRECTION('',(0.,0.,1.));
#73067=DIRECTION('center_axis',(0.939692620785909,0.342020143325668,0.));
#73068=DIRECTION('ref_axis',(-0.342020143325668,0.939692620785909,0.));
#73069=DIRECTION('',(-0.342020143325668,0.939692620785909,0.));
#73070=DIRECTION('',(-0.342020143325668,0.939692620785909,0.));
#73071=DIRECTION('',(0.,0.,1.));
#73072=DIRECTION('center_axis',(0.,1.,0.));
#73073=DIRECTION('ref_axis',(-1.,0.,0.));
#73074=DIRECTION('',(-1.,0.,0.));
#73075=DIRECTION('',(-1.,0.,0.));
#73076=DIRECTION('',(0.,0.,1.));
#73077=DIRECTION('center_axis',(-0.939692620785909,0.342020143325668,0.));
#73078=DIRECTION('ref_axis',(-0.342020143325668,-0.939692620785909,0.));
#73079=DIRECTION('',(-0.342020143325668,-0.939692620785909,0.));
#73080=DIRECTION('',(-0.342020143325668,-0.939692620785909,0.));
#73081=DIRECTION('',(0.,0.,1.));
#73082=DIRECTION('center_axis',(0.,1.,0.));
#73083=DIRECTION('ref_axis',(-1.,0.,0.));
#73084=DIRECTION('',(-1.,0.,0.));
#73085=DIRECTION('',(-1.,0.,0.));
#73086=DIRECTION('',(0.,0.,1.));
#73087=DIRECTION('center_axis',(0.939692620785919,0.342020143325641,0.));
#73088=DIRECTION('ref_axis',(-0.342020143325641,0.939692620785918,0.));
#73089=DIRECTION('',(-0.342020143325641,0.939692620785918,0.));
#73090=DIRECTION('',(-0.342020143325641,0.939692620785918,0.));
#73091=DIRECTION('',(0.,0.,1.));
#73092=DIRECTION('center_axis',(0.,1.,0.));
#73093=DIRECTION('ref_axis',(-1.,0.,0.));
#73094=DIRECTION('',(-1.,0.,0.));
#73095=DIRECTION('',(-1.,0.,0.));
#73096=DIRECTION('',(0.,0.,1.));
#73097=DIRECTION('center_axis',(-0.939692620785909,0.342020143325668,0.));
#73098=DIRECTION('ref_axis',(-0.342020143325668,-0.939692620785909,0.));
#73099=DIRECTION('',(-0.342020143325668,-0.939692620785909,0.));
#73100=DIRECTION('',(-0.342020143325668,-0.939692620785909,0.));
#73101=DIRECTION('',(0.,0.,1.));
#73102=DIRECTION('center_axis',(0.,1.,0.));
#73103=DIRECTION('ref_axis',(-1.,0.,0.));
#73104=DIRECTION('',(-1.,0.,0.));
#73105=DIRECTION('',(-1.,0.,0.));
#73106=DIRECTION('',(0.,0.,1.));
#73107=DIRECTION('center_axis',(0.939692620785909,0.342020143325668,0.));
#73108=DIRECTION('ref_axis',(-0.342020143325668,0.939692620785909,0.));
#73109=DIRECTION('',(-0.342020143325668,0.939692620785909,0.));
#73110=DIRECTION('',(-0.342020143325668,0.939692620785909,0.));
#73111=DIRECTION('',(0.,0.,1.));
#73112=DIRECTION('center_axis',(0.,1.,0.));
#73113=DIRECTION('ref_axis',(-1.,0.,0.));
#73114=DIRECTION('',(-1.,0.,0.));
#73115=DIRECTION('',(-1.,0.,0.));
#73116=DIRECTION('',(0.,0.,1.));
#73117=DIRECTION('center_axis',(-0.939692620785919,0.342020143325641,0.));
#73118=DIRECTION('ref_axis',(-0.342020143325641,-0.939692620785918,0.));
#73119=DIRECTION('',(-0.342020143325641,-0.939692620785918,0.));
#73120=DIRECTION('',(-0.342020143325641,-0.939692620785918,0.));
#73121=DIRECTION('',(0.,0.,1.));
#73122=DIRECTION('center_axis',(0.,1.,0.));
#73123=DIRECTION('ref_axis',(-1.,0.,0.));
#73124=DIRECTION('',(-1.,0.,0.));
#73125=DIRECTION('',(-1.,0.,0.));
#73126=DIRECTION('',(0.,0.,1.));
#73127=DIRECTION('center_axis',(0.939692620785919,0.342020143325641,0.));
#73128=DIRECTION('ref_axis',(-0.342020143325641,0.939692620785918,0.));
#73129=DIRECTION('',(-0.342020143325641,0.939692620785918,0.));
#73130=DIRECTION('',(-0.342020143325641,0.939692620785918,0.));
#73131=DIRECTION('',(0.,0.,1.));
#73132=DIRECTION('center_axis',(0.,1.,0.));
#73133=DIRECTION('ref_axis',(-1.,0.,0.));
#73134=DIRECTION('',(-1.,0.,0.));
#73135=DIRECTION('',(-1.,0.,0.));
#73136=DIRECTION('',(0.,0.,1.));
#73137=DIRECTION('center_axis',(-0.939692620785909,0.342020143325668,0.));
#73138=DIRECTION('ref_axis',(-0.342020143325668,-0.939692620785909,0.));
#73139=DIRECTION('',(-0.342020143325668,-0.939692620785909,0.));
#73140=DIRECTION('',(-0.342020143325668,-0.939692620785909,0.));
#73141=DIRECTION('',(0.,0.,1.));
#73142=DIRECTION('center_axis',(0.,1.,0.));
#73143=DIRECTION('ref_axis',(-1.,0.,0.));
#73144=DIRECTION('',(-1.,0.,0.));
#73145=DIRECTION('',(-1.,0.,0.));
#73146=DIRECTION('',(0.,0.,1.));
#73147=DIRECTION('center_axis',(0.939692620785909,0.342020143325668,0.));
#73148=DIRECTION('ref_axis',(-0.342020143325668,0.939692620785909,0.));
#73149=DIRECTION('',(-0.342020143325668,0.939692620785909,0.));
#73150=DIRECTION('',(-0.342020143325668,0.939692620785909,0.));
#73151=DIRECTION('',(0.,0.,1.));
#73152=DIRECTION('center_axis',(0.,1.,0.));
#73153=DIRECTION('ref_axis',(-1.,0.,0.));
#73154=DIRECTION('',(-1.,0.,0.));
#73155=DIRECTION('',(-1.,0.,0.));
#73156=DIRECTION('',(0.,0.,1.));
#73157=DIRECTION('center_axis',(-0.939692620785919,0.342020143325641,0.));
#73158=DIRECTION('ref_axis',(-0.342020143325641,-0.939692620785918,0.));
#73159=DIRECTION('',(-0.342020143325641,-0.939692620785918,0.));
#73160=DIRECTION('',(-0.342020143325641,-0.939692620785918,0.));
#73161=DIRECTION('',(0.,0.,1.));
#73162=DIRECTION('center_axis',(0.,1.,0.));
#73163=DIRECTION('ref_axis',(-1.,0.,0.));
#73164=DIRECTION('',(-1.,0.,0.));
#73165=DIRECTION('',(-1.,0.,0.));
#73166=DIRECTION('',(0.,0.,1.));
#73167=DIRECTION('center_axis',(0.939692620785919,0.342020143325641,0.));
#73168=DIRECTION('ref_axis',(-0.342020143325641,0.939692620785918,0.));
#73169=DIRECTION('',(-0.342020143325641,0.939692620785918,0.));
#73170=DIRECTION('',(-0.342020143325641,0.939692620785918,0.));
#73171=DIRECTION('',(0.,0.,1.));
#73172=DIRECTION('center_axis',(0.,1.,0.));
#73173=DIRECTION('ref_axis',(-1.,0.,0.));
#73174=DIRECTION('',(-1.,0.,0.));
#73175=DIRECTION('',(-1.,0.,0.));
#73176=DIRECTION('',(0.,0.,1.));
#73177=DIRECTION('center_axis',(-0.939692620785909,0.342020143325668,0.));
#73178=DIRECTION('ref_axis',(-0.342020143325668,-0.939692620785909,0.));
#73179=DIRECTION('',(-0.342020143325668,-0.939692620785909,0.));
#73180=DIRECTION('',(-0.342020143325668,-0.939692620785909,0.));
#73181=DIRECTION('',(0.,0.,1.));
#73182=DIRECTION('center_axis',(0.,1.,0.));
#73183=DIRECTION('ref_axis',(-1.,0.,0.));
#73184=DIRECTION('',(-1.,0.,0.));
#73185=DIRECTION('',(-1.,0.,0.));
#73186=DIRECTION('',(0.,0.,1.));
#73187=DIRECTION('center_axis',(0.939692620785909,0.342020143325668,0.));
#73188=DIRECTION('ref_axis',(-0.342020143325668,0.939692620785909,0.));
#73189=DIRECTION('',(-0.342020143325668,0.939692620785909,0.));
#73190=DIRECTION('',(-0.342020143325668,0.939692620785909,0.));
#73191=DIRECTION('',(0.,0.,1.));
#73192=DIRECTION('center_axis',(0.,1.,0.));
#73193=DIRECTION('ref_axis',(-1.,0.,0.));
#73194=DIRECTION('',(-1.,0.,0.));
#73195=DIRECTION('',(-1.,0.,0.));
#73196=DIRECTION('',(0.,0.,1.));
#73197=DIRECTION('center_axis',(-0.939692620785919,0.342020143325641,0.));
#73198=DIRECTION('ref_axis',(-0.342020143325641,-0.939692620785918,0.));
#73199=DIRECTION('',(-0.342020143325641,-0.939692620785918,0.));
#73200=DIRECTION('',(-0.342020143325641,-0.939692620785918,0.));
#73201=DIRECTION('',(0.,0.,1.));
#73202=DIRECTION('center_axis',(0.,1.,0.));
#73203=DIRECTION('ref_axis',(-1.,0.,0.));
#73204=DIRECTION('',(-1.,0.,0.));
#73205=DIRECTION('',(-1.,0.,0.));
#73206=DIRECTION('',(0.,0.,1.));
#73207=DIRECTION('center_axis',(0.939692620785909,0.342020143325668,0.));
#73208=DIRECTION('ref_axis',(-0.342020143325668,0.939692620785909,0.));
#73209=DIRECTION('',(-0.342020143325668,0.939692620785909,0.));
#73210=DIRECTION('',(-0.342020143325668,0.939692620785909,0.));
#73211=DIRECTION('',(0.,0.,1.));
#73212=DIRECTION('center_axis',(0.,1.,0.));
#73213=DIRECTION('ref_axis',(-1.,0.,0.));
#73214=DIRECTION('',(-1.,0.,0.));
#73215=DIRECTION('',(-1.,0.,0.));
#73216=DIRECTION('',(0.,0.,1.));
#73217=DIRECTION('center_axis',(-0.939692620785909,0.342020143325668,0.));
#73218=DIRECTION('ref_axis',(-0.342020143325668,-0.939692620785909,0.));
#73219=DIRECTION('',(-0.342020143325668,-0.939692620785909,0.));
#73220=DIRECTION('',(-0.342020143325668,-0.939692620785909,0.));
#73221=DIRECTION('',(0.,0.,1.));
#73222=DIRECTION('center_axis',(0.,1.,0.));
#73223=DIRECTION('ref_axis',(-1.,0.,0.));
#73224=DIRECTION('',(-1.,0.,0.));
#73225=DIRECTION('',(-1.,0.,0.));
#73226=DIRECTION('',(0.,0.,1.));
#73227=DIRECTION('center_axis',(0.939692620785909,0.342020143325668,0.));
#73228=DIRECTION('ref_axis',(-0.342020143325668,0.939692620785909,0.));
#73229=DIRECTION('',(-0.342020143325668,0.939692620785909,0.));
#73230=DIRECTION('',(-0.342020143325668,0.939692620785909,0.));
#73231=DIRECTION('',(0.,0.,1.));
#73232=DIRECTION('center_axis',(0.,1.,0.));
#73233=DIRECTION('ref_axis',(-1.,0.,0.));
#73234=DIRECTION('',(-1.,0.,0.));
#73235=DIRECTION('',(-1.,0.,0.));
#73236=DIRECTION('',(0.,0.,1.));
#73237=DIRECTION('center_axis',(-0.939692620785919,0.342020143325641,0.));
#73238=DIRECTION('ref_axis',(-0.342020143325641,-0.939692620785918,0.));
#73239=DIRECTION('',(-0.342020143325641,-0.939692620785918,0.));
#73240=DIRECTION('',(-0.342020143325641,-0.939692620785918,0.));
#73241=DIRECTION('',(0.,0.,1.));
#73242=DIRECTION('center_axis',(0.,1.,0.));
#73243=DIRECTION('ref_axis',(-1.,0.,0.));
#73244=DIRECTION('',(-1.,0.,0.));
#73245=DIRECTION('',(-1.,0.,0.));
#73246=DIRECTION('',(0.,0.,1.));
#73247=DIRECTION('center_axis',(0.939692620785909,0.342020143325668,0.));
#73248=DIRECTION('ref_axis',(-0.342020143325668,0.939692620785909,0.));
#73249=DIRECTION('',(-0.342020143325668,0.939692620785909,0.));
#73250=DIRECTION('',(-0.342020143325668,0.939692620785909,0.));
#73251=DIRECTION('',(0.,0.,1.));
#73252=DIRECTION('center_axis',(0.,1.,0.));
#73253=DIRECTION('ref_axis',(-1.,0.,0.));
#73254=DIRECTION('',(-1.,0.,0.));
#73255=DIRECTION('',(-1.,0.,0.));
#73256=DIRECTION('',(0.,0.,1.));
#73257=DIRECTION('center_axis',(-0.939692620785909,0.342020143325668,0.));
#73258=DIRECTION('ref_axis',(-0.342020143325668,-0.939692620785909,0.));
#73259=DIRECTION('',(-0.342020143325668,-0.939692620785909,0.));
#73260=DIRECTION('',(-0.342020143325668,-0.939692620785909,0.));
#73261=DIRECTION('',(0.,0.,1.));
#73262=DIRECTION('center_axis',(0.,1.,0.));
#73263=DIRECTION('ref_axis',(-1.,0.,0.));
#73264=DIRECTION('',(-1.,0.,0.));
#73265=DIRECTION('',(-1.,0.,0.));
#73266=DIRECTION('',(0.,0.,1.));
#73267=DIRECTION('center_axis',(0.939692620785919,0.342020143325641,0.));
#73268=DIRECTION('ref_axis',(-0.342020143325641,0.939692620785918,0.));
#73269=DIRECTION('',(-0.342020143325641,0.939692620785918,0.));
#73270=DIRECTION('',(-0.342020143325641,0.939692620785918,0.));
#73271=DIRECTION('',(0.,0.,1.));
#73272=DIRECTION('center_axis',(0.,1.,0.));
#73273=DIRECTION('ref_axis',(-1.,0.,0.));
#73274=DIRECTION('',(-1.,0.,0.));
#73275=DIRECTION('',(-1.,0.,0.));
#73276=DIRECTION('',(0.,0.,1.));
#73277=DIRECTION('center_axis',(-0.939692620785909,0.342020143325668,0.));
#73278=DIRECTION('ref_axis',(-0.342020143325668,-0.939692620785909,0.));
#73279=DIRECTION('',(-0.342020143325668,-0.939692620785909,0.));
#73280=DIRECTION('',(-0.342020143325668,-0.939692620785909,0.));
#73281=DIRECTION('',(0.,0.,1.));
#73282=DIRECTION('center_axis',(0.,1.,0.));
#73283=DIRECTION('ref_axis',(-1.,0.,0.));
#73284=DIRECTION('',(-1.,0.,0.));
#73285=DIRECTION('',(-1.,0.,0.));
#73286=DIRECTION('',(0.,0.,1.));
#73287=DIRECTION('center_axis',(0.939692620785909,0.342020143325668,0.));
#73288=DIRECTION('ref_axis',(-0.342020143325668,0.939692620785909,0.));
#73289=DIRECTION('',(-0.342020143325668,0.939692620785909,0.));
#73290=DIRECTION('',(-0.342020143325668,0.939692620785909,0.));
#73291=DIRECTION('',(0.,0.,1.));
#73292=DIRECTION('center_axis',(0.,1.,0.));
#73293=DIRECTION('ref_axis',(-1.,0.,0.));
#73294=DIRECTION('',(-1.,0.,0.));
#73295=DIRECTION('',(-1.,0.,0.));
#73296=DIRECTION('',(0.,0.,1.));
#73297=DIRECTION('center_axis',(-0.939692620785919,0.342020143325641,0.));
#73298=DIRECTION('ref_axis',(-0.342020143325641,-0.939692620785918,0.));
#73299=DIRECTION('',(-0.342020143325641,-0.939692620785918,0.));
#73300=DIRECTION('',(-0.342020143325641,-0.939692620785918,0.));
#73301=DIRECTION('',(0.,0.,1.));
#73302=DIRECTION('center_axis',(0.,1.,0.));
#73303=DIRECTION('ref_axis',(-1.,0.,0.));
#73304=DIRECTION('',(-1.,0.,0.));
#73305=DIRECTION('',(-1.,0.,0.));
#73306=DIRECTION('',(0.,0.,1.));
#73307=DIRECTION('center_axis',(0.939692620785919,0.342020143325641,0.));
#73308=DIRECTION('ref_axis',(-0.342020143325641,0.939692620785918,0.));
#73309=DIRECTION('',(-0.342020143325641,0.939692620785918,0.));
#73310=DIRECTION('',(-0.342020143325641,0.939692620785918,0.));
#73311=DIRECTION('',(0.,0.,1.));
#73312=DIRECTION('center_axis',(0.,1.,0.));
#73313=DIRECTION('ref_axis',(-1.,0.,0.));
#73314=DIRECTION('',(-1.,0.,0.));
#73315=DIRECTION('',(-1.,0.,0.));
#73316=DIRECTION('',(0.,0.,1.));
#73317=DIRECTION('center_axis',(-0.939692620785909,0.342020143325668,0.));
#73318=DIRECTION('ref_axis',(-0.342020143325668,-0.939692620785909,0.));
#73319=DIRECTION('',(-0.342020143325668,-0.939692620785909,0.));
#73320=DIRECTION('',(-0.342020143325668,-0.939692620785909,0.));
#73321=DIRECTION('',(0.,0.,1.));
#73322=DIRECTION('center_axis',(0.,1.,0.));
#73323=DIRECTION('ref_axis',(-1.,0.,0.));
#73324=DIRECTION('',(-1.,0.,0.));
#73325=DIRECTION('',(-1.,0.,0.));
#73326=DIRECTION('',(0.,0.,1.));
#73327=DIRECTION('center_axis',(0.939692620785909,0.342020143325668,0.));
#73328=DIRECTION('ref_axis',(-0.342020143325668,0.939692620785909,0.));
#73329=DIRECTION('',(-0.342020143325668,0.939692620785909,0.));
#73330=DIRECTION('',(-0.342020143325668,0.939692620785909,0.));
#73331=DIRECTION('',(0.,0.,1.));
#73332=DIRECTION('center_axis',(0.,1.,0.));
#73333=DIRECTION('ref_axis',(-1.,0.,0.));
#73334=DIRECTION('',(-1.,0.,0.));
#73335=DIRECTION('',(-1.,0.,0.));
#73336=DIRECTION('',(0.,0.,1.));
#73337=DIRECTION('center_axis',(-0.939692620785919,0.342020143325641,0.));
#73338=DIRECTION('ref_axis',(-0.342020143325641,-0.939692620785918,0.));
#73339=DIRECTION('',(-0.342020143325641,-0.939692620785918,0.));
#73340=DIRECTION('',(-0.342020143325641,-0.939692620785918,0.));
#73341=DIRECTION('',(0.,0.,1.));
#73342=DIRECTION('center_axis',(0.,1.,0.));
#73343=DIRECTION('ref_axis',(-1.,0.,0.));
#73344=DIRECTION('',(-1.,0.,0.));
#73345=DIRECTION('',(-1.,0.,0.));
#73346=DIRECTION('',(0.,0.,1.));
#73347=DIRECTION('center_axis',(0.939692620785909,0.342020143325668,0.));
#73348=DIRECTION('ref_axis',(-0.342020143325668,0.939692620785909,0.));
#73349=DIRECTION('',(-0.342020143325668,0.939692620785909,0.));
#73350=DIRECTION('',(-0.342020143325668,0.939692620785909,0.));
#73351=DIRECTION('',(0.,0.,1.));
#73352=DIRECTION('center_axis',(0.,1.,0.));
#73353=DIRECTION('ref_axis',(-1.,0.,0.));
#73354=DIRECTION('',(-1.,0.,0.));
#73355=DIRECTION('',(-1.,0.,0.));
#73356=DIRECTION('',(0.,0.,1.));
#73357=DIRECTION('center_axis',(-0.939692620785909,0.342020143325668,0.));
#73358=DIRECTION('ref_axis',(-0.342020143325668,-0.939692620785909,0.));
#73359=DIRECTION('',(-0.342020143325668,-0.939692620785909,0.));
#73360=DIRECTION('',(-0.342020143325668,-0.939692620785909,0.));
#73361=DIRECTION('',(0.,0.,1.));
#73362=DIRECTION('center_axis',(0.,1.,0.));
#73363=DIRECTION('ref_axis',(-1.,0.,0.));
#73364=DIRECTION('',(-1.,0.,0.));
#73365=DIRECTION('',(-1.,0.,0.));
#73366=DIRECTION('',(0.,0.,1.));
#73367=DIRECTION('center_axis',(0.939692620785909,0.342020143325668,0.));
#73368=DIRECTION('ref_axis',(-0.342020143325668,0.939692620785909,0.));
#73369=DIRECTION('',(-0.342020143325668,0.939692620785909,0.));
#73370=DIRECTION('',(-0.342020143325668,0.939692620785909,0.));
#73371=DIRECTION('',(0.,0.,1.));
#73372=DIRECTION('center_axis',(0.,1.,0.));
#73373=DIRECTION('ref_axis',(-1.,0.,0.));
#73374=DIRECTION('',(-1.,0.,0.));
#73375=DIRECTION('',(-1.,0.,0.));
#73376=DIRECTION('',(0.,0.,1.));
#73377=DIRECTION('center_axis',(-0.939692620785919,0.342020143325641,0.));
#73378=DIRECTION('ref_axis',(-0.342020143325641,-0.939692620785918,0.));
#73379=DIRECTION('',(-0.342020143325641,-0.939692620785918,0.));
#73380=DIRECTION('',(-0.342020143325641,-0.939692620785918,0.));
#73381=DIRECTION('',(0.,0.,1.));
#73382=DIRECTION('center_axis',(0.,1.,0.));
#73383=DIRECTION('ref_axis',(-1.,0.,0.));
#73384=DIRECTION('',(-1.,0.,0.));
#73385=DIRECTION('',(-1.,0.,0.));
#73386=DIRECTION('',(0.,0.,1.));
#73387=DIRECTION('center_axis',(0.939692620785909,0.342020143325668,0.));
#73388=DIRECTION('ref_axis',(-0.342020143325668,0.939692620785909,0.));
#73389=DIRECTION('',(-0.342020143325668,0.939692620785909,0.));
#73390=DIRECTION('',(-0.342020143325668,0.939692620785909,0.));
#73391=DIRECTION('',(0.,0.,1.));
#73392=DIRECTION('center_axis',(0.,1.,0.));
#73393=DIRECTION('ref_axis',(-1.,0.,0.));
#73394=DIRECTION('',(-1.,0.,0.));
#73395=DIRECTION('',(-1.,0.,0.));
#73396=DIRECTION('',(0.,0.,1.));
#73397=DIRECTION('center_axis',(-0.939692620785909,0.342020143325668,0.));
#73398=DIRECTION('ref_axis',(-0.342020143325668,-0.939692620785909,0.));
#73399=DIRECTION('',(-0.342020143325668,-0.939692620785909,0.));
#73400=DIRECTION('',(-0.342020143325668,-0.939692620785909,0.));
#73401=DIRECTION('',(0.,0.,1.));
#73402=DIRECTION('center_axis',(0.,1.,0.));
#73403=DIRECTION('ref_axis',(-1.,0.,0.));
#73404=DIRECTION('',(-1.,0.,0.));
#73405=DIRECTION('',(-1.,0.,0.));
#73406=DIRECTION('',(0.,0.,1.));
#73407=DIRECTION('center_axis',(0.939692620785919,0.342020143325641,0.));
#73408=DIRECTION('ref_axis',(-0.342020143325641,0.939692620785918,0.));
#73409=DIRECTION('',(-0.342020143325641,0.939692620785918,0.));
#73410=DIRECTION('',(-0.342020143325641,0.939692620785918,0.));
#73411=DIRECTION('',(0.,0.,1.));
#73412=DIRECTION('center_axis',(0.,1.,0.));
#73413=DIRECTION('ref_axis',(-1.,0.,0.));
#73414=DIRECTION('',(-1.,0.,0.));
#73415=DIRECTION('',(-1.,0.,0.));
#73416=DIRECTION('',(0.,0.,1.));
#73417=DIRECTION('center_axis',(-0.939692620785909,0.342020143325668,0.));
#73418=DIRECTION('ref_axis',(-0.342020143325668,-0.939692620785909,0.));
#73419=DIRECTION('',(-0.342020143325668,-0.939692620785909,0.));
#73420=DIRECTION('',(-0.342020143325668,-0.939692620785909,0.));
#73421=DIRECTION('',(0.,0.,1.));
#73422=DIRECTION('center_axis',(0.,1.,0.));
#73423=DIRECTION('ref_axis',(-1.,0.,0.));
#73424=DIRECTION('',(-1.,0.,0.));
#73425=DIRECTION('',(-1.,0.,0.));
#73426=DIRECTION('',(0.,0.,1.));
#73427=DIRECTION('center_axis',(0.939692620785909,0.342020143325668,0.));
#73428=DIRECTION('ref_axis',(-0.342020143325668,0.939692620785909,0.));
#73429=DIRECTION('',(-0.342020143325668,0.939692620785909,0.));
#73430=DIRECTION('',(-0.342020143325668,0.939692620785909,0.));
#73431=DIRECTION('',(0.,0.,1.));
#73432=DIRECTION('center_axis',(0.,1.,0.));
#73433=DIRECTION('ref_axis',(-1.,0.,0.));
#73434=DIRECTION('',(-1.,0.,0.));
#73435=DIRECTION('',(-1.,0.,0.));
#73436=DIRECTION('',(0.,0.,1.));
#73437=DIRECTION('center_axis',(-0.939692620785909,0.342020143325668,0.));
#73438=DIRECTION('ref_axis',(-0.342020143325668,-0.939692620785909,0.));
#73439=DIRECTION('',(-0.342020143325668,-0.939692620785909,0.));
#73440=DIRECTION('',(-0.342020143325668,-0.939692620785909,0.));
#73441=DIRECTION('',(0.,0.,1.));
#73442=DIRECTION('center_axis',(0.,1.,0.));
#73443=DIRECTION('ref_axis',(-1.,0.,0.));
#73444=DIRECTION('',(-1.,0.,0.));
#73445=DIRECTION('',(-1.,0.,0.));
#73446=DIRECTION('',(0.,0.,1.));
#73447=DIRECTION('center_axis',(0.939692620785919,0.342020143325641,0.));
#73448=DIRECTION('ref_axis',(-0.342020143325641,0.939692620785918,0.));
#73449=DIRECTION('',(-0.342020143325641,0.939692620785918,0.));
#73450=DIRECTION('',(-0.342020143325641,0.939692620785918,0.));
#73451=DIRECTION('',(0.,0.,1.));
#73452=DIRECTION('center_axis',(0.,1.,0.));
#73453=DIRECTION('ref_axis',(-1.,0.,0.));
#73454=DIRECTION('',(-1.,0.,0.));
#73455=DIRECTION('',(-1.,0.,0.));
#73456=DIRECTION('',(0.,0.,1.));
#73457=DIRECTION('center_axis',(-0.939692620785909,0.342020143325668,0.));
#73458=DIRECTION('ref_axis',(-0.342020143325668,-0.939692620785909,0.));
#73459=DIRECTION('',(-0.342020143325668,-0.939692620785909,0.));
#73460=DIRECTION('',(-0.342020143325668,-0.939692620785909,0.));
#73461=DIRECTION('',(0.,0.,1.));
#73462=DIRECTION('center_axis',(0.,1.,0.));
#73463=DIRECTION('ref_axis',(-1.,0.,0.));
#73464=DIRECTION('',(-1.,0.,0.));
#73465=DIRECTION('',(-1.,0.,0.));
#73466=DIRECTION('',(0.,0.,1.));
#73467=DIRECTION('center_axis',(0.939692620785909,0.342020143325668,0.));
#73468=DIRECTION('ref_axis',(-0.342020143325668,0.939692620785909,0.));
#73469=DIRECTION('',(-0.342020143325668,0.939692620785909,0.));
#73470=DIRECTION('',(-0.342020143325668,0.939692620785909,0.));
#73471=DIRECTION('',(0.,0.,1.));
#73472=DIRECTION('center_axis',(0.,1.,0.));
#73473=DIRECTION('ref_axis',(-1.,0.,0.));
#73474=DIRECTION('',(-1.,0.,0.));
#73475=DIRECTION('',(-1.,0.,0.));
#73476=DIRECTION('',(0.,0.,1.));
#73477=DIRECTION('center_axis',(-0.939692620785919,0.342020143325641,0.));
#73478=DIRECTION('ref_axis',(-0.342020143325641,-0.939692620785918,0.));
#73479=DIRECTION('',(-0.342020143325641,-0.939692620785918,0.));
#73480=DIRECTION('',(-0.342020143325641,-0.939692620785918,0.));
#73481=DIRECTION('',(0.,0.,1.));
#73482=DIRECTION('center_axis',(0.,1.,0.));
#73483=DIRECTION('ref_axis',(-1.,0.,0.));
#73484=DIRECTION('',(-1.,0.,0.));
#73485=DIRECTION('',(-1.,0.,0.));
#73486=DIRECTION('',(0.,0.,1.));
#73487=DIRECTION('center_axis',(0.939692620785919,0.342020143325641,0.));
#73488=DIRECTION('ref_axis',(-0.342020143325641,0.939692620785918,0.));
#73489=DIRECTION('',(-0.342020143325641,0.939692620785918,0.));
#73490=DIRECTION('',(-0.342020143325641,0.939692620785918,0.));
#73491=DIRECTION('',(0.,0.,1.));
#73492=DIRECTION('center_axis',(0.,1.,0.));
#73493=DIRECTION('ref_axis',(-1.,0.,0.));
#73494=DIRECTION('',(-1.,0.,0.));
#73495=DIRECTION('',(-1.,0.,0.));
#73496=DIRECTION('',(0.,0.,1.));
#73497=DIRECTION('center_axis',(-0.939692620785909,0.342020143325668,0.));
#73498=DIRECTION('ref_axis',(-0.342020143325668,-0.939692620785909,0.));
#73499=DIRECTION('',(-0.342020143325668,-0.939692620785909,0.));
#73500=DIRECTION('',(-0.342020143325668,-0.939692620785909,0.));
#73501=DIRECTION('',(0.,0.,1.));
#73502=DIRECTION('center_axis',(0.,1.,0.));
#73503=DIRECTION('ref_axis',(-1.,0.,0.));
#73504=DIRECTION('',(-1.,0.,0.));
#73505=DIRECTION('',(-1.,0.,0.));
#73506=DIRECTION('',(0.,0.,1.));
#73507=DIRECTION('center_axis',(0.939692620785909,0.342020143325668,0.));
#73508=DIRECTION('ref_axis',(-0.342020143325668,0.939692620785909,0.));
#73509=DIRECTION('',(-0.342020143325668,0.939692620785909,0.));
#73510=DIRECTION('',(-0.342020143325668,0.939692620785909,0.));
#73511=DIRECTION('',(0.,0.,1.));
#73512=DIRECTION('center_axis',(0.,1.,0.));
#73513=DIRECTION('ref_axis',(-1.,0.,0.));
#73514=DIRECTION('',(-1.,0.,0.));
#73515=DIRECTION('',(-1.,0.,0.));
#73516=DIRECTION('',(0.,0.,1.));
#73517=DIRECTION('center_axis',(-0.939692620785919,0.342020143325641,0.));
#73518=DIRECTION('ref_axis',(-0.342020143325641,-0.939692620785918,0.));
#73519=DIRECTION('',(-0.342020143325641,-0.939692620785918,0.));
#73520=DIRECTION('',(-0.342020143325641,-0.939692620785918,0.));
#73521=DIRECTION('',(0.,0.,1.));
#73522=DIRECTION('center_axis',(0.,1.,0.));
#73523=DIRECTION('ref_axis',(-1.,0.,0.));
#73524=DIRECTION('',(-1.,0.,0.));
#73525=DIRECTION('',(-1.,0.,0.));
#73526=DIRECTION('',(0.,0.,1.));
#73527=DIRECTION('center_axis',(0.939692620785909,0.342020143325668,0.));
#73528=DIRECTION('ref_axis',(-0.342020143325668,0.939692620785909,0.));
#73529=DIRECTION('',(-0.342020143325668,0.939692620785909,0.));
#73530=DIRECTION('',(-0.342020143325668,0.939692620785909,0.));
#73531=DIRECTION('',(0.,0.,1.));
#73532=DIRECTION('center_axis',(0.,1.,0.));
#73533=DIRECTION('ref_axis',(-1.,0.,0.));
#73534=DIRECTION('',(-1.,0.,0.));
#73535=DIRECTION('',(-1.,0.,0.));
#73536=DIRECTION('',(0.,0.,1.));
#73537=DIRECTION('center_axis',(-0.939692620785909,0.342020143325668,0.));
#73538=DIRECTION('ref_axis',(-0.342020143325668,-0.939692620785909,0.));
#73539=DIRECTION('',(-0.342020143325668,-0.939692620785909,0.));
#73540=DIRECTION('',(-0.342020143325668,-0.939692620785909,0.));
#73541=DIRECTION('',(0.,0.,1.));
#73542=DIRECTION('center_axis',(0.,1.,0.));
#73543=DIRECTION('ref_axis',(-1.,0.,0.));
#73544=DIRECTION('',(-1.,0.,0.));
#73545=DIRECTION('',(-1.,0.,0.));
#73546=DIRECTION('',(0.,0.,1.));
#73547=DIRECTION('center_axis',(0.939692620785919,0.342020143325641,0.));
#73548=DIRECTION('ref_axis',(-0.342020143325641,0.939692620785918,0.));
#73549=DIRECTION('',(-0.342020143325641,0.939692620785918,0.));
#73550=DIRECTION('',(-0.342020143325641,0.939692620785918,0.));
#73551=DIRECTION('',(0.,0.,1.));
#73552=DIRECTION('center_axis',(0.,1.,0.));
#73553=DIRECTION('ref_axis',(-1.,0.,0.));
#73554=DIRECTION('',(-1.,0.,0.));
#73555=DIRECTION('',(-1.,0.,0.));
#73556=DIRECTION('',(0.,0.,1.));
#73557=DIRECTION('center_axis',(-0.939692620785909,0.342020143325668,0.));
#73558=DIRECTION('ref_axis',(-0.342020143325668,-0.939692620785909,0.));
#73559=DIRECTION('',(-0.342020143325668,-0.939692620785909,0.));
#73560=DIRECTION('',(-0.342020143325668,-0.939692620785909,0.));
#73561=DIRECTION('',(0.,0.,1.));
#73562=DIRECTION('center_axis',(0.,1.,0.));
#73563=DIRECTION('ref_axis',(-1.,0.,0.));
#73564=DIRECTION('',(-1.,0.,0.));
#73565=DIRECTION('',(-1.,0.,0.));
#73566=DIRECTION('',(0.,0.,1.));
#73567=DIRECTION('center_axis',(0.939692620785909,0.342020143325668,0.));
#73568=DIRECTION('ref_axis',(-0.342020143325668,0.939692620785909,0.));
#73569=DIRECTION('',(-0.342020143325668,0.939692620785909,0.));
#73570=DIRECTION('',(-0.342020143325668,0.939692620785909,0.));
#73571=DIRECTION('',(0.,0.,1.));
#73572=DIRECTION('center_axis',(0.,1.,0.));
#73573=DIRECTION('ref_axis',(-1.,0.,0.));
#73574=DIRECTION('',(-1.,0.,0.));
#73575=DIRECTION('',(-1.,0.,0.));
#73576=DIRECTION('',(0.,0.,1.));
#73577=DIRECTION('center_axis',(-0.939692620785919,0.342020143325641,0.));
#73578=DIRECTION('ref_axis',(-0.342020143325641,-0.939692620785918,0.));
#73579=DIRECTION('',(-0.342020143325641,-0.939692620785918,0.));
#73580=DIRECTION('',(-0.342020143325641,-0.939692620785918,0.));
#73581=DIRECTION('',(0.,0.,1.));
#73582=DIRECTION('center_axis',(0.,1.,0.));
#73583=DIRECTION('ref_axis',(-1.,0.,0.));
#73584=DIRECTION('',(-1.,0.,0.));
#73585=DIRECTION('',(-1.,0.,0.));
#73586=DIRECTION('',(0.,0.,1.));
#73587=DIRECTION('center_axis',(0.939692620785919,0.342020143325641,0.));
#73588=DIRECTION('ref_axis',(-0.342020143325641,0.939692620785918,0.));
#73589=DIRECTION('',(-0.342020143325641,0.939692620785918,0.));
#73590=DIRECTION('',(-0.342020143325641,0.939692620785918,0.));
#73591=DIRECTION('',(0.,0.,1.));
#73592=DIRECTION('center_axis',(0.,1.,0.));
#73593=DIRECTION('ref_axis',(-1.,0.,0.));
#73594=DIRECTION('',(-1.,0.,0.));
#73595=DIRECTION('',(-1.,0.,0.));
#73596=DIRECTION('',(0.,0.,1.));
#73597=DIRECTION('center_axis',(-0.939692620785909,0.342020143325668,0.));
#73598=DIRECTION('ref_axis',(-0.342020143325668,-0.939692620785909,0.));
#73599=DIRECTION('',(-0.342020143325668,-0.939692620785909,0.));
#73600=DIRECTION('',(-0.342020143325668,-0.939692620785909,0.));
#73601=DIRECTION('',(0.,0.,1.));
#73602=DIRECTION('center_axis',(0.,1.,0.));
#73603=DIRECTION('ref_axis',(-1.,0.,0.));
#73604=DIRECTION('',(-1.,0.,0.));
#73605=DIRECTION('',(-1.,0.,0.));
#73606=DIRECTION('',(0.,0.,1.));
#73607=DIRECTION('center_axis',(0.939692620785909,0.342020143325668,0.));
#73608=DIRECTION('ref_axis',(-0.342020143325668,0.939692620785909,0.));
#73609=DIRECTION('',(-0.342020143325668,0.939692620785909,0.));
#73610=DIRECTION('',(-0.342020143325668,0.939692620785909,0.));
#73611=DIRECTION('',(0.,0.,1.));
#73612=DIRECTION('center_axis',(0.,1.,0.));
#73613=DIRECTION('ref_axis',(-1.,0.,0.));
#73614=DIRECTION('',(-1.,0.,0.));
#73615=DIRECTION('',(-1.,0.,0.));
#73616=DIRECTION('',(0.,0.,1.));
#73617=DIRECTION('center_axis',(-0.939692620785919,0.342020143325641,0.));
#73618=DIRECTION('ref_axis',(-0.342020143325641,-0.939692620785918,0.));
#73619=DIRECTION('',(-0.342020143325641,-0.939692620785918,0.));
#73620=DIRECTION('',(-0.342020143325641,-0.939692620785918,0.));
#73621=DIRECTION('',(0.,0.,1.));
#73622=DIRECTION('center_axis',(0.,1.,0.));
#73623=DIRECTION('ref_axis',(-1.,0.,0.));
#73624=DIRECTION('',(-1.,0.,0.));
#73625=DIRECTION('',(-1.,0.,0.));
#73626=DIRECTION('',(0.,0.,1.));
#73627=DIRECTION('center_axis',(0.939692620785919,0.342020143325641,0.));
#73628=DIRECTION('ref_axis',(-0.342020143325641,0.939692620785918,0.));
#73629=DIRECTION('',(-0.342020143325641,0.939692620785918,0.));
#73630=DIRECTION('',(-0.342020143325641,0.939692620785918,0.));
#73631=DIRECTION('',(0.,0.,1.));
#73632=DIRECTION('center_axis',(0.,1.,0.));
#73633=DIRECTION('ref_axis',(-1.,0.,0.));
#73634=DIRECTION('',(-1.,0.,0.));
#73635=DIRECTION('',(-1.,0.,0.));
#73636=DIRECTION('',(0.,0.,1.));
#73637=DIRECTION('center_axis',(-0.939692620785909,0.342020143325668,0.));
#73638=DIRECTION('ref_axis',(-0.342020143325668,-0.939692620785909,0.));
#73639=DIRECTION('',(-0.342020143325668,-0.939692620785909,0.));
#73640=DIRECTION('',(-0.342020143325668,-0.939692620785909,0.));
#73641=DIRECTION('',(0.,0.,1.));
#73642=DIRECTION('center_axis',(0.,1.,0.));
#73643=DIRECTION('ref_axis',(-1.,0.,0.));
#73644=DIRECTION('',(-1.,0.,0.));
#73645=DIRECTION('',(-1.,0.,0.));
#73646=DIRECTION('',(0.,0.,1.));
#73647=DIRECTION('center_axis',(0.939692620785909,0.342020143325668,0.));
#73648=DIRECTION('ref_axis',(-0.342020143325668,0.939692620785909,0.));
#73649=DIRECTION('',(-0.342020143325668,0.939692620785909,0.));
#73650=DIRECTION('',(-0.342020143325668,0.939692620785909,0.));
#73651=DIRECTION('',(0.,0.,1.));
#73652=DIRECTION('center_axis',(0.,1.,0.));
#73653=DIRECTION('ref_axis',(-1.,0.,0.));
#73654=DIRECTION('',(-1.,0.,0.));
#73655=DIRECTION('',(-1.,0.,0.));
#73656=DIRECTION('',(0.,0.,1.));
#73657=DIRECTION('center_axis',(-0.939692620785919,0.342020143325641,0.));
#73658=DIRECTION('ref_axis',(-0.342020143325641,-0.939692620785918,0.));
#73659=DIRECTION('',(-0.342020143325641,-0.939692620785918,0.));
#73660=DIRECTION('',(-0.342020143325641,-0.939692620785918,0.));
#73661=DIRECTION('',(0.,0.,1.));
#73662=DIRECTION('center_axis',(0.,1.,0.));
#73663=DIRECTION('ref_axis',(-1.,0.,0.));
#73664=DIRECTION('',(-1.,0.,0.));
#73665=DIRECTION('',(-1.,0.,0.));
#73666=DIRECTION('',(0.,0.,1.));
#73667=DIRECTION('center_axis',(0.939692620785919,0.342020143325641,0.));
#73668=DIRECTION('ref_axis',(-0.342020143325641,0.939692620785918,0.));
#73669=DIRECTION('',(-0.342020143325641,0.939692620785918,0.));
#73670=DIRECTION('',(-0.342020143325641,0.939692620785918,0.));
#73671=DIRECTION('',(0.,0.,1.));
#73672=DIRECTION('center_axis',(0.,1.,0.));
#73673=DIRECTION('ref_axis',(-1.,0.,0.));
#73674=DIRECTION('',(-1.,0.,0.));
#73675=DIRECTION('',(-1.,0.,0.));
#73676=DIRECTION('',(0.,0.,1.));
#73677=DIRECTION('center_axis',(-0.939692620785909,0.342020143325668,0.));
#73678=DIRECTION('ref_axis',(-0.342020143325668,-0.939692620785909,0.));
#73679=DIRECTION('',(-0.342020143325668,-0.939692620785909,0.));
#73680=DIRECTION('',(-0.342020143325668,-0.939692620785909,0.));
#73681=DIRECTION('center_axis',(-1.,0.,0.));
#73682=DIRECTION('ref_axis',(0.,-1.,0.));
#73683=DIRECTION('',(0.,-1.,0.));
#73684=DIRECTION('',(0.,-1.,0.));
#73685=DIRECTION('center_axis',(0.,0.,1.));
#73686=DIRECTION('ref_axis',(1.,0.,0.));
#73687=DIRECTION('center_axis',(0.,0.,1.));
#73688=DIRECTION('ref_axis',(1.,0.,0.));
#73689=DIRECTION('axis',(0.,0.,1.));
#73690=DIRECTION('refdir',(1.,0.,0.));
#73691=DIRECTION('center_axis',(0.,0.,1.));
#73692=DIRECTION('ref_axis',(-0.0793928204885979,0.996843407990877,0.));
#73693=DIRECTION('center_axis',(0.,0.,-1.));
#73694=DIRECTION('ref_axis',(-0.0793928204885979,0.996843407990877,0.));
#73695=DIRECTION('',(0.,0.,1.));
#73696=DIRECTION('center_axis',(0.,0.,1.));
#73697=DIRECTION('ref_axis',(-0.0793928204885979,0.996843407990877,0.));
#73698=DIRECTION('',(0.,0.,-1.));
#73699=DIRECTION('center_axis',(0.,0.,1.));
#73700=DIRECTION('ref_axis',(1.,0.,0.));
#73701=DIRECTION('center_axis',(0.,0.,1.));
#73702=DIRECTION('ref_axis',(1.,0.,0.));
#73703=DIRECTION('',(0.,0.,-1.));
#73704=DIRECTION('center_axis',(0.,0.,1.));
#73705=DIRECTION('ref_axis',(1.,0.,0.));
#73706=DIRECTION('center_axis',(0.,0.,1.));
#73707=DIRECTION('ref_axis',(0.868164295052897,-0.496276895286599,0.));
#73708=DIRECTION('center_axis',(0.,0.,-1.));
#73709=DIRECTION('ref_axis',(0.868164295052897,-0.496276895286599,0.));
#73710=DIRECTION('',(0.,0.,1.));
#73711=DIRECTION('center_axis',(0.,0.,1.));
#73712=DIRECTION('ref_axis',(0.868164295052897,-0.496276895286599,0.));
#73713=DIRECTION('center_axis',(-0.535824439731477,0.844329420182933,0.));
#73714=DIRECTION('ref_axis',(-0.844329420182933,-0.535824439731477,0.));
#73715=DIRECTION('',(0.844329420182933,0.535824439731477,0.));
#73716=DIRECTION('',(0.,0.,1.));
#73717=DIRECTION('',(-0.612832075974817,-0.388912663599404,-0.687883556096824));
#73718=DIRECTION('',(0.,0.,-1.));
#73719=DIRECTION('',(-0.844329420182933,-0.535824439731477,0.));
#73720=DIRECTION('center_axis',(0.,0.,1.));
#73721=DIRECTION('ref_axis',(-0.975916153426266,0.21814596370706,0.));
#73722=DIRECTION('center_axis',(0.,0.,-1.));
#73723=DIRECTION('ref_axis',(-0.975916153426266,0.21814596370706,0.));
#73724=DIRECTION('center_axis',(0.746665039101869,0.,-0.665200209999218));
#73725=DIRECTION('ref_axis',(-0.665200209999218,0.,-0.746665039101869));
#73726=DIRECTION('',(0.,0.,1.));
#73727=DIRECTION('center_axis',(-0.844329420182933,-0.535824439731478,0.));
#73728=DIRECTION('ref_axis',(0.535824439731478,-0.844329420182933,0.));
#73729=DIRECTION('',(0.459172673933159,-0.723544819531037,0.51540600466319));
#73730=DIRECTION('',(-0.535824439731478,0.844329420182933,0.));
#73731=DIRECTION('',(0.,0.,-1.));
#73732=DIRECTION('center_axis',(-0.844329420182933,-0.535824439731478,0.));
#73733=DIRECTION('ref_axis',(0.535824439731478,-0.844329420182933,0.));
#73734=DIRECTION('',(0.459172673933159,-0.723544819531037,0.51540600466319));
#73735=DIRECTION('',(0.483554359415822,-0.76196444514008,-0.43079619988148));
#73736=DIRECTION('',(-0.459172673933159,0.723544819531037,-0.51540600466319));
#73737=DIRECTION('',(-0.535824439731478,0.844329420182933,0.));
#73738=DIRECTION('',(0.,0.,-1.));
#73739=DIRECTION('',(0.535824439731478,-0.844329420182933,0.));
#73740=DIRECTION('center_axis',(0.,0.,1.));
#73741=DIRECTION('ref_axis',(-0.218145963707059,-0.975916153426266,0.));
#73742=DIRECTION('center_axis',(0.,0.,-1.));
#73743=DIRECTION('ref_axis',(-0.218145963707059,-0.975916153426266,0.));
#73744=DIRECTION('center_axis',(0.,0.,1.));
#73745=DIRECTION('ref_axis',(-0.218145963707059,-0.975916153426266,0.));
#73746=DIRECTION('',(0.,0.,1.));
#73747=DIRECTION('center_axis',(0.,0.,1.));
#73748=DIRECTION('ref_axis',(1.,0.,0.));
#73749=DIRECTION('',(0.,1.,0.));
#73750=DIRECTION('',(-1.,0.,0.));
#73751=DIRECTION('center_axis',(0.,0.,-1.));
#73752=DIRECTION('ref_axis',(0.876306008119143,-0.481754896326226,0.));
#73753=DIRECTION('',(-0.844329420182934,-0.535824439731477,0.));
#73754=DIRECTION('center_axis',(0.,0.,1.));
#73755=DIRECTION('ref_axis',(1.,0.,0.));
#73756=DIRECTION('center_axis',(0.,0.,1.));
#73757=DIRECTION('ref_axis',(0.876306008119143,-0.481754896326226,0.));
#73758=DIRECTION('center_axis',(-0.746665039101869,0.,0.665200209999218));
#73759=DIRECTION('ref_axis',(0.665200209999218,0.,0.746665039101869));
#73760=DIRECTION('',(0.,0.,1.));
#73761=DIRECTION('center_axis',(0.746665039101869,0.,-0.665200209999218));
#73762=DIRECTION('ref_axis',(0.665200209999218,0.,0.746665039101869));
#73763=DIRECTION('',(0.,-1.,0.));
#73764=DIRECTION('',(0.665200209999218,0.,0.746665039101869));
#73765=DIRECTION('',(0.,-1.,0.));
#73766=DIRECTION('',(-0.665200209999218,0.,-0.746665039101869));
#73767=DIRECTION('center_axis',(0.665200209999218,0.,0.746665039101869));
#73768=DIRECTION('ref_axis',(-0.746665039101869,0.,0.665200209999218));
#73769=DIRECTION('',(0.,-1.,0.));
#73770=DIRECTION('',(-0.746665039101869,0.,0.665200209999218));
#73771=DIRECTION('center_axis',(-0.746665039101869,0.,0.665200209999218));
#73772=DIRECTION('ref_axis',(-0.665200209999218,0.,-0.746665039101869));
#73773=DIRECTION('',(0.665200209999218,0.,0.746665039101869));
#73774=DIRECTION('',(0.,-1.,0.));
#73775=DIRECTION('',(-0.665200209999218,0.,-0.746665039101869));
#73776=DIRECTION('center_axis',(-0.665200209999218,0.,-0.74666503910187));
#73777=DIRECTION('ref_axis',(0.74666503910187,0.,-0.665200209999218));
#73778=DIRECTION('',(-0.74666503910187,0.,0.665200209999218));
#73779=DIRECTION('',(0.74666503910187,0.,-0.665200209999218));
#73780=DIRECTION('center_axis',(0.,1.,0.));
#73781=DIRECTION('ref_axis',(1.,0.,0.));
#73782=DIRECTION('center_axis',(0.,-1.,0.));
#73783=DIRECTION('ref_axis',(0.,0.,-1.));
#73784=DIRECTION('center_axis',(0.,0.,1.));
#73785=DIRECTION('ref_axis',(1.,0.,0.));
#73786=DIRECTION('',(0.,0.,1.));
#73787=DIRECTION('center_axis',(0.,0.,-1.));
#73788=DIRECTION('ref_axis',(1.,0.,0.));
#73789=DIRECTION('center_axis',(0.535824439731477,-0.844329420182934,0.));
#73790=DIRECTION('ref_axis',(0.844329420182934,0.535824439731477,0.));
#73791=DIRECTION('',(0.844329420182934,0.535824439731477,0.));
#73792=DIRECTION('center_axis',(0.,0.,1.));
#73793=DIRECTION('ref_axis',(1.,0.,0.));
#73794=DIRECTION('axis',(0.,0.,1.));
#73795=DIRECTION('refdir',(1.,0.,0.));
#73796=DIRECTION('center_axis',(1.,0.,0.));
#73797=DIRECTION('ref_axis',(0.,-1.,0.));
#73798=DIRECTION('',(0.,0.,-1.));
#73799=DIRECTION('',(0.,-1.,0.));
#73800=DIRECTION('',(0.,0.,-1.));
#73801=DIRECTION('',(0.,-1.,0.));
#73802=DIRECTION('center_axis',(0.,0.,-1.));
#73803=DIRECTION('ref_axis',(-1.,0.,0.));
#73804=DIRECTION('',(-1.,0.,0.));
#73805=DIRECTION('',(1.,0.,0.));
#73806=DIRECTION('',(0.,1.,0.));
#73807=DIRECTION('center_axis',(0.,1.,0.));
#73808=DIRECTION('ref_axis',(1.,0.,0.));
#73809=DIRECTION('',(1.,0.,0.));
#73810=DIRECTION('',(0.,0.,-1.));
#73811=DIRECTION('center_axis',(-1.,0.,0.));
#73812=DIRECTION('ref_axis',(0.,1.,0.));
#73813=DIRECTION('',(0.,0.,1.));
#73814=DIRECTION('',(0.,1.,0.));
#73815=DIRECTION('center_axis',(1.,0.,0.));
#73816=DIRECTION('ref_axis',(0.,-1.,0.));
#73817=DIRECTION('',(0.,0.,-1.));
#73818=DIRECTION('',(0.,-1.,0.));
#73819=DIRECTION('',(0.,0.,-1.));
#73820=DIRECTION('',(0.,-1.,0.));
#73821=DIRECTION('center_axis',(0.,0.,-1.));
#73822=DIRECTION('ref_axis',(-1.,0.,0.));
#73823=DIRECTION('',(-1.,0.,0.));
#73824=DIRECTION('',(1.,0.,0.));
#73825=DIRECTION('',(0.,1.,0.));
#73826=DIRECTION('center_axis',(0.,1.,0.));
#73827=DIRECTION('ref_axis',(1.,0.,0.));
#73828=DIRECTION('',(1.,0.,0.));
#73829=DIRECTION('',(0.,0.,-1.));
#73830=DIRECTION('center_axis',(-1.,0.,0.));
#73831=DIRECTION('ref_axis',(0.,1.,0.));
#73832=DIRECTION('',(0.,0.,1.));
#73833=DIRECTION('',(0.,1.,0.));
#73834=DIRECTION('center_axis',(1.,0.,0.));
#73835=DIRECTION('ref_axis',(0.,-1.,0.));
#73836=DIRECTION('',(0.,0.,-1.));
#73837=DIRECTION('',(0.,-1.,0.));
#73838=DIRECTION('',(0.,0.,-1.));
#73839=DIRECTION('',(0.,-1.,0.));
#73840=DIRECTION('center_axis',(0.,0.,-1.));
#73841=DIRECTION('ref_axis',(-1.,0.,0.));
#73842=DIRECTION('',(-1.,0.,0.));
#73843=DIRECTION('',(1.,0.,0.));
#73844=DIRECTION('',(0.,1.,0.));
#73845=DIRECTION('center_axis',(0.,1.,0.));
#73846=DIRECTION('ref_axis',(1.,0.,0.));
#73847=DIRECTION('',(1.,0.,0.));
#73848=DIRECTION('',(0.,0.,-1.));
#73849=DIRECTION('center_axis',(-1.,0.,0.));
#73850=DIRECTION('ref_axis',(0.,1.,0.));
#73851=DIRECTION('',(0.,0.,1.));
#73852=DIRECTION('',(0.,1.,0.));
#73853=DIRECTION('center_axis',(1.,0.,0.));
#73854=DIRECTION('ref_axis',(0.,-1.,0.));
#73855=DIRECTION('',(0.,0.,-1.));
#73856=DIRECTION('',(0.,-1.,0.));
#73857=DIRECTION('',(0.,0.,-1.));
#73858=DIRECTION('',(0.,-1.,0.));
#73859=DIRECTION('center_axis',(0.,0.,-1.));
#73860=DIRECTION('ref_axis',(-1.,0.,0.));
#73861=DIRECTION('',(-1.,0.,0.));
#73862=DIRECTION('',(1.,0.,0.));
#73863=DIRECTION('',(0.,1.,0.));
#73864=DIRECTION('center_axis',(0.,1.,0.));
#73865=DIRECTION('ref_axis',(1.,0.,0.));
#73866=DIRECTION('',(1.,0.,0.));
#73867=DIRECTION('',(0.,0.,-1.));
#73868=DIRECTION('center_axis',(-1.,0.,0.));
#73869=DIRECTION('ref_axis',(0.,1.,0.));
#73870=DIRECTION('',(0.,0.,1.));
#73871=DIRECTION('',(0.,1.,0.));
#73872=DIRECTION('center_axis',(1.,0.,0.));
#73873=DIRECTION('ref_axis',(0.,-1.,0.));
#73874=DIRECTION('',(0.,0.,-1.));
#73875=DIRECTION('',(0.,-1.,0.));
#73876=DIRECTION('',(0.,0.,-1.));
#73877=DIRECTION('',(0.,-1.,0.));
#73878=DIRECTION('center_axis',(0.,0.,-1.));
#73879=DIRECTION('ref_axis',(-1.,0.,0.));
#73880=DIRECTION('',(-1.,0.,0.));
#73881=DIRECTION('',(1.,0.,0.));
#73882=DIRECTION('',(0.,1.,0.));
#73883=DIRECTION('center_axis',(0.,1.,0.));
#73884=DIRECTION('ref_axis',(1.,0.,0.));
#73885=DIRECTION('',(1.,0.,0.));
#73886=DIRECTION('',(0.,0.,-1.));
#73887=DIRECTION('center_axis',(-1.,0.,0.));
#73888=DIRECTION('ref_axis',(0.,1.,0.));
#73889=DIRECTION('',(0.,0.,1.));
#73890=DIRECTION('',(0.,1.,0.));
#73891=DIRECTION('center_axis',(1.,0.,0.));
#73892=DIRECTION('ref_axis',(0.,-1.,0.));
#73893=DIRECTION('',(0.,0.,-1.));
#73894=DIRECTION('',(0.,-1.,0.));
#73895=DIRECTION('',(0.,0.,-1.));
#73896=DIRECTION('',(0.,-1.,0.));
#73897=DIRECTION('center_axis',(0.,0.,-1.));
#73898=DIRECTION('ref_axis',(-1.,0.,0.));
#73899=DIRECTION('',(-1.,0.,0.));
#73900=DIRECTION('',(1.,0.,0.));
#73901=DIRECTION('',(0.,1.,0.));
#73902=DIRECTION('center_axis',(0.,1.,0.));
#73903=DIRECTION('ref_axis',(1.,0.,0.));
#73904=DIRECTION('',(1.,0.,0.));
#73905=DIRECTION('',(0.,0.,-1.));
#73906=DIRECTION('center_axis',(-1.,0.,0.));
#73907=DIRECTION('ref_axis',(0.,1.,0.));
#73908=DIRECTION('',(0.,0.,1.));
#73909=DIRECTION('',(0.,1.,0.));
#73910=DIRECTION('center_axis',(1.,0.,0.));
#73911=DIRECTION('ref_axis',(0.,-1.,0.));
#73912=DIRECTION('',(0.,0.,-1.));
#73913=DIRECTION('',(0.,-1.,0.));
#73914=DIRECTION('',(0.,0.,-1.));
#73915=DIRECTION('',(0.,-1.,0.));
#73916=DIRECTION('center_axis',(0.,0.,-1.));
#73917=DIRECTION('ref_axis',(-1.,0.,0.));
#73918=DIRECTION('',(-1.,0.,0.));
#73919=DIRECTION('',(1.,0.,0.));
#73920=DIRECTION('',(0.,1.,0.));
#73921=DIRECTION('center_axis',(0.,1.,0.));
#73922=DIRECTION('ref_axis',(1.,0.,0.));
#73923=DIRECTION('',(1.,0.,0.));
#73924=DIRECTION('',(0.,0.,-1.));
#73925=DIRECTION('center_axis',(-1.,0.,0.));
#73926=DIRECTION('ref_axis',(0.,1.,0.));
#73927=DIRECTION('',(0.,0.,1.));
#73928=DIRECTION('',(0.,1.,0.));
#73929=DIRECTION('center_axis',(1.,0.,0.));
#73930=DIRECTION('ref_axis',(0.,-1.,0.));
#73931=DIRECTION('',(0.,0.,-1.));
#73932=DIRECTION('',(0.,-1.,0.));
#73933=DIRECTION('',(0.,0.,-1.));
#73934=DIRECTION('',(0.,-1.,0.));
#73935=DIRECTION('center_axis',(0.,0.,-1.));
#73936=DIRECTION('ref_axis',(-1.,0.,0.));
#73937=DIRECTION('',(-1.,0.,0.));
#73938=DIRECTION('',(1.,0.,0.));
#73939=DIRECTION('',(0.,1.,0.));
#73940=DIRECTION('center_axis',(0.,1.,0.));
#73941=DIRECTION('ref_axis',(1.,0.,0.));
#73942=DIRECTION('',(1.,0.,0.));
#73943=DIRECTION('',(0.,0.,-1.));
#73944=DIRECTION('center_axis',(-1.,0.,0.));
#73945=DIRECTION('ref_axis',(0.,1.,0.));
#73946=DIRECTION('',(0.,0.,1.));
#73947=DIRECTION('',(0.,1.,0.));
#73948=DIRECTION('center_axis',(1.,0.,0.));
#73949=DIRECTION('ref_axis',(0.,-1.,0.));
#73950=DIRECTION('',(0.,-1.,0.));
#73951=DIRECTION('',(0.,0.,-1.));
#73952=DIRECTION('',(0.,-1.,0.));
#73953=DIRECTION('center_axis',(-1.,0.,0.));
#73954=DIRECTION('ref_axis',(0.,1.,0.));
#73955=DIRECTION('',(0.,1.,0.));
#73956=DIRECTION('',(0.,0.,1.));
#73957=DIRECTION('',(0.,1.,0.));
#73958=DIRECTION('center_axis',(0.,0.,-1.));
#73959=DIRECTION('ref_axis',(-1.,0.,0.));
#73960=DIRECTION('center_axis',(0.,0.,1.));
#73961=DIRECTION('ref_axis',(1.,0.,0.));
#73962=DIRECTION('',(-1.,0.,0.));
#73963=DIRECTION('center_axis',(1.,0.,0.));
#73964=DIRECTION('ref_axis',(0.,-1.,0.));
#73965=DIRECTION('',(0.,0.,-1.));
#73966=DIRECTION('',(0.,-1.,0.));
#73967=DIRECTION('',(0.,0.,-1.));
#73968=DIRECTION('',(0.,-1.,0.));
#73969=DIRECTION('center_axis',(0.,0.,-1.));
#73970=DIRECTION('ref_axis',(-1.,0.,0.));
#73971=DIRECTION('',(-1.,0.,0.));
#73972=DIRECTION('',(1.,0.,0.));
#73973=DIRECTION('',(0.,1.,0.));
#73974=DIRECTION('center_axis',(0.,1.,0.));
#73975=DIRECTION('ref_axis',(1.,0.,0.));
#73976=DIRECTION('',(1.,0.,0.));
#73977=DIRECTION('',(0.,0.,-1.));
#73978=DIRECTION('center_axis',(-1.,0.,0.));
#73979=DIRECTION('ref_axis',(0.,1.,0.));
#73980=DIRECTION('',(0.,0.,1.));
#73981=DIRECTION('',(0.,1.,0.));
#73982=DIRECTION('center_axis',(1.,0.,0.));
#73983=DIRECTION('ref_axis',(0.,-1.,0.));
#73984=DIRECTION('',(0.,0.,-1.));
#73985=DIRECTION('',(0.,-1.,0.));
#73986=DIRECTION('',(0.,0.,-1.));
#73987=DIRECTION('',(0.,-1.,0.));
#73988=DIRECTION('center_axis',(0.,0.,-1.));
#73989=DIRECTION('ref_axis',(-1.,0.,0.));
#73990=DIRECTION('',(-1.,0.,0.));
#73991=DIRECTION('',(1.,0.,0.));
#73992=DIRECTION('',(0.,1.,0.));
#73993=DIRECTION('center_axis',(0.,1.,0.));
#73994=DIRECTION('ref_axis',(1.,0.,0.));
#73995=DIRECTION('',(1.,0.,0.));
#73996=DIRECTION('',(0.,0.,-1.));
#73997=DIRECTION('center_axis',(-1.,0.,0.));
#73998=DIRECTION('ref_axis',(0.,1.,0.));
#73999=DIRECTION('',(0.,0.,1.));
#74000=DIRECTION('',(0.,1.,0.));
#74001=DIRECTION('center_axis',(1.,0.,0.));
#74002=DIRECTION('ref_axis',(0.,-1.,0.));
#74003=DIRECTION('',(0.,0.,-1.));
#74004=DIRECTION('',(0.,-1.,0.));
#74005=DIRECTION('',(0.,0.,-1.));
#74006=DIRECTION('',(0.,-1.,0.));
#74007=DIRECTION('center_axis',(0.,0.,-1.));
#74008=DIRECTION('ref_axis',(-1.,0.,0.));
#74009=DIRECTION('',(-1.,0.,0.));
#74010=DIRECTION('',(1.,0.,0.));
#74011=DIRECTION('',(0.,1.,0.));
#74012=DIRECTION('center_axis',(0.,1.,0.));
#74013=DIRECTION('ref_axis',(1.,0.,0.));
#74014=DIRECTION('',(1.,0.,0.));
#74015=DIRECTION('',(0.,0.,-1.));
#74016=DIRECTION('center_axis',(-1.,0.,0.));
#74017=DIRECTION('ref_axis',(0.,1.,0.));
#74018=DIRECTION('',(0.,0.,1.));
#74019=DIRECTION('',(0.,1.,0.));
#74020=DIRECTION('center_axis',(1.,0.,0.));
#74021=DIRECTION('ref_axis',(0.,-1.,0.));
#74022=DIRECTION('',(0.,0.,-1.));
#74023=DIRECTION('',(0.,-1.,0.));
#74024=DIRECTION('',(0.,0.,-1.));
#74025=DIRECTION('',(0.,-1.,0.));
#74026=DIRECTION('center_axis',(0.,0.,-1.));
#74027=DIRECTION('ref_axis',(-1.,0.,0.));
#74028=DIRECTION('',(-1.,0.,0.));
#74029=DIRECTION('',(1.,0.,0.));
#74030=DIRECTION('',(0.,1.,0.));
#74031=DIRECTION('center_axis',(0.,1.,0.));
#74032=DIRECTION('ref_axis',(1.,0.,0.));
#74033=DIRECTION('',(1.,0.,0.));
#74034=DIRECTION('',(0.,0.,-1.));
#74035=DIRECTION('center_axis',(-1.,0.,0.));
#74036=DIRECTION('ref_axis',(0.,1.,0.));
#74037=DIRECTION('',(0.,0.,1.));
#74038=DIRECTION('',(0.,1.,0.));
#74039=DIRECTION('center_axis',(1.,0.,0.));
#74040=DIRECTION('ref_axis',(0.,-1.,0.));
#74041=DIRECTION('',(0.,0.,-1.));
#74042=DIRECTION('',(0.,-1.,0.));
#74043=DIRECTION('',(0.,0.,-1.));
#74044=DIRECTION('',(0.,-1.,0.));
#74045=DIRECTION('center_axis',(0.,0.,-1.));
#74046=DIRECTION('ref_axis',(-1.,0.,0.));
#74047=DIRECTION('',(-1.,0.,0.));
#74048=DIRECTION('',(1.,0.,0.));
#74049=DIRECTION('',(0.,1.,0.));
#74050=DIRECTION('center_axis',(0.,1.,0.));
#74051=DIRECTION('ref_axis',(1.,0.,0.));
#74052=DIRECTION('',(1.,0.,0.));
#74053=DIRECTION('',(0.,0.,-1.));
#74054=DIRECTION('center_axis',(-1.,0.,0.));
#74055=DIRECTION('ref_axis',(0.,1.,0.));
#74056=DIRECTION('',(0.,0.,1.));
#74057=DIRECTION('',(0.,1.,0.));
#74058=DIRECTION('center_axis',(1.,0.,0.));
#74059=DIRECTION('ref_axis',(0.,-1.,0.));
#74060=DIRECTION('',(0.,0.,-1.));
#74061=DIRECTION('',(0.,-1.,0.));
#74062=DIRECTION('',(0.,0.,-1.));
#74063=DIRECTION('',(0.,-1.,0.));
#74064=DIRECTION('center_axis',(0.,0.,-1.));
#74065=DIRECTION('ref_axis',(-1.,0.,0.));
#74066=DIRECTION('',(-1.,0.,0.));
#74067=DIRECTION('',(1.,0.,0.));
#74068=DIRECTION('',(0.,1.,0.));
#74069=DIRECTION('center_axis',(0.,1.,0.));
#74070=DIRECTION('ref_axis',(1.,0.,0.));
#74071=DIRECTION('',(1.,0.,0.));
#74072=DIRECTION('',(0.,0.,-1.));
#74073=DIRECTION('center_axis',(-1.,0.,0.));
#74074=DIRECTION('ref_axis',(0.,1.,0.));
#74075=DIRECTION('',(0.,0.,1.));
#74076=DIRECTION('',(0.,1.,0.));
#74077=DIRECTION('center_axis',(1.,0.,0.));
#74078=DIRECTION('ref_axis',(0.,-1.,0.));
#74079=DIRECTION('',(0.,0.,-1.));
#74080=DIRECTION('',(0.,-1.,0.));
#74081=DIRECTION('',(0.,0.,-1.));
#74082=DIRECTION('',(0.,-1.,0.));
#74083=DIRECTION('center_axis',(0.,0.,-1.));
#74084=DIRECTION('ref_axis',(-1.,0.,0.));
#74085=DIRECTION('',(-1.,0.,0.));
#74086=DIRECTION('',(1.,0.,0.));
#74087=DIRECTION('',(0.,1.,0.));
#74088=DIRECTION('center_axis',(0.,1.,0.));
#74089=DIRECTION('ref_axis',(1.,0.,0.));
#74090=DIRECTION('',(1.,0.,0.));
#74091=DIRECTION('',(0.,0.,-1.));
#74092=DIRECTION('center_axis',(-1.,0.,0.));
#74093=DIRECTION('ref_axis',(0.,1.,0.));
#74094=DIRECTION('',(0.,0.,1.));
#74095=DIRECTION('',(0.,1.,0.));
#74096=DIRECTION('center_axis',(1.,0.,0.));
#74097=DIRECTION('ref_axis',(0.,-1.,0.));
#74098=DIRECTION('',(0.,-1.,0.));
#74099=DIRECTION('',(0.,0.,-1.));
#74100=DIRECTION('',(0.,-1.,0.));
#74101=DIRECTION('center_axis',(-1.,0.,0.));
#74102=DIRECTION('ref_axis',(0.,1.,0.));
#74103=DIRECTION('',(0.,1.,0.));
#74104=DIRECTION('',(0.,0.,1.));
#74105=DIRECTION('',(0.,1.,0.));
#74106=DIRECTION('center_axis',(0.,0.,-1.));
#74107=DIRECTION('ref_axis',(-1.,0.,0.));
#74108=DIRECTION('center_axis',(0.,0.,1.));
#74109=DIRECTION('ref_axis',(1.,0.,0.));
#74110=DIRECTION('',(-1.,0.,0.));
#74111=DIRECTION('center_axis',(0.,0.,1.));
#74112=DIRECTION('ref_axis',(1.,0.,0.));
#74113=DIRECTION('',(1.,0.,0.));
#74114=DIRECTION('center_axis',(0.,0.,-1.));
#74115=DIRECTION('ref_axis',(1.,0.,0.));
#74116=DIRECTION('center_axis',(0.,0.,1.));
#74117=DIRECTION('ref_axis',(1.,0.,0.));
#74118=DIRECTION('center_axis',(0.,0.,-1.));
#74119=DIRECTION('ref_axis',(1.,0.,0.));
#74120=DIRECTION('',(1.,0.,0.));
#74121=DIRECTION('center_axis',(0.,-1.,0.));
#74122=DIRECTION('ref_axis',(1.,0.,0.));
#74123=DIRECTION('',(1.,0.,0.));
#74124=DIRECTION('',(1.,0.,0.));
#74125=DIRECTION('',(1.,0.,0.));
#74126=DIRECTION('',(1.,0.,0.));
#74127=DIRECTION('',(1.,0.,0.));
#74128=DIRECTION('',(1.,0.,0.));
#74129=DIRECTION('',(1.,0.,0.));
#74130=DIRECTION('',(1.,0.,0.));
#74131=DIRECTION('',(1.,0.,0.));
#74132=DIRECTION('',(1.,0.,0.));
#74133=DIRECTION('',(1.,0.,0.));
#74134=DIRECTION('',(1.,0.,0.));
#74135=DIRECTION('',(1.,0.,0.));
#74136=DIRECTION('',(1.,0.,0.));
#74137=DIRECTION('',(1.,0.,0.));
#74138=DIRECTION('',(1.,0.,0.));
#74139=DIRECTION('',(0.,0.,1.));
#74140=DIRECTION('',(1.,0.,0.));
#74141=DIRECTION('',(0.,0.,1.));
#74142=DIRECTION('',(1.,0.,0.));
#74143=DIRECTION('',(1.,0.,0.));
#74144=DIRECTION('center_axis',(0.,0.,1.));
#74145=DIRECTION('ref_axis',(1.,0.,0.));
#74146=DIRECTION('center_axis',(0.,0.,1.));
#74147=DIRECTION('ref_axis',(1.,0.,0.));
#74148=DIRECTION('',(0.,0.,1.));
#74149=DIRECTION('center_axis',(0.,0.,1.));
#74150=DIRECTION('ref_axis',(1.,0.,0.));
#74151=DIRECTION('center_axis',(0.,0.,1.));
#74152=DIRECTION('ref_axis',(1.,0.,0.));
#74153=DIRECTION('',(-0.707106781186554,-8.65956056235502E-17,0.707106781186541));
#74154=DIRECTION('center_axis',(0.,0.,-1.));
#74155=DIRECTION('ref_axis',(1.,0.,0.));
#74156=DIRECTION('center_axis',(0.,0.,-1.));
#74157=DIRECTION('ref_axis',(1.,0.,0.));
#74158=DIRECTION('center_axis',(0.,0.,-1.));
#74159=DIRECTION('ref_axis',(1.,0.,0.));
#74160=DIRECTION('center_axis',(0.,0.,1.));
#74161=DIRECTION('ref_axis',(1.,0.,0.));
#74162=DIRECTION('',(-1.,0.,0.));
#74163=DIRECTION('center_axis',(0.,0.,-1.));
#74164=DIRECTION('ref_axis',(1.,0.,0.));
#74165=DIRECTION('center_axis',(0.,0.,1.));
#74166=DIRECTION('ref_axis',(1.,0.,0.));
#74167=DIRECTION('',(0.,1.,0.));
#74168=DIRECTION('center_axis',(0.,0.,1.));
#74169=DIRECTION('ref_axis',(1.,0.,0.));
#74170=DIRECTION('',(-1.,0.,0.));
#74171=DIRECTION('center_axis',(0.,0.,1.));
#74172=DIRECTION('ref_axis',(1.,0.,0.));
#74173=DIRECTION('center_axis',(0.,0.,1.));
#74174=DIRECTION('ref_axis',(1.,0.,0.));
#74175=DIRECTION('',(0.,0.,1.));
#74176=DIRECTION('center_axis',(0.,0.,1.));
#74177=DIRECTION('ref_axis',(1.,0.,0.));
#74178=DIRECTION('center_axis',(0.,0.,1.));
#74179=DIRECTION('ref_axis',(1.,0.,0.));
#74180=DIRECTION('',(-0.707106781186547,-8.65956056235493E-17,0.707106781186547));
#74181=DIRECTION('center_axis',(0.,0.,-1.));
#74182=DIRECTION('ref_axis',(1.,0.,0.));
#74183=DIRECTION('center_axis',(0.,0.,-1.));
#74184=DIRECTION('ref_axis',(1.,0.,0.));
#74185=DIRECTION('center_axis',(0.,0.,1.));
#74186=DIRECTION('ref_axis',(1.,0.,0.));
#74187=DIRECTION('',(-1.,0.,0.));
#74188=DIRECTION('center_axis',(0.,0.,1.));
#74189=DIRECTION('ref_axis',(0.,1.,0.));
#74190=DIRECTION('',(0.,-1.,0.));
#74191=DIRECTION('center_axis',(0.,0.,1.));
#74192=DIRECTION('ref_axis',(0.,1.,0.));
#74193=DIRECTION('center_axis',(0.,0.,1.));
#74194=DIRECTION('ref_axis',(0.,1.,0.));
#74195=DIRECTION('',(0.,0.,1.));
#74196=DIRECTION('',(0.,0.,1.));
#74197=DIRECTION('center_axis',(0.,1.,0.));
#74198=DIRECTION('ref_axis',(-1.,0.,0.));
#74199=DIRECTION('',(0.,0.,1.));
#74200=DIRECTION('',(-1.,0.,0.));
#74201=DIRECTION('center_axis',(0.,0.,1.));
#74202=DIRECTION('ref_axis',(1.,0.,0.));
#74203=DIRECTION('center_axis',(0.,0.,1.));
#74204=DIRECTION('ref_axis',(1.,0.,0.));
#74205=DIRECTION('',(0.,0.,1.));
#74206=DIRECTION('center_axis',(1.,0.,0.));
#74207=DIRECTION('ref_axis',(0.,1.,0.));
#74208=DIRECTION('',(0.,1.,0.));
#74209=DIRECTION('center_axis',(-1.,0.,0.));
#74210=DIRECTION('ref_axis',(0.,-1.,0.));
#74211=DIRECTION('',(0.,-1.,0.));
#74212=DIRECTION('center_axis',(0.,0.,1.));
#74213=DIRECTION('ref_axis',(1.,0.,0.));
#74214=DIRECTION('axis',(0.,0.,1.));
#74215=DIRECTION('refdir',(1.,0.,0.));
#74216=DIRECTION('center_axis',(0.,0.,1.));
#74217=DIRECTION('ref_axis',(1.,0.,0.));
#74218=DIRECTION('',(0.,0.,-1.));
#74219=DIRECTION('center_axis',(0.,0.,-1.));
#74220=DIRECTION('ref_axis',(1.,0.,0.));
#74221=DIRECTION('center_axis',(0.,0.,1.));
#74222=DIRECTION('ref_axis',(1.,0.,0.));
#74223=DIRECTION('',(0.,0.,-1.));
#74224=DIRECTION('center_axis',(0.,0.,1.));
#74225=DIRECTION('ref_axis',(1.,0.,0.));
#74226=DIRECTION('',(0.,0.,-1.));
#74227=DIRECTION('center_axis',(0.,0.,1.));
#74228=DIRECTION('ref_axis',(1.,0.,0.));
#74229=DIRECTION('',(0.,0.,-1.));
#74230=DIRECTION('center_axis',(0.,0.,1.));
#74231=DIRECTION('ref_axis',(1.,0.,0.));
#74232=DIRECTION('',(0.,0.,-1.));
#74233=DIRECTION('center_axis',(0.,0.,1.));
#74234=DIRECTION('ref_axis',(1.,0.,0.));
#74235=DIRECTION('',(0.,0.,-1.));
#74236=DIRECTION('center_axis',(0.,0.,1.));
#74237=DIRECTION('ref_axis',(1.,0.,0.));
#74238=DIRECTION('',(0.,0.,-1.));
#74239=DIRECTION('center_axis',(0.,0.,1.));
#74240=DIRECTION('ref_axis',(1.,0.,0.));
#74241=DIRECTION('',(0.,0.,-1.));
#74242=DIRECTION('center_axis',(0.,0.,1.));
#74243=DIRECTION('ref_axis',(1.,0.,0.));
#74244=DIRECTION('',(0.,0.,-1.));
#74245=DIRECTION('center_axis',(0.,0.,1.));
#74246=DIRECTION('ref_axis',(1.,0.,0.));
#74247=DIRECTION('',(0.,0.,-1.));
#74248=DIRECTION('center_axis',(0.,0.,1.));
#74249=DIRECTION('ref_axis',(1.,0.,0.));
#74250=DIRECTION('',(0.,0.,-1.));
#74251=DIRECTION('center_axis',(0.,0.,1.));
#74252=DIRECTION('ref_axis',(1.,5.42442622124796E-14,0.));
#74253=DIRECTION('',(0.,0.,1.));
#74254=DIRECTION('center_axis',(0.,0.,1.));
#74255=DIRECTION('ref_axis',(1.,5.42442622124796E-14,0.));
#74256=DIRECTION('center_axis',(0.,0.,1.));
#74257=DIRECTION('ref_axis',(1.,5.42442622124796E-14,0.));
#74258=DIRECTION('',(0.,0.,1.));
#74259=DIRECTION('center_axis',(0.,0.,1.));
#74260=DIRECTION('ref_axis',(1.,5.42442622124796E-14,0.));
#74261=DIRECTION('',(0.,0.,1.));
#74262=DIRECTION('center_axis',(0.,0.,1.));
#74263=DIRECTION('ref_axis',(1.,5.42442622124796E-14,0.));
#74264=DIRECTION('',(0.,0.,1.));
#74265=DIRECTION('center_axis',(0.,0.,1.));
#74266=DIRECTION('ref_axis',(1.,5.42442622124796E-14,0.));
#74267=DIRECTION('',(0.,0.,1.));
#74268=DIRECTION('center_axis',(0.,0.,1.));
#74269=DIRECTION('ref_axis',(1.,5.42442622124796E-14,0.));
#74270=DIRECTION('',(0.,0.,1.));
#74271=DIRECTION('center_axis',(0.,0.,1.));
#74272=DIRECTION('ref_axis',(1.,5.42442622124796E-14,0.));
#74273=DIRECTION('',(0.,0.,1.));
#74274=DIRECTION('center_axis',(0.,0.,1.));
#74275=DIRECTION('ref_axis',(1.,5.42442622124796E-14,0.));
#74276=DIRECTION('',(0.,0.,1.));
#74277=DIRECTION('center_axis',(0.,0.,1.));
#74278=DIRECTION('ref_axis',(1.,5.42442622124796E-14,0.));
#74279=DIRECTION('',(0.,0.,1.));
#74280=DIRECTION('center_axis',(0.,0.,1.));
#74281=DIRECTION('ref_axis',(1.,5.42442622124796E-14,0.));
#74282=DIRECTION('',(0.,0.,1.));
#74283=DIRECTION('center_axis',(0.,0.,1.));
#74284=DIRECTION('ref_axis',(1.,0.,0.));
#74285=DIRECTION('center_axis',(0.,0.,-1.));
#74286=DIRECTION('ref_axis',(1.,0.,0.));
#74287=DIRECTION('center_axis',(0.,0.,-1.));
#74288=DIRECTION('ref_axis',(1.,0.,0.));
#74289=DIRECTION('center_axis',(0.,0.,1.));
#74290=DIRECTION('ref_axis',(1.,0.,0.));
#74291=DIRECTION('center_axis',(0.,0.,-1.));
#74292=DIRECTION('ref_axis',(1.,0.,0.));
#74293=DIRECTION('center_axis',(0.,0.,-1.));
#74294=DIRECTION('ref_axis',(1.,5.42442622124796E-14,0.));
#74295=DIRECTION('center_axis',(0.,0.,-1.));
#74296=DIRECTION('ref_axis',(1.,0.,0.));
#74297=DIRECTION('center_axis',(0.,0.,1.));
#74298=DIRECTION('ref_axis',(0.889182919820768,0.457551893339995,0.));
#74299=DIRECTION('center_axis',(0.,0.,1.));
#74300=DIRECTION('ref_axis',(1.,0.,0.));
#74301=DIRECTION('center_axis',(0.,0.,1.));
#74302=DIRECTION('ref_axis',(1.,0.,0.));
#74303=DIRECTION('center_axis',(0.,-1.,0.));
#74304=DIRECTION('ref_axis',(-1.,0.,0.));
#74305=DIRECTION('center_axis',(0.,0.,1.));
#74306=DIRECTION('ref_axis',(1.,0.,0.));
#74307=DIRECTION('center_axis',(0.,0.,1.));
#74308=DIRECTION('ref_axis',(1.,0.,0.));
#74309=DIRECTION('center_axis',(0.,0.,1.));
#74310=DIRECTION('ref_axis',(1.,0.,0.));
#74311=DIRECTION('center_axis',(0.,0.,-1.));
#74312=DIRECTION('ref_axis',(1.,0.,0.));
#74313=DIRECTION('center_axis',(0.,1.,0.));
#74314=DIRECTION('ref_axis',(-1.,0.,0.));
#74315=DIRECTION('',(0.,0.,-1.));
#74316=DIRECTION('',(-1.,0.,0.));
#74317=DIRECTION('',(0.,0.,1.));
#74318=DIRECTION('',(-1.,0.,0.));
#74319=DIRECTION('center_axis',(0.,-1.,0.));
#74320=DIRECTION('ref_axis',(1.,0.,0.));
#74321=DIRECTION('',(0.,0.,1.));
#74322=DIRECTION('',(1.,0.,0.));
#74323=DIRECTION('',(0.,0.,-1.));
#74324=DIRECTION('',(1.,0.,0.));
#74325=DIRECTION('center_axis',(0.,0.,1.));
#74326=DIRECTION('ref_axis',(1.,0.,0.));
#74327=DIRECTION('center_axis',(0.,0.,1.));
#74328=DIRECTION('ref_axis',(1.,0.,0.));
#74329=DIRECTION('center_axis',(0.,0.,1.));
#74330=DIRECTION('ref_axis',(1.,0.,0.));
#74331=DIRECTION('center_axis',(0.,0.,1.));
#74332=DIRECTION('ref_axis',(1.,0.,0.));
#74333=DIRECTION('center_axis',(0.,0.,1.));
#74334=DIRECTION('ref_axis',(1.,0.,0.));
#74335=DIRECTION('center_axis',(0.,0.,1.));
#74336=DIRECTION('ref_axis',(1.,0.,0.));
#74337=DIRECTION('center_axis',(0.,0.,1.));
#74338=DIRECTION('ref_axis',(1.,0.,0.));
#74339=DIRECTION('center_axis',(0.,0.,1.));
#74340=DIRECTION('ref_axis',(1.,0.,0.));
#74341=DIRECTION('center_axis',(0.,0.,1.));
#74342=DIRECTION('ref_axis',(1.,0.,0.));
#74343=DIRECTION('center_axis',(0.,0.,1.));
#74344=DIRECTION('ref_axis',(1.,0.,0.));
#74345=DIRECTION('center_axis',(0.,0.,-1.));
#74346=DIRECTION('ref_axis',(-1.,0.,0.));
#74347=DIRECTION('center_axis',(0.,0.,-1.));
#74348=DIRECTION('ref_axis',(-1.,0.,0.));
#74349=DIRECTION('center_axis',(0.,0.,1.));
#74350=DIRECTION('ref_axis',(1.,0.,0.));
#74351=DIRECTION('',(0.,0.,-1.));
#74352=DIRECTION('center_axis',(0.,0.,-1.));
#74353=DIRECTION('ref_axis',(1.,0.,0.));
#74354=DIRECTION('center_axis',(0.,0.,1.));
#74355=DIRECTION('ref_axis',(1.,0.,0.));
#74356=DIRECTION('',(-0.70710678118654,-8.65956056235484E-17,-0.707106781186555));
#74357=DIRECTION('center_axis',(0.,0.,1.));
#74358=DIRECTION('ref_axis',(1.,0.,0.));
#74359=DIRECTION('axis',(0.,0.,1.));
#74360=DIRECTION('refdir',(1.,0.,0.));
#74361=DIRECTION('center_axis',(0.,-1.,0.));
#74362=DIRECTION('ref_axis',(1.,0.,0.));
#74363=DIRECTION('',(0.,1.,0.));
#74364=DIRECTION('center_axis',(0.,-1.,0.));
#74365=DIRECTION('ref_axis',(1.,0.,0.));
#74366=DIRECTION('center_axis',(0.,-1.,0.));
#74367=DIRECTION('ref_axis',(1.,0.,0.));
#74368=DIRECTION('',(0.,1.,0.));
#74369=DIRECTION('center_axis',(0.,-1.,0.));
#74370=DIRECTION('ref_axis',(1.,0.,0.));
#74371=DIRECTION('',(0.,1.,0.));
#74372=DIRECTION('center_axis',(0.,-1.,0.));
#74373=DIRECTION('ref_axis',(1.,0.,0.));
#74374=DIRECTION('',(0.,1.,0.));
#74375=DIRECTION('center_axis',(0.,-1.,0.));
#74376=DIRECTION('ref_axis',(1.,0.,0.));
#74377=DIRECTION('',(0.,1.,0.));
#74378=DIRECTION('center_axis',(0.,-1.,0.));
#74379=DIRECTION('ref_axis',(0.945756964993923,0.,-0.324874996214674));
#74380=DIRECTION('',(0.,-1.,0.));
#74381=DIRECTION('center_axis',(0.,-1.,0.));
#74382=DIRECTION('ref_axis',(1.,0.,-7.54131538696774E-15));
#74383=DIRECTION('center_axis',(0.,-1.,0.));
#74384=DIRECTION('ref_axis',(1.,0.,-7.54131538696774E-15));
#74385=DIRECTION('',(0.,-1.,0.));
#74386=DIRECTION('center_axis',(0.,-1.,0.));
#74387=DIRECTION('ref_axis',(1.,0.,-7.54131538696774E-15));
#74388=DIRECTION('',(0.,-1.,0.));
#74389=DIRECTION('center_axis',(0.,-1.,0.));
#74390=DIRECTION('ref_axis',(1.,0.,-7.54131538696774E-15));
#74391=DIRECTION('',(0.,-1.,0.));
#74392=DIRECTION('center_axis',(0.,1.,0.));
#74393=DIRECTION('ref_axis',(0.,0.,1.));
#74394=DIRECTION('center_axis',(0.,1.,0.));
#74395=DIRECTION('ref_axis',(1.,0.,0.));
#74396=DIRECTION('center_axis',(0.,1.,0.));
#74397=DIRECTION('ref_axis',(1.,0.,0.));
#74398=DIRECTION('center_axis',(0.,1.,0.));
#74399=DIRECTION('ref_axis',(0.,0.,1.));
#74400=DIRECTION('center_axis',(0.,-1.,0.));
#74401=DIRECTION('ref_axis',(1.,0.,0.));
#74402=DIRECTION('center_axis',(0.,-1.,0.));
#74403=DIRECTION('ref_axis',(1.,0.,0.));
#74404=DIRECTION('center_axis',(0.,1.,0.));
#74405=DIRECTION('ref_axis',(1.,0.,-7.54131538696774E-15));
#74406=DIRECTION('center_axis',(0.,-1.,0.));
#74407=DIRECTION('ref_axis',(1.,0.,-7.54131538696774E-15));
#74408=DIRECTION('center_axis',(0.,1.,0.));
#74409=DIRECTION('ref_axis',(1.,0.,0.));
#74410=DIRECTION('center_axis',(0.,-1.,0.));
#74411=DIRECTION('ref_axis',(1.,0.,0.));
#74412=DIRECTION('',(0.70710678118654,-0.707106781186555,8.65956056235484E-17));
#74413=DIRECTION('center_axis',(0.,-1.,0.));
#74414=DIRECTION('ref_axis',(1.,0.,0.));
#74415=DIRECTION('center_axis',(0.,-1.,0.));
#74416=DIRECTION('ref_axis',(1.,0.,0.));
#74417=DIRECTION('center_axis',(0.,-1.,0.));
#74418=DIRECTION('ref_axis',(1.,0.,0.));
#74419=DIRECTION('center_axis',(0.,-1.,0.));
#74420=DIRECTION('ref_axis',(1.,0.,0.));
#74421=DIRECTION('center_axis',(0.,-1.,0.));
#74422=DIRECTION('ref_axis',(1.,0.,0.));
#74423=DIRECTION('center_axis',(0.,-1.,0.));
#74424=DIRECTION('ref_axis',(1.,0.,0.));
#74425=DIRECTION('center_axis',(0.,-1.,0.));
#74426=DIRECTION('ref_axis',(1.,0.,0.));
#74427=DIRECTION('',(0.,1.,0.));
#74428=DIRECTION('',(0.,-1.,0.));
#74429=DIRECTION('center_axis',(0.,1.,0.));
#74430=DIRECTION('ref_axis',(1.,0.,0.));
#74431=DIRECTION('center_axis',(0.,-1.,0.));
#74432=DIRECTION('ref_axis',(1.,0.,0.));
#74433=DIRECTION('',(0.,1.,0.));
#74434=DIRECTION('',(0.,-1.,0.));
#74435=DIRECTION('center_axis',(0.,1.,0.));
#74436=DIRECTION('ref_axis',(1.,0.,0.));
#74437=DIRECTION('center_axis',(0.,-1.,0.));
#74438=DIRECTION('ref_axis',(1.,0.,0.));
#74439=DIRECTION('',(0.,-1.,0.));
#74440=DIRECTION('center_axis',(0.,1.,0.));
#74441=DIRECTION('ref_axis',(1.,0.,0.));
#74442=DIRECTION('',(0.,1.,0.));
#74443=DIRECTION('center_axis',(0.,-1.,0.));
#74444=DIRECTION('ref_axis',(1.,0.,0.));
#74445=DIRECTION('',(0.,1.,0.));
#74446=DIRECTION('',(0.,-1.,0.));
#74447=DIRECTION('center_axis',(0.,1.,0.));
#74448=DIRECTION('ref_axis',(1.,0.,0.));
#74449=DIRECTION('center_axis',(0.,-1.,0.));
#74450=DIRECTION('ref_axis',(1.,0.,0.));
#74451=DIRECTION('',(0.,-1.,0.));
#74452=DIRECTION('center_axis',(0.,1.,0.));
#74453=DIRECTION('ref_axis',(1.,0.,0.));
#74454=DIRECTION('',(0.,1.,0.));
#74455=DIRECTION('center_axis',(0.,-1.,0.));
#74456=DIRECTION('ref_axis',(1.,0.,0.));
#74457=DIRECTION('',(0.,-1.,0.));
#74458=DIRECTION('center_axis',(0.,1.,0.));
#74459=DIRECTION('ref_axis',(1.,0.,0.));
#74460=DIRECTION('',(0.,1.,0.));
#74461=DIRECTION('center_axis',(0.86602540378444,0.,0.499999999999997));
#74462=DIRECTION('ref_axis',(-0.499999999999997,0.,0.86602540378444));
#74463=DIRECTION('',(-0.499999999999997,0.,0.86602540378444));
#74464=DIRECTION('',(0.,-1.,0.));
#74465=DIRECTION('',(-0.499999999999997,0.,0.86602540378444));
#74466=DIRECTION('',(0.,-1.,0.));
#74467=DIRECTION('center_axis',(0.86602540378444,0.,-0.499999999999997));
#74468=DIRECTION('ref_axis',(0.499999999999997,0.,0.86602540378444));
#74469=DIRECTION('',(0.499999999999997,0.,0.86602540378444));
#74470=DIRECTION('',(0.,-1.,0.));
#74471=DIRECTION('',(0.499999999999997,0.,0.86602540378444));
#74472=DIRECTION('center_axis',(0.,0.,-1.));
#74473=DIRECTION('ref_axis',(1.,0.,0.));
#74474=DIRECTION('',(1.,0.,0.));
#74475=DIRECTION('',(0.,-1.,0.));
#74476=DIRECTION('',(1.,0.,0.));
#74477=DIRECTION('center_axis',(0.,1.,0.));
#74478=DIRECTION('ref_axis',(0.,0.,1.));
#74479=DIRECTION('center_axis',(0.,1.,0.));
#74480=DIRECTION('ref_axis',(0.,0.,1.));
#74481=DIRECTION('center_axis',(0.,1.,0.));
#74482=DIRECTION('ref_axis',(0.,0.,1.));
#74483=DIRECTION('',(0.499999999999997,0.,-0.86602540378444));
#74484=DIRECTION('center_axis',(0.,1.,0.));
#74485=DIRECTION('ref_axis',(0.,0.,1.));
#74486=DIRECTION('center_axis',(0.,1.,0.));
#74487=DIRECTION('ref_axis',(0.,0.,1.));
#74488=DIRECTION('',(-0.499999999999997,0.,-0.86602540378444));
#74489=DIRECTION('center_axis',(0.,1.,0.));
#74490=DIRECTION('ref_axis',(0.,0.,1.));
#74491=DIRECTION('',(-1.,0.,0.));
#74492=DIRECTION('center_axis',(0.,1.,0.));
#74493=DIRECTION('ref_axis',(0.,0.,1.));
#74494=DIRECTION('',(0.499999999999997,0.,-0.86602540378444));
#74495=DIRECTION('center_axis',(0.,-1.,0.));
#74496=DIRECTION('ref_axis',(1.,0.,0.));
#74497=DIRECTION('center_axis',(0.,1.,0.));
#74498=DIRECTION('ref_axis',(0.,0.,1.));
#74499=DIRECTION('center_axis',(0.,-1.,0.));
#74500=DIRECTION('ref_axis',(1.,0.,0.));
#74501=DIRECTION('center_axis',(0.,1.,0.));
#74502=DIRECTION('ref_axis',(0.,0.,1.));
#74503=DIRECTION('center_axis',(0.,-1.,0.));
#74504=DIRECTION('ref_axis',(1.,0.,0.));
#74505=DIRECTION('center_axis',(0.,1.,0.));
#74506=DIRECTION('ref_axis',(0.,0.,1.));
#74507=DIRECTION('center_axis',(0.,-1.,0.));
#74508=DIRECTION('ref_axis',(1.,0.,0.));
#74509=DIRECTION('center_axis',(0.,1.,0.));
#74510=DIRECTION('ref_axis',(0.,0.,1.));
#74511=DIRECTION('',(-1.,0.,0.));
#74512=DIRECTION('center_axis',(0.,-1.,0.));
#74513=DIRECTION('ref_axis',(1.,0.,0.));
#74514=DIRECTION('center_axis',(0.,1.,0.));
#74515=DIRECTION('ref_axis',(0.,0.,1.));
#74516=DIRECTION('',(-0.499999999999997,0.,-0.86602540378444));
#74517=DIRECTION('center_axis',(0.,-1.,0.));
#74518=DIRECTION('ref_axis',(1.,0.,0.));
#74519=DIRECTION('center_axis',(0.,1.,0.));
#74520=DIRECTION('ref_axis',(1.,0.,0.));
#74521=DIRECTION('',(0.857167300702111,-0.515038074910056,1.04972719113862E-16));
#74522=DIRECTION('center_axis',(-0.86602540378444,0.,-0.499999999999997));
#74523=DIRECTION('ref_axis',(0.499999999999997,0.,-0.86602540378444));
#74524=DIRECTION('',(0.,-1.,0.));
#74525=DIRECTION('center_axis',(-0.86602540378444,0.,0.499999999999997));
#74526=DIRECTION('ref_axis',(-0.499999999999997,0.,-0.86602540378444));
#74527=DIRECTION('',(0.,-1.,0.));
#74528=DIRECTION('center_axis',(0.,0.,1.));
#74529=DIRECTION('ref_axis',(-1.,0.,0.));
#74530=DIRECTION('center_axis',(0.,1.,0.));
#74531=DIRECTION('ref_axis',(0.,0.,1.));
#74532=DIRECTION('center_axis',(0.,-1.,0.));
#74533=DIRECTION('ref_axis',(1.,0.,0.));
#74534=DIRECTION('center_axis',(0.,-1.,0.));
#74535=DIRECTION('ref_axis',(1.,0.,0.));
#74536=DIRECTION('',(0.707106781186537,0.707106781186558,8.6595605623548E-17));
#74537=DIRECTION('center_axis',(0.,-1.,0.));
#74538=DIRECTION('ref_axis',(1.,0.,0.));
#74539=DIRECTION('center_axis',(0.,1.,0.));
#74540=DIRECTION('ref_axis',(1.,0.,0.));
#74541=DIRECTION('center_axis',(0.,1.,0.));
#74542=DIRECTION('ref_axis',(1.,0.,0.));
#74543=DIRECTION('center_axis',(0.,-1.,0.));
#74544=DIRECTION('ref_axis',(1.,0.,0.));
#74545=DIRECTION('',(-0.707106781186554,0.707106781186541,-8.65956056235501E-17));
#74546=DIRECTION('center_axis',(0.,-1.,0.));
#74547=DIRECTION('ref_axis',(0.,0.,-1.));
#74548=DIRECTION('axis',(0.,0.,1.));
#74549=DIRECTION('refdir',(1.,0.,0.));
#74550=DIRECTION('center_axis',(0.,-1.,0.));
#74551=DIRECTION('ref_axis',(1.,0.,0.));
#74552=DIRECTION('',(0.,1.,0.));
#74553=DIRECTION('center_axis',(0.,-1.,0.));
#74554=DIRECTION('ref_axis',(1.,0.,0.));
#74555=DIRECTION('center_axis',(0.,-1.,0.));
#74556=DIRECTION('ref_axis',(1.,0.,0.));
#74557=DIRECTION('',(0.,1.,0.));
#74558=DIRECTION('center_axis',(0.,-1.,0.));
#74559=DIRECTION('ref_axis',(1.,0.,0.));
#74560=DIRECTION('',(0.,1.,0.));
#74561=DIRECTION('center_axis',(0.,-1.,0.));
#74562=DIRECTION('ref_axis',(1.,0.,0.));
#74563=DIRECTION('',(0.,1.,0.));
#74564=DIRECTION('center_axis',(0.,1.,0.));
#74565=DIRECTION('ref_axis',(1.,0.,0.));
#74566=DIRECTION('center_axis',(0.,-1.,0.));
#74567=DIRECTION('ref_axis',(0.495633595239364,0.,-0.868531714602353));
#74568=DIRECTION('',(0.,-1.,0.));
#74569=DIRECTION('center_axis',(0.,-1.,0.));
#74570=DIRECTION('ref_axis',(1.,0.,0.));
#74571=DIRECTION('center_axis',(0.,-1.,0.));
#74572=DIRECTION('ref_axis',(1.,0.,0.));
#74573=DIRECTION('',(0.,-1.,0.));
#74574=DIRECTION('center_axis',(0.,-1.,0.));
#74575=DIRECTION('ref_axis',(1.,0.,0.));
#74576=DIRECTION('',(0.,-1.,0.));
#74577=DIRECTION('center_axis',(0.,1.,0.));
#74578=DIRECTION('ref_axis',(0.,0.,1.));
#74579=DIRECTION('center_axis',(0.,1.,0.));
#74580=DIRECTION('ref_axis',(1.,0.,0.));
#74581=DIRECTION('center_axis',(0.,1.,0.));
#74582=DIRECTION('ref_axis',(0.,0.,1.));
#74583=DIRECTION('center_axis',(0.,-1.,0.));
#74584=DIRECTION('ref_axis',(1.,0.,0.));
#74585=DIRECTION('center_axis',(0.,-1.,0.));
#74586=DIRECTION('ref_axis',(1.,0.,0.));
#74587=DIRECTION('center_axis',(0.,1.,0.));
#74588=DIRECTION('ref_axis',(1.,0.,0.));
#74589=DIRECTION('center_axis',(0.,-1.,0.));
#74590=DIRECTION('ref_axis',(1.,0.,0.));
#74591=DIRECTION('center_axis',(0.,1.,0.));
#74592=DIRECTION('ref_axis',(1.,0.,0.));
#74593=DIRECTION('center_axis',(0.,-1.,0.));
#74594=DIRECTION('ref_axis',(1.,0.,0.));
#74595=DIRECTION('',(0.70710678118654,-0.707106781186555,8.65956056235484E-17));
#74596=DIRECTION('center_axis',(0.,-1.,0.));
#74597=DIRECTION('ref_axis',(1.,0.,0.));
#74598=DIRECTION('center_axis',(0.,-1.,0.));
#74599=DIRECTION('ref_axis',(1.,0.,0.));
#74600=DIRECTION('center_axis',(0.,-1.,0.));
#74601=DIRECTION('ref_axis',(1.,0.,0.));
#74602=DIRECTION('center_axis',(0.,-1.,0.));
#74603=DIRECTION('ref_axis',(1.,0.,0.));
#74604=DIRECTION('center_axis',(0.,-1.,0.));
#74605=DIRECTION('ref_axis',(1.,0.,0.));
#74606=DIRECTION('center_axis',(0.,-1.,0.));
#74607=DIRECTION('ref_axis',(1.,0.,0.));
#74608=DIRECTION('center_axis',(0.,-1.,0.));
#74609=DIRECTION('ref_axis',(1.,0.,0.));
#74610=DIRECTION('',(0.,1.,0.));
#74611=DIRECTION('',(0.,-1.,0.));
#74612=DIRECTION('center_axis',(0.,1.,0.));
#74613=DIRECTION('ref_axis',(1.,0.,0.));
#74614=DIRECTION('center_axis',(0.,-1.,0.));
#74615=DIRECTION('ref_axis',(1.,0.,0.));
#74616=DIRECTION('',(0.,1.,0.));
#74617=DIRECTION('',(0.,-1.,0.));
#74618=DIRECTION('center_axis',(0.,1.,0.));
#74619=DIRECTION('ref_axis',(1.,0.,0.));
#74620=DIRECTION('center_axis',(0.,-1.,0.));
#74621=DIRECTION('ref_axis',(1.,0.,0.));
#74622=DIRECTION('',(0.,-1.,0.));
#74623=DIRECTION('center_axis',(0.,1.,0.));
#74624=DIRECTION('ref_axis',(1.,0.,0.));
#74625=DIRECTION('',(0.,1.,0.));
#74626=DIRECTION('center_axis',(0.,-1.,0.));
#74627=DIRECTION('ref_axis',(1.,0.,0.));
#74628=DIRECTION('',(0.,1.,0.));
#74629=DIRECTION('',(0.,-1.,0.));
#74630=DIRECTION('center_axis',(0.,1.,0.));
#74631=DIRECTION('ref_axis',(1.,0.,0.));
#74632=DIRECTION('center_axis',(0.,-1.,0.));
#74633=DIRECTION('ref_axis',(1.,0.,0.));
#74634=DIRECTION('',(0.,-1.,0.));
#74635=DIRECTION('center_axis',(0.,1.,0.));
#74636=DIRECTION('ref_axis',(1.,0.,0.));
#74637=DIRECTION('',(0.,1.,0.));
#74638=DIRECTION('center_axis',(0.,-1.,0.));
#74639=DIRECTION('ref_axis',(1.,0.,0.));
#74640=DIRECTION('',(0.,-1.,0.));
#74641=DIRECTION('center_axis',(0.,1.,0.));
#74642=DIRECTION('ref_axis',(1.,0.,0.));
#74643=DIRECTION('',(0.,1.,0.));
#74644=DIRECTION('center_axis',(0.86602540378445,0.,0.499999999999979));
#74645=DIRECTION('ref_axis',(-0.499999999999979,0.,0.86602540378445));
#74646=DIRECTION('',(-0.499999999999979,0.,0.86602540378445));
#74647=DIRECTION('',(0.,-1.,0.));
#74648=DIRECTION('',(-0.499999999999979,0.,0.86602540378445));
#74649=DIRECTION('',(0.,-1.,0.));
#74650=DIRECTION('center_axis',(0.86602540378445,0.,-0.499999999999979));
#74651=DIRECTION('ref_axis',(0.499999999999979,0.,0.86602540378445));
#74652=DIRECTION('',(0.499999999999979,0.,0.86602540378445));
#74653=DIRECTION('',(0.,-1.,0.));
#74654=DIRECTION('',(0.499999999999979,0.,0.86602540378445));
#74655=DIRECTION('center_axis',(0.,0.,-1.));
#74656=DIRECTION('ref_axis',(1.,0.,0.));
#74657=DIRECTION('',(1.,0.,0.));
#74658=DIRECTION('',(0.,-1.,0.));
#74659=DIRECTION('',(1.,0.,0.));
#74660=DIRECTION('center_axis',(0.,1.,0.));
#74661=DIRECTION('ref_axis',(0.,0.,1.));
#74662=DIRECTION('center_axis',(0.,1.,0.));
#74663=DIRECTION('ref_axis',(0.,0.,1.));
#74664=DIRECTION('center_axis',(0.,1.,0.));
#74665=DIRECTION('ref_axis',(0.,0.,1.));
#74666=DIRECTION('',(0.499999999999979,0.,-0.86602540378445));
#74667=DIRECTION('center_axis',(0.,1.,0.));
#74668=DIRECTION('ref_axis',(0.,0.,1.));
#74669=DIRECTION('center_axis',(0.,1.,0.));
#74670=DIRECTION('ref_axis',(0.,0.,1.));
#74671=DIRECTION('',(-0.499999999999979,0.,-0.86602540378445));
#74672=DIRECTION('center_axis',(0.,1.,0.));
#74673=DIRECTION('ref_axis',(0.,0.,1.));
#74674=DIRECTION('',(-1.,0.,0.));
#74675=DIRECTION('center_axis',(0.,1.,0.));
#74676=DIRECTION('ref_axis',(0.,0.,1.));
#74677=DIRECTION('',(0.499999999999979,0.,-0.86602540378445));
#74678=DIRECTION('center_axis',(0.,-1.,0.));
#74679=DIRECTION('ref_axis',(1.,0.,0.));
#74680=DIRECTION('center_axis',(0.,1.,0.));
#74681=DIRECTION('ref_axis',(0.,0.,1.));
#74682=DIRECTION('center_axis',(0.,-1.,0.));
#74683=DIRECTION('ref_axis',(1.,0.,0.));
#74684=DIRECTION('center_axis',(0.,1.,0.));
#74685=DIRECTION('ref_axis',(0.,0.,1.));
#74686=DIRECTION('center_axis',(0.,-1.,0.));
#74687=DIRECTION('ref_axis',(1.,0.,0.));
#74688=DIRECTION('center_axis',(0.,1.,0.));
#74689=DIRECTION('ref_axis',(0.,0.,1.));
#74690=DIRECTION('center_axis',(0.,-1.,0.));
#74691=DIRECTION('ref_axis',(1.,0.,0.));
#74692=DIRECTION('center_axis',(0.,1.,0.));
#74693=DIRECTION('ref_axis',(0.,0.,1.));
#74694=DIRECTION('',(-1.,0.,0.));
#74695=DIRECTION('center_axis',(0.,-1.,0.));
#74696=DIRECTION('ref_axis',(1.,0.,0.));
#74697=DIRECTION('center_axis',(0.,1.,0.));
#74698=DIRECTION('ref_axis',(0.,0.,1.));
#74699=DIRECTION('',(-0.499999999999979,0.,-0.86602540378445));
#74700=DIRECTION('center_axis',(0.,-1.,0.));
#74701=DIRECTION('ref_axis',(1.,0.,0.));
#74702=DIRECTION('center_axis',(0.,1.,0.));
#74703=DIRECTION('ref_axis',(1.,0.,0.));
#74704=DIRECTION('',(0.857167300702112,-0.515038074910054,1.04972719113862E-16));
#74705=DIRECTION('center_axis',(-0.86602540378445,0.,-0.499999999999979));
#74706=DIRECTION('ref_axis',(0.499999999999979,0.,-0.86602540378445));
#74707=DIRECTION('',(0.,-1.,0.));
#74708=DIRECTION('center_axis',(-0.86602540378445,0.,0.499999999999979));
#74709=DIRECTION('ref_axis',(-0.499999999999979,0.,-0.86602540378445));
#74710=DIRECTION('',(0.,-1.,0.));
#74711=DIRECTION('center_axis',(0.,0.,1.));
#74712=DIRECTION('ref_axis',(-1.,0.,0.));
#74713=DIRECTION('center_axis',(0.,1.,0.));
#74714=DIRECTION('ref_axis',(0.,0.,1.));
#74715=DIRECTION('center_axis',(0.,-1.,0.));
#74716=DIRECTION('ref_axis',(1.,0.,0.));
#74717=DIRECTION('center_axis',(0.,-1.,0.));
#74718=DIRECTION('ref_axis',(1.,0.,0.));
#74719=DIRECTION('',(0.707106781186541,0.707106781186554,8.65956056235485E-17));
#74720=DIRECTION('center_axis',(0.,-1.,0.));
#74721=DIRECTION('ref_axis',(-0.906528546186737,0.,-0.422144519031766));
#74722=DIRECTION('center_axis',(0.,1.,0.));
#74723=DIRECTION('ref_axis',(1.,0.,0.));
#74724=DIRECTION('center_axis',(0.,1.,0.));
#74725=DIRECTION('ref_axis',(1.,0.,0.));
#74726=DIRECTION('center_axis',(0.,-1.,0.));
#74727=DIRECTION('ref_axis',(1.,0.,0.));
#74728=DIRECTION('',(-0.707106781186541,0.707106781186554,-8.65956056235486E-17));
#74729=DIRECTION('center_axis',(0.,-1.,0.));
#74730=DIRECTION('ref_axis',(0.,0.,-1.));
#74731=DIRECTION('axis',(0.,0.,1.));
#74732=DIRECTION('refdir',(1.,0.,0.));
#74733=DIRECTION('center_axis',(0.,0.,1.));
#74734=DIRECTION('ref_axis',(1.,0.,0.));
#74735=DIRECTION('',(0.,0.,-1.));
#74736=DIRECTION('center_axis',(0.,0.,1.));
#74737=DIRECTION('ref_axis',(1.,0.,0.));
#74738=DIRECTION('center_axis',(0.,0.,1.));
#74739=DIRECTION('ref_axis',(1.,0.,0.));
#74740=DIRECTION('',(0.,0.,-1.));
#74741=DIRECTION('center_axis',(0.,0.,1.));
#74742=DIRECTION('ref_axis',(1.,0.,0.));
#74743=DIRECTION('',(0.,0.,-1.));
#74744=DIRECTION('center_axis',(0.,0.,1.));
#74745=DIRECTION('ref_axis',(1.,0.,0.));
#74746=DIRECTION('',(0.,0.,-1.));
#74747=DIRECTION('center_axis',(0.,0.,1.));
#74748=DIRECTION('ref_axis',(1.,0.,0.));
#74749=DIRECTION('',(0.,0.,-1.));
#74750=DIRECTION('center_axis',(0.,0.,1.));
#74751=DIRECTION('ref_axis',(1.,0.,0.));
#74752=DIRECTION('',(0.,0.,-1.));
#74753=DIRECTION('center_axis',(0.,0.,1.));
#74754=DIRECTION('ref_axis',(1.,0.,0.));
#74755=DIRECTION('',(0.,0.,-1.));
#74756=DIRECTION('center_axis',(0.,0.,1.));
#74757=DIRECTION('ref_axis',(1.,0.,0.));
#74758=DIRECTION('',(0.,0.,-1.));
#74759=DIRECTION('center_axis',(0.,0.,1.));
#74760=DIRECTION('ref_axis',(1.,0.,0.));
#74761=DIRECTION('',(0.,0.,-1.));
#74762=DIRECTION('center_axis',(0.,0.,1.));
#74763=DIRECTION('ref_axis',(1.,0.,0.));
#74764=DIRECTION('',(0.,0.,-1.));
#74765=DIRECTION('center_axis',(0.,0.,1.));
#74766=DIRECTION('ref_axis',(1.,0.,0.));
#74767=DIRECTION('',(0.,0.,-1.));
#74768=DIRECTION('center_axis',(0.,0.,1.));
#74769=DIRECTION('ref_axis',(0.945752973643215,-0.324886615367603,0.));
#74770=DIRECTION('',(0.,0.,1.));
#74771=DIRECTION('center_axis',(0.,0.,1.));
#74772=DIRECTION('ref_axis',(1.,6.22158519424838E-14,0.));
#74773=DIRECTION('center_axis',(0.,0.,1.));
#74774=DIRECTION('ref_axis',(1.,6.22158519424838E-14,0.));
#74775=DIRECTION('',(0.,0.,1.));
#74776=DIRECTION('center_axis',(0.,0.,1.));
#74777=DIRECTION('ref_axis',(1.,6.22158519424838E-14,0.));
#74778=DIRECTION('',(0.,0.,1.));
#74779=DIRECTION('center_axis',(0.,0.,1.));
#74780=DIRECTION('ref_axis',(1.,6.22158519424838E-14,0.));
#74781=DIRECTION('',(0.,0.,1.));
#74782=DIRECTION('center_axis',(0.,0.,1.));
#74783=DIRECTION('ref_axis',(1.,6.22158519424838E-14,0.));
#74784=DIRECTION('',(0.,0.,1.));
#74785=DIRECTION('center_axis',(0.,0.,1.));
#74786=DIRECTION('ref_axis',(1.,6.22158519424838E-14,0.));
#74787=DIRECTION('',(0.,0.,1.));
#74788=DIRECTION('center_axis',(0.,0.,1.));
#74789=DIRECTION('ref_axis',(1.,6.22158519424838E-14,0.));
#74790=DIRECTION('',(0.,0.,1.));
#74791=DIRECTION('center_axis',(0.,0.,1.));
#74792=DIRECTION('ref_axis',(1.,6.22158519424838E-14,0.));
#74793=DIRECTION('',(0.,0.,1.));
#74794=DIRECTION('center_axis',(0.,0.,1.));
#74795=DIRECTION('ref_axis',(1.,6.22158519424838E-14,0.));
#74796=DIRECTION('',(0.,0.,1.));
#74797=DIRECTION('center_axis',(0.,0.,1.));
#74798=DIRECTION('ref_axis',(1.,6.22158519424838E-14,0.));
#74799=DIRECTION('',(0.,0.,1.));
#74800=DIRECTION('center_axis',(0.,0.,1.));
#74801=DIRECTION('ref_axis',(1.,0.,0.));
#74802=DIRECTION('center_axis',(0.,0.,-1.));
#74803=DIRECTION('ref_axis',(1.,0.,0.));
#74804=DIRECTION('center_axis',(0.,0.,-1.));
#74805=DIRECTION('ref_axis',(1.,0.,0.));
#74806=DIRECTION('center_axis',(0.,0.,1.));
#74807=DIRECTION('ref_axis',(1.,0.,0.));
#74808=DIRECTION('center_axis',(0.,0.,1.));
#74809=DIRECTION('ref_axis',(1.,0.,0.));
#74810=DIRECTION('center_axis',(0.,0.,1.));
#74811=DIRECTION('ref_axis',(1.,0.,0.));
#74812=DIRECTION('center_axis',(0.,0.,-1.));
#74813=DIRECTION('ref_axis',(1.,6.22158519424838E-14,0.));
#74814=DIRECTION('center_axis',(0.,0.,1.));
#74815=DIRECTION('ref_axis',(1.,6.22158519424838E-14,0.));
#74816=DIRECTION('center_axis',(0.,0.,-1.));
#74817=DIRECTION('ref_axis',(1.,0.,0.));
#74818=DIRECTION('center_axis',(0.,0.,1.));
#74819=DIRECTION('ref_axis',(1.,0.,0.));
#74820=DIRECTION('',(0.707106781186573,8.65956056235524E-17,0.707106781186522));
#74821=DIRECTION('center_axis',(0.,0.,1.));
#74822=DIRECTION('ref_axis',(1.,0.,0.));
#74823=DIRECTION('center_axis',(0.,0.,1.));
#74824=DIRECTION('ref_axis',(1.,0.,0.));
#74825=DIRECTION('center_axis',(0.,0.,1.));
#74826=DIRECTION('ref_axis',(1.,0.,0.));
#74827=DIRECTION('center_axis',(0.,0.,1.));
#74828=DIRECTION('ref_axis',(1.,0.,0.));
#74829=DIRECTION('center_axis',(0.,0.,1.));
#74830=DIRECTION('ref_axis',(1.,0.,0.));
#74831=DIRECTION('center_axis',(0.,0.,1.));
#74832=DIRECTION('ref_axis',(1.,0.,0.));
#74833=DIRECTION('center_axis',(0.,0.,1.));
#74834=DIRECTION('ref_axis',(1.,0.,0.));
#74835=DIRECTION('',(0.,0.,-1.));
#74836=DIRECTION('',(0.,0.,1.));
#74837=DIRECTION('center_axis',(0.,0.,-1.));
#74838=DIRECTION('ref_axis',(1.,0.,0.));
#74839=DIRECTION('center_axis',(0.,0.,1.));
#74840=DIRECTION('ref_axis',(1.,0.,0.));
#74841=DIRECTION('',(0.,0.,-1.));
#74842=DIRECTION('',(0.,0.,1.));
#74843=DIRECTION('center_axis',(0.,0.,-1.));
#74844=DIRECTION('ref_axis',(1.,0.,0.));
#74845=DIRECTION('center_axis',(0.,0.,1.));
#74846=DIRECTION('ref_axis',(1.,0.,0.));
#74847=DIRECTION('',(0.,0.,1.));
#74848=DIRECTION('center_axis',(0.,0.,-1.));
#74849=DIRECTION('ref_axis',(1.,0.,0.));
#74850=DIRECTION('',(0.,0.,-1.));
#74851=DIRECTION('center_axis',(0.,0.,1.));
#74852=DIRECTION('ref_axis',(1.,0.,0.));
#74853=DIRECTION('',(0.,0.,-1.));
#74854=DIRECTION('',(0.,0.,1.));
#74855=DIRECTION('center_axis',(0.,0.,-1.));
#74856=DIRECTION('ref_axis',(1.,0.,0.));
#74857=DIRECTION('center_axis',(0.,0.,1.));
#74858=DIRECTION('ref_axis',(1.,0.,0.));
#74859=DIRECTION('',(0.,0.,1.));
#74860=DIRECTION('center_axis',(0.,0.,-1.));
#74861=DIRECTION('ref_axis',(1.,0.,0.));
#74862=DIRECTION('',(0.,0.,-1.));
#74863=DIRECTION('center_axis',(0.,0.,1.));
#74864=DIRECTION('ref_axis',(1.,0.,0.));
#74865=DIRECTION('',(0.,0.,1.));
#74866=DIRECTION('center_axis',(0.,0.,-1.));
#74867=DIRECTION('ref_axis',(1.,0.,0.));
#74868=DIRECTION('',(0.,0.,-1.));
#74869=DIRECTION('center_axis',(0.,1.,0.));
#74870=DIRECTION('ref_axis',(-1.,0.,0.));
#74871=DIRECTION('',(-1.,0.,0.));
#74872=DIRECTION('',(0.,0.,1.));
#74873=DIRECTION('',(-1.,0.,0.));
#74874=DIRECTION('',(0.,0.,1.));
#74875=DIRECTION('center_axis',(0.86602540378444,0.499999999999998,0.));
#74876=DIRECTION('ref_axis',(-0.499999999999998,0.86602540378444,0.));
#74877=DIRECTION('',(-0.499999999999998,0.86602540378444,0.));
#74878=DIRECTION('',(0.,0.,1.));
#74879=DIRECTION('',(-0.499999999999998,0.86602540378444,0.));
#74880=DIRECTION('center_axis',(0.86602540378444,-0.499999999999998,0.));
#74881=DIRECTION('ref_axis',(0.499999999999998,0.86602540378444,0.));
#74882=DIRECTION('',(0.499999999999998,0.86602540378444,0.));
#74883=DIRECTION('',(0.,0.,1.));
#74884=DIRECTION('',(0.499999999999998,0.86602540378444,0.));
#74885=DIRECTION('center_axis',(0.,0.,-1.));
#74886=DIRECTION('ref_axis',(-1.,0.,0.));
#74887=DIRECTION('center_axis',(0.,0.,-1.));
#74888=DIRECTION('ref_axis',(-1.,0.,0.));
#74889=DIRECTION('center_axis',(0.,0.,-1.));
#74890=DIRECTION('ref_axis',(-1.,0.,0.));
#74891=DIRECTION('',(1.,0.,0.));
#74892=DIRECTION('center_axis',(0.,0.,-1.));
#74893=DIRECTION('ref_axis',(-1.,0.,0.));
#74894=DIRECTION('center_axis',(0.,0.,-1.));
#74895=DIRECTION('ref_axis',(-1.,0.,0.));
#74896=DIRECTION('',(0.499999999999983,-0.866025403784448,0.));
#74897=DIRECTION('center_axis',(0.,0.,-1.));
#74898=DIRECTION('ref_axis',(-1.,0.,0.));
#74899=DIRECTION('',(-0.499999999999983,-0.866025403784448,0.));
#74900=DIRECTION('center_axis',(0.,0.,-1.));
#74901=DIRECTION('ref_axis',(-1.,0.,0.));
#74902=DIRECTION('',(1.,0.,0.));
#74903=DIRECTION('center_axis',(0.,0.,1.));
#74904=DIRECTION('ref_axis',(1.,0.,0.));
#74905=DIRECTION('center_axis',(0.,0.,-1.));
#74906=DIRECTION('ref_axis',(-1.,0.,0.));
#74907=DIRECTION('center_axis',(0.,0.,1.));
#74908=DIRECTION('ref_axis',(1.,0.,0.));
#74909=DIRECTION('center_axis',(0.,0.,-1.));
#74910=DIRECTION('ref_axis',(-1.,0.,0.));
#74911=DIRECTION('center_axis',(0.,0.,1.));
#74912=DIRECTION('ref_axis',(1.,0.,0.));
#74913=DIRECTION('center_axis',(0.,0.,-1.));
#74914=DIRECTION('ref_axis',(-1.,0.,0.));
#74915=DIRECTION('center_axis',(0.,0.,1.));
#74916=DIRECTION('ref_axis',(1.,0.,0.));
#74917=DIRECTION('center_axis',(0.,0.,-1.));
#74918=DIRECTION('ref_axis',(-1.,0.,0.));
#74919=DIRECTION('',(-0.499999999999983,-0.866025403784448,0.));
#74920=DIRECTION('center_axis',(0.,0.,1.));
#74921=DIRECTION('ref_axis',(1.,0.,0.));
#74922=DIRECTION('center_axis',(0.,0.,-1.));
#74923=DIRECTION('ref_axis',(-1.,0.,0.));
#74924=DIRECTION('',(0.499999999999983,-0.866025403784448,0.));
#74925=DIRECTION('center_axis',(0.,0.,1.));
#74926=DIRECTION('ref_axis',(1.,0.,0.));
#74927=DIRECTION('center_axis',(0.,0.,-1.));
#74928=DIRECTION('ref_axis',(1.,0.,0.));
#74929=DIRECTION('',(0.85716730070211,1.04972719113862E-16,0.515038074910057));
#74930=DIRECTION('center_axis',(0.,-1.,0.));
#74931=DIRECTION('ref_axis',(1.,0.,0.));
#74932=DIRECTION('',(0.,0.,1.));
#74933=DIRECTION('center_axis',(-0.866025403784449,-0.499999999999983,0.));
#74934=DIRECTION('ref_axis',(0.499999999999983,-0.866025403784448,0.));
#74935=DIRECTION('',(0.,0.,1.));
#74936=DIRECTION('center_axis',(-0.866025403784449,0.499999999999983,0.));
#74937=DIRECTION('ref_axis',(-0.499999999999983,-0.866025403784448,0.));
#74938=DIRECTION('center_axis',(0.,0.,-1.));
#74939=DIRECTION('ref_axis',(-1.,0.,0.));
#74940=DIRECTION('center_axis',(0.,0.,1.));
#74941=DIRECTION('ref_axis',(1.,0.,0.));
#74942=DIRECTION('center_axis',(0.,0.,1.));
#74943=DIRECTION('ref_axis',(1.,0.,0.));
#74944=DIRECTION('',(0.70710678118654,8.65956056235484E-17,-0.707106781186555));
#74945=DIRECTION('center_axis',(0.,0.,1.));
#74946=DIRECTION('ref_axis',(1.,0.,0.));
#74947=DIRECTION('center_axis',(0.,0.,-1.));
#74948=DIRECTION('ref_axis',(1.,0.,0.));
#74949=DIRECTION('center_axis',(0.,0.,-1.));
#74950=DIRECTION('ref_axis',(1.,0.,0.));
#74951=DIRECTION('center_axis',(0.,0.,1.));
#74952=DIRECTION('ref_axis',(1.,0.,0.));
#74953=DIRECTION('',(-0.707106781186541,-8.65956056235486E-17,-0.707106781186554));
#74954=DIRECTION('center_axis',(0.,0.,1.));
#74955=DIRECTION('ref_axis',(1.,0.,0.));
#74956=DIRECTION('axis',(0.,0.,1.));
#74957=DIRECTION('refdir',(1.,0.,0.));
#74958=DIRECTION('center_axis',(0.,-1.,0.));
#74959=DIRECTION('ref_axis',(1.,0.,0.));
#74960=DIRECTION('',(0.,1.,0.));
#74961=DIRECTION('center_axis',(0.,-1.,0.));
#74962=DIRECTION('ref_axis',(1.,0.,0.));
#74963=DIRECTION('center_axis',(0.,-1.,0.));
#74964=DIRECTION('ref_axis',(1.,0.,0.));
#74965=DIRECTION('',(0.,1.,0.));
#74966=DIRECTION('center_axis',(0.,-1.,0.));
#74967=DIRECTION('ref_axis',(1.,0.,0.));
#74968=DIRECTION('',(0.,1.,0.));
#74969=DIRECTION('center_axis',(0.,-1.,0.));
#74970=DIRECTION('ref_axis',(1.,0.,0.));
#74971=DIRECTION('',(0.,1.,0.));
#74972=DIRECTION('center_axis',(0.,-1.,0.));
#74973=DIRECTION('ref_axis',(1.,0.,0.));
#74974=DIRECTION('',(0.,1.,0.));
#74975=DIRECTION('center_axis',(0.,-1.,0.));
#74976=DIRECTION('ref_axis',(1.,0.,0.));
#74977=DIRECTION('',(0.,1.,0.));
#74978=DIRECTION('center_axis',(0.,-1.,0.));
#74979=DIRECTION('ref_axis',(1.,0.,1.20186524993251E-14));
#74980=DIRECTION('',(0.,-1.,0.));
#74981=DIRECTION('center_axis',(0.,-1.,0.));
#74982=DIRECTION('ref_axis',(1.,0.,1.20186524993251E-14));
#74983=DIRECTION('center_axis',(0.,-1.,0.));
#74984=DIRECTION('ref_axis',(1.,0.,1.20186524993251E-14));
#74985=DIRECTION('',(0.,-1.,0.));
#74986=DIRECTION('center_axis',(0.,-1.,0.));
#74987=DIRECTION('ref_axis',(1.,0.,1.20186524993251E-14));
#74988=DIRECTION('center_axis',(0.,-1.,0.));
#74989=DIRECTION('ref_axis',(1.,0.,1.20186524993251E-14));
#74990=DIRECTION('',(0.,-1.,0.));
#74991=DIRECTION('center_axis',(0.,-1.,0.));
#74992=DIRECTION('ref_axis',(1.,0.,1.20186524993251E-14));
#74993=DIRECTION('',(0.,-1.,0.));
#74994=DIRECTION('center_axis',(0.,-1.,0.));
#74995=DIRECTION('ref_axis',(1.,0.,1.20186524993251E-14));
#74996=DIRECTION('',(0.,-1.,0.));
#74997=DIRECTION('center_axis',(0.,-1.,0.));
#74998=DIRECTION('ref_axis',(1.,0.,1.20186524993251E-14));
#74999=DIRECTION('',(0.,-1.,0.));
#75000=DIRECTION('center_axis',(0.,1.,0.));
#75001=DIRECTION('ref_axis',(0.,0.,1.));
#75002=DIRECTION('center_axis',(0.,1.,0.));
#75003=DIRECTION('ref_axis',(1.,0.,0.));
#75004=DIRECTION('center_axis',(0.,1.,0.));
#75005=DIRECTION('ref_axis',(1.,0.,0.));
#75006=DIRECTION('center_axis',(0.,1.,0.));
#75007=DIRECTION('ref_axis',(0.,0.,1.));
#75008=DIRECTION('center_axis',(0.,-1.,0.));
#75009=DIRECTION('ref_axis',(1.,0.,0.));
#75010=DIRECTION('center_axis',(0.,-1.,0.));
#75011=DIRECTION('ref_axis',(1.,0.,0.));
#75012=DIRECTION('center_axis',(0.,1.,0.));
#75013=DIRECTION('ref_axis',(1.,0.,1.20186524993251E-14));
#75014=DIRECTION('center_axis',(0.,-1.,0.));
#75015=DIRECTION('ref_axis',(1.,0.,1.20186524993251E-14));
#75016=DIRECTION('center_axis',(0.,1.,0.));
#75017=DIRECTION('ref_axis',(1.,0.,0.));
#75018=DIRECTION('center_axis',(0.,-1.,0.));
#75019=DIRECTION('ref_axis',(1.,0.,0.));
#75020=DIRECTION('',(0.70710678118654,-0.707106781186555,8.65956056235484E-17));
#75021=DIRECTION('center_axis',(0.,-1.,0.));
#75022=DIRECTION('ref_axis',(1.,0.,0.));
#75023=DIRECTION('center_axis',(0.,-1.,0.));
#75024=DIRECTION('ref_axis',(1.,0.,0.));
#75025=DIRECTION('center_axis',(0.,-1.,0.));
#75026=DIRECTION('ref_axis',(1.,0.,0.));
#75027=DIRECTION('center_axis',(0.,-1.,0.));
#75028=DIRECTION('ref_axis',(1.,0.,0.));
#75029=DIRECTION('center_axis',(0.,-1.,0.));
#75030=DIRECTION('ref_axis',(1.,0.,0.));
#75031=DIRECTION('center_axis',(0.,-1.,0.));
#75032=DIRECTION('ref_axis',(1.,0.,0.));
#75033=DIRECTION('center_axis',(0.,-1.,0.));
#75034=DIRECTION('ref_axis',(1.,0.,0.));
#75035=DIRECTION('',(0.,1.,0.));
#75036=DIRECTION('',(0.,-1.,0.));
#75037=DIRECTION('center_axis',(0.,1.,0.));
#75038=DIRECTION('ref_axis',(1.,0.,0.));
#75039=DIRECTION('center_axis',(0.,-1.,0.));
#75040=DIRECTION('ref_axis',(1.,0.,0.));
#75041=DIRECTION('',(0.,1.,0.));
#75042=DIRECTION('',(0.,-1.,0.));
#75043=DIRECTION('center_axis',(0.,1.,0.));
#75044=DIRECTION('ref_axis',(1.,0.,0.));
#75045=DIRECTION('center_axis',(0.,-1.,0.));
#75046=DIRECTION('ref_axis',(1.,0.,0.));
#75047=DIRECTION('',(0.,-1.,0.));
#75048=DIRECTION('center_axis',(0.,1.,0.));
#75049=DIRECTION('ref_axis',(1.,0.,0.));
#75050=DIRECTION('',(0.,1.,0.));
#75051=DIRECTION('center_axis',(0.,-1.,0.));
#75052=DIRECTION('ref_axis',(1.,0.,0.));
#75053=DIRECTION('',(0.,1.,0.));
#75054=DIRECTION('',(0.,-1.,0.));
#75055=DIRECTION('center_axis',(0.,1.,0.));
#75056=DIRECTION('ref_axis',(1.,0.,0.));
#75057=DIRECTION('center_axis',(0.,-1.,0.));
#75058=DIRECTION('ref_axis',(1.,0.,0.));
#75059=DIRECTION('',(0.,-1.,0.));
#75060=DIRECTION('center_axis',(0.,1.,0.));
#75061=DIRECTION('ref_axis',(1.,0.,0.));
#75062=DIRECTION('',(0.,1.,0.));
#75063=DIRECTION('center_axis',(0.,-1.,0.));
#75064=DIRECTION('ref_axis',(1.,0.,0.));
#75065=DIRECTION('',(0.,-1.,0.));
#75066=DIRECTION('center_axis',(0.,1.,0.));
#75067=DIRECTION('ref_axis',(1.,0.,0.));
#75068=DIRECTION('',(0.,1.,0.));
#75069=DIRECTION('center_axis',(0.866025403784448,0.,0.499999999999983));
#75070=DIRECTION('ref_axis',(-0.499999999999983,0.,0.866025403784448));
#75071=DIRECTION('',(-0.499999999999983,0.,0.866025403784448));
#75072=DIRECTION('',(0.,-1.,0.));
#75073=DIRECTION('',(-0.499999999999983,0.,0.866025403784448));
#75074=DIRECTION('',(0.,-1.,0.));
#75075=DIRECTION('center_axis',(0.866025403784453,0.,-0.499999999999976));
#75076=DIRECTION('ref_axis',(0.499999999999976,0.,0.866025403784453));
#75077=DIRECTION('',(0.499999999999976,0.,0.866025403784453));
#75078=DIRECTION('',(0.,-1.,0.));
#75079=DIRECTION('',(0.499999999999976,0.,0.866025403784453));
#75080=DIRECTION('center_axis',(0.,0.,-1.));
#75081=DIRECTION('ref_axis',(1.,0.,0.));
#75082=DIRECTION('',(1.,0.,0.));
#75083=DIRECTION('',(0.,-1.,0.));
#75084=DIRECTION('',(1.,0.,0.));
#75085=DIRECTION('center_axis',(0.,1.,0.));
#75086=DIRECTION('ref_axis',(0.,0.,1.));
#75087=DIRECTION('center_axis',(0.,1.,0.));
#75088=DIRECTION('ref_axis',(0.,0.,1.));
#75089=DIRECTION('center_axis',(0.,1.,0.));
#75090=DIRECTION('ref_axis',(0.,0.,1.));
#75091=DIRECTION('',(0.499999999999976,0.,-0.866025403784453));
#75092=DIRECTION('center_axis',(0.,1.,0.));
#75093=DIRECTION('ref_axis',(0.,0.,1.));
#75094=DIRECTION('center_axis',(0.,1.,0.));
#75095=DIRECTION('ref_axis',(0.,0.,1.));
#75096=DIRECTION('',(-0.499999999999983,0.,-0.866025403784448));
#75097=DIRECTION('center_axis',(0.,1.,0.));
#75098=DIRECTION('ref_axis',(0.,0.,1.));
#75099=DIRECTION('',(-1.,0.,0.));
#75100=DIRECTION('center_axis',(0.,1.,0.));
#75101=DIRECTION('ref_axis',(0.,0.,1.));
#75102=DIRECTION('',(0.499999999999976,0.,-0.866025403784453));
#75103=DIRECTION('center_axis',(0.,-1.,0.));
#75104=DIRECTION('ref_axis',(1.,0.,0.));
#75105=DIRECTION('center_axis',(0.,1.,0.));
#75106=DIRECTION('ref_axis',(0.,0.,1.));
#75107=DIRECTION('center_axis',(0.,-1.,0.));
#75108=DIRECTION('ref_axis',(1.,0.,0.));
#75109=DIRECTION('center_axis',(0.,1.,0.));
#75110=DIRECTION('ref_axis',(0.,0.,1.));
#75111=DIRECTION('center_axis',(0.,-1.,0.));
#75112=DIRECTION('ref_axis',(1.,0.,0.));
#75113=DIRECTION('center_axis',(0.,1.,0.));
#75114=DIRECTION('ref_axis',(0.,0.,1.));
#75115=DIRECTION('center_axis',(0.,-1.,0.));
#75116=DIRECTION('ref_axis',(1.,0.,0.));
#75117=DIRECTION('center_axis',(0.,1.,0.));
#75118=DIRECTION('ref_axis',(0.,0.,1.));
#75119=DIRECTION('',(-1.,0.,0.));
#75120=DIRECTION('center_axis',(0.,-1.,0.));
#75121=DIRECTION('ref_axis',(1.,0.,0.));
#75122=DIRECTION('center_axis',(0.,1.,0.));
#75123=DIRECTION('ref_axis',(0.,0.,1.));
#75124=DIRECTION('',(-0.499999999999983,0.,-0.866025403784448));
#75125=DIRECTION('center_axis',(0.,-1.,0.));
#75126=DIRECTION('ref_axis',(1.,0.,0.));
#75127=DIRECTION('center_axis',(0.,1.,0.));
#75128=DIRECTION('ref_axis',(1.,0.,0.));
#75129=DIRECTION('',(0.857167300702109,-0.51503807491006,1.04972719113861E-16));
#75130=DIRECTION('center_axis',(-0.866025403784453,0.,-0.499999999999976));
#75131=DIRECTION('ref_axis',(0.499999999999976,0.,-0.866025403784453));
#75132=DIRECTION('',(0.,-1.,0.));
#75133=DIRECTION('center_axis',(-0.866025403784448,0.,0.499999999999983));
#75134=DIRECTION('ref_axis',(-0.499999999999983,0.,-0.866025403784448));
#75135=DIRECTION('',(0.,-1.,0.));
#75136=DIRECTION('center_axis',(0.,0.,1.));
#75137=DIRECTION('ref_axis',(-1.,0.,0.));
#75138=DIRECTION('center_axis',(0.,1.,0.));
#75139=DIRECTION('ref_axis',(0.,0.,1.));
#75140=DIRECTION('center_axis',(0.,-1.,0.));
#75141=DIRECTION('ref_axis',(1.,0.,0.));
#75142=DIRECTION('center_axis',(0.,-1.,0.));
#75143=DIRECTION('ref_axis',(1.,0.,0.));
#75144=DIRECTION('',(0.707106781186534,0.707106781186561,8.65956056235477E-17));
#75145=DIRECTION('center_axis',(0.,-1.,0.));
#75146=DIRECTION('ref_axis',(1.,0.,0.));
#75147=DIRECTION('center_axis',(0.,1.,0.));
#75148=DIRECTION('ref_axis',(1.,0.,0.));
#75149=DIRECTION('center_axis',(0.,1.,0.));
#75150=DIRECTION('ref_axis',(1.,0.,0.));
#75151=DIRECTION('center_axis',(0.,-1.,0.));
#75152=DIRECTION('ref_axis',(1.,0.,0.));
#75153=DIRECTION('',(-0.707106781186538,0.707106781186557,-8.65956056235482E-17));
#75154=DIRECTION('center_axis',(0.,-1.,0.));
#75155=DIRECTION('ref_axis',(0.,0.,-1.));
#75156=DIRECTION('axis',(0.,0.,1.));
#75157=DIRECTION('refdir',(1.,0.,0.));
#75158=DIRECTION('center_axis',(0.,0.,1.));
#75159=DIRECTION('ref_axis',(1.,0.,0.));
#75160=DIRECTION('',(0.,0.,-1.));
#75161=DIRECTION('center_axis',(0.,0.,1.));
#75162=DIRECTION('ref_axis',(1.,0.,0.));
#75163=DIRECTION('center_axis',(0.,0.,1.));
#75164=DIRECTION('ref_axis',(1.,0.,0.));
#75165=DIRECTION('',(0.,0.,-1.));
#75166=DIRECTION('center_axis',(0.,0.,1.));
#75167=DIRECTION('ref_axis',(1.,0.,0.));
#75168=DIRECTION('',(0.,0.,-1.));
#75169=DIRECTION('center_axis',(0.,0.,1.));
#75170=DIRECTION('ref_axis',(1.,0.,0.));
#75171=DIRECTION('',(0.,0.,-1.));
#75172=DIRECTION('center_axis',(0.,0.,1.));
#75173=DIRECTION('ref_axis',(1.,0.,0.));
#75174=DIRECTION('',(0.,0.,-1.));
#75175=DIRECTION('center_axis',(0.,0.,1.));
#75176=DIRECTION('ref_axis',(1.,0.,0.));
#75177=DIRECTION('',(0.,0.,-1.));
#75178=DIRECTION('center_axis',(0.,0.,1.));
#75179=DIRECTION('ref_axis',(1.,0.,0.));
#75180=DIRECTION('',(0.,0.,-1.));
#75181=DIRECTION('center_axis',(0.,0.,1.));
#75182=DIRECTION('ref_axis',(1.,0.,0.));
#75183=DIRECTION('',(0.,0.,-1.));
#75184=DIRECTION('center_axis',(0.,0.,1.));
#75185=DIRECTION('ref_axis',(1.,0.,0.));
#75186=DIRECTION('center_axis',(0.,0.,1.));
#75187=DIRECTION('ref_axis',(0.305350463707712,-0.95224004028054,0.));
#75188=DIRECTION('',(0.,0.,1.));
#75189=DIRECTION('center_axis',(0.,0.,1.));
#75190=DIRECTION('ref_axis',(1.,2.70419681234815E-14,0.));
#75191=DIRECTION('center_axis',(0.,0.,1.));
#75192=DIRECTION('ref_axis',(1.,2.70419681234815E-14,0.));
#75193=DIRECTION('',(0.,0.,1.));
#75194=DIRECTION('center_axis',(0.,0.,1.));
#75195=DIRECTION('ref_axis',(1.,2.70419681234815E-14,0.));
#75196=DIRECTION('',(0.,0.,1.));
#75197=DIRECTION('center_axis',(0.,0.,1.));
#75198=DIRECTION('ref_axis',(1.,2.70419681234815E-14,0.));
#75199=DIRECTION('',(0.,0.,1.));
#75200=DIRECTION('center_axis',(0.,0.,1.));
#75201=DIRECTION('ref_axis',(1.,2.70419681234815E-14,0.));
#75202=DIRECTION('',(0.,0.,1.));
#75203=DIRECTION('center_axis',(0.,0.,1.));
#75204=DIRECTION('ref_axis',(1.,2.70419681234815E-14,0.));
#75205=DIRECTION('',(0.,0.,1.));
#75206=DIRECTION('center_axis',(0.,0.,1.));
#75207=DIRECTION('ref_axis',(1.,2.70419681234815E-14,0.));
#75208=DIRECTION('',(0.,0.,1.));
#75209=DIRECTION('center_axis',(0.,0.,1.));
#75210=DIRECTION('ref_axis',(1.,0.,0.));
#75211=DIRECTION('center_axis',(0.,0.,1.));
#75212=DIRECTION('ref_axis',(1.,0.,0.));
#75213=DIRECTION('center_axis',(0.,0.,1.));
#75214=DIRECTION('ref_axis',(1.,0.,0.));
#75215=DIRECTION('center_axis',(0.,0.,1.));
#75216=DIRECTION('ref_axis',(1.,0.,0.));
#75217=DIRECTION('center_axis',(0.,0.,1.));
#75218=DIRECTION('ref_axis',(1.,0.,0.));
#75219=DIRECTION('center_axis',(0.,0.,-1.));
#75220=DIRECTION('ref_axis',(1.,2.70419681234815E-14,0.));
#75221=DIRECTION('center_axis',(0.,0.,1.));
#75222=DIRECTION('ref_axis',(1.,2.70419681234815E-14,0.));
#75223=DIRECTION('center_axis',(0.866025403784442,0.499999999999995,0.));
#75224=DIRECTION('ref_axis',(0.499999999999995,-0.866025403784442,0.));
#75225=DIRECTION('',(0.499999999999995,-0.866025403784442,0.));
#75226=DIRECTION('',(0.,0.,-1.));
#75227=DIRECTION('',(0.499999999999995,-0.866025403784442,0.));
#75228=DIRECTION('',(0.,0.,-1.));
#75229=DIRECTION('center_axis',(0.,1.,0.));
#75230=DIRECTION('ref_axis',(1.,0.,0.));
#75231=DIRECTION('',(1.,0.,0.));
#75232=DIRECTION('',(0.,0.,-1.));
#75233=DIRECTION('',(1.,0.,0.));
#75234=DIRECTION('center_axis',(-0.866025403784442,0.499999999999995,0.));
#75235=DIRECTION('ref_axis',(0.499999999999995,0.866025403784442,0.));
#75236=DIRECTION('',(0.499999999999995,0.866025403784442,0.));
#75237=DIRECTION('',(0.,0.,-1.));
#75238=DIRECTION('',(0.499999999999995,0.866025403784442,0.));
#75239=DIRECTION('center_axis',(-0.866025403784442,-0.499999999999993,0.));
#75240=DIRECTION('ref_axis',(-0.499999999999993,0.866025403784442,0.));
#75241=DIRECTION('',(-0.499999999999993,0.866025403784442,0.));
#75242=DIRECTION('',(0.,0.,-1.));
#75243=DIRECTION('',(-0.499999999999993,0.866025403784442,0.));
#75244=DIRECTION('center_axis',(0.,-1.,0.));
#75245=DIRECTION('ref_axis',(-1.,0.,0.));
#75246=DIRECTION('',(-1.,0.,0.));
#75247=DIRECTION('',(0.,0.,-1.));
#75248=DIRECTION('',(-1.,0.,0.));
#75249=DIRECTION('center_axis',(0.866025403784442,-0.499999999999993,0.));
#75250=DIRECTION('ref_axis',(-0.499999999999993,-0.866025403784442,0.));
#75251=DIRECTION('',(-0.499999999999993,-0.866025403784442,0.));
#75252=DIRECTION('',(-0.499999999999993,-0.866025403784442,0.));
#75253=DIRECTION('center_axis',(0.,0.,-1.));
#75254=DIRECTION('ref_axis',(-1.,0.,0.));
#75255=DIRECTION('center_axis',(0.,0.,-1.));
#75256=DIRECTION('ref_axis',(-1.,0.,0.));
#75257=DIRECTION('center_axis',(0.,0.,1.));
#75258=DIRECTION('ref_axis',(1.,0.,0.));
#75259=DIRECTION('center_axis',(0.,0.,1.));
#75260=DIRECTION('ref_axis',(1.,0.,0.));
#75261=DIRECTION('',(0.707106781186532,8.65956056235474E-17,-0.707106781186563));
#75262=DIRECTION('center_axis',(0.,0.,1.));
#75263=DIRECTION('ref_axis',(-0.974166089596959,-0.225832747579639,0.));
#75264=DIRECTION('center_axis',(0.,0.,1.));
#75265=DIRECTION('ref_axis',(1.,0.,0.));
#75266=DIRECTION('center_axis',(0.,0.,1.));
#75267=DIRECTION('ref_axis',(1.,0.,0.));
#75268=DIRECTION('center_axis',(0.,0.,1.));
#75269=DIRECTION('ref_axis',(1.,0.,0.));
#75270=DIRECTION('',(0.707106781186547,8.65956056235493E-17,-0.707106781186547));
#75271=DIRECTION('center_axis',(0.,0.,1.));
#75272=DIRECTION('ref_axis',(1.,0.,0.));
#75273=DIRECTION('axis',(0.,0.,1.));
#75274=DIRECTION('refdir',(1.,0.,0.));
#75275=DIRECTION('center_axis',(0.,-1.,0.));
#75276=DIRECTION('ref_axis',(1.,0.,0.));
#75277=DIRECTION('',(0.,1.,0.));
#75278=DIRECTION('center_axis',(0.,1.,0.));
#75279=DIRECTION('ref_axis',(1.,0.,0.));
#75280=DIRECTION('center_axis',(0.,-1.,0.));
#75281=DIRECTION('ref_axis',(1.,0.,0.));
#75282=DIRECTION('',(0.,1.,0.));
#75283=DIRECTION('center_axis',(0.,-1.,0.));
#75284=DIRECTION('ref_axis',(1.,0.,0.));
#75285=DIRECTION('',(0.,1.,0.));
#75286=DIRECTION('center_axis',(0.,-1.,0.));
#75287=DIRECTION('ref_axis',(1.,0.,0.));
#75288=DIRECTION('',(0.,1.,0.));
#75289=DIRECTION('center_axis',(0.,-1.,0.));
#75290=DIRECTION('ref_axis',(1.,0.,0.));
#75291=DIRECTION('',(0.,1.,0.));
#75292=DIRECTION('center_axis',(0.,-1.,0.));
#75293=DIRECTION('ref_axis',(1.,0.,0.));
#75294=DIRECTION('',(0.,1.,0.));
#75295=DIRECTION('center_axis',(0.,-1.,0.));
#75296=DIRECTION('ref_axis',(1.,0.,0.));
#75297=DIRECTION('',(0.,1.,0.));
#75298=DIRECTION('center_axis',(0.,-1.,0.));
#75299=DIRECTION('ref_axis',(1.,0.,0.));
#75300=DIRECTION('',(0.,1.,0.));
#75301=DIRECTION('center_axis',(0.,-1.,0.));
#75302=DIRECTION('ref_axis',(1.,0.,0.));
#75303=DIRECTION('',(0.,1.,0.));
#75304=DIRECTION('center_axis',(0.,-1.,0.));
#75305=DIRECTION('ref_axis',(1.,0.,0.));
#75306=DIRECTION('',(0.,1.,0.));
#75307=DIRECTION('center_axis',(0.,-1.,0.));
#75308=DIRECTION('ref_axis',(1.,0.,0.));
#75309=DIRECTION('',(0.,1.,0.));
#75310=DIRECTION('center_axis',(0.,-1.,0.));
#75311=DIRECTION('ref_axis',(1.,0.,0.));
#75312=DIRECTION('',(0.,1.,0.));
#75313=DIRECTION('center_axis',(0.,-1.,0.));
#75314=DIRECTION('ref_axis',(1.,0.,0.));
#75315=DIRECTION('',(0.,1.,0.));
#75316=DIRECTION('center_axis',(0.,-1.,0.));
#75317=DIRECTION('ref_axis',(1.,0.,8.34187923537817E-14));
#75318=DIRECTION('',(0.,-1.,0.));
#75319=DIRECTION('center_axis',(0.,-1.,0.));
#75320=DIRECTION('ref_axis',(1.,0.,8.34187923537817E-14));
#75321=DIRECTION('center_axis',(0.,-1.,0.));
#75322=DIRECTION('ref_axis',(1.,0.,8.34187923537817E-14));
#75323=DIRECTION('',(0.,-1.,0.));
#75324=DIRECTION('center_axis',(0.,-1.,0.));
#75325=DIRECTION('ref_axis',(1.,0.,8.34187923537817E-14));
#75326=DIRECTION('',(0.,-1.,0.));
#75327=DIRECTION('center_axis',(0.,-1.,0.));
#75328=DIRECTION('ref_axis',(1.,0.,8.34187923537817E-14));
#75329=DIRECTION('',(0.,-1.,0.));
#75330=DIRECTION('center_axis',(0.,-1.,0.));
#75331=DIRECTION('ref_axis',(1.,0.,8.34187923537817E-14));
#75332=DIRECTION('',(0.,-1.,0.));
#75333=DIRECTION('center_axis',(0.,-1.,0.));
#75334=DIRECTION('ref_axis',(1.,0.,8.34187923537817E-14));
#75335=DIRECTION('',(0.,-1.,0.));
#75336=DIRECTION('center_axis',(0.,-1.,0.));
#75337=DIRECTION('ref_axis',(1.,0.,8.34187923537817E-14));
#75338=DIRECTION('',(0.,-1.,0.));
#75339=DIRECTION('center_axis',(0.,-1.,0.));
#75340=DIRECTION('ref_axis',(1.,0.,8.34187923537817E-14));
#75341=DIRECTION('',(0.,-1.,0.));
#75342=DIRECTION('center_axis',(0.,-1.,0.));
#75343=DIRECTION('ref_axis',(1.,0.,8.34187923537817E-14));
#75344=DIRECTION('',(0.,-1.,0.));
#75345=DIRECTION('center_axis',(0.,-1.,0.));
#75346=DIRECTION('ref_axis',(1.,0.,8.34187923537817E-14));
#75347=DIRECTION('',(0.,-1.,0.));
#75348=DIRECTION('center_axis',(0.,-1.,0.));
#75349=DIRECTION('ref_axis',(1.,0.,8.34187923537817E-14));
#75350=DIRECTION('',(0.,-1.,0.));
#75351=DIRECTION('center_axis',(0.,-1.,0.));
#75352=DIRECTION('ref_axis',(1.,0.,8.34187923537817E-14));
#75353=DIRECTION('',(0.,-1.,0.));
#75354=DIRECTION('center_axis',(0.,1.,0.));
#75355=DIRECTION('ref_axis',(0.,0.,1.));
#75356=DIRECTION('center_axis',(0.,-1.,0.));
#75357=DIRECTION('ref_axis',(1.,0.,0.));
#75358=DIRECTION('center_axis',(0.,-1.,0.));
#75359=DIRECTION('ref_axis',(1.,0.,0.));
#75360=DIRECTION('center_axis',(0.,1.,0.));
#75361=DIRECTION('ref_axis',(0.,0.,1.));
#75362=DIRECTION('center_axis',(0.,1.,0.));
#75363=DIRECTION('ref_axis',(1.,0.,0.));
#75364=DIRECTION('center_axis',(0.,1.,0.));
#75365=DIRECTION('ref_axis',(1.,0.,8.34187923537817E-14));
#75366=DIRECTION('center_axis',(0.,1.,0.));
#75367=DIRECTION('ref_axis',(1.,0.,0.));
#75368=DIRECTION('center_axis',(0.,-1.,0.));
#75369=DIRECTION('ref_axis',(1.,0.,8.34187923537817E-14));
#75370=DIRECTION('center_axis',(0.,1.,0.));
#75371=DIRECTION('ref_axis',(0.,0.,1.));
#75372=DIRECTION('center_axis',(-1.,0.,0.));
#75373=DIRECTION('ref_axis',(0.,0.,-1.));
#75374=DIRECTION('center_axis',(0.,-1.,0.));
#75375=DIRECTION('ref_axis',(1.,0.,0.));
#75376=DIRECTION('center_axis',(0.,-1.,0.));
#75377=DIRECTION('ref_axis',(1.,0.,0.));
#75378=DIRECTION('center_axis',(0.,-1.,0.));
#75379=DIRECTION('ref_axis',(1.,0.,0.));
#75380=DIRECTION('center_axis',(0.,1.,0.));
#75381=DIRECTION('ref_axis',(1.,0.,0.));
#75382=DIRECTION('center_axis',(0.,1.,0.));
#75383=DIRECTION('ref_axis',(1.,0.,0.));
#75384=DIRECTION('center_axis',(0.,1.,0.));
#75385=DIRECTION('ref_axis',(1.,0.,0.));
#75386=DIRECTION('',(0.707106781186548,-0.707106781186548,-8.65956056235493E-17));
#75387=DIRECTION('center_axis',(0.,1.,0.));
#75388=DIRECTION('ref_axis',(1.,0.,0.));
#75389=DIRECTION('center_axis',(0.,1.,0.));
#75390=DIRECTION('ref_axis',(1.,0.,0.));
#75391=DIRECTION('center_axis',(-0.493533981978479,0.,-0.869726513699833));
#75392=DIRECTION('ref_axis',(0.869726513699833,0.,-0.493533981978479));
#75393=DIRECTION('',(0.,-1.,0.));
#75394=DIRECTION('',(0.869726513699833,0.,-0.493533981978479));
#75395=DIRECTION('',(0.,-1.,0.));
#75396=DIRECTION('center_axis',(0.,-1.,0.));
#75397=DIRECTION('ref_axis',(-0.17364817766693,0.,-0.984807753012208));
#75398=DIRECTION('center_axis',(0.,-1.,0.));
#75399=DIRECTION('ref_axis',(1.,0.,0.));
#75400=DIRECTION('',(-0.986074150277955,0.,-0.166306254102511));
#75401=DIRECTION('center_axis',(-0.166306254102511,0.,0.986074150277955));
#75402=DIRECTION('ref_axis',(-0.986074150277955,0.,-0.166306254102511));
#75403=DIRECTION('',(0.,1.,0.));
#75404=DIRECTION('center_axis',(0.,1.,0.));
#75405=DIRECTION('ref_axis',(1.,0.,0.));
#75406=DIRECTION('center_axis',(0.,1.,0.));
#75407=DIRECTION('ref_axis',(1.,0.,0.));
#75408=DIRECTION('',(0.,-1.,0.));
#75409=DIRECTION('center_axis',(0.,-1.,0.));
#75410=DIRECTION('ref_axis',(1.,0.,0.));
#75411=DIRECTION('',(0.,1.,0.));
#75412=DIRECTION('center_axis',(0.,1.,0.));
#75413=DIRECTION('ref_axis',(1.,0.,0.));
#75414=DIRECTION('',(0.,-1.,0.));
#75415=DIRECTION('center_axis',(0.,-1.,0.));
#75416=DIRECTION('ref_axis',(1.,0.,0.));
#75417=DIRECTION('',(0.,1.,0.));
#75418=DIRECTION('center_axis',(0.,1.,0.));
#75419=DIRECTION('ref_axis',(1.,0.,0.));
#75420=DIRECTION('',(0.,-1.,0.));
#75421=DIRECTION('center_axis',(0.,-1.,0.));
#75422=DIRECTION('ref_axis',(1.,0.,0.));
#75423=DIRECTION('',(0.,1.,0.));
#75424=DIRECTION('center_axis',(0.,1.,0.));
#75425=DIRECTION('ref_axis',(1.,0.,0.));
#75426=DIRECTION('',(0.,-1.,0.));
#75427=DIRECTION('center_axis',(0.,-1.,0.));
#75428=DIRECTION('ref_axis',(1.,0.,0.));
#75429=DIRECTION('',(0.,1.,0.));
#75430=DIRECTION('center_axis',(0.,1.,0.));
#75431=DIRECTION('ref_axis',(1.,0.,0.));
#75432=DIRECTION('',(0.,-1.,0.));
#75433=DIRECTION('center_axis',(0.,-1.,0.));
#75434=DIRECTION('ref_axis',(1.,0.,0.));
#75435=DIRECTION('',(0.,1.,0.));
#75436=DIRECTION('center_axis',(0.,1.,0.));
#75437=DIRECTION('ref_axis',(1.,0.,0.));
#75438=DIRECTION('',(0.,-1.,0.));
#75439=DIRECTION('center_axis',(0.,-1.,0.));
#75440=DIRECTION('ref_axis',(1.,0.,0.));
#75441=DIRECTION('',(0.,1.,0.));
#75442=DIRECTION('center_axis',(0.,1.,0.));
#75443=DIRECTION('ref_axis',(1.,0.,0.));
#75444=DIRECTION('',(0.,-1.,0.));
#75445=DIRECTION('center_axis',(0.,-1.,0.));
#75446=DIRECTION('ref_axis',(1.,0.,0.));
#75447=DIRECTION('',(0.,1.,0.));
#75448=DIRECTION('center_axis',(0.,1.,0.));
#75449=DIRECTION('ref_axis',(1.,0.,0.));
#75450=DIRECTION('',(0.,-1.,0.));
#75451=DIRECTION('center_axis',(0.,-1.,0.));
#75452=DIRECTION('ref_axis',(1.,0.,0.));
#75453=DIRECTION('',(0.,1.,0.));
#75454=DIRECTION('center_axis',(0.,1.,0.));
#75455=DIRECTION('ref_axis',(1.,0.,0.));
#75456=DIRECTION('',(0.,-1.,0.));
#75457=DIRECTION('center_axis',(0.,-1.,0.));
#75458=DIRECTION('ref_axis',(1.,0.,0.));
#75459=DIRECTION('',(0.,1.,0.));
#75460=DIRECTION('center_axis',(0.,1.,0.));
#75461=DIRECTION('ref_axis',(1.,0.,0.));
#75462=DIRECTION('',(0.,-1.,0.));
#75463=DIRECTION('center_axis',(0.,-1.,0.));
#75464=DIRECTION('ref_axis',(1.,0.,0.));
#75465=DIRECTION('',(0.,1.,0.));
#75466=DIRECTION('center_axis',(0.,1.,0.));
#75467=DIRECTION('ref_axis',(1.,0.,0.));
#75468=DIRECTION('',(0.,-1.,0.));
#75469=DIRECTION('center_axis',(0.,-1.,0.));
#75470=DIRECTION('ref_axis',(1.,0.,0.));
#75471=DIRECTION('',(0.,1.,0.));
#75472=DIRECTION('center_axis',(0.,1.,0.));
#75473=DIRECTION('ref_axis',(1.,0.,0.));
#75474=DIRECTION('',(0.,-1.,0.));
#75475=DIRECTION('center_axis',(0.,-1.,0.));
#75476=DIRECTION('ref_axis',(1.,0.,0.));
#75477=DIRECTION('',(0.,1.,0.));
#75478=DIRECTION('center_axis',(0.,1.,0.));
#75479=DIRECTION('ref_axis',(1.,0.,0.));
#75480=DIRECTION('',(0.,-1.,0.));
#75481=DIRECTION('center_axis',(0.,-1.,0.));
#75482=DIRECTION('ref_axis',(1.,0.,0.));
#75483=DIRECTION('',(0.,1.,0.));
#75484=DIRECTION('center_axis',(0.,1.,0.));
#75485=DIRECTION('ref_axis',(1.,0.,0.));
#75486=DIRECTION('',(0.,-1.,0.));
#75487=DIRECTION('center_axis',(0.,-1.,0.));
#75488=DIRECTION('ref_axis',(1.,0.,0.));
#75489=DIRECTION('',(0.,1.,0.));
#75490=DIRECTION('center_axis',(0.,1.,0.));
#75491=DIRECTION('ref_axis',(1.,0.,0.));
#75492=DIRECTION('',(0.,-1.,0.));
#75493=DIRECTION('center_axis',(0.,-1.,0.));
#75494=DIRECTION('ref_axis',(1.,0.,0.));
#75495=DIRECTION('',(0.,1.,0.));
#75496=DIRECTION('center_axis',(0.,1.,0.));
#75497=DIRECTION('ref_axis',(1.,0.,0.));
#75498=DIRECTION('',(0.,-1.,0.));
#75499=DIRECTION('center_axis',(0.,-1.,0.));
#75500=DIRECTION('ref_axis',(1.,0.,0.));
#75501=DIRECTION('',(0.,1.,0.));
#75502=DIRECTION('center_axis',(0.,1.,0.));
#75503=DIRECTION('ref_axis',(1.,0.,0.));
#75504=DIRECTION('',(0.,-1.,0.));
#75505=DIRECTION('center_axis',(0.,-1.,0.));
#75506=DIRECTION('ref_axis',(1.,0.,0.));
#75507=DIRECTION('',(0.,1.,0.));
#75508=DIRECTION('center_axis',(0.,1.,0.));
#75509=DIRECTION('ref_axis',(1.,0.,0.));
#75510=DIRECTION('',(0.,-1.,0.));
#75511=DIRECTION('center_axis',(0.,-1.,0.));
#75512=DIRECTION('ref_axis',(1.,0.,0.));
#75513=DIRECTION('',(0.,1.,0.));
#75514=DIRECTION('center_axis',(0.,1.,0.));
#75515=DIRECTION('ref_axis',(1.,0.,0.));
#75516=DIRECTION('',(0.,-1.,0.));
#75517=DIRECTION('center_axis',(0.,-1.,0.));
#75518=DIRECTION('ref_axis',(1.,0.,0.));
#75519=DIRECTION('',(0.,-1.,0.));
#75520=DIRECTION('center_axis',(0.,-1.,0.));
#75521=DIRECTION('ref_axis',(1.,0.,0.));
#75522=DIRECTION('center_axis',(0.,-1.,0.));
#75523=DIRECTION('ref_axis',(1.,0.,0.));
#75524=DIRECTION('center_axis',(0.,-1.,0.));
#75525=DIRECTION('ref_axis',(1.,0.,0.));
#75526=DIRECTION('',(0.,1.,0.));
#75527=DIRECTION('center_axis',(0.,1.,0.));
#75528=DIRECTION('ref_axis',(1.,0.,0.));
#75529=DIRECTION('',(0.,-1.,0.));
#75530=DIRECTION('center_axis',(0.,-1.,0.));
#75531=DIRECTION('ref_axis',(1.,0.,0.));
#75532=DIRECTION('',(0.,1.,0.));
#75533=DIRECTION('center_axis',(0.,1.,0.));
#75534=DIRECTION('ref_axis',(1.,0.,0.));
#75535=DIRECTION('',(0.,-1.,0.));
#75536=DIRECTION('center_axis',(0.,-1.,0.));
#75537=DIRECTION('ref_axis',(1.,0.,0.));
#75538=DIRECTION('',(0.,1.,0.));
#75539=DIRECTION('center_axis',(0.,1.,0.));
#75540=DIRECTION('ref_axis',(1.,0.,0.));
#75541=DIRECTION('',(0.,-1.,0.));
#75542=DIRECTION('center_axis',(0.,-1.,0.));
#75543=DIRECTION('ref_axis',(1.,0.,0.));
#75544=DIRECTION('',(0.,1.,0.));
#75545=DIRECTION('center_axis',(0.,1.,0.));
#75546=DIRECTION('ref_axis',(1.,0.,0.));
#75547=DIRECTION('',(0.,-1.,0.));
#75548=DIRECTION('center_axis',(0.,-1.,0.));
#75549=DIRECTION('ref_axis',(1.,0.,0.));
#75550=DIRECTION('',(0.,1.,0.));
#75551=DIRECTION('center_axis',(0.,1.,0.));
#75552=DIRECTION('ref_axis',(1.,0.,0.));
#75553=DIRECTION('',(0.,-1.,0.));
#75554=DIRECTION('center_axis',(0.,-1.,0.));
#75555=DIRECTION('ref_axis',(1.,0.,0.));
#75556=DIRECTION('',(0.,1.,0.));
#75557=DIRECTION('center_axis',(0.,1.,0.));
#75558=DIRECTION('ref_axis',(1.,0.,0.));
#75559=DIRECTION('',(0.,-1.,0.));
#75560=DIRECTION('center_axis',(0.,-1.,0.));
#75561=DIRECTION('ref_axis',(1.,0.,0.));
#75562=DIRECTION('',(0.,1.,0.));
#75563=DIRECTION('center_axis',(0.,1.,0.));
#75564=DIRECTION('ref_axis',(1.,0.,0.));
#75565=DIRECTION('',(0.,-1.,0.));
#75566=DIRECTION('center_axis',(0.,-1.,0.));
#75567=DIRECTION('ref_axis',(1.,0.,0.));
#75568=DIRECTION('',(0.,1.,0.));
#75569=DIRECTION('center_axis',(0.,1.,0.));
#75570=DIRECTION('ref_axis',(1.,0.,0.));
#75571=DIRECTION('',(0.,-1.,0.));
#75572=DIRECTION('center_axis',(0.,-1.,0.));
#75573=DIRECTION('ref_axis',(1.,0.,0.));
#75574=DIRECTION('',(0.,1.,0.));
#75575=DIRECTION('center_axis',(0.,1.,0.));
#75576=DIRECTION('ref_axis',(1.,0.,0.));
#75577=DIRECTION('',(0.,-1.,0.));
#75578=DIRECTION('center_axis',(0.,-1.,0.));
#75579=DIRECTION('ref_axis',(1.,0.,0.));
#75580=DIRECTION('',(0.,1.,0.));
#75581=DIRECTION('center_axis',(0.,1.,0.));
#75582=DIRECTION('ref_axis',(1.,0.,0.));
#75583=DIRECTION('',(0.,-1.,0.));
#75584=DIRECTION('center_axis',(0.,-1.,0.));
#75585=DIRECTION('ref_axis',(1.,0.,0.));
#75586=DIRECTION('',(0.,1.,0.));
#75587=DIRECTION('center_axis',(0.,1.,0.));
#75588=DIRECTION('ref_axis',(1.,0.,0.));
#75589=DIRECTION('',(0.,-1.,0.));
#75590=DIRECTION('center_axis',(0.,-1.,0.));
#75591=DIRECTION('ref_axis',(1.,0.,0.));
#75592=DIRECTION('',(0.,1.,0.));
#75593=DIRECTION('center_axis',(0.,1.,0.));
#75594=DIRECTION('ref_axis',(1.,0.,0.));
#75595=DIRECTION('',(0.,-1.,0.));
#75596=DIRECTION('center_axis',(0.,-1.,0.));
#75597=DIRECTION('ref_axis',(1.,0.,0.));
#75598=DIRECTION('',(0.,1.,0.));
#75599=DIRECTION('center_axis',(0.,1.,0.));
#75600=DIRECTION('ref_axis',(1.,0.,0.));
#75601=DIRECTION('',(0.,-1.,0.));
#75602=DIRECTION('center_axis',(0.,-1.,0.));
#75603=DIRECTION('ref_axis',(1.,0.,0.));
#75604=DIRECTION('',(0.,1.,0.));
#75605=DIRECTION('center_axis',(0.,1.,0.));
#75606=DIRECTION('ref_axis',(1.,0.,0.));
#75607=DIRECTION('',(0.,-1.,0.));
#75608=DIRECTION('center_axis',(0.,-1.,0.));
#75609=DIRECTION('ref_axis',(1.,0.,0.));
#75610=DIRECTION('',(0.,1.,0.));
#75611=DIRECTION('center_axis',(0.,1.,0.));
#75612=DIRECTION('ref_axis',(1.,0.,0.));
#75613=DIRECTION('',(0.,-1.,0.));
#75614=DIRECTION('center_axis',(0.,-1.,0.));
#75615=DIRECTION('ref_axis',(1.,0.,0.));
#75616=DIRECTION('',(0.,1.,0.));
#75617=DIRECTION('center_axis',(0.,1.,0.));
#75618=DIRECTION('ref_axis',(1.,0.,0.));
#75619=DIRECTION('',(0.,-1.,0.));
#75620=DIRECTION('center_axis',(0.,-1.,0.));
#75621=DIRECTION('ref_axis',(1.,0.,0.));
#75622=DIRECTION('',(0.,1.,0.));
#75623=DIRECTION('center_axis',(0.,1.,0.));
#75624=DIRECTION('ref_axis',(1.,0.,0.));
#75625=DIRECTION('center_axis',(-0.637062515999983,0.,-0.770812137104607));
#75626=DIRECTION('ref_axis',(0.770812137104607,0.,-0.637062515999983));
#75627=DIRECTION('',(0.,-1.,0.));
#75628=DIRECTION('',(0.770812137104607,0.,-0.637062515999983));
#75629=DIRECTION('center_axis',(0.,-1.,0.));
#75630=DIRECTION('ref_axis',(-0.342020143325669,0.,-0.939692620785908));
#75631=DIRECTION('',(-0.99997224619817,0.,0.0074502908256634));
#75632=DIRECTION('center_axis',(0.00745029082566334,0.,0.99997224619817));
#75633=DIRECTION('ref_axis',(-0.99997224619817,0.,0.00745029082566334));
#75634=DIRECTION('center_axis',(-0.761234227842014,0.,-0.64847702377322));
#75635=DIRECTION('ref_axis',(0.64847702377322,0.,-0.761234227842014));
#75636=DIRECTION('',(0.,-1.,0.));
#75637=DIRECTION('',(0.64847702377322,0.,-0.761234227842014));
#75638=DIRECTION('center_axis',(0.,-1.,0.));
#75639=DIRECTION('ref_axis',(-0.5,0.,-0.866025403784438));
#75640=DIRECTION('',(-0.983486691428025,0.,0.180980462437128));
#75641=DIRECTION('center_axis',(0.180980462437128,0.,0.983486691428025));
#75642=DIRECTION('ref_axis',(-0.983486691428025,0.,0.180980462437128));
#75643=DIRECTION('center_axis',(-0.862276222874171,0.,-0.506438264219691));
#75644=DIRECTION('ref_axis',(0.506438264219691,0.,-0.862276222874171));
#75645=DIRECTION('',(0.,-1.,0.));
#75646=DIRECTION('',(0.506438264219691,0.,-0.862276222874171));
#75647=DIRECTION('center_axis',(0.,-1.,0.));
#75648=DIRECTION('ref_axis',(-0.64278760968654,0.,-0.766044443118978));
#75649=DIRECTION('',(-0.937118391207119,0.,0.349011634277973));
#75650=DIRECTION('center_axis',(0.349011634277973,0.,0.937118391207119));
#75651=DIRECTION('ref_axis',(-0.937118391207118,0.,0.349011634277973));
#75652=DIRECTION('center_axis',(-0.937118391207119,0.,-0.349011634277973));
#75653=DIRECTION('ref_axis',(0.349011634277973,0.,-0.937118391207119));
#75654=DIRECTION('',(0.,-1.,0.));
#75655=DIRECTION('',(0.349011634277973,0.,-0.937118391207119));
#75656=DIRECTION('center_axis',(0.,-1.,0.));
#75657=DIRECTION('ref_axis',(-0.766044443118978,0.,-0.642787609686539));
#75658=DIRECTION('',(-0.862276222874171,0.,0.506438264219691));
#75659=DIRECTION('center_axis',(0.506438264219691,0.,0.862276222874171));
#75660=DIRECTION('ref_axis',(-0.862276222874171,0.,0.506438264219691));
#75661=DIRECTION('center_axis',(-0.983486691428025,0.,-0.180980462437128));
#75662=DIRECTION('ref_axis',(0.180980462437128,0.,-0.983486691428025));
#75663=DIRECTION('',(0.,-1.,0.));
#75664=DIRECTION('',(0.180980462437128,0.,-0.983486691428025));
#75665=DIRECTION('center_axis',(0.,-1.,0.));
#75666=DIRECTION('ref_axis',(-0.866025403784439,0.,-0.5));
#75667=DIRECTION('',(-0.761234227842013,0.,0.64847702377322));
#75668=DIRECTION('center_axis',(0.64847702377322,0.,0.761234227842013));
#75669=DIRECTION('ref_axis',(-0.761234227842013,0.,0.64847702377322));
#75670=DIRECTION('center_axis',(-0.99997224619817,0.,-0.00745029082566206));
#75671=DIRECTION('ref_axis',(0.00745029082566206,0.,-0.99997224619817));
#75672=DIRECTION('',(0.,-1.,0.));
#75673=DIRECTION('',(0.00745029082566206,0.,-0.99997224619817));
#75674=DIRECTION('center_axis',(0.,-1.,0.));
#75675=DIRECTION('ref_axis',(-0.939692620785909,0.,-0.342020143325668));
#75676=DIRECTION('',(-0.637062515999982,0.,0.770812137104608));
#75677=DIRECTION('center_axis',(0.770812137104608,0.,0.637062515999982));
#75678=DIRECTION('ref_axis',(-0.637062515999982,0.,0.770812137104608));
#75679=DIRECTION('center_axis',(-0.986074150277955,0.,0.166306254102511));
#75680=DIRECTION('ref_axis',(-0.166306254102511,0.,-0.986074150277955));
#75681=DIRECTION('',(0.,-1.,0.));
#75682=DIRECTION('',(-0.166306254102511,0.,-0.986074150277955));
#75683=DIRECTION('center_axis',(0.,-1.,0.));
#75684=DIRECTION('ref_axis',(-0.984807753012208,0.,-0.17364817766693));
#75685=DIRECTION('',(-0.493533981978478,0.,0.869726513699834));
#75686=DIRECTION('center_axis',(0.869726513699834,0.,0.493533981978479));
#75687=DIRECTION('ref_axis',(-0.493533981978479,0.,0.869726513699834));
#75688=DIRECTION('center_axis',(-0.942214690279141,0.,0.335009667654805));
#75689=DIRECTION('ref_axis',(-0.335009667654805,0.,-0.942214690279141));
#75690=DIRECTION('',(0.,-1.,0.));
#75691=DIRECTION('',(-0.335009667654805,0.,-0.942214690279141));
#75692=DIRECTION('center_axis',(0.,-1.,0.));
#75693=DIRECTION('ref_axis',(-1.,0.,1.83697019872103E-16));
#75694=DIRECTION('',(-0.335009667654805,0.,0.942214690279141));
#75695=DIRECTION('center_axis',(0.942214690279141,0.,0.335009667654805));
#75696=DIRECTION('ref_axis',(-0.335009667654805,0.,0.942214690279141));
#75697=DIRECTION('center_axis',(-0.869726513699833,0.,0.493533981978479));
#75698=DIRECTION('ref_axis',(-0.493533981978479,0.,-0.869726513699833));
#75699=DIRECTION('',(0.,-1.,0.));
#75700=DIRECTION('',(-0.493533981978479,0.,-0.869726513699833));
#75701=DIRECTION('center_axis',(0.,-1.,0.));
#75702=DIRECTION('ref_axis',(-0.984807753012208,0.,0.17364817766693));
#75703=DIRECTION('',(-0.166306254102511,0.,0.986074150277955));
#75704=DIRECTION('center_axis',(0.986074150277955,0.,0.166306254102511));
#75705=DIRECTION('ref_axis',(-0.166306254102511,0.,0.986074150277955));
#75706=DIRECTION('center_axis',(-0.770812137104607,0.,0.637062515999983));
#75707=DIRECTION('ref_axis',(-0.637062515999983,0.,-0.770812137104607));
#75708=DIRECTION('',(0.,-1.,0.));
#75709=DIRECTION('',(-0.637062515999983,0.,-0.770812137104607));
#75710=DIRECTION('center_axis',(0.,-1.,0.));
#75711=DIRECTION('ref_axis',(-0.939692620785908,0.,0.342020143325669));
#75712=DIRECTION('',(0.00745029082566329,0.,0.99997224619817));
#75713=DIRECTION('center_axis',(0.99997224619817,0.,-0.00745029082566323));
#75714=DIRECTION('ref_axis',(0.00745029082566323,0.,0.99997224619817));
#75715=DIRECTION('center_axis',(-0.64847702377322,0.,0.761234227842014));
#75716=DIRECTION('ref_axis',(-0.761234227842014,0.,-0.64847702377322));
#75717=DIRECTION('',(0.,-1.,0.));
#75718=DIRECTION('',(-0.761234227842014,0.,-0.64847702377322));
#75719=DIRECTION('center_axis',(0.,-1.,0.));
#75720=DIRECTION('ref_axis',(-0.866025403784438,0.,0.5));
#75721=DIRECTION('',(0.180980462437128,0.,0.983486691428025));
#75722=DIRECTION('center_axis',(0.983486691428025,0.,-0.180980462437128));
#75723=DIRECTION('ref_axis',(0.180980462437128,0.,0.983486691428025));
#75724=DIRECTION('center_axis',(-0.506438264219691,0.,0.862276222874171));
#75725=DIRECTION('ref_axis',(-0.862276222874171,0.,-0.506438264219691));
#75726=DIRECTION('',(0.,-1.,0.));
#75727=DIRECTION('',(-0.862276222874171,0.,-0.506438264219691));
#75728=DIRECTION('center_axis',(0.,-1.,0.));
#75729=DIRECTION('ref_axis',(-0.766044443118978,0.,0.642787609686539));
#75730=DIRECTION('',(0.349011634277973,0.,0.937118391207119));
#75731=DIRECTION('center_axis',(0.937118391207119,0.,-0.349011634277973));
#75732=DIRECTION('ref_axis',(0.349011634277973,0.,0.937118391207118));
#75733=DIRECTION('center_axis',(-0.349011634277973,0.,0.937118391207119));
#75734=DIRECTION('ref_axis',(-0.937118391207119,0.,-0.349011634277973));
#75735=DIRECTION('',(0.,-1.,0.));
#75736=DIRECTION('',(-0.937118391207119,0.,-0.349011634277973));
#75737=DIRECTION('center_axis',(0.,-1.,0.));
#75738=DIRECTION('ref_axis',(-0.642787609686539,0.,0.766044443118978));
#75739=DIRECTION('',(0.506438264219691,0.,0.862276222874171));
#75740=DIRECTION('center_axis',(0.862276222874171,0.,-0.506438264219691));
#75741=DIRECTION('ref_axis',(0.506438264219691,0.,0.862276222874171));
#75742=DIRECTION('center_axis',(-0.180980462437127,0.,0.983486691428025));
#75743=DIRECTION('ref_axis',(-0.983486691428025,0.,-0.180980462437127));
#75744=DIRECTION('',(0.,-1.,0.));
#75745=DIRECTION('',(-0.983486691428025,0.,-0.180980462437127));
#75746=DIRECTION('center_axis',(0.,-1.,0.));
#75747=DIRECTION('ref_axis',(-0.5,0.,0.866025403784439));
#75748=DIRECTION('',(0.648477023773221,0.,0.761234227842013));
#75749=DIRECTION('center_axis',(0.761234227842013,0.,-0.648477023773221));
#75750=DIRECTION('ref_axis',(0.648477023773221,0.,0.761234227842013));
#75751=DIRECTION('center_axis',(-0.00745029082566251,0.,0.99997224619817));
#75752=DIRECTION('ref_axis',(-0.99997224619817,0.,-0.00745029082566251));
#75753=DIRECTION('',(0.,-1.,0.));
#75754=DIRECTION('',(-0.99997224619817,0.,-0.00745029082566251));
#75755=DIRECTION('center_axis',(0.,-1.,0.));
#75756=DIRECTION('ref_axis',(-0.342020143325669,0.,0.939692620785909));
#75757=DIRECTION('',(0.770812137104608,0.,0.637062515999982));
#75758=DIRECTION('center_axis',(0.637062515999982,0.,-0.770812137104608));
#75759=DIRECTION('ref_axis',(0.770812137104608,0.,0.637062515999982));
#75760=DIRECTION('center_axis',(0.166306254102511,0.,0.986074150277955));
#75761=DIRECTION('ref_axis',(-0.986074150277955,0.,0.166306254102511));
#75762=DIRECTION('',(0.,-1.,0.));
#75763=DIRECTION('',(-0.986074150277955,0.,0.166306254102511));
#75764=DIRECTION('center_axis',(0.,-1.,0.));
#75765=DIRECTION('ref_axis',(-0.17364817766693,0.,0.984807753012208));
#75766=DIRECTION('',(0.869726513699833,0.,0.493533981978479));
#75767=DIRECTION('center_axis',(0.493533981978479,0.,-0.869726513699834));
#75768=DIRECTION('ref_axis',(0.869726513699834,0.,0.493533981978479));
#75769=DIRECTION('center_axis',(0.335009667654805,0.,0.942214690279141));
#75770=DIRECTION('ref_axis',(-0.942214690279141,0.,0.335009667654805));
#75771=DIRECTION('',(0.,-1.,0.));
#75772=DIRECTION('',(-0.942214690279141,0.,0.335009667654805));
#75773=DIRECTION('center_axis',(0.,-1.,0.));
#75774=DIRECTION('ref_axis',(1.22464679914735E-16,0.,1.));
#75775=DIRECTION('',(0.942214690279141,0.,0.335009667654805));
#75776=DIRECTION('center_axis',(0.335009667654805,0.,-0.942214690279141));
#75777=DIRECTION('ref_axis',(0.942214690279141,0.,0.335009667654805));
#75778=DIRECTION('center_axis',(0.493533981978479,0.,0.869726513699833));
#75779=DIRECTION('ref_axis',(-0.869726513699833,0.,0.493533981978479));
#75780=DIRECTION('',(0.,-1.,0.));
#75781=DIRECTION('',(-0.869726513699833,0.,0.493533981978479));
#75782=DIRECTION('center_axis',(0.,-1.,0.));
#75783=DIRECTION('ref_axis',(0.173648177666931,0.,0.984807753012208));
#75784=DIRECTION('',(0.986074150277955,0.,0.166306254102511));
#75785=DIRECTION('center_axis',(0.166306254102511,0.,-0.986074150277955));
#75786=DIRECTION('ref_axis',(0.986074150277955,0.,0.166306254102511));
#75787=DIRECTION('center_axis',(0.637062515999982,0.,0.770812137104607));
#75788=DIRECTION('ref_axis',(-0.770812137104608,0.,0.637062515999982));
#75789=DIRECTION('',(0.,-1.,0.));
#75790=DIRECTION('',(-0.770812137104608,0.,0.637062515999982));
#75791=DIRECTION('center_axis',(0.,-1.,0.));
#75792=DIRECTION('ref_axis',(0.342020143325669,0.,0.939692620785908));
#75793=DIRECTION('',(0.99997224619817,0.,-0.00745029082566279));
#75794=DIRECTION('center_axis',(-0.00745029082566278,0.,-0.99997224619817));
#75795=DIRECTION('ref_axis',(0.99997224619817,0.,-0.00745029082566278));
#75796=DIRECTION('center_axis',(0.761234227842013,0.,0.64847702377322));
#75797=DIRECTION('ref_axis',(-0.64847702377322,0.,0.761234227842013));
#75798=DIRECTION('',(0.,-1.,0.));
#75799=DIRECTION('',(-0.64847702377322,0.,0.761234227842013));
#75800=DIRECTION('center_axis',(0.,-1.,0.));
#75801=DIRECTION('ref_axis',(0.5,0.,0.866025403784439));
#75802=DIRECTION('',(0.983486691428025,0.,-0.180980462437127));
#75803=DIRECTION('center_axis',(-0.180980462437127,0.,-0.983486691428025));
#75804=DIRECTION('ref_axis',(0.983486691428025,0.,-0.180980462437127));
#75805=DIRECTION('center_axis',(0.862276222874171,0.,0.506438264219691));
#75806=DIRECTION('ref_axis',(-0.506438264219691,0.,0.862276222874171));
#75807=DIRECTION('',(0.,-1.,0.));
#75808=DIRECTION('',(-0.506438264219691,0.,0.862276222874171));
#75809=DIRECTION('center_axis',(0.,-1.,0.));
#75810=DIRECTION('ref_axis',(0.642787609686539,0.,0.766044443118978));
#75811=DIRECTION('',(0.937118391207119,0.,-0.349011634277973));
#75812=DIRECTION('center_axis',(-0.349011634277973,0.,-0.937118391207119));
#75813=DIRECTION('ref_axis',(0.937118391207118,0.,-0.349011634277973));
#75814=DIRECTION('center_axis',(0.937118391207119,0.,0.349011634277973));
#75815=DIRECTION('ref_axis',(-0.349011634277973,0.,0.937118391207119));
#75816=DIRECTION('',(0.,-1.,0.));
#75817=DIRECTION('',(-0.349011634277973,0.,0.937118391207119));
#75818=DIRECTION('center_axis',(0.,-1.,0.));
#75819=DIRECTION('ref_axis',(0.766044443118978,0.,0.642787609686539));
#75820=DIRECTION('',(0.862276222874171,0.,-0.506438264219691));
#75821=DIRECTION('center_axis',(-0.506438264219691,0.,-0.862276222874171));
#75822=DIRECTION('ref_axis',(0.862276222874171,0.,-0.506438264219691));
#75823=DIRECTION('center_axis',(0.983486691428025,0.,0.180980462437127));
#75824=DIRECTION('ref_axis',(-0.180980462437127,0.,0.983486691428025));
#75825=DIRECTION('',(0.,-1.,0.));
#75826=DIRECTION('',(-0.180980462437127,0.,0.983486691428025));
#75827=DIRECTION('center_axis',(0.,-1.,0.));
#75828=DIRECTION('ref_axis',(0.866025403784439,0.,0.5));
#75829=DIRECTION('',(0.761234227842013,0.,-0.64847702377322));
#75830=DIRECTION('center_axis',(-0.648477023773221,0.,-0.761234227842013));
#75831=DIRECTION('ref_axis',(0.761234227842013,0.,-0.648477023773221));
#75832=DIRECTION('center_axis',(0.99997224619817,0.,0.00745029082566256));
#75833=DIRECTION('ref_axis',(-0.00745029082566256,0.,0.99997224619817));
#75834=DIRECTION('',(0.,-1.,0.));
#75835=DIRECTION('',(-0.00745029082566256,0.,0.99997224619817));
#75836=DIRECTION('center_axis',(0.,-1.,0.));
#75837=DIRECTION('ref_axis',(0.939692620785908,0.,0.342020143325669));
#75838=DIRECTION('',(0.637062515999982,0.,-0.770812137104608));
#75839=DIRECTION('center_axis',(-0.770812137104608,0.,-0.637062515999982));
#75840=DIRECTION('ref_axis',(0.637062515999982,0.,-0.770812137104608));
#75841=DIRECTION('center_axis',(0.986074150277955,0.,-0.166306254102511));
#75842=DIRECTION('ref_axis',(0.166306254102511,0.,0.986074150277955));
#75843=DIRECTION('',(0.,-1.,0.));
#75844=DIRECTION('',(0.166306254102511,0.,0.986074150277955));
#75845=DIRECTION('center_axis',(0.,-1.,0.));
#75846=DIRECTION('ref_axis',(0.984807753012208,0.,0.17364817766693));
#75847=DIRECTION('',(0.493533981978479,0.,-0.869726513699833));
#75848=DIRECTION('center_axis',(-0.869726513699833,0.,-0.493533981978479));
#75849=DIRECTION('ref_axis',(0.493533981978479,0.,-0.869726513699833));
#75850=DIRECTION('center_axis',(0.942214690279141,0.,-0.335009667654805));
#75851=DIRECTION('ref_axis',(0.335009667654805,0.,0.942214690279141));
#75852=DIRECTION('',(0.,-1.,0.));
#75853=DIRECTION('',(0.335009667654805,0.,0.942214690279141));
#75854=DIRECTION('center_axis',(0.,-1.,0.));
#75855=DIRECTION('ref_axis',(1.,0.,-6.12323399573677E-17));
#75856=DIRECTION('',(0.335009667654805,0.,-0.942214690279141));
#75857=DIRECTION('center_axis',(-0.942214690279141,0.,-0.335009667654805));
#75858=DIRECTION('ref_axis',(0.335009667654805,0.,-0.942214690279141));
#75859=DIRECTION('center_axis',(0.869726513699833,0.,-0.493533981978479));
#75860=DIRECTION('ref_axis',(0.493533981978479,0.,0.869726513699833));
#75861=DIRECTION('',(0.,-1.,0.));
#75862=DIRECTION('',(0.493533981978479,0.,0.869726513699833));
#75863=DIRECTION('center_axis',(0.,-1.,0.));
#75864=DIRECTION('ref_axis',(0.984807753012208,0.,-0.17364817766693));
#75865=DIRECTION('',(0.166306254102511,0.,-0.986074150277955));
#75866=DIRECTION('center_axis',(-0.986074150277955,0.,-0.166306254102511));
#75867=DIRECTION('ref_axis',(0.166306254102511,0.,-0.986074150277955));
#75868=DIRECTION('center_axis',(0.770812137104608,0.,-0.637062515999982));
#75869=DIRECTION('ref_axis',(0.637062515999982,0.,0.770812137104608));
#75870=DIRECTION('',(0.,-1.,0.));
#75871=DIRECTION('',(0.637062515999982,0.,0.770812137104608));
#75872=DIRECTION('center_axis',(0.,-1.,0.));
#75873=DIRECTION('ref_axis',(0.939692620785908,0.,-0.342020143325669));
#75874=DIRECTION('',(-0.00745029082566273,0.,-0.99997224619817));
#75875=DIRECTION('center_axis',(-0.99997224619817,0.,0.00745029082566273));
#75876=DIRECTION('ref_axis',(-0.00745029082566273,0.,-0.99997224619817));
#75877=DIRECTION('center_axis',(0.64847702377322,0.,-0.761234227842013));
#75878=DIRECTION('ref_axis',(0.761234227842013,0.,0.64847702377322));
#75879=DIRECTION('',(0.,-1.,0.));
#75880=DIRECTION('',(0.761234227842013,0.,0.64847702377322));
#75881=DIRECTION('center_axis',(0.,-1.,0.));
#75882=DIRECTION('ref_axis',(0.866025403784439,0.,-0.5));
#75883=DIRECTION('',(-0.180980462437128,0.,-0.983486691428025));
#75884=DIRECTION('center_axis',(-0.983486691428025,0.,0.180980462437128));
#75885=DIRECTION('ref_axis',(-0.180980462437128,0.,-0.983486691428025));
#75886=DIRECTION('center_axis',(0.506438264219691,0.,-0.862276222874171));
#75887=DIRECTION('ref_axis',(0.862276222874171,0.,0.506438264219691));
#75888=DIRECTION('',(0.,-1.,0.));
#75889=DIRECTION('',(0.862276222874171,0.,0.506438264219691));
#75890=DIRECTION('center_axis',(0.,-1.,0.));
#75891=DIRECTION('ref_axis',(0.766044443118978,0.,-0.642787609686539));
#75892=DIRECTION('',(-0.349011634277973,0.,-0.937118391207119));
#75893=DIRECTION('center_axis',(-0.937118391207119,0.,0.349011634277973));
#75894=DIRECTION('ref_axis',(-0.349011634277973,0.,-0.937118391207119));
#75895=DIRECTION('center_axis',(0.349011634277973,0.,-0.937118391207119));
#75896=DIRECTION('ref_axis',(0.937118391207119,0.,0.349011634277973));
#75897=DIRECTION('',(0.,-1.,0.));
#75898=DIRECTION('',(0.937118391207119,0.,0.349011634277973));
#75899=DIRECTION('center_axis',(0.,-1.,0.));
#75900=DIRECTION('ref_axis',(0.642787609686539,0.,-0.766044443118978));
#75901=DIRECTION('',(-0.506438264219691,0.,-0.862276222874171));
#75902=DIRECTION('center_axis',(-0.862276222874171,0.,0.506438264219691));
#75903=DIRECTION('ref_axis',(-0.506438264219691,0.,-0.862276222874171));
#75904=DIRECTION('center_axis',(0.180980462437127,0.,-0.983486691428025));
#75905=DIRECTION('ref_axis',(0.983486691428025,0.,0.180980462437127));
#75906=DIRECTION('',(0.,-1.,0.));
#75907=DIRECTION('',(0.983486691428025,0.,0.180980462437127));
#75908=DIRECTION('center_axis',(0.,-1.,0.));
#75909=DIRECTION('ref_axis',(0.5,0.,-0.866025403784439));
#75910=DIRECTION('',(-0.64847702377322,0.,-0.761234227842013));
#75911=DIRECTION('center_axis',(-0.761234227842013,0.,0.64847702377322));
#75912=DIRECTION('ref_axis',(-0.64847702377322,0.,-0.761234227842013));
#75913=DIRECTION('center_axis',(0.00745029082566256,0.,-0.99997224619817));
#75914=DIRECTION('ref_axis',(0.99997224619817,0.,0.00745029082566256));
#75915=DIRECTION('',(0.,-1.,0.));
#75916=DIRECTION('',(0.99997224619817,0.,0.00745029082566256));
#75917=DIRECTION('center_axis',(0.,-1.,0.));
#75918=DIRECTION('ref_axis',(0.342020143325669,0.,-0.939692620785908));
#75919=DIRECTION('',(-0.770812137104608,0.,-0.637062515999982));
#75920=DIRECTION('center_axis',(-0.637062515999982,0.,0.770812137104608));
#75921=DIRECTION('ref_axis',(-0.770812137104608,0.,-0.637062515999982));
#75922=DIRECTION('center_axis',(-0.166306254102511,0.,-0.986074150277955));
#75923=DIRECTION('ref_axis',(0.986074150277955,0.,-0.166306254102511));
#75924=DIRECTION('',(0.,-1.,0.));
#75925=DIRECTION('',(0.986074150277955,0.,-0.166306254102511));
#75926=DIRECTION('center_axis',(0.,-1.,0.));
#75927=DIRECTION('ref_axis',(0.17364817766693,0.,-0.984807753012208));
#75928=DIRECTION('',(-0.869726513699833,0.,-0.493533981978479));
#75929=DIRECTION('center_axis',(-0.493533981978479,0.,0.869726513699833));
#75930=DIRECTION('ref_axis',(-0.869726513699833,0.,-0.493533981978479));
#75931=DIRECTION('center_axis',(-0.335009667654805,0.,-0.942214690279141));
#75932=DIRECTION('ref_axis',(0.942214690279141,0.,-0.335009667654805));
#75933=DIRECTION('',(0.,-1.,0.));
#75934=DIRECTION('',(0.942214690279141,0.,-0.335009667654805));
#75935=DIRECTION('center_axis',(0.,-1.,0.));
#75936=DIRECTION('ref_axis',(0.,0.,-1.));
#75937=DIRECTION('',(-0.942214690279141,0.,-0.335009667654805));
#75938=DIRECTION('center_axis',(-0.335009667654805,0.,0.942214690279141));
#75939=DIRECTION('ref_axis',(-0.942214690279141,0.,-0.335009667654805));
#75940=DIRECTION('center_axis',(0.,1.,0.));
#75941=DIRECTION('ref_axis',(0.,0.,1.));
#75942=DIRECTION('center_axis',(-1.,0.,0.));
#75943=DIRECTION('ref_axis',(0.,0.,-1.));
#75944=DIRECTION('center_axis',(0.,-1.,0.));
#75945=DIRECTION('ref_axis',(1.,0.,0.));
#75946=DIRECTION('center_axis',(0.,-1.,0.));
#75947=DIRECTION('ref_axis',(1.,0.,0.));
#75948=DIRECTION('',(-0.707106781186547,-0.707106781186547,8.65956056235493E-17));
#75949=DIRECTION('center_axis',(0.,1.,0.));
#75950=DIRECTION('ref_axis',(1.,0.,0.));
#75951=DIRECTION('center_axis',(0.,-1.,0.));
#75952=DIRECTION('ref_axis',(1.,0.,0.));
#75953=DIRECTION('center_axis',(0.,1.,0.));
#75954=DIRECTION('ref_axis',(1.,0.,0.));
#75955=DIRECTION('',(0.707106781186551,-0.707106781186544,8.65956056235498E-17));
#75956=DIRECTION('center_axis',(0.,-1.,0.));
#75957=DIRECTION('ref_axis',(1.,0.,0.));
#75958=DIRECTION('center_axis',(0.,-1.,0.));
#75959=DIRECTION('ref_axis',(1.,0.,0.));
#75960=DIRECTION('center_axis',(0.,-1.,0.));
#75961=DIRECTION('ref_axis',(1.,0.,0.));
#75962=DIRECTION('center_axis',(0.,-1.,0.));
#75963=DIRECTION('ref_axis',(1.,0.,0.));
#75964=DIRECTION('center_axis',(0.,-1.,0.));
#75965=DIRECTION('ref_axis',(1.,0.,0.));
#75966=DIRECTION('center_axis',(0.,-1.,0.));
#75967=DIRECTION('ref_axis',(1.,0.,0.));
#75968=DIRECTION('center_axis',(0.,-1.,0.));
#75969=DIRECTION('ref_axis',(1.,0.,0.));
#75970=DIRECTION('',(0.,1.,0.));
#75971=DIRECTION('',(0.,-1.,0.));
#75972=DIRECTION('center_axis',(0.,1.,0.));
#75973=DIRECTION('ref_axis',(1.,0.,0.));
#75974=DIRECTION('center_axis',(0.,-1.,0.));
#75975=DIRECTION('ref_axis',(1.,0.,0.));
#75976=DIRECTION('',(0.,1.,0.));
#75977=DIRECTION('',(0.,-1.,0.));
#75978=DIRECTION('center_axis',(0.,1.,0.));
#75979=DIRECTION('ref_axis',(1.,0.,0.));
#75980=DIRECTION('center_axis',(0.,-1.,0.));
#75981=DIRECTION('ref_axis',(1.,0.,0.));
#75982=DIRECTION('',(0.,-1.,0.));
#75983=DIRECTION('center_axis',(0.,1.,0.));
#75984=DIRECTION('ref_axis',(1.,0.,0.));
#75985=DIRECTION('',(0.,1.,0.));
#75986=DIRECTION('center_axis',(0.,-1.,0.));
#75987=DIRECTION('ref_axis',(1.,0.,0.));
#75988=DIRECTION('',(0.,1.,0.));
#75989=DIRECTION('',(0.,-1.,0.));
#75990=DIRECTION('center_axis',(0.,1.,0.));
#75991=DIRECTION('ref_axis',(1.,0.,0.));
#75992=DIRECTION('center_axis',(0.,-1.,0.));
#75993=DIRECTION('ref_axis',(1.,0.,0.));
#75994=DIRECTION('',(0.,-1.,0.));
#75995=DIRECTION('center_axis',(0.,1.,0.));
#75996=DIRECTION('ref_axis',(1.,0.,0.));
#75997=DIRECTION('',(0.,1.,0.));
#75998=DIRECTION('center_axis',(0.,-1.,0.));
#75999=DIRECTION('ref_axis',(1.,0.,0.));
#76000=DIRECTION('',(0.,-1.,0.));
#76001=DIRECTION('center_axis',(0.,1.,0.));
#76002=DIRECTION('ref_axis',(1.,0.,0.));
#76003=DIRECTION('',(0.,1.,0.));
#76004=DIRECTION('center_axis',(0.866025403784439,0.,0.5));
#76005=DIRECTION('ref_axis',(-0.5,0.,0.866025403784439));
#76006=DIRECTION('',(-0.5,0.,0.866025403784439));
#76007=DIRECTION('',(0.,-1.,0.));
#76008=DIRECTION('',(-0.5,0.,0.866025403784439));
#76009=DIRECTION('',(0.,-1.,0.));
#76010=DIRECTION('center_axis',(0.866025403784439,0.,-0.5));
#76011=DIRECTION('ref_axis',(0.5,0.,0.866025403784439));
#76012=DIRECTION('',(0.5,0.,0.866025403784439));
#76013=DIRECTION('',(0.,-1.,0.));
#76014=DIRECTION('',(0.5,0.,0.866025403784439));
#76015=DIRECTION('center_axis',(0.,0.,-1.));
#76016=DIRECTION('ref_axis',(1.,0.,0.));
#76017=DIRECTION('',(1.,0.,0.));
#76018=DIRECTION('',(0.,-1.,0.));
#76019=DIRECTION('',(1.,0.,0.));
#76020=DIRECTION('center_axis',(0.,1.,0.));
#76021=DIRECTION('ref_axis',(1.,0.,0.));
#76022=DIRECTION('center_axis',(0.,1.,0.));
#76023=DIRECTION('ref_axis',(1.,0.,0.));
#76024=DIRECTION('center_axis',(0.,1.,0.));
#76025=DIRECTION('ref_axis',(1.,0.,0.));
#76026=DIRECTION('',(0.499999999999999,0.,-0.866025403784439));
#76027=DIRECTION('center_axis',(0.,1.,0.));
#76028=DIRECTION('ref_axis',(1.,0.,0.));
#76029=DIRECTION('center_axis',(0.,1.,0.));
#76030=DIRECTION('ref_axis',(1.,0.,0.));
#76031=DIRECTION('',(-0.5,0.,-0.866025403784439));
#76032=DIRECTION('center_axis',(0.,1.,0.));
#76033=DIRECTION('ref_axis',(1.,0.,0.));
#76034=DIRECTION('',(-1.,0.,0.));
#76035=DIRECTION('center_axis',(0.,1.,0.));
#76036=DIRECTION('ref_axis',(0.,0.,1.));
#76037=DIRECTION('',(0.499999999999999,0.,-0.866025403784439));
#76038=DIRECTION('center_axis',(0.,-1.,0.));
#76039=DIRECTION('ref_axis',(1.,0.,0.));
#76040=DIRECTION('center_axis',(0.,1.,0.));
#76041=DIRECTION('ref_axis',(0.,0.,1.));
#76042=DIRECTION('center_axis',(0.,-1.,0.));
#76043=DIRECTION('ref_axis',(1.,0.,0.));
#76044=DIRECTION('center_axis',(0.,1.,0.));
#76045=DIRECTION('ref_axis',(0.,0.,1.));
#76046=DIRECTION('center_axis',(0.,-1.,0.));
#76047=DIRECTION('ref_axis',(1.,0.,0.));
#76048=DIRECTION('center_axis',(0.,1.,0.));
#76049=DIRECTION('ref_axis',(0.,0.,1.));
#76050=DIRECTION('center_axis',(0.,-1.,0.));
#76051=DIRECTION('ref_axis',(1.,0.,0.));
#76052=DIRECTION('center_axis',(0.,1.,0.));
#76053=DIRECTION('ref_axis',(0.,0.,1.));
#76054=DIRECTION('',(-1.,0.,0.));
#76055=DIRECTION('center_axis',(0.,-1.,0.));
#76056=DIRECTION('ref_axis',(1.,0.,0.));
#76057=DIRECTION('center_axis',(0.,1.,0.));
#76058=DIRECTION('ref_axis',(0.,0.,1.));
#76059=DIRECTION('',(-0.5,0.,-0.866025403784439));
#76060=DIRECTION('center_axis',(0.,-1.,0.));
#76061=DIRECTION('ref_axis',(1.,0.,0.));
#76062=DIRECTION('center_axis',(0.,1.,0.));
#76063=DIRECTION('ref_axis',(1.,0.,0.));
#76064=DIRECTION('',(0.857167300702113,-0.515038074910054,1.04972719113862E-16));
#76065=DIRECTION('center_axis',(-0.866025403784439,0.,-0.499999999999999));
#76066=DIRECTION('ref_axis',(0.499999999999999,0.,-0.866025403784439));
#76067=DIRECTION('',(0.,-1.,0.));
#76068=DIRECTION('center_axis',(-0.866025403784439,0.,0.5));
#76069=DIRECTION('ref_axis',(-0.5,0.,-0.866025403784439));
#76070=DIRECTION('',(0.,-1.,0.));
#76071=DIRECTION('center_axis',(0.,0.,1.));
#76072=DIRECTION('ref_axis',(-1.,0.,0.));
#76073=DIRECTION('axis',(0.,0.,1.));
#76074=DIRECTION('refdir',(1.,0.,0.));
#76075=DIRECTION('center_axis',(0.,1.,0.));
#76076=DIRECTION('ref_axis',(0.,0.,1.));
#76077=DIRECTION('center_axis',(0.,-1.,0.));
#76078=DIRECTION('ref_axis',(1.,0.,0.));
#76079=DIRECTION('center_axis',(0.,-1.,0.));
#76080=DIRECTION('ref_axis',(1.,0.,0.));
#76081=DIRECTION('center_axis',(0.,-1.,0.));
#76082=DIRECTION('ref_axis',(1.,0.,0.));
#76083=DIRECTION('',(0.707106781186547,0.707106781186548,8.65956056235493E-17));
#76084=DIRECTION('center_axis',(0.,-1.,0.));
#76085=DIRECTION('ref_axis',(1.,0.,0.));
#76086=DIRECTION('center_axis',(0.,-1.,0.));
#76087=DIRECTION('ref_axis',(1.,0.,0.));
#76088=DIRECTION('',(0.,1.,0.));
#76089=DIRECTION('center_axis',(0.,1.,0.));
#76090=DIRECTION('ref_axis',(1.,0.,0.));
#76091=DIRECTION('center_axis',(0.,-1.,0.));
#76092=DIRECTION('ref_axis',(1.,0.,0.));
#76093=DIRECTION('',(-0.707106781186548,0.707106781186547,-8.65956056235493E-17));
#76094=DIRECTION('center_axis',(0.,-1.,0.));
#76095=DIRECTION('ref_axis',(0.,0.,-1.));
#76096=DIRECTION('',(0.,0.,1.));
#76097=DIRECTION('',(1.,0.,0.));
#76098=DIRECTION('',(0.,0.,1.));
#76099=DIRECTION('',(1.,0.,0.));
#76100=DIRECTION('',(0.,0.,1.));
#76101=DIRECTION('',(1.,0.,0.));
#76102=DIRECTION('',(0.,0.,1.));
#76103=DIRECTION('',(1.,0.,0.));
#76104=DIRECTION('',(0.,0.,1.));
#76105=DIRECTION('',(1.,0.,0.));
#76106=DIRECTION('',(0.,0.,1.));
#76107=DIRECTION('',(1.,0.,0.));
#76108=DIRECTION('',(0.,0.,1.));
#76109=DIRECTION('',(1.,0.,0.));
#76110=DIRECTION('',(0.,0.,1.));
#76111=DIRECTION('',(1.,0.,0.));
#76112=DIRECTION('',(0.,0.,1.));
#76113=DIRECTION('',(1.,0.,0.));
#76114=DIRECTION('',(0.,0.,1.));
#76115=DIRECTION('',(1.,0.,0.));
#76116=DIRECTION('',(0.,0.,1.));
#76117=DIRECTION('',(1.,0.,0.));
#76118=DIRECTION('',(0.,0.,1.));
#76119=DIRECTION('',(1.,0.,0.));
#76120=DIRECTION('',(0.,0.,1.));
#76121=DIRECTION('',(1.,0.,0.));
#76122=DIRECTION('',(0.,0.,1.));
#76123=DIRECTION('',(1.,0.,0.));
#76124=DIRECTION('',(0.,0.,1.));
#76125=DIRECTION('',(1.,0.,0.));
#76126=DIRECTION('',(0.,0.,1.));
#76127=DIRECTION('',(1.,0.,0.));
#76128=DIRECTION('',(0.,0.,1.));
#76129=DIRECTION('',(1.,0.,0.));
#76130=DIRECTION('',(0.,0.,1.));
#76131=DIRECTION('',(1.,0.,0.));
#76132=DIRECTION('',(0.,0.,1.));
#76133=DIRECTION('',(1.,0.,0.));
#76134=DIRECTION('',(0.,0.,1.));
#76135=DIRECTION('',(1.,0.,0.));
#76136=DIRECTION('',(0.,0.,1.));
#76137=DIRECTION('',(1.,0.,0.));
#76138=DIRECTION('',(0.,0.,1.));
#76139=DIRECTION('',(1.,0.,0.));
#76140=DIRECTION('',(0.,0.,1.));
#76141=DIRECTION('',(1.,0.,0.));
#76142=DIRECTION('',(0.,0.,1.));
#76143=DIRECTION('',(1.,0.,0.));
#76144=CARTESIAN_POINT('',(0.,0.,0.));
#76145=CARTESIAN_POINT('',(0.,0.,0.));
#76146=CARTESIAN_POINT('Ctrl Pts',(200.85163737461,3.38540250062943,48.5));
#76147=CARTESIAN_POINT('Ctrl Pts',(200.85163737461,3.38540250062943,48.35));
#76148=CARTESIAN_POINT('Ctrl Pts',(200.665552567691,3.38540250062943,48.5));
#76149=CARTESIAN_POINT('Ctrl Pts',(200.665552567691,3.38540250062943,48.35));
#76150=CARTESIAN_POINT('Ctrl Pts',(200.55450225994,3.22783091664314,48.5));
#76151=CARTESIAN_POINT('Ctrl Pts',(200.55450225994,3.22783091664314,48.35));
#76152=CARTESIAN_POINT('',(200.85163737461,3.38540250062943,48.5));
#76153=CARTESIAN_POINT('',(200.55450225994,3.22783091664314,48.5));
#76154=CARTESIAN_POINT('Ctrl Pts',(200.85163737461,3.38540250062943,48.5));
#76155=CARTESIAN_POINT('Ctrl Pts',(200.665552567691,3.38540250062943,48.5));
#76156=CARTESIAN_POINT('Ctrl Pts',(200.55450225994,3.22783091664314,48.5));
#76157=CARTESIAN_POINT('',(200.85163737461,3.38540250062943,48.35));
#76158=CARTESIAN_POINT('',(200.85163737461,3.38540250062943,48.5));
#76159=CARTESIAN_POINT('',(200.55450225994,3.22783091664314,48.35));
#76160=CARTESIAN_POINT('Ctrl Pts',(200.85163737461,3.38540250062943,48.35));
#76161=CARTESIAN_POINT('Ctrl Pts',(200.665552567691,3.38540250062943,48.35));
#76162=CARTESIAN_POINT('Ctrl Pts',(200.55450225994,3.22783091664314,48.35));
#76163=CARTESIAN_POINT('',(200.55450225994,3.22783091664314,48.5));
#76164=CARTESIAN_POINT('Ctrl Pts',(201.167530667037,3.2068213224411,48.5));
#76165=CARTESIAN_POINT('Ctrl Pts',(201.167530667037,3.2068213224411,48.35));
#76166=CARTESIAN_POINT('Ctrl Pts',(201.04072297737,3.38540250062943,48.5));
#76167=CARTESIAN_POINT('Ctrl Pts',(201.04072297737,3.38540250062943,48.35));
#76168=CARTESIAN_POINT('Ctrl Pts',(200.85163737461,3.38540250062943,48.5));
#76169=CARTESIAN_POINT('Ctrl Pts',(200.85163737461,3.38540250062943,48.35));
#76170=CARTESIAN_POINT('',(201.167530667037,3.2068213224411,48.5));
#76171=CARTESIAN_POINT('Ctrl Pts',(201.167530667037,3.2068213224411,48.5));
#76172=CARTESIAN_POINT('Ctrl Pts',(201.04072297737,3.38540250062943,48.5));
#76173=CARTESIAN_POINT('Ctrl Pts',(200.85163737461,3.38540250062943,48.5));
#76174=CARTESIAN_POINT('',(201.167530667037,3.2068213224411,48.35));
#76175=CARTESIAN_POINT('',(201.167530667037,3.2068213224411,48.5));
#76176=CARTESIAN_POINT('Ctrl Pts',(201.167530667037,3.2068213224411,48.35));
#76177=CARTESIAN_POINT('Ctrl Pts',(201.04072297737,3.38540250062943,48.35));
#76178=CARTESIAN_POINT('Ctrl Pts',(200.85163737461,3.38540250062943,48.35));
#76179=CARTESIAN_POINT('Ctrl Pts',(201.294338356704,2.48499327898026,48.5));
#76180=CARTESIAN_POINT('Ctrl Pts',(201.294338356704,2.48499327898026,48.35));
#76181=CARTESIAN_POINT('Ctrl Pts',(201.294338356704,3.02824014425278,48.5));
#76182=CARTESIAN_POINT('Ctrl Pts',(201.294338356704,3.02824014425278,48.35));
#76183=CARTESIAN_POINT('Ctrl Pts',(201.167530667037,3.2068213224411,48.5));
#76184=CARTESIAN_POINT('Ctrl Pts',(201.167530667037,3.2068213224411,48.35));
#76185=CARTESIAN_POINT('',(201.294338356704,2.48499327898026,48.5));
#76186=CARTESIAN_POINT('Ctrl Pts',(201.294338356704,2.48499327898026,48.5));
#76187=CARTESIAN_POINT('Ctrl Pts',(201.294338356704,3.02824014425278,48.5));
#76188=CARTESIAN_POINT('Ctrl Pts',(201.167530667037,3.2068213224411,48.5));
#76189=CARTESIAN_POINT('',(201.294338356704,2.48499327898026,48.35));
#76190=CARTESIAN_POINT('',(201.294338356704,2.48499327898026,48.5));
#76191=CARTESIAN_POINT('Ctrl Pts',(201.294338356704,2.48499327898026,48.35));
#76192=CARTESIAN_POINT('Ctrl Pts',(201.294338356704,3.02824014425278,48.35));
#76193=CARTESIAN_POINT('Ctrl Pts',(201.167530667037,3.2068213224411,48.35));
#76194=CARTESIAN_POINT('Ctrl Pts',(201.167530667037,1.76466578245163,48.5));
#76195=CARTESIAN_POINT('Ctrl Pts',(201.167530667037,1.76466578245163,48.35));
#76196=CARTESIAN_POINT('Ctrl Pts',(201.294338356704,1.9447478055954,48.5));
#76197=CARTESIAN_POINT('Ctrl Pts',(201.294338356704,1.9447478055954,48.35));
#76198=CARTESIAN_POINT('Ctrl Pts',(201.294338356704,2.48499327898026,48.5));
#76199=CARTESIAN_POINT('Ctrl Pts',(201.294338356704,2.48499327898026,48.35));
#76200=CARTESIAN_POINT('',(201.167530667037,1.76466578245163,48.5));
#76201=CARTESIAN_POINT('Ctrl Pts',(201.167530667037,1.76466578245163,48.5));
#76202=CARTESIAN_POINT('Ctrl Pts',(201.294338356704,1.9447478055954,48.5));
#76203=CARTESIAN_POINT('Ctrl Pts',(201.294338356704,2.48499327898026,48.5));
#76204=CARTESIAN_POINT('',(201.167530667037,1.76466578245163,48.35));
#76205=CARTESIAN_POINT('',(201.167530667037,1.76466578245163,48.5));
#76206=CARTESIAN_POINT('Ctrl Pts',(201.167530667037,1.76466578245163,48.35));
#76207=CARTESIAN_POINT('Ctrl Pts',(201.294338356704,1.9447478055954,48.35));
#76208=CARTESIAN_POINT('Ctrl Pts',(201.294338356704,2.48499327898026,48.35));
#76209=CARTESIAN_POINT('Ctrl Pts',(200.854638468474,1.58458405733109,48.5));
#76210=CARTESIAN_POINT('Ctrl Pts',(200.854638468474,1.58458405733109,48.35));
#76211=CARTESIAN_POINT('Ctrl Pts',(201.04072297737,1.58458405733109,48.5));
#76212=CARTESIAN_POINT('Ctrl Pts',(201.04072297737,1.58458405733109,48.35));
#76213=CARTESIAN_POINT('Ctrl Pts',(201.167530667037,1.76466578245163,48.5));
#76214=CARTESIAN_POINT('Ctrl Pts',(201.167530667037,1.76466578245163,48.35));
#76215=CARTESIAN_POINT('',(200.854638468474,1.58458405733109,48.5));
#76216=CARTESIAN_POINT('Ctrl Pts',(200.854638468474,1.58458405733109,48.5));
#76217=CARTESIAN_POINT('Ctrl Pts',(201.04072297737,1.58458405733109,48.5));
#76218=CARTESIAN_POINT('Ctrl Pts',(201.167530667037,1.76466578245163,48.5));
#76219=CARTESIAN_POINT('',(200.854638468474,1.58458405733109,48.35));
#76220=CARTESIAN_POINT('',(200.854638468474,1.58458405733109,48.5));
#76221=CARTESIAN_POINT('Ctrl Pts',(200.854638468474,1.58458405733109,48.35));
#76222=CARTESIAN_POINT('Ctrl Pts',(201.04072297737,1.58458405733109,48.35));
#76223=CARTESIAN_POINT('Ctrl Pts',(201.167530667037,1.76466578245163,48.35));
#76224=CARTESIAN_POINT('Ctrl Pts',(200.541746269912,1.76391565799713,48.5));
#76225=CARTESIAN_POINT('Ctrl Pts',(200.541746269912,1.76391565799713,48.35));
#76226=CARTESIAN_POINT('Ctrl Pts',(200.668553959578,1.58458405733109,48.5));
#76227=CARTESIAN_POINT('Ctrl Pts',(200.668553959578,1.58458405733109,48.35));
#76228=CARTESIAN_POINT('Ctrl Pts',(200.854638468474,1.58458405733109,48.5));
#76229=CARTESIAN_POINT('Ctrl Pts',(200.854638468474,1.58458405733109,48.35));
#76230=CARTESIAN_POINT('',(200.541746269912,1.76391565799713,48.5));
#76231=CARTESIAN_POINT('Ctrl Pts',(200.541746269912,1.76391565799713,48.5));
#76232=CARTESIAN_POINT('Ctrl Pts',(200.668553959578,1.58458405733109,48.5));
#76233=CARTESIAN_POINT('Ctrl Pts',(200.854638468474,1.58458405733109,48.5));
#76234=CARTESIAN_POINT('',(200.541746269912,1.76391565799713,48.35));
#76235=CARTESIAN_POINT('',(200.541746269912,1.76391565799713,48.5));
#76236=CARTESIAN_POINT('Ctrl Pts',(200.541746269912,1.76391565799713,48.35));
#76237=CARTESIAN_POINT('Ctrl Pts',(200.668553959578,1.58458405733109,48.35));
#76238=CARTESIAN_POINT('Ctrl Pts',(200.854638468474,1.58458405733109,48.35));
#76239=CARTESIAN_POINT('Ctrl Pts',(200.414938580245,2.48499327898026,48.5));
#76240=CARTESIAN_POINT('Ctrl Pts',(200.414938580245,2.48499327898026,48.35));
#76241=CARTESIAN_POINT('Ctrl Pts',(200.414938580245,1.94324696063995,48.5));
#76242=CARTESIAN_POINT('Ctrl Pts',(200.414938580245,1.94324696063995,48.35));
#76243=CARTESIAN_POINT('Ctrl Pts',(200.541746269912,1.76391565799713,48.5));
#76244=CARTESIAN_POINT('Ctrl Pts',(200.541746269912,1.76391565799713,48.35));
#76245=CARTESIAN_POINT('',(200.414938580245,2.48499327898026,48.5));
#76246=CARTESIAN_POINT('Ctrl Pts',(200.414938580245,2.48499327898026,48.5));
#76247=CARTESIAN_POINT('Ctrl Pts',(200.414938580245,1.94324696063995,48.5));
#76248=CARTESIAN_POINT('Ctrl Pts',(200.541746269912,1.76391565799713,48.5));
#76249=CARTESIAN_POINT('',(200.414938580245,2.48499327898026,48.35));
#76250=CARTESIAN_POINT('',(200.414938580245,2.48499327898026,48.5));
#76251=CARTESIAN_POINT('Ctrl Pts',(200.414938580245,2.48499327898026,48.35));
#76252=CARTESIAN_POINT('Ctrl Pts',(200.414938580245,1.94324696063995,48.35));
#76253=CARTESIAN_POINT('Ctrl Pts',(200.541746269912,1.76391565799713,48.35));
#76254=CARTESIAN_POINT('Ctrl Pts',(200.55450225994,3.22783091664314,48.5));
#76255=CARTESIAN_POINT('Ctrl Pts',(200.55450225994,3.22783091664314,48.35));
#76256=CARTESIAN_POINT('Ctrl Pts',(200.414938580245,3.02673944830894,48.5));
#76257=CARTESIAN_POINT('Ctrl Pts',(200.414938580245,3.02673944830894,48.35));
#76258=CARTESIAN_POINT('Ctrl Pts',(200.414938580245,2.48499327898026,48.5));
#76259=CARTESIAN_POINT('Ctrl Pts',(200.414938580245,2.48499327898026,48.35));
#76260=CARTESIAN_POINT('Ctrl Pts',(200.55450225994,3.22783091664314,48.5));
#76261=CARTESIAN_POINT('Ctrl Pts',(200.414938580245,3.02673944830894,48.5));
#76262=CARTESIAN_POINT('Ctrl Pts',(200.414938580245,2.48499327898026,48.5));
#76263=CARTESIAN_POINT('Ctrl Pts',(200.55450225994,3.22783091664314,48.35));
#76264=CARTESIAN_POINT('Ctrl Pts',(200.414938580245,3.02673944830894,48.35));
#76265=CARTESIAN_POINT('Ctrl Pts',(200.414938580245,2.48499327898026,48.35));
#76266=CARTESIAN_POINT('Ctrl Pts',(200.854638468474,1.36248314380646,48.5));
#76267=CARTESIAN_POINT('Ctrl Pts',(200.854638468474,1.36248314380646,48.35));
#76268=CARTESIAN_POINT('Ctrl Pts',(200.536493908614,1.36248314380646,48.5));
#76269=CARTESIAN_POINT('Ctrl Pts',(200.536493908614,1.36248314380646,48.35));
#76270=CARTESIAN_POINT('Ctrl Pts',(200.354911338538,1.59058684110642,48.5));
#76271=CARTESIAN_POINT('Ctrl Pts',(200.354911338538,1.59058684110642,48.35));
#76272=CARTESIAN_POINT('',(200.854638468474,1.36248314380646,48.5));
#76273=CARTESIAN_POINT('',(200.354911338538,1.59058684110642,48.5));
#76274=CARTESIAN_POINT('Ctrl Pts',(200.854638468474,1.36248314380646,48.5));
#76275=CARTESIAN_POINT('Ctrl Pts',(200.536493908614,1.36248314380646,48.5));
#76276=CARTESIAN_POINT('Ctrl Pts',(200.354911338538,1.59058684110642,48.5));
#76277=CARTESIAN_POINT('',(200.854638468474,1.36248314380646,48.35));
#76278=CARTESIAN_POINT('',(200.854638468474,1.36248314380646,48.5));
#76279=CARTESIAN_POINT('',(200.354911338538,1.59058684110642,48.35));
#76280=CARTESIAN_POINT('Ctrl Pts',(200.854638468474,1.36248314380646,48.35));
#76281=CARTESIAN_POINT('Ctrl Pts',(200.536493908614,1.36248314380646,48.35));
#76282=CARTESIAN_POINT('Ctrl Pts',(200.354911338538,1.59058684110642,48.35));
#76283=CARTESIAN_POINT('',(200.354911338538,1.59058684110642,48.5));
#76284=CARTESIAN_POINT('Ctrl Pts',(201.254570137709,1.49229192733765,48.5));
#76285=CARTESIAN_POINT('Ctrl Pts',(201.254570137709,1.49229192733765,48.35));
#76286=CARTESIAN_POINT('Ctrl Pts',(201.096248280257,1.36248314380646,48.5));
#76287=CARTESIAN_POINT('Ctrl Pts',(201.096248280257,1.36248314380646,48.35));
#76288=CARTESIAN_POINT('Ctrl Pts',(200.854638468474,1.36248314380646,48.5));
#76289=CARTESIAN_POINT('Ctrl Pts',(200.854638468474,1.36248314380646,48.35));
#76290=CARTESIAN_POINT('',(201.254570137709,1.49229192733765,48.5));
#76291=CARTESIAN_POINT('Ctrl Pts',(201.254570137709,1.49229192733765,48.5));
#76292=CARTESIAN_POINT('Ctrl Pts',(201.096248280257,1.36248314380646,48.5));
#76293=CARTESIAN_POINT('Ctrl Pts',(200.854638468474,1.36248314380646,48.5));
#76294=CARTESIAN_POINT('',(201.254570137709,1.49229192733765,48.35));
#76295=CARTESIAN_POINT('',(201.254570137709,1.49229192733765,48.5));
#76296=CARTESIAN_POINT('Ctrl Pts',(201.254570137709,1.49229192733765,48.35));
#76297=CARTESIAN_POINT('Ctrl Pts',(201.096248280257,1.36248314380646,48.35));
#76298=CARTESIAN_POINT('Ctrl Pts',(200.854638468474,1.36248314380646,48.35));
#76299=CARTESIAN_POINT('Ctrl Pts',(201.49242843315,1.85995900630951,48.5));
#76300=CARTESIAN_POINT('Ctrl Pts',(201.49242843315,1.85995900630951,48.35));
#76301=CARTESIAN_POINT('Ctrl Pts',(201.412891995162,1.62210100889206,48.5));
#76302=CARTESIAN_POINT('Ctrl Pts',(201.412891995162,1.62210100889206,48.35));
#76303=CARTESIAN_POINT('Ctrl Pts',(201.254570137709,1.49229192733765,48.5));
#76304=CARTESIAN_POINT('Ctrl Pts',(201.254570137709,1.49229192733765,48.35));
#76305=CARTESIAN_POINT('',(201.49242843315,1.85995900630951,48.5));
#76306=CARTESIAN_POINT('Ctrl Pts',(201.49242843315,1.85995900630951,48.5));
#76307=CARTESIAN_POINT('Ctrl Pts',(201.412891995162,1.62210100889206,48.5));
#76308=CARTESIAN_POINT('Ctrl Pts',(201.254570137709,1.49229192733765,48.5));
#76309=CARTESIAN_POINT('',(201.49242843315,1.85995900630951,48.35));
#76310=CARTESIAN_POINT('',(201.49242843315,1.85995900630951,48.5));
#76311=CARTESIAN_POINT('Ctrl Pts',(201.49242843315,1.85995900630951,48.35));
#76312=CARTESIAN_POINT('Ctrl Pts',(201.412891995162,1.62210100889206,48.35));
#76313=CARTESIAN_POINT('Ctrl Pts',(201.254570137709,1.49229192733765,48.35));
#76314=CARTESIAN_POINT('Ctrl Pts',(201.571964275092,2.48499327898026,48.5));
#76315=CARTESIAN_POINT('Ctrl Pts',(201.571964275092,2.48499327898026,48.35));
#76316=CARTESIAN_POINT('Ctrl Pts',(201.571964275092,2.09781730175018,48.5));
#76317=CARTESIAN_POINT('Ctrl Pts',(201.571964275092,2.09781730175018,48.35));
#76318=CARTESIAN_POINT('Ctrl Pts',(201.49242843315,1.85995900630951,48.5));
#76319=CARTESIAN_POINT('Ctrl Pts',(201.49242843315,1.85995900630951,48.35));
#76320=CARTESIAN_POINT('',(201.571964275092,2.48499327898026,48.5));
#76321=CARTESIAN_POINT('Ctrl Pts',(201.571964275092,2.48499327898026,48.5));
#76322=CARTESIAN_POINT('Ctrl Pts',(201.571964275092,2.09781730175018,48.5));
#76323=CARTESIAN_POINT('Ctrl Pts',(201.49242843315,1.85995900630951,48.5));
#76324=CARTESIAN_POINT('',(201.571964275092,2.48499327898026,48.35));
#76325=CARTESIAN_POINT('',(201.571964275092,2.48499327898026,48.5));
#76326=CARTESIAN_POINT('Ctrl Pts',(201.571964275092,2.48499327898026,48.35));
#76327=CARTESIAN_POINT('Ctrl Pts',(201.571964275092,2.09781730175018,48.35));
#76328=CARTESIAN_POINT('Ctrl Pts',(201.49242843315,1.85995900630951,48.35));
#76329=CARTESIAN_POINT('Ctrl Pts',(201.52244175598,3.00497958064079,48.5));
#76330=CARTESIAN_POINT('Ctrl Pts',(201.52244175598,3.00497958064079,48.35));
#76331=CARTESIAN_POINT('Ctrl Pts',(201.571964275092,2.81214186549187,48.5));
#76332=CARTESIAN_POINT('Ctrl Pts',(201.571964275092,2.81214186549187,48.35));
#76333=CARTESIAN_POINT('Ctrl Pts',(201.571964275092,2.48499327898026,48.5));
#76334=CARTESIAN_POINT('Ctrl Pts',(201.571964275092,2.48499327898026,48.35));
#76335=CARTESIAN_POINT('',(201.52244175598,3.00497958064079,48.5));
#76336=CARTESIAN_POINT('Ctrl Pts',(201.52244175598,3.00497958064079,48.5));
#76337=CARTESIAN_POINT('Ctrl Pts',(201.571964275092,2.81214186549187,48.5));
#76338=CARTESIAN_POINT('Ctrl Pts',(201.571964275092,2.48499327898026,48.5));
#76339=CARTESIAN_POINT('',(201.52244175598,3.00497958064079,48.35));
#76340=CARTESIAN_POINT('',(201.52244175598,3.00497958064079,48.5));
#76341=CARTESIAN_POINT('Ctrl Pts',(201.52244175598,3.00497958064079,48.35));
#76342=CARTESIAN_POINT('Ctrl Pts',(201.571964275092,2.81214186549187,48.35));
#76343=CARTESIAN_POINT('Ctrl Pts',(201.571964275092,2.48499327898026,48.35));
#76344=CARTESIAN_POINT('Ctrl Pts',(201.385879766196,3.33212831616402,48.5));
#76345=CARTESIAN_POINT('Ctrl Pts',(201.385879766196,3.33212831616402,48.35));
#76346=CARTESIAN_POINT('Ctrl Pts',(201.472919236869,3.19781729578972,48.5));
#76347=CARTESIAN_POINT('Ctrl Pts',(201.472919236869,3.19781729578972,48.35));
#76348=CARTESIAN_POINT('Ctrl Pts',(201.52244175598,3.00497958064079,48.5));
#76349=CARTESIAN_POINT('Ctrl Pts',(201.52244175598,3.00497958064079,48.35));
#76350=CARTESIAN_POINT('',(201.385879766196,3.33212831616402,48.5));
#76351=CARTESIAN_POINT('Ctrl Pts',(201.385879766196,3.33212831616402,48.5));
#76352=CARTESIAN_POINT('Ctrl Pts',(201.472919236869,3.19781729578972,48.5));
#76353=CARTESIAN_POINT('Ctrl Pts',(201.52244175598,3.00497958064079,48.5));
#76354=CARTESIAN_POINT('',(201.385879766196,3.33212831616402,48.35));
#76355=CARTESIAN_POINT('',(201.385879766196,3.33212831616402,48.5));
#76356=CARTESIAN_POINT('Ctrl Pts',(201.385879766196,3.33212831616402,48.35));
#76357=CARTESIAN_POINT('Ctrl Pts',(201.472919236869,3.19781729578972,48.35));
#76358=CARTESIAN_POINT('Ctrl Pts',(201.52244175598,3.00497958064079,48.35));
#76359=CARTESIAN_POINT('Ctrl Pts',(201.16527999565,3.5377217233181,48.5));
#76360=CARTESIAN_POINT('Ctrl Pts',(201.16527999565,3.5377217233181,48.35));
#76361=CARTESIAN_POINT('Ctrl Pts',(201.298840295523,3.46643933653831,48.5));
#76362=CARTESIAN_POINT('Ctrl Pts',(201.298840295523,3.46643933653831,48.35));
#76363=CARTESIAN_POINT('Ctrl Pts',(201.385879766196,3.33212831616402,48.5));
#76364=CARTESIAN_POINT('Ctrl Pts',(201.385879766196,3.33212831616402,48.35));
#76365=CARTESIAN_POINT('',(201.16527999565,3.5377217233181,48.5));
#76366=CARTESIAN_POINT('Ctrl Pts',(201.16527999565,3.5377217233181,48.5));
#76367=CARTESIAN_POINT('Ctrl Pts',(201.298840295523,3.46643933653831,48.5));
#76368=CARTESIAN_POINT('Ctrl Pts',(201.385879766196,3.33212831616402,48.5));
#76369=CARTESIAN_POINT('',(201.16527999565,3.5377217233181,48.35));
#76370=CARTESIAN_POINT('',(201.16527999565,3.5377217233181,48.5));
#76371=CARTESIAN_POINT('Ctrl Pts',(201.16527999565,3.5377217233181,48.35));
#76372=CARTESIAN_POINT('Ctrl Pts',(201.298840295523,3.46643933653831,48.35));
#76373=CARTESIAN_POINT('Ctrl Pts',(201.385879766196,3.33212831616402,48.35));
#76374=CARTESIAN_POINT('Ctrl Pts',(200.854638468474,3.60900411009789,48.5));
#76375=CARTESIAN_POINT('Ctrl Pts',(200.854638468474,3.60900411009789,48.35));
#76376=CARTESIAN_POINT('Ctrl Pts',(201.03171909973,3.60900411009789,48.5));
#76377=CARTESIAN_POINT('Ctrl Pts',(201.03171909973,3.60900411009789,48.35));
#76378=CARTESIAN_POINT('Ctrl Pts',(201.16527999565,3.5377217233181,48.5));
#76379=CARTESIAN_POINT('Ctrl Pts',(201.16527999565,3.5377217233181,48.35));
#76380=CARTESIAN_POINT('',(200.854638468474,3.60900411009789,48.5));
#76381=CARTESIAN_POINT('Ctrl Pts',(200.854638468474,3.60900411009789,48.5));
#76382=CARTESIAN_POINT('Ctrl Pts',(201.03171909973,3.60900411009789,48.5));
#76383=CARTESIAN_POINT('Ctrl Pts',(201.16527999565,3.5377217233181,48.5));
#76384=CARTESIAN_POINT('',(200.854638468474,3.60900411009789,48.35));
#76385=CARTESIAN_POINT('',(200.854638468474,3.60900411009789,48.5));
#76386=CARTESIAN_POINT('Ctrl Pts',(200.854638468474,3.60900411009789,48.35));
#76387=CARTESIAN_POINT('Ctrl Pts',(201.03171909973,3.60900411009789,48.35));
#76388=CARTESIAN_POINT('Ctrl Pts',(201.16527999565,3.5377217233181,48.35));
#76389=CARTESIAN_POINT('Ctrl Pts',(200.456207644194,3.47994545102119,48.5));
#76390=CARTESIAN_POINT('Ctrl Pts',(200.456207644194,3.47994545102119,48.35));
#76391=CARTESIAN_POINT('Ctrl Pts',(200.614529501647,3.60900411009789,48.5));
#76392=CARTESIAN_POINT('Ctrl Pts',(200.614529501647,3.60900411009789,48.35));
#76393=CARTESIAN_POINT('Ctrl Pts',(200.854638468474,3.60900411009789,48.5));
#76394=CARTESIAN_POINT('Ctrl Pts',(200.854638468474,3.60900411009789,48.35));
#76395=CARTESIAN_POINT('',(200.456207644194,3.47994545102119,48.5));
#76396=CARTESIAN_POINT('Ctrl Pts',(200.456207644194,3.47994545102119,48.5));
#76397=CARTESIAN_POINT('Ctrl Pts',(200.614529501647,3.60900411009789,48.5));
#76398=CARTESIAN_POINT('Ctrl Pts',(200.854638468474,3.60900411009789,48.5));
#76399=CARTESIAN_POINT('',(200.456207644194,3.47994545102119,48.35));
#76400=CARTESIAN_POINT('',(200.456207644194,3.47994545102119,48.5));
#76401=CARTESIAN_POINT('Ctrl Pts',(200.456207644194,3.47994545102119,48.35));
#76402=CARTESIAN_POINT('Ctrl Pts',(200.614529501647,3.60900411009789,48.35));
#76403=CARTESIAN_POINT('Ctrl Pts',(200.854638468474,3.60900411009789,48.35));
#76404=CARTESIAN_POINT('Ctrl Pts',(200.217598926276,3.11302864551544,48.5));
#76405=CARTESIAN_POINT('Ctrl Pts',(200.217598926276,3.11302864551544,48.35));
#76406=CARTESIAN_POINT('Ctrl Pts',(200.297885488719,3.3508867919445,48.5));
#76407=CARTESIAN_POINT('Ctrl Pts',(200.297885488719,3.3508867919445,48.35));
#76408=CARTESIAN_POINT('Ctrl Pts',(200.456207644194,3.47994545102119,48.5));
#76409=CARTESIAN_POINT('Ctrl Pts',(200.456207644194,3.47994545102119,48.35));
#76410=CARTESIAN_POINT('',(200.217598926276,3.11302864551544,48.5));
#76411=CARTESIAN_POINT('Ctrl Pts',(200.217598926276,3.11302864551544,48.5));
#76412=CARTESIAN_POINT('Ctrl Pts',(200.297885488719,3.3508867919445,48.5));
#76413=CARTESIAN_POINT('Ctrl Pts',(200.456207644194,3.47994545102119,48.5));
#76414=CARTESIAN_POINT('',(200.217598926276,3.11302864551544,48.35));
#76415=CARTESIAN_POINT('',(200.217598926276,3.11302864551544,48.5));
#76416=CARTESIAN_POINT('Ctrl Pts',(200.217598926276,3.11302864551544,48.35));
#76417=CARTESIAN_POINT('Ctrl Pts',(200.297885488719,3.3508867919445,48.35));
#76418=CARTESIAN_POINT('Ctrl Pts',(200.456207644194,3.47994545102119,48.35));
#76419=CARTESIAN_POINT('Ctrl Pts',(200.137312661856,2.48499327898026,48.5));
#76420=CARTESIAN_POINT('Ctrl Pts',(200.137312661856,2.48499327898026,48.35));
#76421=CARTESIAN_POINT('Ctrl Pts',(200.137312661856,2.87517049908638,48.5));
#76422=CARTESIAN_POINT('Ctrl Pts',(200.137312661856,2.87517049908638,48.35));
#76423=CARTESIAN_POINT('Ctrl Pts',(200.217598926276,3.11302864551544,48.5));
#76424=CARTESIAN_POINT('Ctrl Pts',(200.217598926276,3.11302864551544,48.35));
#76425=CARTESIAN_POINT('',(200.137312661856,2.48499327898026,48.5));
#76426=CARTESIAN_POINT('Ctrl Pts',(200.137312661856,2.48499327898026,48.5));
#76427=CARTESIAN_POINT('Ctrl Pts',(200.137312661856,2.87517049908638,48.5));
#76428=CARTESIAN_POINT('Ctrl Pts',(200.217598926276,3.11302864551544,48.5));
#76429=CARTESIAN_POINT('',(200.137312661856,2.48499327898026,48.35));
#76430=CARTESIAN_POINT('',(200.137312661856,2.48499327898026,48.5));
#76431=CARTESIAN_POINT('Ctrl Pts',(200.137312661856,2.48499327898026,48.35));
#76432=CARTESIAN_POINT('Ctrl Pts',(200.137312661856,2.87517049908638,48.35));
#76433=CARTESIAN_POINT('Ctrl Pts',(200.217598926276,3.11302864551544,48.35));
#76434=CARTESIAN_POINT('Ctrl Pts',(200.354911338538,1.59058684110642,48.5));
#76435=CARTESIAN_POINT('Ctrl Pts',(200.354911338538,1.59058684110642,48.35));
#76436=CARTESIAN_POINT('Ctrl Pts',(200.137312661856,1.86521166563034,48.5));
#76437=CARTESIAN_POINT('Ctrl Pts',(200.137312661856,1.86521166563034,48.35));
#76438=CARTESIAN_POINT('Ctrl Pts',(200.137312661856,2.48499327898026,48.5));
#76439=CARTESIAN_POINT('Ctrl Pts',(200.137312661856,2.48499327898026,48.35));
#76440=CARTESIAN_POINT('Ctrl Pts',(200.354911338538,1.59058684110642,48.5));
#76441=CARTESIAN_POINT('Ctrl Pts',(200.137312661856,1.86521166563034,48.5));
#76442=CARTESIAN_POINT('Ctrl Pts',(200.137312661856,2.48499327898026,48.5));
#76443=CARTESIAN_POINT('Ctrl Pts',(200.354911338538,1.59058684110642,48.35));
#76444=CARTESIAN_POINT('Ctrl Pts',(200.137312661856,1.86521166563034,48.35));
#76445=CARTESIAN_POINT('Ctrl Pts',(200.137312661856,2.48499327898026,48.35));
#76446=CARTESIAN_POINT('Origin',(199.999999951571,2.48574362695217,48.35));
#76447=CARTESIAN_POINT('Ctrl Pts',(199.145361732692,2.38444769382477,48.5));
#76448=CARTESIAN_POINT('Ctrl Pts',(199.145361732692,2.38444769382477,48.35));
#76449=CARTESIAN_POINT('Ctrl Pts',(199.332946937531,2.38444769382477,48.5));
#76450=CARTESIAN_POINT('Ctrl Pts',(199.332946937531,2.38444769382477,48.35));
#76451=CARTESIAN_POINT('Ctrl Pts',(199.453751694411,2.5157573223114,48.5));
#76452=CARTESIAN_POINT('Ctrl Pts',(199.453751694411,2.5157573223114,48.35));
#76453=CARTESIAN_POINT('',(199.145361732692,2.38444769382477,48.5));
#76454=CARTESIAN_POINT('',(199.453751694411,2.5157573223114,48.5));
#76455=CARTESIAN_POINT('Ctrl Pts',(199.145361732692,2.38444769382477,48.5));
#76456=CARTESIAN_POINT('Ctrl Pts',(199.332946937531,2.38444769382477,48.5));
#76457=CARTESIAN_POINT('Ctrl Pts',(199.453751694411,2.5157573223114,48.5));
#76458=CARTESIAN_POINT('',(199.145361732692,2.38444769382477,48.35));
#76459=CARTESIAN_POINT('',(199.145361732692,2.38444769382477,48.5));
#76460=CARTESIAN_POINT('',(199.453751694411,2.5157573223114,48.35));
#76461=CARTESIAN_POINT('Ctrl Pts',(199.145361732692,2.38444769382477,48.35));
#76462=CARTESIAN_POINT('Ctrl Pts',(199.332946937531,2.38444769382477,48.35));
#76463=CARTESIAN_POINT('Ctrl Pts',(199.453751694411,2.5157573223114,48.35));
#76464=CARTESIAN_POINT('',(199.453751694411,2.5157573223114,48.5));
#76465=CARTESIAN_POINT('Ctrl Pts',(198.832469534129,2.5157573223114,48.5));
#76466=CARTESIAN_POINT('Ctrl Pts',(198.832469534129,2.5157573223114,48.35));
#76467=CARTESIAN_POINT('Ctrl Pts',(198.959277223796,2.38444769382477,48.5));
#76468=CARTESIAN_POINT('Ctrl Pts',(198.959277223796,2.38444769382477,48.35));
#76469=CARTESIAN_POINT('Ctrl Pts',(199.145361732692,2.38444769382477,48.5));
#76470=CARTESIAN_POINT('Ctrl Pts',(199.145361732692,2.38444769382477,48.35));
#76471=CARTESIAN_POINT('',(198.832469534129,2.5157573223114,48.5));
#76472=CARTESIAN_POINT('Ctrl Pts',(198.832469534129,2.5157573223114,48.5));
#76473=CARTESIAN_POINT('Ctrl Pts',(198.959277223796,2.38444769382477,48.5));
#76474=CARTESIAN_POINT('Ctrl Pts',(199.145361732692,2.38444769382477,48.5));
#76475=CARTESIAN_POINT('',(198.832469534129,2.5157573223114,48.35));
#76476=CARTESIAN_POINT('',(198.832469534129,2.5157573223114,48.5));
#76477=CARTESIAN_POINT('Ctrl Pts',(198.832469534129,2.5157573223114,48.35));
#76478=CARTESIAN_POINT('Ctrl Pts',(198.959277223796,2.38444769382477,48.35));
#76479=CARTESIAN_POINT('Ctrl Pts',(199.145361732692,2.38444769382477,48.35));
#76480=CARTESIAN_POINT('Ctrl Pts',(198.705661844462,2.85716244578362,48.5));
#76481=CARTESIAN_POINT('Ctrl Pts',(198.705661844462,2.85716244578362,48.35));
#76482=CARTESIAN_POINT('Ctrl Pts',(198.705661844462,2.64706695079803,48.5));
#76483=CARTESIAN_POINT('Ctrl Pts',(198.705661844462,2.64706695079803,48.35));
#76484=CARTESIAN_POINT('Ctrl Pts',(198.832469534129,2.5157573223114,48.5));
#76485=CARTESIAN_POINT('Ctrl Pts',(198.832469534129,2.5157573223114,48.35));
#76486=CARTESIAN_POINT('',(198.705661844462,2.85716244578362,48.5));
#76487=CARTESIAN_POINT('Ctrl Pts',(198.705661844462,2.85716244578362,48.5));
#76488=CARTESIAN_POINT('Ctrl Pts',(198.705661844462,2.64706695079803,48.5));
#76489=CARTESIAN_POINT('Ctrl Pts',(198.832469534129,2.5157573223114,48.5));
#76490=CARTESIAN_POINT('',(198.705661844462,2.85716244578362,48.35));
#76491=CARTESIAN_POINT('',(198.705661844462,2.85716244578362,48.5));
#76492=CARTESIAN_POINT('Ctrl Pts',(198.705661844462,2.85716244578362,48.35));
#76493=CARTESIAN_POINT('Ctrl Pts',(198.705661844462,2.64706695079803,48.35));
#76494=CARTESIAN_POINT('Ctrl Pts',(198.832469534129,2.5157573223114,48.35));
#76495=CARTESIAN_POINT('Ctrl Pts',(198.839222442359,3.23833563923836,48.5));
#76496=CARTESIAN_POINT('Ctrl Pts',(198.839222442359,3.23833563923836,48.35));
#76497=CARTESIAN_POINT('Ctrl Pts',(198.705661844462,3.09126877784729,48.5));
#76498=CARTESIAN_POINT('Ctrl Pts',(198.705661844462,3.09126877784729,48.35));
#76499=CARTESIAN_POINT('Ctrl Pts',(198.705661844462,2.85716244578362,48.5));
#76500=CARTESIAN_POINT('Ctrl Pts',(198.705661844462,2.85716244578362,48.35));
#76501=CARTESIAN_POINT('',(198.839222442359,3.23833563923836,48.5));
#76502=CARTESIAN_POINT('Ctrl Pts',(198.839222442359,3.23833563923836,48.5));
#76503=CARTESIAN_POINT('Ctrl Pts',(198.705661844462,3.09126877784729,48.5));
#76504=CARTESIAN_POINT('Ctrl Pts',(198.705661844462,2.85716244578362,48.5));
#76505=CARTESIAN_POINT('',(198.839222442359,3.23833563923836,48.35));
#76506=CARTESIAN_POINT('',(198.839222442359,3.23833563923836,48.5));
#76507=CARTESIAN_POINT('Ctrl Pts',(198.839222442359,3.23833563923836,48.35));
#76508=CARTESIAN_POINT('Ctrl Pts',(198.705661844462,3.09126877784729,48.35));
#76509=CARTESIAN_POINT('Ctrl Pts',(198.705661844462,2.85716244578362,48.35));
#76510=CARTESIAN_POINT('Ctrl Pts',(199.152865063399,3.38540250062943,48.5));
#76511=CARTESIAN_POINT('Ctrl Pts',(199.152865063399,3.38540250062943,48.35));
#76512=CARTESIAN_POINT('Ctrl Pts',(198.972783338279,3.38540250062943,48.5));
#76513=CARTESIAN_POINT('Ctrl Pts',(198.972783338279,3.38540250062943,48.35));
#76514=CARTESIAN_POINT('Ctrl Pts',(198.839222442359,3.23833563923836,48.5));
#76515=CARTESIAN_POINT('Ctrl Pts',(198.839222442359,3.23833563923836,48.35));
#76516=CARTESIAN_POINT('',(199.152865063399,3.38540250062943,48.5));
#76517=CARTESIAN_POINT('Ctrl Pts',(199.152865063399,3.38540250062943,48.5));
#76518=CARTESIAN_POINT('Ctrl Pts',(198.972783338279,3.38540250062943,48.5));
#76519=CARTESIAN_POINT('Ctrl Pts',(198.839222442359,3.23833563923836,48.5));
#76520=CARTESIAN_POINT('',(199.152865063399,3.38540250062943,48.35));
#76521=CARTESIAN_POINT('',(199.152865063399,3.38540250062943,48.5));
#76522=CARTESIAN_POINT('Ctrl Pts',(199.152865063399,3.38540250062943,48.35));
#76523=CARTESIAN_POINT('Ctrl Pts',(198.972783338279,3.38540250062943,48.35));
#76524=CARTESIAN_POINT('Ctrl Pts',(198.839222442359,3.23833563923836,48.35));
#76525=CARTESIAN_POINT('Ctrl Pts',(199.450750600547,3.24884036183357,48.5));
#76526=CARTESIAN_POINT('Ctrl Pts',(199.450750600547,3.24884036183357,48.35));
#76527=CARTESIAN_POINT('Ctrl Pts',(199.326944302768,3.38540250062943,48.5));
#76528=CARTESIAN_POINT('Ctrl Pts',(199.326944302768,3.38540250062943,48.35));
#76529=CARTESIAN_POINT('Ctrl Pts',(199.152865063399,3.38540250062943,48.5));
#76530=CARTESIAN_POINT('Ctrl Pts',(199.152865063399,3.38540250062943,48.35));
#76531=CARTESIAN_POINT('',(199.450750600547,3.24884036183357,48.5));
#76532=CARTESIAN_POINT('Ctrl Pts',(199.450750600547,3.24884036183357,48.5));
#76533=CARTESIAN_POINT('Ctrl Pts',(199.326944302768,3.38540250062943,48.5));
#76534=CARTESIAN_POINT('Ctrl Pts',(199.152865063399,3.38540250062943,48.5));
#76535=CARTESIAN_POINT('',(199.450750600547,3.24884036183357,48.35));
#76536=CARTESIAN_POINT('',(199.450750600547,3.24884036183357,48.5));
#76537=CARTESIAN_POINT('Ctrl Pts',(199.450750600547,3.24884036183357,48.35));
#76538=CARTESIAN_POINT('Ctrl Pts',(199.326944302768,3.38540250062943,48.35));
#76539=CARTESIAN_POINT('Ctrl Pts',(199.152865063399,3.38540250062943,48.35));
#76540=CARTESIAN_POINT('Ctrl Pts',(199.574556600302,2.87967258691788,48.5));
#76541=CARTESIAN_POINT('Ctrl Pts',(199.574556600302,2.87967258691788,48.35));
#76542=CARTESIAN_POINT('Ctrl Pts',(199.574556600302,3.11227837204933,48.5));
#76543=CARTESIAN_POINT('Ctrl Pts',(199.574556600302,3.11227837204933,48.35));
#76544=CARTESIAN_POINT('Ctrl Pts',(199.450750600547,3.24884036183357,48.5));
#76545=CARTESIAN_POINT('Ctrl Pts',(199.450750600547,3.24884036183357,48.35));
#76546=CARTESIAN_POINT('',(199.574556600302,2.87967258691788,48.5));
#76547=CARTESIAN_POINT('Ctrl Pts',(199.574556600302,2.87967258691788,48.5));
#76548=CARTESIAN_POINT('Ctrl Pts',(199.574556600302,3.11227837204933,48.5));
#76549=CARTESIAN_POINT('Ctrl Pts',(199.450750600547,3.24884036183357,48.5));
#76550=CARTESIAN_POINT('',(199.574556600302,2.87967258691788,48.35));
#76551=CARTESIAN_POINT('',(199.574556600302,2.87967258691788,48.5));
#76552=CARTESIAN_POINT('Ctrl Pts',(199.574556600302,2.87967258691788,48.35));
#76553=CARTESIAN_POINT('Ctrl Pts',(199.574556600302,3.11227837204933,48.35));
#76554=CARTESIAN_POINT('Ctrl Pts',(199.450750600547,3.24884036183357,48.35));
#76555=CARTESIAN_POINT('Ctrl Pts',(199.453751694411,2.5157573223114,48.5));
#76556=CARTESIAN_POINT('Ctrl Pts',(199.453751694411,2.5157573223114,48.35));
#76557=CARTESIAN_POINT('Ctrl Pts',(199.574556600302,2.64706695079803,48.5));
#76558=CARTESIAN_POINT('Ctrl Pts',(199.574556600302,2.64706695079803,48.35));
#76559=CARTESIAN_POINT('Ctrl Pts',(199.574556600302,2.87967258691788,48.5));
#76560=CARTESIAN_POINT('Ctrl Pts',(199.574556600302,2.87967258691788,48.35));
#76561=CARTESIAN_POINT('Ctrl Pts',(199.453751694411,2.5157573223114,48.5));
#76562=CARTESIAN_POINT('Ctrl Pts',(199.574556600302,2.64706695079803,48.5));
#76563=CARTESIAN_POINT('Ctrl Pts',(199.574556600302,2.87967258691788,48.5));
#76564=CARTESIAN_POINT('Ctrl Pts',(199.453751694411,2.5157573223114,48.35));
#76565=CARTESIAN_POINT('Ctrl Pts',(199.574556600302,2.64706695079803,48.35));
#76566=CARTESIAN_POINT('Ctrl Pts',(199.574556600302,2.87967258691788,48.35));
#76567=CARTESIAN_POINT('Ctrl Pts',(199.086835037917,1.36248314380646,48.5));
#76568=CARTESIAN_POINT('Ctrl Pts',(199.086835037917,1.36248314380646,48.35));
#76569=CARTESIAN_POINT('Ctrl Pts',(198.828717719764,1.36248314380646,48.5));
#76570=CARTESIAN_POINT('Ctrl Pts',(198.828717719764,1.36248314380646,48.35));
#76571=CARTESIAN_POINT('Ctrl Pts',(198.665143501014,1.50579804182053,48.5));
#76572=CARTESIAN_POINT('Ctrl Pts',(198.665143501014,1.50579804182053,48.35));
#76573=CARTESIAN_POINT('',(199.086835037917,1.36248314380646,48.5));
#76574=CARTESIAN_POINT('',(198.665143501014,1.50579804182053,48.5));
#76575=CARTESIAN_POINT('Ctrl Pts',(199.086835037917,1.36248314380646,48.5));
#76576=CARTESIAN_POINT('Ctrl Pts',(198.828717719764,1.36248314380646,48.5));
#76577=CARTESIAN_POINT('Ctrl Pts',(198.665143501014,1.50579804182053,48.5));
#76578=CARTESIAN_POINT('',(199.086835037917,1.36248314380646,48.35));
#76579=CARTESIAN_POINT('',(199.086835037917,1.36248314380646,48.5));
#76580=CARTESIAN_POINT('',(198.665143501014,1.50579804182053,48.35));
#76581=CARTESIAN_POINT('Ctrl Pts',(199.086835037917,1.36248314380646,48.35));
#76582=CARTESIAN_POINT('Ctrl Pts',(198.828717719764,1.36248314380646,48.35));
#76583=CARTESIAN_POINT('Ctrl Pts',(198.665143501014,1.50579804182053,48.35));
#76584=CARTESIAN_POINT('',(198.665143501014,1.50579804182053,48.5));
#76585=CARTESIAN_POINT('Ctrl Pts',(199.510777842253,1.49304234981537,48.5));
#76586=CARTESIAN_POINT('Ctrl Pts',(199.510777842253,1.49304234981537,48.35));
#76587=CARTESIAN_POINT('Ctrl Pts',(199.329945545644,1.36248314380646,48.5));
#76588=CARTESIAN_POINT('Ctrl Pts',(199.329945545644,1.36248314380646,48.35));
#76589=CARTESIAN_POINT('Ctrl Pts',(199.086835037917,1.36248314380646,48.5));
#76590=CARTESIAN_POINT('Ctrl Pts',(199.086835037917,1.36248314380646,48.35));
#76591=CARTESIAN_POINT('',(199.510777842253,1.49304234981537,48.5));
#76592=CARTESIAN_POINT('Ctrl Pts',(199.510777842253,1.49304234981537,48.5));
#76593=CARTESIAN_POINT('Ctrl Pts',(199.329945545644,1.36248314380646,48.5));
#76594=CARTESIAN_POINT('Ctrl Pts',(199.086835037917,1.36248314380646,48.5));
#76595=CARTESIAN_POINT('',(199.510777842253,1.49304234981537,48.35));
#76596=CARTESIAN_POINT('',(199.510777842253,1.49304234981537,48.5));
#76597=CARTESIAN_POINT('Ctrl Pts',(199.510777842253,1.49304234981537,48.35));
#76598=CARTESIAN_POINT('Ctrl Pts',(199.329945545644,1.36248314380646,48.35));
#76599=CARTESIAN_POINT('Ctrl Pts',(199.086835037917,1.36248314380646,48.35));
#76600=CARTESIAN_POINT('Ctrl Pts',(199.783151399344,1.87346541881561,48.5));
#76601=CARTESIAN_POINT('Ctrl Pts',(199.783151399344,1.87346541881561,48.35));
#76602=CARTESIAN_POINT('Ctrl Pts',(199.691609989852,1.6236018538475,48.5));
#76603=CARTESIAN_POINT('Ctrl Pts',(199.691609989852,1.6236018538475,48.35));
#76604=CARTESIAN_POINT('Ctrl Pts',(199.510777842253,1.49304234981537,48.5));
#76605=CARTESIAN_POINT('Ctrl Pts',(199.510777842253,1.49304234981537,48.35));
#76606=CARTESIAN_POINT('',(199.783151399344,1.87346541881561,48.5));
#76607=CARTESIAN_POINT('Ctrl Pts',(199.783151399344,1.87346541881561,48.5));
#76608=CARTESIAN_POINT('Ctrl Pts',(199.691609989852,1.6236018538475,48.5));
#76609=CARTESIAN_POINT('Ctrl Pts',(199.510777842253,1.49304234981537,48.5));
#76610=CARTESIAN_POINT('',(199.783151399344,1.87346541881561,48.35));
#76611=CARTESIAN_POINT('',(199.783151399344,1.87346541881561,48.5));
#76612=CARTESIAN_POINT('Ctrl Pts',(199.783151399344,1.87346541881561,48.35));
#76613=CARTESIAN_POINT('Ctrl Pts',(199.691609989852,1.6236018538475,48.35));
#76614=CARTESIAN_POINT('Ctrl Pts',(199.510777842253,1.49304234981537,48.35));
#76615=CARTESIAN_POINT('Ctrl Pts',(199.874693404883,2.5450205206871,48.5));
#76616=CARTESIAN_POINT('Ctrl Pts',(199.874693404883,2.5450205206871,48.35));
#76617=CARTESIAN_POINT('Ctrl Pts',(199.874693404883,2.12332898378372,48.5));
#76618=CARTESIAN_POINT('Ctrl Pts',(199.874693404883,2.12332898378372,48.35));
#76619=CARTESIAN_POINT('Ctrl Pts',(199.783151399344,1.87346541881561,48.5));
#76620=CARTESIAN_POINT('Ctrl Pts',(199.783151399344,1.87346541881561,48.35));
#76621=CARTESIAN_POINT('',(199.874693404883,2.5450205206871,48.5));
#76622=CARTESIAN_POINT('Ctrl Pts',(199.874693404883,2.5450205206871,48.5));
#76623=CARTESIAN_POINT('Ctrl Pts',(199.874693404883,2.12332898378372,48.5));
#76624=CARTESIAN_POINT('Ctrl Pts',(199.783151399344,1.87346541881561,48.5));
#76625=CARTESIAN_POINT('',(199.874693404883,2.5450205206871,48.35));
#76626=CARTESIAN_POINT('',(199.874693404883,2.5450205206871,48.5));
#76627=CARTESIAN_POINT('Ctrl Pts',(199.874693404883,2.5450205206871,48.35));
#76628=CARTESIAN_POINT('Ctrl Pts',(199.874693404883,2.12332898378372,48.35));
#76629=CARTESIAN_POINT('Ctrl Pts',(199.783151399344,1.87346541881561,48.35));
#76630=CARTESIAN_POINT('Ctrl Pts',(199.78240127489,3.16405186057091,48.5));
#76631=CARTESIAN_POINT('Ctrl Pts',(199.78240127489,3.16405186057091,48.35));
#76632=CARTESIAN_POINT('Ctrl Pts',(199.874693404883,2.95020470023155,48.5));
#76633=CARTESIAN_POINT('Ctrl Pts',(199.874693404883,2.95020470023155,48.35));
#76634=CARTESIAN_POINT('Ctrl Pts',(199.874693404883,2.5450205206871,48.5));
#76635=CARTESIAN_POINT('Ctrl Pts',(199.874693404883,2.5450205206871,48.35));
#76636=CARTESIAN_POINT('',(199.78240127489,3.16405186057091,48.5));
#76637=CARTESIAN_POINT('Ctrl Pts',(199.78240127489,3.16405186057091,48.5));
#76638=CARTESIAN_POINT('Ctrl Pts',(199.874693404883,2.95020470023155,48.5));
#76639=CARTESIAN_POINT('Ctrl Pts',(199.874693404883,2.5450205206871,48.5));
#76640=CARTESIAN_POINT('',(199.78240127489,3.16405186057091,48.35));
#76641=CARTESIAN_POINT('',(199.78240127489,3.16405186057091,48.5));
#76642=CARTESIAN_POINT('Ctrl Pts',(199.78240127489,3.16405186057091,48.35));
#76643=CARTESIAN_POINT('Ctrl Pts',(199.874693404883,2.95020470023155,48.35));
#76644=CARTESIAN_POINT('Ctrl Pts',(199.874693404883,2.5450205206871,48.35));
#76645=CARTESIAN_POINT('Ctrl Pts',(199.512278389186,3.49345156550407,48.5));
#76646=CARTESIAN_POINT('Ctrl Pts',(199.512278389186,3.49345156550407,48.35));
#76647=CARTESIAN_POINT('Ctrl Pts',(199.690109144896,3.37789902091026,48.5));
#76648=CARTESIAN_POINT('Ctrl Pts',(199.690109144896,3.37789902091026,48.35));
#76649=CARTESIAN_POINT('Ctrl Pts',(199.78240127489,3.16405186057091,48.5));
#76650=CARTESIAN_POINT('Ctrl Pts',(199.78240127489,3.16405186057091,48.35));
#76651=CARTESIAN_POINT('',(199.512278389186,3.49345156550407,48.5));
#76652=CARTESIAN_POINT('Ctrl Pts',(199.512278389186,3.49345156550407,48.5));
#76653=CARTESIAN_POINT('Ctrl Pts',(199.690109144896,3.37789902091026,48.5));
#76654=CARTESIAN_POINT('Ctrl Pts',(199.78240127489,3.16405186057091,48.5));
#76655=CARTESIAN_POINT('',(199.512278389186,3.49345156550407,48.35));
#76656=CARTESIAN_POINT('',(199.512278389186,3.49345156550407,48.5));
#76657=CARTESIAN_POINT('Ctrl Pts',(199.512278389186,3.49345156550407,48.35));
#76658=CARTESIAN_POINT('Ctrl Pts',(199.690109144896,3.37789902091026,48.35));
#76659=CARTESIAN_POINT('Ctrl Pts',(199.78240127489,3.16405186057091,48.35));
#76660=CARTESIAN_POINT('Ctrl Pts',(199.119850050658,3.60900411009789,48.5));
#76661=CARTESIAN_POINT('Ctrl Pts',(199.119850050658,3.60900411009789,48.35));
#76662=CARTESIAN_POINT('Ctrl Pts',(199.334447633475,3.60900411009789,48.5));
#76663=CARTESIAN_POINT('Ctrl Pts',(199.334447633475,3.60900411009789,48.35));
#76664=CARTESIAN_POINT('Ctrl Pts',(199.512278389186,3.49345156550407,48.5));
#76665=CARTESIAN_POINT('Ctrl Pts',(199.512278389186,3.49345156550407,48.35));
#76666=CARTESIAN_POINT('',(199.119850050658,3.60900411009789,48.5));
#76667=CARTESIAN_POINT('Ctrl Pts',(199.119850050658,3.60900411009789,48.5));
#76668=CARTESIAN_POINT('Ctrl Pts',(199.334447633475,3.60900411009789,48.5));
#76669=CARTESIAN_POINT('Ctrl Pts',(199.512278389186,3.49345156550407,48.5));
#76670=CARTESIAN_POINT('',(199.119850050658,3.60900411009789,48.35));
#76671=CARTESIAN_POINT('',(199.119850050658,3.60900411009789,48.5));
#76672=CARTESIAN_POINT('Ctrl Pts',(199.119850050658,3.60900411009789,48.35));
#76673=CARTESIAN_POINT('Ctrl Pts',(199.334447633475,3.60900411009789,48.35));
#76674=CARTESIAN_POINT('Ctrl Pts',(199.512278389186,3.49345156550407,48.35));
#76675=CARTESIAN_POINT('Ctrl Pts',(198.625375282019,3.40491139888763,48.5));
#76676=CARTESIAN_POINT('Ctrl Pts',(198.625375282019,3.40491139888763,48.35));
#76677=CARTESIAN_POINT('Ctrl Pts',(198.822714935988,3.60900411009789,48.5));
#76678=CARTESIAN_POINT('Ctrl Pts',(198.822714935988,3.60900411009789,48.35));
#76679=CARTESIAN_POINT('Ctrl Pts',(199.119850050658,3.60900411009789,48.5));
#76680=CARTESIAN_POINT('Ctrl Pts',(199.119850050658,3.60900411009789,48.35));
#76681=CARTESIAN_POINT('',(198.625375282019,3.40491139888763,48.5));
#76682=CARTESIAN_POINT('Ctrl Pts',(198.625375282019,3.40491139888763,48.5));
#76683=CARTESIAN_POINT('Ctrl Pts',(198.822714935988,3.60900411009789,48.5));
#76684=CARTESIAN_POINT('Ctrl Pts',(199.119850050658,3.60900411009789,48.5));
#76685=CARTESIAN_POINT('',(198.625375282019,3.40491139888763,48.35));
#76686=CARTESIAN_POINT('',(198.625375282019,3.40491139888763,48.5));
#76687=CARTESIAN_POINT('Ctrl Pts',(198.625375282019,3.40491139888763,48.35));
#76688=CARTESIAN_POINT('Ctrl Pts',(198.822714935988,3.60900411009789,48.35));
#76689=CARTESIAN_POINT('Ctrl Pts',(199.119850050658,3.60900411009789,48.35));
#76690=CARTESIAN_POINT('Ctrl Pts',(198.428035628051,2.866166472435,48.5));
#76691=CARTESIAN_POINT('Ctrl Pts',(198.428035628051,2.866166472435,48.35));
#76692=CARTESIAN_POINT('Ctrl Pts',(198.428035628051,3.20081853866577,48.5));
#76693=CARTESIAN_POINT('Ctrl Pts',(198.428035628051,3.20081853866577,48.35));
#76694=CARTESIAN_POINT('Ctrl Pts',(198.625375282019,3.40491139888763,48.5));
#76695=CARTESIAN_POINT('Ctrl Pts',(198.625375282019,3.40491139888763,48.35));
#76696=CARTESIAN_POINT('',(198.428035628051,2.866166472435,48.5));
#76697=CARTESIAN_POINT('Ctrl Pts',(198.428035628051,2.866166472435,48.5));
#76698=CARTESIAN_POINT('Ctrl Pts',(198.428035628051,3.20081853866577,48.5));
#76699=CARTESIAN_POINT('Ctrl Pts',(198.625375282019,3.40491139888763,48.5));
#76700=CARTESIAN_POINT('',(198.428035628051,2.866166472435,48.35));
#76701=CARTESIAN_POINT('',(198.428035628051,2.866166472435,48.5));
#76702=CARTESIAN_POINT('Ctrl Pts',(198.428035628051,2.866166472435,48.35));
#76703=CARTESIAN_POINT('Ctrl Pts',(198.428035628051,3.20081853866577,48.35));
#76704=CARTESIAN_POINT('Ctrl Pts',(198.625375282019,3.40491139888763,48.35));
#76705=CARTESIAN_POINT('Ctrl Pts',(198.617121528834,2.34392920136452,48.5));
#76706=CARTESIAN_POINT('Ctrl Pts',(198.617121528834,2.34392920136452,48.35));
#76707=CARTESIAN_POINT('Ctrl Pts',(198.428035628051,2.54201912879944,48.5));
#76708=CARTESIAN_POINT('Ctrl Pts',(198.428035628051,2.54201912879944,48.35));
#76709=CARTESIAN_POINT('Ctrl Pts',(198.428035628051,2.866166472435,48.5));
#76710=CARTESIAN_POINT('Ctrl Pts',(198.428035628051,2.866166472435,48.35));
#76711=CARTESIAN_POINT('',(198.617121528834,2.34392920136452,48.5));
#76712=CARTESIAN_POINT('Ctrl Pts',(198.617121528834,2.34392920136452,48.5));
#76713=CARTESIAN_POINT('Ctrl Pts',(198.428035628051,2.54201912879944,48.5));
#76714=CARTESIAN_POINT('Ctrl Pts',(198.428035628051,2.866166472435,48.5));
#76715=CARTESIAN_POINT('',(198.617121528834,2.34392920136452,48.35));
#76716=CARTESIAN_POINT('',(198.617121528834,2.34392920136452,48.5));
#76717=CARTESIAN_POINT('Ctrl Pts',(198.617121528834,2.34392920136452,48.35));
#76718=CARTESIAN_POINT('Ctrl Pts',(198.428035628051,2.54201912879944,48.35));
#76719=CARTESIAN_POINT('Ctrl Pts',(198.428035628051,2.866166472435,48.35));
#76720=CARTESIAN_POINT('Ctrl Pts',(199.079331707209,2.14583912491798,48.5));
#76721=CARTESIAN_POINT('Ctrl Pts',(199.079331707209,2.14583912491798,48.35));
#76722=CARTESIAN_POINT('Ctrl Pts',(198.806207429618,2.14583912491798,48.5));
#76723=CARTESIAN_POINT('Ctrl Pts',(198.806207429618,2.14583912491798,48.35));
#76724=CARTESIAN_POINT('Ctrl Pts',(198.617121528834,2.34392920136452,48.5));
#76725=CARTESIAN_POINT('Ctrl Pts',(198.617121528834,2.34392920136452,48.35));
#76726=CARTESIAN_POINT('',(199.079331707209,2.14583912491798,48.5));
#76727=CARTESIAN_POINT('Ctrl Pts',(199.079331707209,2.14583912491798,48.5));
#76728=CARTESIAN_POINT('Ctrl Pts',(198.806207429618,2.14583912491798,48.5));
#76729=CARTESIAN_POINT('Ctrl Pts',(198.617121528834,2.34392920136452,48.5));
#76730=CARTESIAN_POINT('',(199.079331707209,2.14583912491798,48.35));
#76731=CARTESIAN_POINT('',(199.079331707209,2.14583912491798,48.5));
#76732=CARTESIAN_POINT('Ctrl Pts',(199.079331707209,2.14583912491798,48.35));
#76733=CARTESIAN_POINT('Ctrl Pts',(198.806207429618,2.14583912491798,48.35));
#76734=CARTESIAN_POINT('Ctrl Pts',(198.617121528834,2.34392920136452,48.35));
#76735=CARTESIAN_POINT('Ctrl Pts',(199.383219730109,2.22612553834915,48.5));
#76736=CARTESIAN_POINT('Ctrl Pts',(199.383219730109,2.22612553834915,48.35));
#76737=CARTESIAN_POINT('Ctrl Pts',(199.242905925959,2.14583912491798,48.5));
#76738=CARTESIAN_POINT('Ctrl Pts',(199.242905925959,2.14583912491798,48.35));
#76739=CARTESIAN_POINT('Ctrl Pts',(199.079331707209,2.14583912491798,48.5));
#76740=CARTESIAN_POINT('Ctrl Pts',(199.079331707209,2.14583912491798,48.35));
#76741=CARTESIAN_POINT('',(199.383219730109,2.22612553834915,48.5));
#76742=CARTESIAN_POINT('Ctrl Pts',(199.383219730109,2.22612553834915,48.5));
#76743=CARTESIAN_POINT('Ctrl Pts',(199.242905925959,2.14583912491798,48.5));
#76744=CARTESIAN_POINT('Ctrl Pts',(199.079331707209,2.14583912491798,48.5));
#76745=CARTESIAN_POINT('',(199.383219730109,2.22612553834915,48.35));
#76746=CARTESIAN_POINT('',(199.383219730109,2.22612553834915,48.5));
#76747=CARTESIAN_POINT('Ctrl Pts',(199.383219730109,2.22612553834915,48.35));
#76748=CARTESIAN_POINT('Ctrl Pts',(199.242905925959,2.14583912491798,48.35));
#76749=CARTESIAN_POINT('Ctrl Pts',(199.079331707209,2.14583912491798,48.35));
#76750=CARTESIAN_POINT('Ctrl Pts',(199.604570519179,2.43547075986862,48.5));
#76751=CARTESIAN_POINT('Ctrl Pts',(199.604570519179,2.43547075986862,48.35));
#76752=CARTESIAN_POINT('Ctrl Pts',(199.523533534259,2.30641210079193,48.5));
#76753=CARTESIAN_POINT('Ctrl Pts',(199.523533534259,2.30641210079193,48.35));
#76754=CARTESIAN_POINT('Ctrl Pts',(199.383219730109,2.22612553834915,48.5));
#76755=CARTESIAN_POINT('Ctrl Pts',(199.383219730109,2.22612553834915,48.35));
#76756=CARTESIAN_POINT('',(199.604570519179,2.43547075986862,48.5));
#76757=CARTESIAN_POINT('Ctrl Pts',(199.604570519179,2.43547075986862,48.5));
#76758=CARTESIAN_POINT('Ctrl Pts',(199.523533534259,2.30641210079193,48.5));
#76759=CARTESIAN_POINT('Ctrl Pts',(199.383219730109,2.22612553834915,48.5));
#76760=CARTESIAN_POINT('',(199.604570519179,2.43547075986862,48.35));
#76761=CARTESIAN_POINT('',(199.604570519179,2.43547075986862,48.5));
#76762=CARTESIAN_POINT('Ctrl Pts',(199.604570519179,2.43547075986862,48.35));
#76763=CARTESIAN_POINT('Ctrl Pts',(199.523533534259,2.30641210079193,48.35));
#76764=CARTESIAN_POINT('Ctrl Pts',(199.383219730109,2.22612553834915,48.35));
#76765=CARTESIAN_POINT('Ctrl Pts',(199.606071066111,2.3814463019371,48.5));
#76766=CARTESIAN_POINT('Ctrl Pts',(199.606071066111,2.3814463019371,48.35));
#76767=CARTESIAN_POINT('Ctrl Pts',(199.606071066111,2.39945435523987,48.5));
#76768=CARTESIAN_POINT('Ctrl Pts',(199.606071066111,2.39945435523987,48.35));
#76769=CARTESIAN_POINT('Ctrl Pts',(199.604570519179,2.43547075986862,48.5));
#76770=CARTESIAN_POINT('Ctrl Pts',(199.604570519179,2.43547075986862,48.35));
#76771=CARTESIAN_POINT('',(199.606071066111,2.3814463019371,48.5));
#76772=CARTESIAN_POINT('Ctrl Pts',(199.606071066111,2.3814463019371,48.5));
#76773=CARTESIAN_POINT('Ctrl Pts',(199.606071066111,2.39945435523987,48.5));
#76774=CARTESIAN_POINT('Ctrl Pts',(199.604570519179,2.43547075986862,48.5));
#76775=CARTESIAN_POINT('',(199.606071066111,2.3814463019371,48.35));
#76776=CARTESIAN_POINT('',(199.606071066111,2.3814463019371,48.5));
#76777=CARTESIAN_POINT('Ctrl Pts',(199.606071066111,2.3814463019371,48.35));
#76778=CARTESIAN_POINT('Ctrl Pts',(199.606071066111,2.39945435523987,48.35));
#76779=CARTESIAN_POINT('Ctrl Pts',(199.604570519179,2.43547075986862,48.35));
#76780=CARTESIAN_POINT('Ctrl Pts',(199.565552722663,2.05129617452621,48.5));
#76781=CARTESIAN_POINT('Ctrl Pts',(199.565552722663,2.05129617452621,48.35));
#76782=CARTESIAN_POINT('Ctrl Pts',(199.606071066111,2.21336984634399,48.5));
#76783=CARTESIAN_POINT('Ctrl Pts',(199.606071066111,2.21336984634399,48.35));
#76784=CARTESIAN_POINT('Ctrl Pts',(199.606071066111,2.3814463019371,48.5));
#76785=CARTESIAN_POINT('Ctrl Pts',(199.606071066111,2.3814463019371,48.35));
#76786=CARTESIAN_POINT('',(199.565552722663,2.05129617452621,48.5));
#76787=CARTESIAN_POINT('Ctrl Pts',(199.565552722663,2.05129617452621,48.5));
#76788=CARTESIAN_POINT('Ctrl Pts',(199.606071066111,2.21336984634399,48.5));
#76789=CARTESIAN_POINT('Ctrl Pts',(199.606071066111,2.3814463019371,48.5));
#76790=CARTESIAN_POINT('',(199.565552722663,2.05129617452621,48.35));
#76791=CARTESIAN_POINT('',(199.565552722663,2.05129617452621,48.5));
#76792=CARTESIAN_POINT('Ctrl Pts',(199.565552722663,2.05129617452621,48.35));
#76793=CARTESIAN_POINT('Ctrl Pts',(199.606071066111,2.21336984634399,48.35));
#76794=CARTESIAN_POINT('Ctrl Pts',(199.606071066111,2.3814463019371,48.35));
#76795=CARTESIAN_POINT('Ctrl Pts',(199.465006839484,1.79392898082733,48.5));
#76796=CARTESIAN_POINT('Ctrl Pts',(199.465006839484,1.79392898082733,48.35));
#76797=CARTESIAN_POINT('Ctrl Pts',(199.525034081191,1.88922250270844,48.5));
#76798=CARTESIAN_POINT('Ctrl Pts',(199.525034081191,1.88922250270844,48.35));
#76799=CARTESIAN_POINT('Ctrl Pts',(199.565552722663,2.05129617452621,48.5));
#76800=CARTESIAN_POINT('Ctrl Pts',(199.565552722663,2.05129617452621,48.35));
#76801=CARTESIAN_POINT('',(199.465006839484,1.79392898082733,48.5));
#76802=CARTESIAN_POINT('Ctrl Pts',(199.465006839484,1.79392898082733,48.5));
#76803=CARTESIAN_POINT('Ctrl Pts',(199.525034081191,1.88922250270844,48.5));
#76804=CARTESIAN_POINT('Ctrl Pts',(199.565552722663,2.05129617452621,48.5));
#76805=CARTESIAN_POINT('',(199.465006839484,1.79392898082733,48.35));
#76806=CARTESIAN_POINT('',(199.465006839484,1.79392898082733,48.5));
#76807=CARTESIAN_POINT('Ctrl Pts',(199.465006839484,1.79392898082733,48.35));
#76808=CARTESIAN_POINT('Ctrl Pts',(199.525034081191,1.88922250270844,48.35));
#76809=CARTESIAN_POINT('Ctrl Pts',(199.565552722663,2.05129617452621,48.35));
#76810=CARTESIAN_POINT('Ctrl Pts',(199.311187069863,1.64160990715027,48.5));
#76811=CARTESIAN_POINT('Ctrl Pts',(199.311187069863,1.64160990715027,48.35));
#76812=CARTESIAN_POINT('Ctrl Pts',(199.404979597777,1.69863575696945,48.5));
#76813=CARTESIAN_POINT('Ctrl Pts',(199.404979597777,1.69863575696945,48.35));
#76814=CARTESIAN_POINT('Ctrl Pts',(199.465006839484,1.79392898082733,48.5));
#76815=CARTESIAN_POINT('Ctrl Pts',(199.465006839484,1.79392898082733,48.35));
#76816=CARTESIAN_POINT('',(199.311187069863,1.64160990715027,48.5));
#76817=CARTESIAN_POINT('Ctrl Pts',(199.311187069863,1.64160990715027,48.5));
#76818=CARTESIAN_POINT('Ctrl Pts',(199.404979597777,1.69863575696945,48.5));
#76819=CARTESIAN_POINT('Ctrl Pts',(199.465006839484,1.79392898082733,48.5));
#76820=CARTESIAN_POINT('',(199.311187069863,1.64160990715027,48.35));
#76821=CARTESIAN_POINT('',(199.311187069863,1.64160990715027,48.5));
#76822=CARTESIAN_POINT('Ctrl Pts',(199.311187069863,1.64160990715027,48.35));
#76823=CARTESIAN_POINT('Ctrl Pts',(199.404979597777,1.69863575696945,48.35));
#76824=CARTESIAN_POINT('Ctrl Pts',(199.465006839484,1.79392898082733,48.35));
#76825=CARTESIAN_POINT('Ctrl Pts',(199.092837821692,1.58458405733109,48.5));
#76826=CARTESIAN_POINT('Ctrl Pts',(199.092837821692,1.58458405733109,48.35));
#76827=CARTESIAN_POINT('Ctrl Pts',(199.217394392937,1.58458405733109,48.5));
#76828=CARTESIAN_POINT('Ctrl Pts',(199.217394392937,1.58458405733109,48.35));
#76829=CARTESIAN_POINT('Ctrl Pts',(199.311187069863,1.64160990715027,48.5));
#76830=CARTESIAN_POINT('Ctrl Pts',(199.311187069863,1.64160990715027,48.35));
#76831=CARTESIAN_POINT('',(199.092837821692,1.58458405733109,48.5));
#76832=CARTESIAN_POINT('Ctrl Pts',(199.092837821692,1.58458405733109,48.5));
#76833=CARTESIAN_POINT('Ctrl Pts',(199.217394392937,1.58458405733109,48.5));
#76834=CARTESIAN_POINT('Ctrl Pts',(199.311187069863,1.64160990715027,48.5));
#76835=CARTESIAN_POINT('',(199.092837821692,1.58458405733109,48.35));
#76836=CARTESIAN_POINT('',(199.092837821692,1.58458405733109,48.5));
#76837=CARTESIAN_POINT('Ctrl Pts',(199.092837821692,1.58458405733109,48.35));
#76838=CARTESIAN_POINT('Ctrl Pts',(199.217394392937,1.58458405733109,48.35));
#76839=CARTESIAN_POINT('Ctrl Pts',(199.311187069863,1.64160990715027,48.35));
#76840=CARTESIAN_POINT('Ctrl Pts',(198.854229401797,1.66712158918381,48.5));
#76841=CARTESIAN_POINT('Ctrl Pts',(198.854229401797,1.66712158918381,48.35));
#76842=CARTESIAN_POINT('Ctrl Pts',(198.947271656245,1.58458405733109,48.5));
#76843=CARTESIAN_POINT('Ctrl Pts',(198.947271656245,1.58458405733109,48.35));
#76844=CARTESIAN_POINT('Ctrl Pts',(199.092837821692,1.58458405733109,48.5));
#76845=CARTESIAN_POINT('Ctrl Pts',(199.092837821692,1.58458405733109,48.35));
#76846=CARTESIAN_POINT('',(198.854229401797,1.66712158918381,48.5));
#76847=CARTESIAN_POINT('Ctrl Pts',(198.854229401797,1.66712158918381,48.5));
#76848=CARTESIAN_POINT('Ctrl Pts',(198.947271656245,1.58458405733109,48.5));
#76849=CARTESIAN_POINT('Ctrl Pts',(199.092837821692,1.58458405733109,48.5));
#76850=CARTESIAN_POINT('',(198.854229401797,1.66712158918381,48.35));
#76851=CARTESIAN_POINT('',(198.854229401797,1.66712158918381,48.5));
#76852=CARTESIAN_POINT('Ctrl Pts',(198.854229401797,1.66712158918381,48.35));
#76853=CARTESIAN_POINT('Ctrl Pts',(198.947271656245,1.58458405733109,48.35));
#76854=CARTESIAN_POINT('Ctrl Pts',(199.092837821692,1.58458405733109,48.35));
#76855=CARTESIAN_POINT('Ctrl Pts',(198.728172134608,1.93274223804474,48.5));
#76856=CARTESIAN_POINT('Ctrl Pts',(198.728172134608,1.93274223804474,48.35));
#76857=CARTESIAN_POINT('Ctrl Pts',(198.761187147349,1.74965912103653,48.5));
#76858=CARTESIAN_POINT('Ctrl Pts',(198.761187147349,1.74965912103653,48.35));
#76859=CARTESIAN_POINT('Ctrl Pts',(198.854229401797,1.66712158918381,48.5));
#76860=CARTESIAN_POINT('Ctrl Pts',(198.854229401797,1.66712158918381,48.35));
#76861=CARTESIAN_POINT('',(198.728172134608,1.93274223804474,48.5));
#76862=CARTESIAN_POINT('Ctrl Pts',(198.728172134608,1.93274223804474,48.5));
#76863=CARTESIAN_POINT('Ctrl Pts',(198.761187147349,1.74965912103653,48.5));
#76864=CARTESIAN_POINT('Ctrl Pts',(198.854229401797,1.66712158918381,48.5));
#76865=CARTESIAN_POINT('',(198.728172134608,1.93274223804474,48.35));
#76866=CARTESIAN_POINT('',(198.728172134608,1.93274223804474,48.5));
#76867=CARTESIAN_POINT('Ctrl Pts',(198.728172134608,1.93274223804474,48.35));
#76868=CARTESIAN_POINT('Ctrl Pts',(198.761187147349,1.74965912103653,48.35));
#76869=CARTESIAN_POINT('Ctrl Pts',(198.854229401797,1.66712158918381,48.35));
#76870=CARTESIAN_POINT('Origin',(198.468554120511,1.90873140096664,48.5));
#76871=CARTESIAN_POINT('',(198.468554120511,1.90873140096664,48.5));
#76872=CARTESIAN_POINT('',(100.355168273367,-7.16530967028919,48.5));
#76873=CARTESIAN_POINT('',(198.468554120511,1.90873140096664,48.35));
#76874=CARTESIAN_POINT('',(198.468554120511,1.90873140096664,48.5));
#76875=CARTESIAN_POINT('',(198.468554120511,1.90873140096664,48.35));
#76876=CARTESIAN_POINT('Ctrl Pts',(198.665143501014,1.50579804182053,48.5));
#76877=CARTESIAN_POINT('Ctrl Pts',(198.665143501014,1.50579804182053,48.35));
#76878=CARTESIAN_POINT('Ctrl Pts',(198.501569133252,1.64911323785782,48.5));
#76879=CARTESIAN_POINT('Ctrl Pts',(198.501569133252,1.64911323785782,48.35));
#76880=CARTESIAN_POINT('Ctrl Pts',(198.468554120511,1.90873140096664,48.5));
#76881=CARTESIAN_POINT('Ctrl Pts',(198.468554120511,1.90873140096664,48.35));
#76882=CARTESIAN_POINT('Ctrl Pts',(198.665143501014,1.50579804182053,48.5));
#76883=CARTESIAN_POINT('Ctrl Pts',(198.501569133252,1.64911323785782,48.5));
#76884=CARTESIAN_POINT('Ctrl Pts',(198.468554120511,1.90873140096664,48.5));
#76885=CARTESIAN_POINT('Ctrl Pts',(198.665143501014,1.50579804182053,48.35));
#76886=CARTESIAN_POINT('Ctrl Pts',(198.501569133252,1.64911323785782,48.35));
#76887=CARTESIAN_POINT('Ctrl Pts',(198.468554120511,1.90873140096664,48.35));
#76888=CARTESIAN_POINT('Origin',(199.999999951571,2.48574362695217,48.35));
#76889=CARTESIAN_POINT('Origin',(0.,8.,48.5));
#76890=CARTESIAN_POINT('Origin',(0.,8.,48.5));
#76891=CARTESIAN_POINT('Ctrl Pts',(190.853137893602,3.38540250062943,48.5));
#76892=CARTESIAN_POINT('Ctrl Pts',(190.853137893602,3.38540250062943,48.35));
#76893=CARTESIAN_POINT('Ctrl Pts',(190.667053086683,3.38540250062943,48.5));
#76894=CARTESIAN_POINT('Ctrl Pts',(190.667053086683,3.38540250062943,48.35));
#76895=CARTESIAN_POINT('Ctrl Pts',(190.556002778932,3.22783091664314,48.5));
#76896=CARTESIAN_POINT('Ctrl Pts',(190.556002778932,3.22783091664314,48.35));
#76897=CARTESIAN_POINT('',(190.853137893602,3.38540250062943,48.5));
#76898=CARTESIAN_POINT('',(190.556002778932,3.22783091664314,48.5));
#76899=CARTESIAN_POINT('Ctrl Pts',(190.853137893602,3.38540250062943,48.5));
#76900=CARTESIAN_POINT('Ctrl Pts',(190.667053086683,3.38540250062943,48.5));
#76901=CARTESIAN_POINT('Ctrl Pts',(190.556002778932,3.22783091664314,48.5));
#76902=CARTESIAN_POINT('',(190.853137893602,3.38540250062943,48.35));
#76903=CARTESIAN_POINT('',(190.853137893602,3.38540250062943,48.5));
#76904=CARTESIAN_POINT('',(190.556002778932,3.22783091664314,48.35));
#76905=CARTESIAN_POINT('Ctrl Pts',(190.853137893602,3.38540250062943,48.35));
#76906=CARTESIAN_POINT('Ctrl Pts',(190.667053086683,3.38540250062943,48.35));
#76907=CARTESIAN_POINT('Ctrl Pts',(190.556002778932,3.22783091664314,48.35));
#76908=CARTESIAN_POINT('',(190.556002778932,3.22783091664314,48.5));
#76909=CARTESIAN_POINT('Ctrl Pts',(191.169031186029,3.2068213224411,48.5));
#76910=CARTESIAN_POINT('Ctrl Pts',(191.169031186029,3.2068213224411,48.35));
#76911=CARTESIAN_POINT('Ctrl Pts',(191.042223496363,3.38540250062943,48.5));
#76912=CARTESIAN_POINT('Ctrl Pts',(191.042223496363,3.38540250062943,48.35));
#76913=CARTESIAN_POINT('Ctrl Pts',(190.853137893602,3.38540250062943,48.5));
#76914=CARTESIAN_POINT('Ctrl Pts',(190.853137893602,3.38540250062943,48.35));
#76915=CARTESIAN_POINT('',(191.169031186029,3.2068213224411,48.5));
#76916=CARTESIAN_POINT('Ctrl Pts',(191.169031186029,3.2068213224411,48.5));
#76917=CARTESIAN_POINT('Ctrl Pts',(191.042223496363,3.38540250062943,48.5));
#76918=CARTESIAN_POINT('Ctrl Pts',(190.853137893602,3.38540250062943,48.5));
#76919=CARTESIAN_POINT('',(191.169031186029,3.2068213224411,48.35));
#76920=CARTESIAN_POINT('',(191.169031186029,3.2068213224411,48.5));
#76921=CARTESIAN_POINT('Ctrl Pts',(191.169031186029,3.2068213224411,48.35));
#76922=CARTESIAN_POINT('Ctrl Pts',(191.042223496363,3.38540250062943,48.35));
#76923=CARTESIAN_POINT('Ctrl Pts',(190.853137893602,3.38540250062943,48.35));
#76924=CARTESIAN_POINT('Ctrl Pts',(191.295838875696,2.48499327898026,48.5));
#76925=CARTESIAN_POINT('Ctrl Pts',(191.295838875696,2.48499327898026,48.35));
#76926=CARTESIAN_POINT('Ctrl Pts',(191.295838875696,3.02824014425278,48.5));
#76927=CARTESIAN_POINT('Ctrl Pts',(191.295838875696,3.02824014425278,48.35));
#76928=CARTESIAN_POINT('Ctrl Pts',(191.169031186029,3.2068213224411,48.5));
#76929=CARTESIAN_POINT('Ctrl Pts',(191.169031186029,3.2068213224411,48.35));
#76930=CARTESIAN_POINT('',(191.295838875696,2.48499327898026,48.5));
#76931=CARTESIAN_POINT('Ctrl Pts',(191.295838875696,2.48499327898026,48.5));
#76932=CARTESIAN_POINT('Ctrl Pts',(191.295838875696,3.02824014425278,48.5));
#76933=CARTESIAN_POINT('Ctrl Pts',(191.169031186029,3.2068213224411,48.5));
#76934=CARTESIAN_POINT('',(191.295838875696,2.48499327898026,48.35));
#76935=CARTESIAN_POINT('',(191.295838875696,2.48499327898026,48.5));
#76936=CARTESIAN_POINT('Ctrl Pts',(191.295838875696,2.48499327898026,48.35));
#76937=CARTESIAN_POINT('Ctrl Pts',(191.295838875696,3.02824014425278,48.35));
#76938=CARTESIAN_POINT('Ctrl Pts',(191.169031186029,3.2068213224411,48.35));
#76939=CARTESIAN_POINT('Ctrl Pts',(191.169031186029,1.76466578245163,48.5));
#76940=CARTESIAN_POINT('Ctrl Pts',(191.169031186029,1.76466578245163,48.35));
#76941=CARTESIAN_POINT('Ctrl Pts',(191.295838875696,1.9447478055954,48.5));
#76942=CARTESIAN_POINT('Ctrl Pts',(191.295838875696,1.9447478055954,48.35));
#76943=CARTESIAN_POINT('Ctrl Pts',(191.295838875696,2.48499327898026,48.5));
#76944=CARTESIAN_POINT('Ctrl Pts',(191.295838875696,2.48499327898026,48.35));
#76945=CARTESIAN_POINT('',(191.169031186029,1.76466578245163,48.5));
#76946=CARTESIAN_POINT('Ctrl Pts',(191.169031186029,1.76466578245163,48.5));
#76947=CARTESIAN_POINT('Ctrl Pts',(191.295838875696,1.9447478055954,48.5));
#76948=CARTESIAN_POINT('Ctrl Pts',(191.295838875696,2.48499327898026,48.5));
#76949=CARTESIAN_POINT('',(191.169031186029,1.76466578245163,48.35));
#76950=CARTESIAN_POINT('',(191.169031186029,1.76466578245163,48.5));
#76951=CARTESIAN_POINT('Ctrl Pts',(191.169031186029,1.76466578245163,48.35));
#76952=CARTESIAN_POINT('Ctrl Pts',(191.295838875696,1.9447478055954,48.35));
#76953=CARTESIAN_POINT('Ctrl Pts',(191.295838875696,2.48499327898026,48.35));
#76954=CARTESIAN_POINT('Ctrl Pts',(190.856138987467,1.58458405733109,48.5));
#76955=CARTESIAN_POINT('Ctrl Pts',(190.856138987467,1.58458405733109,48.35));
#76956=CARTESIAN_POINT('Ctrl Pts',(191.042223496363,1.58458405733109,48.5));
#76957=CARTESIAN_POINT('Ctrl Pts',(191.042223496363,1.58458405733109,48.35));
#76958=CARTESIAN_POINT('Ctrl Pts',(191.169031186029,1.76466578245163,48.5));
#76959=CARTESIAN_POINT('Ctrl Pts',(191.169031186029,1.76466578245163,48.35));
#76960=CARTESIAN_POINT('',(190.856138987467,1.58458405733109,48.5));
#76961=CARTESIAN_POINT('Ctrl Pts',(190.856138987467,1.58458405733109,48.5));
#76962=CARTESIAN_POINT('Ctrl Pts',(191.042223496363,1.58458405733109,48.5));
#76963=CARTESIAN_POINT('Ctrl Pts',(191.169031186029,1.76466578245163,48.5));
#76964=CARTESIAN_POINT('',(190.856138987467,1.58458405733109,48.35));
#76965=CARTESIAN_POINT('',(190.856138987467,1.58458405733109,48.5));
#76966=CARTESIAN_POINT('Ctrl Pts',(190.856138987467,1.58458405733109,48.35));
#76967=CARTESIAN_POINT('Ctrl Pts',(191.042223496363,1.58458405733109,48.35));
#76968=CARTESIAN_POINT('Ctrl Pts',(191.169031186029,1.76466578245163,48.35));
#76969=CARTESIAN_POINT('Ctrl Pts',(190.543246788904,1.76391565799713,48.5));
#76970=CARTESIAN_POINT('Ctrl Pts',(190.543246788904,1.76391565799713,48.35));
#76971=CARTESIAN_POINT('Ctrl Pts',(190.670054478571,1.58458405733109,48.5));
#76972=CARTESIAN_POINT('Ctrl Pts',(190.670054478571,1.58458405733109,48.35));
#76973=CARTESIAN_POINT('Ctrl Pts',(190.856138987467,1.58458405733109,48.5));
#76974=CARTESIAN_POINT('Ctrl Pts',(190.856138987467,1.58458405733109,48.35));
#76975=CARTESIAN_POINT('',(190.543246788904,1.76391565799713,48.5));
#76976=CARTESIAN_POINT('Ctrl Pts',(190.543246788904,1.76391565799713,48.5));
#76977=CARTESIAN_POINT('Ctrl Pts',(190.670054478571,1.58458405733109,48.5));
#76978=CARTESIAN_POINT('Ctrl Pts',(190.856138987467,1.58458405733109,48.5));
#76979=CARTESIAN_POINT('',(190.543246788904,1.76391565799713,48.35));
#76980=CARTESIAN_POINT('',(190.543246788904,1.76391565799713,48.5));
#76981=CARTESIAN_POINT('Ctrl Pts',(190.543246788904,1.76391565799713,48.35));
#76982=CARTESIAN_POINT('Ctrl Pts',(190.670054478571,1.58458405733109,48.35));
#76983=CARTESIAN_POINT('Ctrl Pts',(190.856138987467,1.58458405733109,48.35));
#76984=CARTESIAN_POINT('Ctrl Pts',(190.416439099237,2.48499327898026,48.5));
#76985=CARTESIAN_POINT('Ctrl Pts',(190.416439099237,2.48499327898026,48.35));
#76986=CARTESIAN_POINT('Ctrl Pts',(190.416439099237,1.94324696063995,48.5));
#76987=CARTESIAN_POINT('Ctrl Pts',(190.416439099237,1.94324696063995,48.35));
#76988=CARTESIAN_POINT('Ctrl Pts',(190.543246788904,1.76391565799713,48.5));
#76989=CARTESIAN_POINT('Ctrl Pts',(190.543246788904,1.76391565799713,48.35));
#76990=CARTESIAN_POINT('',(190.416439099237,2.48499327898026,48.5));
#76991=CARTESIAN_POINT('Ctrl Pts',(190.416439099237,2.48499327898026,48.5));
#76992=CARTESIAN_POINT('Ctrl Pts',(190.416439099237,1.94324696063995,48.5));
#76993=CARTESIAN_POINT('Ctrl Pts',(190.543246788904,1.76391565799713,48.5));
#76994=CARTESIAN_POINT('',(190.416439099237,2.48499327898026,48.35));
#76995=CARTESIAN_POINT('',(190.416439099237,2.48499327898026,48.5));
#76996=CARTESIAN_POINT('Ctrl Pts',(190.416439099237,2.48499327898026,48.35));
#76997=CARTESIAN_POINT('Ctrl Pts',(190.416439099237,1.94324696063995,48.35));
#76998=CARTESIAN_POINT('Ctrl Pts',(190.543246788904,1.76391565799713,48.35));
#76999=CARTESIAN_POINT('Ctrl Pts',(190.556002778932,3.22783091664314,48.5));
#77000=CARTESIAN_POINT('Ctrl Pts',(190.556002778932,3.22783091664314,48.35));
#77001=CARTESIAN_POINT('Ctrl Pts',(190.416439099237,3.02673944830894,48.5));
#77002=CARTESIAN_POINT('Ctrl Pts',(190.416439099237,3.02673944830894,48.35));
#77003=CARTESIAN_POINT('Ctrl Pts',(190.416439099237,2.48499327898026,48.5));
#77004=CARTESIAN_POINT('Ctrl Pts',(190.416439099237,2.48499327898026,48.35));
#77005=CARTESIAN_POINT('Ctrl Pts',(190.556002778932,3.22783091664314,48.5));
#77006=CARTESIAN_POINT('Ctrl Pts',(190.416439099237,3.02673944830894,48.5));
#77007=CARTESIAN_POINT('Ctrl Pts',(190.416439099237,2.48499327898026,48.5));
#77008=CARTESIAN_POINT('Ctrl Pts',(190.556002778932,3.22783091664314,48.35));
#77009=CARTESIAN_POINT('Ctrl Pts',(190.416439099237,3.02673944830894,48.35));
#77010=CARTESIAN_POINT('Ctrl Pts',(190.416439099237,2.48499327898026,48.35));
#77011=CARTESIAN_POINT('Ctrl Pts',(190.856138987467,1.36248314380646,48.5));
#77012=CARTESIAN_POINT('Ctrl Pts',(190.856138987467,1.36248314380646,48.35));
#77013=CARTESIAN_POINT('Ctrl Pts',(190.537994427606,1.36248314380646,48.5));
#77014=CARTESIAN_POINT('Ctrl Pts',(190.537994427606,1.36248314380646,48.35));
#77015=CARTESIAN_POINT('Ctrl Pts',(190.35641185753,1.59058684110642,48.5));
#77016=CARTESIAN_POINT('Ctrl Pts',(190.35641185753,1.59058684110642,48.35));
#77017=CARTESIAN_POINT('',(190.856138987467,1.36248314380646,48.5));
#77018=CARTESIAN_POINT('',(190.35641185753,1.59058684110642,48.5));
#77019=CARTESIAN_POINT('Ctrl Pts',(190.856138987467,1.36248314380646,48.5));
#77020=CARTESIAN_POINT('Ctrl Pts',(190.537994427606,1.36248314380646,48.5));
#77021=CARTESIAN_POINT('Ctrl Pts',(190.35641185753,1.59058684110642,48.5));
#77022=CARTESIAN_POINT('',(190.856138987467,1.36248314380646,48.35));
#77023=CARTESIAN_POINT('',(190.856138987467,1.36248314380646,48.5));
#77024=CARTESIAN_POINT('',(190.35641185753,1.59058684110642,48.35));
#77025=CARTESIAN_POINT('Ctrl Pts',(190.856138987467,1.36248314380646,48.35));
#77026=CARTESIAN_POINT('Ctrl Pts',(190.537994427606,1.36248314380646,48.35));
#77027=CARTESIAN_POINT('Ctrl Pts',(190.35641185753,1.59058684110642,48.35));
#77028=CARTESIAN_POINT('',(190.35641185753,1.59058684110642,48.5));
#77029=CARTESIAN_POINT('Ctrl Pts',(191.256070656702,1.49229192733765,48.5));
#77030=CARTESIAN_POINT('Ctrl Pts',(191.256070656702,1.49229192733765,48.35));
#77031=CARTESIAN_POINT('Ctrl Pts',(191.09774879925,1.36248314380646,48.5));
#77032=CARTESIAN_POINT('Ctrl Pts',(191.09774879925,1.36248314380646,48.35));
#77033=CARTESIAN_POINT('Ctrl Pts',(190.856138987467,1.36248314380646,48.5));
#77034=CARTESIAN_POINT('Ctrl Pts',(190.856138987467,1.36248314380646,48.35));
#77035=CARTESIAN_POINT('',(191.256070656702,1.49229192733765,48.5));
#77036=CARTESIAN_POINT('Ctrl Pts',(191.256070656702,1.49229192733765,48.5));
#77037=CARTESIAN_POINT('Ctrl Pts',(191.09774879925,1.36248314380646,48.5));
#77038=CARTESIAN_POINT('Ctrl Pts',(190.856138987467,1.36248314380646,48.5));
#77039=CARTESIAN_POINT('',(191.256070656702,1.49229192733765,48.35));
#77040=CARTESIAN_POINT('',(191.256070656702,1.49229192733765,48.5));
#77041=CARTESIAN_POINT('Ctrl Pts',(191.256070656702,1.49229192733765,48.35));
#77042=CARTESIAN_POINT('Ctrl Pts',(191.09774879925,1.36248314380646,48.35));
#77043=CARTESIAN_POINT('Ctrl Pts',(190.856138987467,1.36248314380646,48.35));
#77044=CARTESIAN_POINT('Ctrl Pts',(191.493928952143,1.85995900630951,48.5));
#77045=CARTESIAN_POINT('Ctrl Pts',(191.493928952143,1.85995900630951,48.35));
#77046=CARTESIAN_POINT('Ctrl Pts',(191.414392514154,1.62210100889206,48.5));
#77047=CARTESIAN_POINT('Ctrl Pts',(191.414392514154,1.62210100889206,48.35));
#77048=CARTESIAN_POINT('Ctrl Pts',(191.256070656702,1.49229192733765,48.5));
#77049=CARTESIAN_POINT('Ctrl Pts',(191.256070656702,1.49229192733765,48.35));
#77050=CARTESIAN_POINT('',(191.493928952143,1.85995900630951,48.5));
#77051=CARTESIAN_POINT('Ctrl Pts',(191.493928952143,1.85995900630951,48.5));
#77052=CARTESIAN_POINT('Ctrl Pts',(191.414392514154,1.62210100889206,48.5));
#77053=CARTESIAN_POINT('Ctrl Pts',(191.256070656702,1.49229192733765,48.5));
#77054=CARTESIAN_POINT('',(191.493928952143,1.85995900630951,48.35));
#77055=CARTESIAN_POINT('',(191.493928952143,1.85995900630951,48.5));
#77056=CARTESIAN_POINT('Ctrl Pts',(191.493928952143,1.85995900630951,48.35));
#77057=CARTESIAN_POINT('Ctrl Pts',(191.414392514154,1.62210100889206,48.35));
#77058=CARTESIAN_POINT('Ctrl Pts',(191.256070656702,1.49229192733765,48.35));
#77059=CARTESIAN_POINT('Ctrl Pts',(191.573464794084,2.48499327898026,48.5));
#77060=CARTESIAN_POINT('Ctrl Pts',(191.573464794084,2.48499327898026,48.35));
#77061=CARTESIAN_POINT('Ctrl Pts',(191.573464794084,2.09781730175018,48.5));
#77062=CARTESIAN_POINT('Ctrl Pts',(191.573464794084,2.09781730175018,48.35));
#77063=CARTESIAN_POINT('Ctrl Pts',(191.493928952143,1.85995900630951,48.5));
#77064=CARTESIAN_POINT('Ctrl Pts',(191.493928952143,1.85995900630951,48.35));
#77065=CARTESIAN_POINT('',(191.573464794084,2.48499327898026,48.5));
#77066=CARTESIAN_POINT('Ctrl Pts',(191.573464794084,2.48499327898026,48.5));
#77067=CARTESIAN_POINT('Ctrl Pts',(191.573464794084,2.09781730175018,48.5));
#77068=CARTESIAN_POINT('Ctrl Pts',(191.493928952143,1.85995900630951,48.5));
#77069=CARTESIAN_POINT('',(191.573464794084,2.48499327898026,48.35));
#77070=CARTESIAN_POINT('',(191.573464794084,2.48499327898026,48.5));
#77071=CARTESIAN_POINT('Ctrl Pts',(191.573464794084,2.48499327898026,48.35));
#77072=CARTESIAN_POINT('Ctrl Pts',(191.573464794084,2.09781730175018,48.35));
#77073=CARTESIAN_POINT('Ctrl Pts',(191.493928952143,1.85995900630951,48.35));
#77074=CARTESIAN_POINT('Ctrl Pts',(191.523942274973,3.00497958064079,48.5));
#77075=CARTESIAN_POINT('Ctrl Pts',(191.523942274973,3.00497958064079,48.35));
#77076=CARTESIAN_POINT('Ctrl Pts',(191.573464794084,2.81214186549187,48.5));
#77077=CARTESIAN_POINT('Ctrl Pts',(191.573464794084,2.81214186549187,48.35));
#77078=CARTESIAN_POINT('Ctrl Pts',(191.573464794084,2.48499327898026,48.5));
#77079=CARTESIAN_POINT('Ctrl Pts',(191.573464794084,2.48499327898026,48.35));
#77080=CARTESIAN_POINT('',(191.523942274973,3.00497958064079,48.5));
#77081=CARTESIAN_POINT('Ctrl Pts',(191.523942274973,3.00497958064079,48.5));
#77082=CARTESIAN_POINT('Ctrl Pts',(191.573464794084,2.81214186549187,48.5));
#77083=CARTESIAN_POINT('Ctrl Pts',(191.573464794084,2.48499327898026,48.5));
#77084=CARTESIAN_POINT('',(191.523942274973,3.00497958064079,48.35));
#77085=CARTESIAN_POINT('',(191.523942274973,3.00497958064079,48.5));
#77086=CARTESIAN_POINT('Ctrl Pts',(191.523942274973,3.00497958064079,48.35));
#77087=CARTESIAN_POINT('Ctrl Pts',(191.573464794084,2.81214186549187,48.35));
#77088=CARTESIAN_POINT('Ctrl Pts',(191.573464794084,2.48499327898026,48.35));
#77089=CARTESIAN_POINT('Ctrl Pts',(191.387380285189,3.33212831616402,48.5));
#77090=CARTESIAN_POINT('Ctrl Pts',(191.387380285189,3.33212831616402,48.35));
#77091=CARTESIAN_POINT('Ctrl Pts',(191.474419755861,3.19781729578972,48.5));
#77092=CARTESIAN_POINT('Ctrl Pts',(191.474419755861,3.19781729578972,48.35));
#77093=CARTESIAN_POINT('Ctrl Pts',(191.523942274973,3.00497958064079,48.5));
#77094=CARTESIAN_POINT('Ctrl Pts',(191.523942274973,3.00497958064079,48.35));
#77095=CARTESIAN_POINT('',(191.387380285189,3.33212831616402,48.5));
#77096=CARTESIAN_POINT('Ctrl Pts',(191.387380285189,3.33212831616402,48.5));
#77097=CARTESIAN_POINT('Ctrl Pts',(191.474419755861,3.19781729578972,48.5));
#77098=CARTESIAN_POINT('Ctrl Pts',(191.523942274973,3.00497958064079,48.5));
#77099=CARTESIAN_POINT('',(191.387380285189,3.33212831616402,48.35));
#77100=CARTESIAN_POINT('',(191.387380285189,3.33212831616402,48.5));
#77101=CARTESIAN_POINT('Ctrl Pts',(191.387380285189,3.33212831616402,48.35));
#77102=CARTESIAN_POINT('Ctrl Pts',(191.474419755861,3.19781729578972,48.35));
#77103=CARTESIAN_POINT('Ctrl Pts',(191.523942274973,3.00497958064079,48.35));
#77104=CARTESIAN_POINT('Ctrl Pts',(191.166780514643,3.5377217233181,48.5));
#77105=CARTESIAN_POINT('Ctrl Pts',(191.166780514643,3.5377217233181,48.35));
#77106=CARTESIAN_POINT('Ctrl Pts',(191.300340814516,3.46643933653831,48.5));
#77107=CARTESIAN_POINT('Ctrl Pts',(191.300340814516,3.46643933653831,48.35));
#77108=CARTESIAN_POINT('Ctrl Pts',(191.387380285189,3.33212831616402,48.5));
#77109=CARTESIAN_POINT('Ctrl Pts',(191.387380285189,3.33212831616402,48.35));
#77110=CARTESIAN_POINT('',(191.166780514643,3.5377217233181,48.5));
#77111=CARTESIAN_POINT('Ctrl Pts',(191.166780514643,3.5377217233181,48.5));
#77112=CARTESIAN_POINT('Ctrl Pts',(191.300340814516,3.46643933653831,48.5));
#77113=CARTESIAN_POINT('Ctrl Pts',(191.387380285189,3.33212831616402,48.5));
#77114=CARTESIAN_POINT('',(191.166780514643,3.5377217233181,48.35));
#77115=CARTESIAN_POINT('',(191.166780514643,3.5377217233181,48.5));
#77116=CARTESIAN_POINT('Ctrl Pts',(191.166780514643,3.5377217233181,48.35));
#77117=CARTESIAN_POINT('Ctrl Pts',(191.300340814516,3.46643933653831,48.35));
#77118=CARTESIAN_POINT('Ctrl Pts',(191.387380285189,3.33212831616402,48.35));
#77119=CARTESIAN_POINT('Ctrl Pts',(190.856138987467,3.60900411009789,48.5));
#77120=CARTESIAN_POINT('Ctrl Pts',(190.856138987467,3.60900411009789,48.35));
#77121=CARTESIAN_POINT('Ctrl Pts',(191.033219618723,3.60900411009789,48.5));
#77122=CARTESIAN_POINT('Ctrl Pts',(191.033219618723,3.60900411009789,48.35));
#77123=CARTESIAN_POINT('Ctrl Pts',(191.166780514643,3.5377217233181,48.5));
#77124=CARTESIAN_POINT('Ctrl Pts',(191.166780514643,3.5377217233181,48.35));
#77125=CARTESIAN_POINT('',(190.856138987467,3.60900411009789,48.5));
#77126=CARTESIAN_POINT('Ctrl Pts',(190.856138987467,3.60900411009789,48.5));
#77127=CARTESIAN_POINT('Ctrl Pts',(191.033219618723,3.60900411009789,48.5));
#77128=CARTESIAN_POINT('Ctrl Pts',(191.166780514643,3.5377217233181,48.5));
#77129=CARTESIAN_POINT('',(190.856138987467,3.60900411009789,48.35));
#77130=CARTESIAN_POINT('',(190.856138987467,3.60900411009789,48.5));
#77131=CARTESIAN_POINT('Ctrl Pts',(190.856138987467,3.60900411009789,48.35));
#77132=CARTESIAN_POINT('Ctrl Pts',(191.033219618723,3.60900411009789,48.35));
#77133=CARTESIAN_POINT('Ctrl Pts',(191.166780514643,3.5377217233181,48.35));
#77134=CARTESIAN_POINT('Ctrl Pts',(190.457708163187,3.47994545102119,48.5));
#77135=CARTESIAN_POINT('Ctrl Pts',(190.457708163187,3.47994545102119,48.35));
#77136=CARTESIAN_POINT('Ctrl Pts',(190.616030020639,3.60900411009789,48.5));
#77137=CARTESIAN_POINT('Ctrl Pts',(190.616030020639,3.60900411009789,48.35));
#77138=CARTESIAN_POINT('Ctrl Pts',(190.856138987467,3.60900411009789,48.5));
#77139=CARTESIAN_POINT('Ctrl Pts',(190.856138987467,3.60900411009789,48.35));
#77140=CARTESIAN_POINT('',(190.457708163187,3.47994545102119,48.5));
#77141=CARTESIAN_POINT('Ctrl Pts',(190.457708163187,3.47994545102119,48.5));
#77142=CARTESIAN_POINT('Ctrl Pts',(190.616030020639,3.60900411009789,48.5));
#77143=CARTESIAN_POINT('Ctrl Pts',(190.856138987467,3.60900411009789,48.5));
#77144=CARTESIAN_POINT('',(190.457708163187,3.47994545102119,48.35));
#77145=CARTESIAN_POINT('',(190.457708163187,3.47994545102119,48.5));
#77146=CARTESIAN_POINT('Ctrl Pts',(190.457708163187,3.47994545102119,48.35));
#77147=CARTESIAN_POINT('Ctrl Pts',(190.616030020639,3.60900411009789,48.35));
#77148=CARTESIAN_POINT('Ctrl Pts',(190.856138987467,3.60900411009789,48.35));
#77149=CARTESIAN_POINT('Ctrl Pts',(190.219099445269,3.11302864551544,48.5));
#77150=CARTESIAN_POINT('Ctrl Pts',(190.219099445269,3.11302864551544,48.35));
#77151=CARTESIAN_POINT('Ctrl Pts',(190.299386007711,3.3508867919445,48.5));
#77152=CARTESIAN_POINT('Ctrl Pts',(190.299386007711,3.3508867919445,48.35));
#77153=CARTESIAN_POINT('Ctrl Pts',(190.457708163187,3.47994545102119,48.5));
#77154=CARTESIAN_POINT('Ctrl Pts',(190.457708163187,3.47994545102119,48.35));
#77155=CARTESIAN_POINT('',(190.219099445269,3.11302864551544,48.5));
#77156=CARTESIAN_POINT('Ctrl Pts',(190.219099445269,3.11302864551544,48.5));
#77157=CARTESIAN_POINT('Ctrl Pts',(190.299386007711,3.3508867919445,48.5));
#77158=CARTESIAN_POINT('Ctrl Pts',(190.457708163187,3.47994545102119,48.5));
#77159=CARTESIAN_POINT('',(190.219099445269,3.11302864551544,48.35));
#77160=CARTESIAN_POINT('',(190.219099445269,3.11302864551544,48.5));
#77161=CARTESIAN_POINT('Ctrl Pts',(190.219099445269,3.11302864551544,48.35));
#77162=CARTESIAN_POINT('Ctrl Pts',(190.299386007711,3.3508867919445,48.35));
#77163=CARTESIAN_POINT('Ctrl Pts',(190.457708163187,3.47994545102119,48.35));
#77164=CARTESIAN_POINT('Ctrl Pts',(190.138813180849,2.48499327898026,48.5));
#77165=CARTESIAN_POINT('Ctrl Pts',(190.138813180849,2.48499327898026,48.35));
#77166=CARTESIAN_POINT('Ctrl Pts',(190.138813180849,2.87517049908638,48.5));
#77167=CARTESIAN_POINT('Ctrl Pts',(190.138813180849,2.87517049908638,48.35));
#77168=CARTESIAN_POINT('Ctrl Pts',(190.219099445269,3.11302864551544,48.5));
#77169=CARTESIAN_POINT('Ctrl Pts',(190.219099445269,3.11302864551544,48.35));
#77170=CARTESIAN_POINT('',(190.138813180849,2.48499327898026,48.5));
#77171=CARTESIAN_POINT('Ctrl Pts',(190.138813180849,2.48499327898026,48.5));
#77172=CARTESIAN_POINT('Ctrl Pts',(190.138813180849,2.87517049908638,48.5));
#77173=CARTESIAN_POINT('Ctrl Pts',(190.219099445269,3.11302864551544,48.5));
#77174=CARTESIAN_POINT('',(190.138813180849,2.48499327898026,48.35));
#77175=CARTESIAN_POINT('',(190.138813180849,2.48499327898026,48.5));
#77176=CARTESIAN_POINT('Ctrl Pts',(190.138813180849,2.48499327898026,48.35));
#77177=CARTESIAN_POINT('Ctrl Pts',(190.138813180849,2.87517049908638,48.35));
#77178=CARTESIAN_POINT('Ctrl Pts',(190.219099445269,3.11302864551544,48.35));
#77179=CARTESIAN_POINT('Ctrl Pts',(190.35641185753,1.59058684110642,48.5));
#77180=CARTESIAN_POINT('Ctrl Pts',(190.35641185753,1.59058684110642,48.35));
#77181=CARTESIAN_POINT('Ctrl Pts',(190.138813180849,1.86521166563034,48.5));
#77182=CARTESIAN_POINT('Ctrl Pts',(190.138813180849,1.86521166563034,48.35));
#77183=CARTESIAN_POINT('Ctrl Pts',(190.138813180849,2.48499327898026,48.5));
#77184=CARTESIAN_POINT('Ctrl Pts',(190.138813180849,2.48499327898026,48.35));
#77185=CARTESIAN_POINT('Ctrl Pts',(190.35641185753,1.59058684110642,48.5));
#77186=CARTESIAN_POINT('Ctrl Pts',(190.138813180849,1.86521166563034,48.5));
#77187=CARTESIAN_POINT('Ctrl Pts',(190.138813180849,2.48499327898026,48.5));
#77188=CARTESIAN_POINT('Ctrl Pts',(190.35641185753,1.59058684110642,48.35));
#77189=CARTESIAN_POINT('Ctrl Pts',(190.138813180849,1.86521166563034,48.35));
#77190=CARTESIAN_POINT('Ctrl Pts',(190.138813180849,2.48499327898026,48.35));
#77191=CARTESIAN_POINT('Origin',(189.99999977462,2.48574362695217,48.35));
#77192=CARTESIAN_POINT('Ctrl Pts',(189.149863643572,3.38690319657326,48.5));
#77193=CARTESIAN_POINT('Ctrl Pts',(189.149863643572,3.38690319657326,48.35));
#77194=CARTESIAN_POINT('Ctrl Pts',(188.995293302462,3.38690319657326,48.5));
#77195=CARTESIAN_POINT('Ctrl Pts',(188.995293302462,3.38690319657326,48.35));
#77196=CARTESIAN_POINT('Ctrl Pts',(188.893246872351,3.28785815834999,48.5));
#77197=CARTESIAN_POINT('Ctrl Pts',(188.893246872351,3.28785815834999,48.35));
#77198=CARTESIAN_POINT('',(189.149863643572,3.38690319657326,48.5));
#77199=CARTESIAN_POINT('',(188.893246872351,3.28785815834999,48.5));
#77200=CARTESIAN_POINT('Ctrl Pts',(189.149863643572,3.38690319657326,48.5));
#77201=CARTESIAN_POINT('Ctrl Pts',(188.995293302462,3.38690319657326,48.5));
#77202=CARTESIAN_POINT('Ctrl Pts',(188.893246872351,3.28785815834999,48.5));
#77203=CARTESIAN_POINT('',(189.149863643572,3.38690319657326,48.35));
#77204=CARTESIAN_POINT('',(189.149863643572,3.38690319657326,48.5));
#77205=CARTESIAN_POINT('',(188.893246872351,3.28785815834999,48.35));
#77206=CARTESIAN_POINT('Ctrl Pts',(189.149863643572,3.38690319657326,48.35));
#77207=CARTESIAN_POINT('Ctrl Pts',(188.995293302462,3.38690319657326,48.35));
#77208=CARTESIAN_POINT('Ctrl Pts',(188.893246872351,3.28785815834999,48.35));
#77209=CARTESIAN_POINT('',(188.893246872351,3.28785815834999,48.5));
#77210=CARTESIAN_POINT('Ctrl Pts',(189.405729992315,3.28560718894005,48.5));
#77211=CARTESIAN_POINT('Ctrl Pts',(189.405729992315,3.28560718894005,48.35));
#77212=CARTESIAN_POINT('Ctrl Pts',(189.302933139727,3.38690319657326,48.5));
#77213=CARTESIAN_POINT('Ctrl Pts',(189.302933139727,3.38690319657326,48.35));
#77214=CARTESIAN_POINT('Ctrl Pts',(189.149863643572,3.38690319657326,48.5));
#77215=CARTESIAN_POINT('Ctrl Pts',(189.149863643572,3.38690319657326,48.35));
#77216=CARTESIAN_POINT('',(189.405729992315,3.28560718894005,48.5));
#77217=CARTESIAN_POINT('Ctrl Pts',(189.405729992315,3.28560718894005,48.5));
#77218=CARTESIAN_POINT('Ctrl Pts',(189.302933139727,3.38690319657326,48.5));
#77219=CARTESIAN_POINT('Ctrl Pts',(189.149863643572,3.38690319657326,48.5));
#77220=CARTESIAN_POINT('',(189.405729992315,3.28560718894005,48.35));
#77221=CARTESIAN_POINT('',(189.405729992315,3.28560718894005,48.5));
#77222=CARTESIAN_POINT('Ctrl Pts',(189.405729992315,3.28560718894005,48.35));
#77223=CARTESIAN_POINT('Ctrl Pts',(189.302933139727,3.38690319657326,48.35));
#77224=CARTESIAN_POINT('Ctrl Pts',(189.149863643572,3.38690319657326,48.35));
#77225=CARTESIAN_POINT('Ctrl Pts',(189.508526546881,3.03574362397194,48.5));
#77226=CARTESIAN_POINT('Ctrl Pts',(189.508526546881,3.03574362397194,48.35));
#77227=CARTESIAN_POINT('Ctrl Pts',(189.508526546881,3.18431103229523,48.5));
#77228=CARTESIAN_POINT('Ctrl Pts',(189.508526546881,3.18431103229523,48.35));
#77229=CARTESIAN_POINT('Ctrl Pts',(189.405729992315,3.28560718894005,48.5));
#77230=CARTESIAN_POINT('Ctrl Pts',(189.405729992315,3.28560718894005,48.35));
#77231=CARTESIAN_POINT('',(189.508526546881,3.03574362397194,48.5));
#77232=CARTESIAN_POINT('Ctrl Pts',(189.508526546881,3.03574362397194,48.5));
#77233=CARTESIAN_POINT('Ctrl Pts',(189.508526546881,3.18431103229523,48.5));
#77234=CARTESIAN_POINT('Ctrl Pts',(189.405729992315,3.28560718894005,48.5));
#77235=CARTESIAN_POINT('',(189.508526546881,3.03574362397194,48.35));
#77236=CARTESIAN_POINT('',(189.508526546881,3.03574362397194,48.5));
#77237=CARTESIAN_POINT('Ctrl Pts',(189.508526546881,3.03574362397194,48.35));
#77238=CARTESIAN_POINT('Ctrl Pts',(189.508526546881,3.18431103229523,48.35));
#77239=CARTESIAN_POINT('Ctrl Pts',(189.405729992315,3.28560718894005,48.35));
#77240=CARTESIAN_POINT('Ctrl Pts',(189.408731384203,2.79488408565521,48.5));
#77241=CARTESIAN_POINT('Ctrl Pts',(189.408731384203,2.79488408565521,48.35));
#77242=CARTESIAN_POINT('Ctrl Pts',(189.508526546881,2.89317870140076,48.5));
#77243=CARTESIAN_POINT('Ctrl Pts',(189.508526546881,2.89317870140076,48.35));
#77244=CARTESIAN_POINT('Ctrl Pts',(189.508526546881,3.03574362397194,48.5));
#77245=CARTESIAN_POINT('Ctrl Pts',(189.508526546881,3.03574362397194,48.35));
#77246=CARTESIAN_POINT('',(189.408731384203,2.79488408565521,48.5));
#77247=CARTESIAN_POINT('Ctrl Pts',(189.408731384203,2.79488408565521,48.5));
#77248=CARTESIAN_POINT('Ctrl Pts',(189.508526546881,2.89317870140076,48.5));
#77249=CARTESIAN_POINT('Ctrl Pts',(189.508526546881,3.03574362397194,48.5));
#77250=CARTESIAN_POINT('',(189.408731384203,2.79488408565521,48.35));
#77251=CARTESIAN_POINT('',(189.408731384203,2.79488408565521,48.5));
#77252=CARTESIAN_POINT('Ctrl Pts',(189.408731384203,2.79488408565521,48.35));
#77253=CARTESIAN_POINT('Ctrl Pts',(189.508526546881,2.89317870140076,48.35));
#77254=CARTESIAN_POINT('Ctrl Pts',(189.508526546881,3.03574362397194,48.35));
#77255=CARTESIAN_POINT('Ctrl Pts',(189.152865035459,2.69658946990967,48.5));
#77256=CARTESIAN_POINT('Ctrl Pts',(189.152865035459,2.69658946990967,48.35));
#77257=CARTESIAN_POINT('Ctrl Pts',(189.308935923502,2.69658946990967,48.5));
#77258=CARTESIAN_POINT('Ctrl Pts',(189.308935923502,2.69658946990967,48.35));
#77259=CARTESIAN_POINT('Ctrl Pts',(189.408731384203,2.79488408565521,48.5));
#77260=CARTESIAN_POINT('Ctrl Pts',(189.408731384203,2.79488408565521,48.35));
#77261=CARTESIAN_POINT('',(189.152865035459,2.69658946990967,48.5));
#77262=CARTESIAN_POINT('Ctrl Pts',(189.152865035459,2.69658946990967,48.5));
#77263=CARTESIAN_POINT('Ctrl Pts',(189.308935923502,2.69658946990967,48.5));
#77264=CARTESIAN_POINT('Ctrl Pts',(189.408731384203,2.79488408565521,48.5));
#77265=CARTESIAN_POINT('',(189.152865035459,2.69658946990967,48.35));
#77266=CARTESIAN_POINT('',(189.152865035459,2.69658946990967,48.5));
#77267=CARTESIAN_POINT('Ctrl Pts',(189.152865035459,2.69658946990967,48.35));
#77268=CARTESIAN_POINT('Ctrl Pts',(189.308935923502,2.69658946990967,48.35));
#77269=CARTESIAN_POINT('Ctrl Pts',(189.408731384203,2.79488408565521,48.35));
#77270=CARTESIAN_POINT('Ctrl Pts',(188.891746325418,2.79563435912132,48.5));
#77271=CARTESIAN_POINT('Ctrl Pts',(188.891746325418,2.79563435912132,48.35));
#77272=CARTESIAN_POINT('Ctrl Pts',(188.992291910574,2.69658946990967,48.5));
#77273=CARTESIAN_POINT('Ctrl Pts',(188.992291910574,2.69658946990967,48.35));
#77274=CARTESIAN_POINT('Ctrl Pts',(189.152865035459,2.69658946990967,48.5));
#77275=CARTESIAN_POINT('Ctrl Pts',(189.152865035459,2.69658946990967,48.35));
#77276=CARTESIAN_POINT('',(188.891746325418,2.79563435912132,48.5));
#77277=CARTESIAN_POINT('Ctrl Pts',(188.891746325418,2.79563435912132,48.5));
#77278=CARTESIAN_POINT('Ctrl Pts',(188.992291910574,2.69658946990967,48.5));
#77279=CARTESIAN_POINT('Ctrl Pts',(189.152865035459,2.69658946990967,48.5));
#77280=CARTESIAN_POINT('',(188.891746325418,2.79563435912132,48.35));
#77281=CARTESIAN_POINT('',(188.891746325418,2.79563435912132,48.5));
#77282=CARTESIAN_POINT('Ctrl Pts',(188.891746325418,2.79563435912132,48.35));
#77283=CARTESIAN_POINT('Ctrl Pts',(188.992291910574,2.69658946990967,48.35));
#77284=CARTESIAN_POINT('Ctrl Pts',(189.152865035459,2.69658946990967,48.35));
#77285=CARTESIAN_POINT('Ctrl Pts',(188.791200591251,3.05075043439865,48.5));
#77286=CARTESIAN_POINT('Ctrl Pts',(188.791200591251,3.05075043439865,48.35));
#77287=CARTESIAN_POINT('Ctrl Pts',(188.791200591251,2.89467939734459,48.5));
#77288=CARTESIAN_POINT('Ctrl Pts',(188.791200591251,2.89467939734459,48.35));
#77289=CARTESIAN_POINT('Ctrl Pts',(188.891746325418,2.79563435912132,48.5));
#77290=CARTESIAN_POINT('Ctrl Pts',(188.891746325418,2.79563435912132,48.35));
#77291=CARTESIAN_POINT('',(188.791200591251,3.05075043439865,48.5));
#77292=CARTESIAN_POINT('Ctrl Pts',(188.791200591251,3.05075043439865,48.5));
#77293=CARTESIAN_POINT('Ctrl Pts',(188.791200591251,2.89467939734459,48.5));
#77294=CARTESIAN_POINT('Ctrl Pts',(188.891746325418,2.79563435912132,48.5));
#77295=CARTESIAN_POINT('',(188.791200591251,3.05075043439865,48.35));
#77296=CARTESIAN_POINT('',(188.791200591251,3.05075043439865,48.5));
#77297=CARTESIAN_POINT('Ctrl Pts',(188.791200591251,3.05075043439865,48.35));
#77298=CARTESIAN_POINT('Ctrl Pts',(188.791200591251,2.89467939734459,48.35));
#77299=CARTESIAN_POINT('Ctrl Pts',(188.891746325418,2.79563435912132,48.35));
#77300=CARTESIAN_POINT('Ctrl Pts',(188.893246872351,3.28785815834999,48.5));
#77301=CARTESIAN_POINT('Ctrl Pts',(188.893246872351,3.28785815834999,48.35));
#77302=CARTESIAN_POINT('Ctrl Pts',(188.791200591251,3.18881312012672,48.5));
#77303=CARTESIAN_POINT('Ctrl Pts',(188.791200591251,3.18881312012672,48.35));
#77304=CARTESIAN_POINT('Ctrl Pts',(188.791200591251,3.05075043439865,48.5));
#77305=CARTESIAN_POINT('Ctrl Pts',(188.791200591251,3.05075043439865,48.35));
#77306=CARTESIAN_POINT('Ctrl Pts',(188.893246872351,3.28785815834999,48.5));
#77307=CARTESIAN_POINT('Ctrl Pts',(188.791200591251,3.18881312012672,48.5));
#77308=CARTESIAN_POINT('Ctrl Pts',(188.791200591251,3.05075043439865,48.5));
#77309=CARTESIAN_POINT('Ctrl Pts',(188.893246872351,3.28785815834999,48.35));
#77310=CARTESIAN_POINT('Ctrl Pts',(188.791200591251,3.18881312012672,48.35));
#77311=CARTESIAN_POINT('Ctrl Pts',(188.791200591251,3.05075043439865,48.35));
#77312=CARTESIAN_POINT('Ctrl Pts',(189.14536155574,2.47598910331726,48.5));
#77313=CARTESIAN_POINT('Ctrl Pts',(189.14536155574,2.47598910331726,48.35));
#77314=CARTESIAN_POINT('Ctrl Pts',(188.954774959013,2.47598910331726,48.5));
#77315=CARTESIAN_POINT('Ctrl Pts',(188.954774959013,2.47598910331726,48.35));
#77316=CARTESIAN_POINT('Ctrl Pts',(188.82946796529,2.34993183612823,48.5));
#77317=CARTESIAN_POINT('Ctrl Pts',(188.82946796529,2.34993183612823,48.35));
#77318=CARTESIAN_POINT('',(189.14536155574,2.47598910331726,48.5));
#77319=CARTESIAN_POINT('',(188.82946796529,2.34993183612823,48.5));
#77320=CARTESIAN_POINT('Ctrl Pts',(189.14536155574,2.47598910331726,48.5));
#77321=CARTESIAN_POINT('Ctrl Pts',(188.954774959013,2.47598910331726,48.5));
#77322=CARTESIAN_POINT('Ctrl Pts',(188.82946796529,2.34993183612823,48.5));
#77323=CARTESIAN_POINT('',(189.14536155574,2.47598910331726,48.35));
#77324=CARTESIAN_POINT('',(189.14536155574,2.47598910331726,48.5));
#77325=CARTESIAN_POINT('',(188.82946796529,2.34993183612823,48.35));
#77326=CARTESIAN_POINT('Ctrl Pts',(189.14536155574,2.47598910331726,48.35));
#77327=CARTESIAN_POINT('Ctrl Pts',(188.954774959013,2.47598910331726,48.35));
#77328=CARTESIAN_POINT('Ctrl Pts',(188.82946796529,2.34993183612823,48.35));
#77329=CARTESIAN_POINT('',(188.82946796529,2.34993183612823,48.5));
#77330=CARTESIAN_POINT('Ctrl Pts',(189.470259172842,2.34843128919601,48.5));
#77331=CARTESIAN_POINT('Ctrl Pts',(189.470259172842,2.34843128919601,48.35));
#77332=CARTESIAN_POINT('Ctrl Pts',(189.340450240299,2.47598910331726,48.5));
#77333=CARTESIAN_POINT('Ctrl Pts',(189.340450240299,2.47598910331726,48.35));
#77334=CARTESIAN_POINT('Ctrl Pts',(189.14536155574,2.47598910331726,48.5));
#77335=CARTESIAN_POINT('Ctrl Pts',(189.14536155574,2.47598910331726,48.35));
#77336=CARTESIAN_POINT('',(189.470259172842,2.34843128919601,48.5));
#77337=CARTESIAN_POINT('Ctrl Pts',(189.470259172842,2.34843128919601,48.5));
#77338=CARTESIAN_POINT('Ctrl Pts',(189.340450240299,2.47598910331726,48.5));
#77339=CARTESIAN_POINT('Ctrl Pts',(189.14536155574,2.47598910331726,48.5));
#77340=CARTESIAN_POINT('',(189.470259172842,2.34843128919601,48.35));
#77341=CARTESIAN_POINT('',(189.470259172842,2.34843128919601,48.5));
#77342=CARTESIAN_POINT('Ctrl Pts',(189.470259172842,2.34843128919601,48.35));
#77343=CARTESIAN_POINT('Ctrl Pts',(189.340450240299,2.47598910331726,48.35));
#77344=CARTESIAN_POINT('Ctrl Pts',(189.14536155574,2.47598910331726,48.35));
#77345=CARTESIAN_POINT('Ctrl Pts',(189.600068254396,2.02578449249268,48.5));
#77346=CARTESIAN_POINT('Ctrl Pts',(189.600068254396,2.02578449249268,48.35));
#77347=CARTESIAN_POINT('Ctrl Pts',(189.600068254396,2.22087317705154,48.5));
#77348=CARTESIAN_POINT('Ctrl Pts',(189.600068254396,2.22087317705154,48.35));
#77349=CARTESIAN_POINT('Ctrl Pts',(189.470259172842,2.34843128919601,48.5));
#77350=CARTESIAN_POINT('Ctrl Pts',(189.470259172842,2.34843128919601,48.35));
#77351=CARTESIAN_POINT('',(189.600068254396,2.02578449249268,48.5));
#77352=CARTESIAN_POINT('Ctrl Pts',(189.600068254396,2.02578449249268,48.5));
#77353=CARTESIAN_POINT('Ctrl Pts',(189.600068254396,2.22087317705154,48.5));
#77354=CARTESIAN_POINT('Ctrl Pts',(189.470259172842,2.34843128919601,48.5));
#77355=CARTESIAN_POINT('',(189.600068254396,2.02578449249268,48.35));
#77356=CARTESIAN_POINT('',(189.600068254396,2.02578449249268,48.5));
#77357=CARTESIAN_POINT('Ctrl Pts',(189.600068254396,2.02578449249268,48.35));
#77358=CARTESIAN_POINT('Ctrl Pts',(189.600068254396,2.22087317705154,48.35));
#77359=CARTESIAN_POINT('Ctrl Pts',(189.470259172842,2.34843128919601,48.35));
#77360=CARTESIAN_POINT('Ctrl Pts',(189.474010987207,1.70914047956467,48.5));
#77361=CARTESIAN_POINT('Ctrl Pts',(189.474010987207,1.70914047956467,48.35));
#77362=CARTESIAN_POINT('Ctrl Pts',(189.600068254396,1.83369719982147,48.5));
#77363=CARTESIAN_POINT('Ctrl Pts',(189.600068254396,1.83369719982147,48.35));
#77364=CARTESIAN_POINT('Ctrl Pts',(189.600068254396,2.02578449249268,48.5));
#77365=CARTESIAN_POINT('Ctrl Pts',(189.600068254396,2.02578449249268,48.35));
#77366=CARTESIAN_POINT('',(189.474010987207,1.70914047956467,48.5));
#77367=CARTESIAN_POINT('Ctrl Pts',(189.474010987207,1.70914047956467,48.5));
#77368=CARTESIAN_POINT('Ctrl Pts',(189.600068254396,1.83369719982147,48.5));
#77369=CARTESIAN_POINT('Ctrl Pts',(189.600068254396,2.02578449249268,48.5));
#77370=CARTESIAN_POINT('',(189.474010987207,1.70914047956467,48.35));
#77371=CARTESIAN_POINT('',(189.474010987207,1.70914047956467,48.5));
#77372=CARTESIAN_POINT('Ctrl Pts',(189.474010987207,1.70914047956467,48.35));
#77373=CARTESIAN_POINT('Ctrl Pts',(189.600068254396,1.83369719982147,48.35));
#77374=CARTESIAN_POINT('Ctrl Pts',(189.600068254396,2.02578449249268,48.35));
#77375=CARTESIAN_POINT('Ctrl Pts',(189.154365582392,1.58458405733109,48.5));
#77376=CARTESIAN_POINT('Ctrl Pts',(189.154365582392,1.58458405733109,48.35));
#77377=CARTESIAN_POINT('Ctrl Pts',(189.347953720018,1.58458405733109,48.5));
#77378=CARTESIAN_POINT('Ctrl Pts',(189.347953720018,1.58458405733109,48.35));
#77379=CARTESIAN_POINT('Ctrl Pts',(189.474010987207,1.70914047956467,48.5));
#77380=CARTESIAN_POINT('Ctrl Pts',(189.474010987207,1.70914047956467,48.35));
#77381=CARTESIAN_POINT('',(189.154365582392,1.58458405733109,48.5));
#77382=CARTESIAN_POINT('Ctrl Pts',(189.154365582392,1.58458405733109,48.5));
#77383=CARTESIAN_POINT('Ctrl Pts',(189.347953720018,1.58458405733109,48.5));
#77384=CARTESIAN_POINT('Ctrl Pts',(189.474010987207,1.70914047956467,48.5));
#77385=CARTESIAN_POINT('',(189.154365582392,1.58458405733109,48.35));
#77386=CARTESIAN_POINT('',(189.154365582392,1.58458405733109,48.5));
#77387=CARTESIAN_POINT('Ctrl Pts',(189.154365582392,1.58458405733109,48.35));
#77388=CARTESIAN_POINT('Ctrl Pts',(189.347953720018,1.58458405733109,48.35));
#77389=CARTESIAN_POINT('Ctrl Pts',(189.474010987207,1.70914047956467,48.35));
#77390=CARTESIAN_POINT('Ctrl Pts',(188.921759946272,1.64386087656021,48.5));
#77391=CARTESIAN_POINT('Ctrl Pts',(188.921759946272,1.64386087656021,48.35));
#77392=CARTESIAN_POINT('Ctrl Pts',(189.029809011146,1.58458405733109,48.5));
#77393=CARTESIAN_POINT('Ctrl Pts',(189.029809011146,1.58458405733109,48.35));
#77394=CARTESIAN_POINT('Ctrl Pts',(189.154365582392,1.58458405733109,48.5));
#77395=CARTESIAN_POINT('Ctrl Pts',(189.154365582392,1.58458405733109,48.35));
#77396=CARTESIAN_POINT('',(188.921759946272,1.64386087656021,48.5));
#77397=CARTESIAN_POINT('Ctrl Pts',(188.921759946272,1.64386087656021,48.5));
#77398=CARTESIAN_POINT('Ctrl Pts',(189.029809011146,1.58458405733109,48.5));
#77399=CARTESIAN_POINT('Ctrl Pts',(189.154365582392,1.58458405733109,48.5));
#77400=CARTESIAN_POINT('',(188.921759946272,1.64386087656021,48.35));
#77401=CARTESIAN_POINT('',(188.921759946272,1.64386087656021,48.5));
#77402=CARTESIAN_POINT('Ctrl Pts',(188.921759946272,1.64386087656021,48.35));
#77403=CARTESIAN_POINT('Ctrl Pts',(189.029809011146,1.58458405733109,48.35));
#77404=CARTESIAN_POINT('Ctrl Pts',(189.154365582392,1.58458405733109,48.35));
#77405=CARTESIAN_POINT('Ctrl Pts',(188.758935851976,1.8111869096756,48.5));
#77406=CARTESIAN_POINT('Ctrl Pts',(188.758935851976,1.8111869096756,48.35));
#77407=CARTESIAN_POINT('Ctrl Pts',(188.813710732386,1.70313799381256,48.5));
#77408=CARTESIAN_POINT('Ctrl Pts',(188.813710732386,1.70313799381256,48.35));
#77409=CARTESIAN_POINT('Ctrl Pts',(188.921759946272,1.64386087656021,48.5));
#77410=CARTESIAN_POINT('Ctrl Pts',(188.921759946272,1.64386087656021,48.35));
#77411=CARTESIAN_POINT('',(188.758935851976,1.8111869096756,48.5));
#77412=CARTESIAN_POINT('Ctrl Pts',(188.758935851976,1.8111869096756,48.5));
#77413=CARTESIAN_POINT('Ctrl Pts',(188.813710732386,1.70313799381256,48.5));
#77414=CARTESIAN_POINT('Ctrl Pts',(188.921759946272,1.64386087656021,48.5));
#77415=CARTESIAN_POINT('',(188.758935851976,1.8111869096756,48.35));
#77416=CARTESIAN_POINT('',(188.758935851976,1.8111869096756,48.5));
#77417=CARTESIAN_POINT('Ctrl Pts',(188.758935851976,1.8111869096756,48.35));
#77418=CARTESIAN_POINT('Ctrl Pts',(188.813710732386,1.70313799381256,48.35));
#77419=CARTESIAN_POINT('Ctrl Pts',(188.921759946272,1.64386087656021,48.35));
#77420=CARTESIAN_POINT('Ctrl Pts',(188.704160971567,2.03478866815567,48.5));
#77421=CARTESIAN_POINT('Ctrl Pts',(188.704160971567,2.03478866815567,48.35));
#77422=CARTESIAN_POINT('Ctrl Pts',(188.704160971567,1.91923612356186,48.5));
#77423=CARTESIAN_POINT('Ctrl Pts',(188.704160971567,1.91923612356186,48.35));
#77424=CARTESIAN_POINT('Ctrl Pts',(188.758935851976,1.8111869096756,48.5));
#77425=CARTESIAN_POINT('Ctrl Pts',(188.758935851976,1.8111869096756,48.35));
#77426=CARTESIAN_POINT('',(188.704160971567,2.03478866815567,48.5));
#77427=CARTESIAN_POINT('Ctrl Pts',(188.704160971567,2.03478866815567,48.5));
#77428=CARTESIAN_POINT('Ctrl Pts',(188.704160971567,1.91923612356186,48.5));
#77429=CARTESIAN_POINT('Ctrl Pts',(188.758935851976,1.8111869096756,48.5));
#77430=CARTESIAN_POINT('',(188.704160971567,2.03478866815567,48.35));
#77431=CARTESIAN_POINT('',(188.704160971567,2.03478866815567,48.5));
#77432=CARTESIAN_POINT('Ctrl Pts',(188.704160971567,2.03478866815567,48.35));
#77433=CARTESIAN_POINT('Ctrl Pts',(188.704160971567,1.91923612356186,48.35));
#77434=CARTESIAN_POINT('Ctrl Pts',(188.758935851976,1.8111869096756,48.35));
#77435=CARTESIAN_POINT('Ctrl Pts',(188.82946796529,2.34993183612823,48.5));
#77436=CARTESIAN_POINT('Ctrl Pts',(188.82946796529,2.34993183612823,48.35));
#77437=CARTESIAN_POINT('Ctrl Pts',(188.704160971567,2.22387456893921,48.5));
#77438=CARTESIAN_POINT('Ctrl Pts',(188.704160971567,2.22387456893921,48.35));
#77439=CARTESIAN_POINT('Ctrl Pts',(188.704160971567,2.03478866815567,48.5));
#77440=CARTESIAN_POINT('Ctrl Pts',(188.704160971567,2.03478866815567,48.35));
#77441=CARTESIAN_POINT('Ctrl Pts',(188.82946796529,2.34993183612823,48.5));
#77442=CARTESIAN_POINT('Ctrl Pts',(188.704160971567,2.22387456893921,48.5));
#77443=CARTESIAN_POINT('Ctrl Pts',(188.704160971567,2.03478866815567,48.5));
#77444=CARTESIAN_POINT('Ctrl Pts',(188.82946796529,2.34993183612823,48.35));
#77445=CARTESIAN_POINT('Ctrl Pts',(188.704160971567,2.22387456893921,48.35));
#77446=CARTESIAN_POINT('Ctrl Pts',(188.704160971567,2.03478866815567,48.35));
#77447=CARTESIAN_POINT('Ctrl Pts',(188.426534755155,2.03628921508789,48.5));
#77448=CARTESIAN_POINT('Ctrl Pts',(188.426534755155,2.03628921508789,48.35));
#77449=CARTESIAN_POINT('Ctrl Pts',(188.426534755155,2.25088679790497,48.5));
#77450=CARTESIAN_POINT('Ctrl Pts',(188.426534755155,2.25088679790497,48.35));
#77451=CARTESIAN_POINT('Ctrl Pts',(188.535334242508,2.39570268988609,48.5));
#77452=CARTESIAN_POINT('Ctrl Pts',(188.535334242508,2.39570268988609,48.35));
#77453=CARTESIAN_POINT('',(188.426534755155,2.03628921508789,48.5));
#77454=CARTESIAN_POINT('',(188.535334242508,2.39570268988609,48.5));
#77455=CARTESIAN_POINT('Ctrl Pts',(188.426534755155,2.03628921508789,48.5));
#77456=CARTESIAN_POINT('Ctrl Pts',(188.426534755155,2.25088679790497,48.5));
#77457=CARTESIAN_POINT('Ctrl Pts',(188.535334242508,2.39570268988609,48.5));
#77458=CARTESIAN_POINT('',(188.426534755155,2.03628921508789,48.35));
#77459=CARTESIAN_POINT('',(188.426534755155,2.03628921508789,48.5));
#77460=CARTESIAN_POINT('',(188.535334242508,2.39570268988609,48.35));
#77461=CARTESIAN_POINT('Ctrl Pts',(188.426534755155,2.03628921508789,48.35));
#77462=CARTESIAN_POINT('Ctrl Pts',(188.426534755155,2.25088679790497,48.35));
#77463=CARTESIAN_POINT('Ctrl Pts',(188.535334242508,2.39570268988609,48.35));
#77464=CARTESIAN_POINT('',(188.535334242508,2.39570268988609,48.5));
#77465=CARTESIAN_POINT('Ctrl Pts',(188.626125527546,1.55532056093216,48.5));
#77466=CARTESIAN_POINT('Ctrl Pts',(188.626125527546,1.55532056093216,48.35));
#77467=CARTESIAN_POINT('Ctrl Pts',(188.426534755155,1.74815827608109,48.5));
#77468=CARTESIAN_POINT('Ctrl Pts',(188.426534755155,1.74815827608109,48.35));
#77469=CARTESIAN_POINT('Ctrl Pts',(188.426534755155,2.03628921508789,48.5));
#77470=CARTESIAN_POINT('Ctrl Pts',(188.426534755155,2.03628921508789,48.35));
#77471=CARTESIAN_POINT('',(188.626125527546,1.55532056093216,48.5));
#77472=CARTESIAN_POINT('Ctrl Pts',(188.626125527546,1.55532056093216,48.5));
#77473=CARTESIAN_POINT('Ctrl Pts',(188.426534755155,1.74815827608109,48.5));
#77474=CARTESIAN_POINT('Ctrl Pts',(188.426534755155,2.03628921508789,48.5));
#77475=CARTESIAN_POINT('',(188.626125527546,1.55532056093216,48.35));
#77476=CARTESIAN_POINT('',(188.626125527546,1.55532056093216,48.5));
#77477=CARTESIAN_POINT('Ctrl Pts',(188.626125527546,1.55532056093216,48.35));
#77478=CARTESIAN_POINT('Ctrl Pts',(188.426534755155,1.74815827608109,48.35));
#77479=CARTESIAN_POINT('Ctrl Pts',(188.426534755155,2.03628921508789,48.35));
#77480=CARTESIAN_POINT('Ctrl Pts',(189.151364190504,1.36248314380646,48.5));
#77481=CARTESIAN_POINT('Ctrl Pts',(189.151364190504,1.36248314380646,48.35));
#77482=CARTESIAN_POINT('Ctrl Pts',(188.825716299936,1.36248314380646,48.5));
#77483=CARTESIAN_POINT('Ctrl Pts',(188.825716299936,1.36248314380646,48.35));
#77484=CARTESIAN_POINT('Ctrl Pts',(188.626125527546,1.55532056093216,48.5));
#77485=CARTESIAN_POINT('Ctrl Pts',(188.626125527546,1.55532056093216,48.35));
#77486=CARTESIAN_POINT('',(189.151364190504,1.36248314380646,48.5));
#77487=CARTESIAN_POINT('Ctrl Pts',(189.151364190504,1.36248314380646,48.5));
#77488=CARTESIAN_POINT('Ctrl Pts',(188.825716299936,1.36248314380646,48.5));
#77489=CARTESIAN_POINT('Ctrl Pts',(188.626125527546,1.55532056093216,48.5));
#77490=CARTESIAN_POINT('',(189.151364190504,1.36248314380646,48.35));
#77491=CARTESIAN_POINT('',(189.151364190504,1.36248314380646,48.5));
#77492=CARTESIAN_POINT('Ctrl Pts',(189.151364190504,1.36248314380646,48.35));
#77493=CARTESIAN_POINT('Ctrl Pts',(188.825716299936,1.36248314380646,48.35));
#77494=CARTESIAN_POINT('Ctrl Pts',(188.626125527546,1.55532056093216,48.35));
#77495=CARTESIAN_POINT('Ctrl Pts',(189.676603002474,1.55457043647766,48.5));
#77496=CARTESIAN_POINT('Ctrl Pts',(189.676603002474,1.55457043647766,48.35));
#77497=CARTESIAN_POINT('Ctrl Pts',(189.477012379095,1.36248314380646,48.5));
#77498=CARTESIAN_POINT('Ctrl Pts',(189.477012379095,1.36248314380646,48.35));
#77499=CARTESIAN_POINT('Ctrl Pts',(189.151364190504,1.36248314380646,48.5));
#77500=CARTESIAN_POINT('Ctrl Pts',(189.151364190504,1.36248314380646,48.35));
#77501=CARTESIAN_POINT('',(189.676603002474,1.55457043647766,48.5));
#77502=CARTESIAN_POINT('Ctrl Pts',(189.676603002474,1.55457043647766,48.5));
#77503=CARTESIAN_POINT('Ctrl Pts',(189.477012379095,1.36248314380646,48.5));
#77504=CARTESIAN_POINT('Ctrl Pts',(189.151364190504,1.36248314380646,48.5));
#77505=CARTESIAN_POINT('',(189.676603002474,1.55457043647766,48.35));
#77506=CARTESIAN_POINT('',(189.676603002474,1.55457043647766,48.5));
#77507=CARTESIAN_POINT('Ctrl Pts',(189.676603002474,1.55457043647766,48.35));
#77508=CARTESIAN_POINT('Ctrl Pts',(189.477012379095,1.36248314380646,48.35));
#77509=CARTESIAN_POINT('Ctrl Pts',(189.151364190504,1.36248314380646,48.35));
#77510=CARTESIAN_POINT('Ctrl Pts',(189.876193625852,2.02878588438034,48.5));
#77511=CARTESIAN_POINT('Ctrl Pts',(189.876193625852,2.02878588438034,48.35));
#77512=CARTESIAN_POINT('Ctrl Pts',(189.876193625852,1.74665772914886,48.5));
#77513=CARTESIAN_POINT('Ctrl Pts',(189.876193625852,1.74665772914886,48.35));
#77514=CARTESIAN_POINT('Ctrl Pts',(189.676603002474,1.55457043647766,48.5));
#77515=CARTESIAN_POINT('Ctrl Pts',(189.676603002474,1.55457043647766,48.35));
#77516=CARTESIAN_POINT('',(189.876193625852,2.02878588438034,48.5));
#77517=CARTESIAN_POINT('Ctrl Pts',(189.876193625852,2.02878588438034,48.5));
#77518=CARTESIAN_POINT('Ctrl Pts',(189.876193625852,1.74665772914886,48.5));
#77519=CARTESIAN_POINT('Ctrl Pts',(189.676603002474,1.55457043647766,48.5));
#77520=CARTESIAN_POINT('',(189.876193625852,2.02878588438034,48.35));
#77521=CARTESIAN_POINT('',(189.876193625852,2.02878588438034,48.5));
#77522=CARTESIAN_POINT('Ctrl Pts',(189.876193625852,2.02878588438034,48.35));
#77523=CARTESIAN_POINT('Ctrl Pts',(189.876193625852,1.74665772914886,48.35));
#77524=CARTESIAN_POINT('Ctrl Pts',(189.676603002474,1.55457043647766,48.35));
#77525=CARTESIAN_POINT('Ctrl Pts',(189.770395679399,2.37994545698166,48.5));
#77526=CARTESIAN_POINT('Ctrl Pts',(189.770395679399,2.37994545698166,48.35));
#77527=CARTESIAN_POINT('Ctrl Pts',(189.876193625852,2.2328787446022,48.5));
#77528=CARTESIAN_POINT('Ctrl Pts',(189.876193625852,2.2328787446022,48.35));
#77529=CARTESIAN_POINT('Ctrl Pts',(189.876193625852,2.02878588438034,48.5));
#77530=CARTESIAN_POINT('Ctrl Pts',(189.876193625852,2.02878588438034,48.35));
#77531=CARTESIAN_POINT('',(189.770395679399,2.37994545698166,48.5));
#77532=CARTESIAN_POINT('Ctrl Pts',(189.770395679399,2.37994545698166,48.5));
#77533=CARTESIAN_POINT('Ctrl Pts',(189.876193625852,2.2328787446022,48.5));
#77534=CARTESIAN_POINT('Ctrl Pts',(189.876193625852,2.02878588438034,48.5));
#77535=CARTESIAN_POINT('',(189.770395679399,2.37994545698166,48.35));
#77536=CARTESIAN_POINT('',(189.770395679399,2.37994545698166,48.5));
#77537=CARTESIAN_POINT('Ctrl Pts',(189.770395679399,2.37994545698166,48.35));
#77538=CARTESIAN_POINT('Ctrl Pts',(189.876193625852,2.2328787446022,48.35));
#77539=CARTESIAN_POINT('Ctrl Pts',(189.876193625852,2.02878588438034,48.35));
#77540=CARTESIAN_POINT('Ctrl Pts',(189.462005419657,2.59304249286652,48.5));
#77541=CARTESIAN_POINT('Ctrl Pts',(189.462005419657,2.59304249286652,48.35));
#77542=CARTESIAN_POINT('Ctrl Pts',(189.664597434923,2.52701246738434,48.5));
#77543=CARTESIAN_POINT('Ctrl Pts',(189.664597434923,2.52701246738434,48.35));
#77544=CARTESIAN_POINT('Ctrl Pts',(189.770395679399,2.37994545698166,48.5));
#77545=CARTESIAN_POINT('Ctrl Pts',(189.770395679399,2.37994545698166,48.35));
#77546=CARTESIAN_POINT('',(189.462005419657,2.59304249286652,48.5));
#77547=CARTESIAN_POINT('Ctrl Pts',(189.462005419657,2.59304249286652,48.5));
#77548=CARTESIAN_POINT('Ctrl Pts',(189.664597434923,2.52701246738434,48.5));
#77549=CARTESIAN_POINT('Ctrl Pts',(189.770395679399,2.37994545698166,48.5));
#77550=CARTESIAN_POINT('',(189.462005419657,2.59304249286652,48.35));
#77551=CARTESIAN_POINT('',(189.462005419657,2.59304249286652,48.5));
#77552=CARTESIAN_POINT('Ctrl Pts',(189.462005419657,2.59304249286652,48.35));
#77553=CARTESIAN_POINT('Ctrl Pts',(189.664597434923,2.52701246738434,48.35));
#77554=CARTESIAN_POINT('Ctrl Pts',(189.770395679399,2.37994545698166,48.35));
#77555=CARTESIAN_POINT('Ctrl Pts',(189.705866200849,2.76787185668945,48.5));
#77556=CARTESIAN_POINT('Ctrl Pts',(189.705866200849,2.76787185668945,48.35));
#77557=CARTESIAN_POINT('Ctrl Pts',(189.625579638407,2.65457028150558,48.5));
#77558=CARTESIAN_POINT('Ctrl Pts',(189.625579638407,2.65457028150558,48.35));
#77559=CARTESIAN_POINT('Ctrl Pts',(189.462005419657,2.59304249286652,48.5));
#77560=CARTESIAN_POINT('Ctrl Pts',(189.462005419657,2.59304249286652,48.35));
#77561=CARTESIAN_POINT('',(189.705866200849,2.76787185668945,48.5));
#77562=CARTESIAN_POINT('Ctrl Pts',(189.705866200849,2.76787185668945,48.5));
#77563=CARTESIAN_POINT('Ctrl Pts',(189.625579638407,2.65457028150558,48.5));
#77564=CARTESIAN_POINT('Ctrl Pts',(189.462005419657,2.59304249286652,48.5));
#77565=CARTESIAN_POINT('',(189.705866200849,2.76787185668945,48.35));
#77566=CARTESIAN_POINT('',(189.705866200849,2.76787185668945,48.5));
#77567=CARTESIAN_POINT('Ctrl Pts',(189.705866200849,2.76787185668945,48.35));
#77568=CARTESIAN_POINT('Ctrl Pts',(189.625579638407,2.65457028150558,48.35));
#77569=CARTESIAN_POINT('Ctrl Pts',(189.462005419657,2.59304249286652,48.35));
#77570=CARTESIAN_POINT('Ctrl Pts',(189.786152763292,3.03424292802811,48.5));
#77571=CARTESIAN_POINT('Ctrl Pts',(189.786152763292,3.03424292802811,48.35));
#77572=CARTESIAN_POINT('Ctrl Pts',(189.786152763292,2.88117328286171,48.5));
#77573=CARTESIAN_POINT('Ctrl Pts',(189.786152763292,2.88117328286171,48.35));
#77574=CARTESIAN_POINT('Ctrl Pts',(189.705866200849,2.76787185668945,48.5));
#77575=CARTESIAN_POINT('Ctrl Pts',(189.705866200849,2.76787185668945,48.35));
#77576=CARTESIAN_POINT('',(189.786152763292,3.03424292802811,48.5));
#77577=CARTESIAN_POINT('Ctrl Pts',(189.786152763292,3.03424292802811,48.5));
#77578=CARTESIAN_POINT('Ctrl Pts',(189.786152763292,2.88117328286171,48.5));
#77579=CARTESIAN_POINT('Ctrl Pts',(189.705866200849,2.76787185668945,48.5));
#77580=CARTESIAN_POINT('',(189.786152763292,3.03424292802811,48.35));
#77581=CARTESIAN_POINT('',(189.786152763292,3.03424292802811,48.5));
#77582=CARTESIAN_POINT('Ctrl Pts',(189.786152763292,3.03424292802811,48.35));
#77583=CARTESIAN_POINT('Ctrl Pts',(189.786152763292,2.88117328286171,48.35));
#77584=CARTESIAN_POINT('Ctrl Pts',(189.705866200849,2.76787185668945,48.35));
#77585=CARTESIAN_POINT('Ctrl Pts',(189.610572976992,3.4416780769825,48.5));
#77586=CARTESIAN_POINT('Ctrl Pts',(189.610572976992,3.4416780769825,48.35));
#77587=CARTESIAN_POINT('Ctrl Pts',(189.786152763292,3.27435204386711,48.5));
#77588=CARTESIAN_POINT('Ctrl Pts',(189.786152763292,3.27435204386711,48.35));
#77589=CARTESIAN_POINT('Ctrl Pts',(189.786152763292,3.03424292802811,48.5));
#77590=CARTESIAN_POINT('Ctrl Pts',(189.786152763292,3.03424292802811,48.35));
#77591=CARTESIAN_POINT('',(189.610572976992,3.4416780769825,48.5));
#77592=CARTESIAN_POINT('Ctrl Pts',(189.610572976992,3.4416780769825,48.5));
#77593=CARTESIAN_POINT('Ctrl Pts',(189.786152763292,3.27435204386711,48.5));
#77594=CARTESIAN_POINT('Ctrl Pts',(189.786152763292,3.03424292802811,48.5));
#77595=CARTESIAN_POINT('',(189.610572976992,3.4416780769825,48.35));
#77596=CARTESIAN_POINT('',(189.610572976992,3.4416780769825,48.5));
#77597=CARTESIAN_POINT('Ctrl Pts',(189.610572976992,3.4416780769825,48.35));
#77598=CARTESIAN_POINT('Ctrl Pts',(189.786152763292,3.27435204386711,48.35));
#77599=CARTESIAN_POINT('Ctrl Pts',(189.786152763292,3.03424292802811,48.35));
#77600=CARTESIAN_POINT('Ctrl Pts',(189.146862251684,3.60900411009789,48.5));
#77601=CARTESIAN_POINT('Ctrl Pts',(189.146862251684,3.60900411009789,48.35));
#77602=CARTESIAN_POINT('Ctrl Pts',(189.434993190691,3.60900411009789,48.5));
#77603=CARTESIAN_POINT('Ctrl Pts',(189.434993190691,3.60900411009789,48.35));
#77604=CARTESIAN_POINT('Ctrl Pts',(189.610572976992,3.4416780769825,48.5));
#77605=CARTESIAN_POINT('Ctrl Pts',(189.610572976992,3.4416780769825,48.35));
#77606=CARTESIAN_POINT('',(189.146862251684,3.60900411009789,48.5));
#77607=CARTESIAN_POINT('Ctrl Pts',(189.146862251684,3.60900411009789,48.5));
#77608=CARTESIAN_POINT('Ctrl Pts',(189.434993190691,3.60900411009789,48.5));
#77609=CARTESIAN_POINT('Ctrl Pts',(189.610572976992,3.4416780769825,48.5));
#77610=CARTESIAN_POINT('',(189.146862251684,3.60900411009789,48.35));
#77611=CARTESIAN_POINT('',(189.146862251684,3.60900411009789,48.5));
#77612=CARTESIAN_POINT('Ctrl Pts',(189.146862251684,3.60900411009789,48.35));
#77613=CARTESIAN_POINT('Ctrl Pts',(189.434993190691,3.60900411009789,48.35));
#77614=CARTESIAN_POINT('Ctrl Pts',(189.610572976992,3.4416780769825,48.35));
#77615=CARTESIAN_POINT('Ctrl Pts',(188.687653465196,3.44542974233627,48.5));
#77616=CARTESIAN_POINT('Ctrl Pts',(188.687653465196,3.44542974233627,48.35));
#77617=CARTESIAN_POINT('Ctrl Pts',(188.860231859609,3.60900411009789,48.5));
#77618=CARTESIAN_POINT('Ctrl Pts',(188.860231859609,3.60900411009789,48.35));
#77619=CARTESIAN_POINT('Ctrl Pts',(189.146862251684,3.60900411009789,48.5));
#77620=CARTESIAN_POINT('Ctrl Pts',(189.146862251684,3.60900411009789,48.35));
#77621=CARTESIAN_POINT('',(188.687653465196,3.44542974233627,48.5));
#77622=CARTESIAN_POINT('Ctrl Pts',(188.687653465196,3.44542974233627,48.5));
#77623=CARTESIAN_POINT('Ctrl Pts',(188.860231859609,3.60900411009789,48.5));
#77624=CARTESIAN_POINT('Ctrl Pts',(189.146862251684,3.60900411009789,48.5));
#77625=CARTESIAN_POINT('',(188.687653465196,3.44542974233627,48.35));
#77626=CARTESIAN_POINT('',(188.687653465196,3.44542974233627,48.5));
#77627=CARTESIAN_POINT('Ctrl Pts',(188.687653465196,3.44542974233627,48.35));
#77628=CARTESIAN_POINT('Ctrl Pts',(188.860231859609,3.60900411009789,48.35));
#77629=CARTESIAN_POINT('Ctrl Pts',(189.146862251684,3.60900411009789,48.35));
#77630=CARTESIAN_POINT('Ctrl Pts',(188.515075070783,3.04174625873566,48.5));
#77631=CARTESIAN_POINT('Ctrl Pts',(188.515075070783,3.04174625873566,48.35));
#77632=CARTESIAN_POINT('Ctrl Pts',(188.515075070783,3.28185537457466,48.5));
#77633=CARTESIAN_POINT('Ctrl Pts',(188.515075070783,3.28185537457466,48.35));
#77634=CARTESIAN_POINT('Ctrl Pts',(188.687653465196,3.44542974233627,48.5));
#77635=CARTESIAN_POINT('Ctrl Pts',(188.687653465196,3.44542974233627,48.35));
#77636=CARTESIAN_POINT('',(188.515075070783,3.04174625873566,48.5));
#77637=CARTESIAN_POINT('Ctrl Pts',(188.515075070783,3.04174625873566,48.5));
#77638=CARTESIAN_POINT('Ctrl Pts',(188.515075070783,3.28185537457466,48.5));
#77639=CARTESIAN_POINT('Ctrl Pts',(188.687653465196,3.44542974233627,48.5));
#77640=CARTESIAN_POINT('',(188.515075070783,3.04174625873566,48.35));
#77641=CARTESIAN_POINT('',(188.515075070783,3.04174625873566,48.5));
#77642=CARTESIAN_POINT('Ctrl Pts',(188.515075070783,3.04174625873566,48.35));
#77643=CARTESIAN_POINT('Ctrl Pts',(188.515075070783,3.28185537457466,48.35));
#77644=CARTESIAN_POINT('Ctrl Pts',(188.687653465196,3.44542974233627,48.35));
#77645=CARTESIAN_POINT('Ctrl Pts',(188.596111906692,2.76862213015556,48.5));
#77646=CARTESIAN_POINT('Ctrl Pts',(188.596111906692,2.76862213015556,48.35));
#77647=CARTESIAN_POINT('Ctrl Pts',(188.515075070783,2.88267397880554,48.5));
#77648=CARTESIAN_POINT('Ctrl Pts',(188.515075070783,2.88267397880554,48.35));
#77649=CARTESIAN_POINT('Ctrl Pts',(188.515075070783,3.04174625873566,48.5));
#77650=CARTESIAN_POINT('Ctrl Pts',(188.515075070783,3.04174625873566,48.35));
#77651=CARTESIAN_POINT('',(188.596111906692,2.76862213015556,48.5));
#77652=CARTESIAN_POINT('Ctrl Pts',(188.596111906692,2.76862213015556,48.5));
#77653=CARTESIAN_POINT('Ctrl Pts',(188.515075070783,2.88267397880554,48.5));
#77654=CARTESIAN_POINT('Ctrl Pts',(188.515075070783,3.04174625873566,48.5));
#77655=CARTESIAN_POINT('',(188.596111906692,2.76862213015556,48.35));
#77656=CARTESIAN_POINT('',(188.596111906692,2.76862213015556,48.5));
#77657=CARTESIAN_POINT('Ctrl Pts',(188.596111906692,2.76862213015556,48.35));
#77658=CARTESIAN_POINT('Ctrl Pts',(188.515075070783,2.88267397880554,48.35));
#77659=CARTESIAN_POINT('Ctrl Pts',(188.515075070783,3.04174625873566,48.35));
#77660=CARTESIAN_POINT('Ctrl Pts',(188.845225049183,2.59304249286652,48.5));
#77661=CARTESIAN_POINT('Ctrl Pts',(188.845225049183,2.59304249286652,48.35));
#77662=CARTESIAN_POINT('Ctrl Pts',(188.677148742601,2.65457028150558,48.5));
#77663=CARTESIAN_POINT('Ctrl Pts',(188.677148742601,2.65457028150558,48.35));
#77664=CARTESIAN_POINT('Ctrl Pts',(188.596111906692,2.76862213015556,48.5));
#77665=CARTESIAN_POINT('Ctrl Pts',(188.596111906692,2.76862213015556,48.35));
#77666=CARTESIAN_POINT('',(188.845225049183,2.59304249286652,48.5));
#77667=CARTESIAN_POINT('Ctrl Pts',(188.845225049183,2.59304249286652,48.5));
#77668=CARTESIAN_POINT('Ctrl Pts',(188.677148742601,2.65457028150558,48.5));
#77669=CARTESIAN_POINT('Ctrl Pts',(188.596111906692,2.76862213015556,48.5));
#77670=CARTESIAN_POINT('',(188.845225049183,2.59304249286652,48.35));
#77671=CARTESIAN_POINT('',(188.845225049183,2.59304249286652,48.5));
#77672=CARTESIAN_POINT('Ctrl Pts',(188.845225049183,2.59304249286652,48.35));
#77673=CARTESIAN_POINT('Ctrl Pts',(188.677148742601,2.65457028150558,48.35));
#77674=CARTESIAN_POINT('Ctrl Pts',(188.596111906692,2.76862213015556,48.35));
#77675=CARTESIAN_POINT('Ctrl Pts',(188.535334242508,2.39570268988609,48.5));
#77676=CARTESIAN_POINT('Ctrl Pts',(188.535334242508,2.39570268988609,48.35));
#77677=CARTESIAN_POINT('Ctrl Pts',(188.64413372986,2.54051858186722,48.5));
#77678=CARTESIAN_POINT('Ctrl Pts',(188.64413372986,2.54051858186722,48.35));
#77679=CARTESIAN_POINT('Ctrl Pts',(188.845225049183,2.59304249286652,48.5));
#77680=CARTESIAN_POINT('Ctrl Pts',(188.845225049183,2.59304249286652,48.35));
#77681=CARTESIAN_POINT('Ctrl Pts',(188.535334242508,2.39570268988609,48.5));
#77682=CARTESIAN_POINT('Ctrl Pts',(188.64413372986,2.54051858186722,48.5));
#77683=CARTESIAN_POINT('Ctrl Pts',(188.845225049183,2.59304249286652,48.5));
#77684=CARTESIAN_POINT('Ctrl Pts',(188.535334242508,2.39570268988609,48.35));
#77685=CARTESIAN_POINT('Ctrl Pts',(188.64413372986,2.54051858186722,48.35));
#77686=CARTESIAN_POINT('Ctrl Pts',(188.845225049183,2.59304249286652,48.35));
#77687=CARTESIAN_POINT('Origin',(189.99999977462,2.48574362695217,48.35));
#77688=CARTESIAN_POINT('Origin',(0.,8.,48.5));
#77689=CARTESIAN_POINT('Origin',(0.,8.,48.5));
#77690=CARTESIAN_POINT('Origin',(0.,8.,48.5));
#77691=CARTESIAN_POINT('Ctrl Pts',(180.842633068562,3.38540250062943,48.5));
#77692=CARTESIAN_POINT('Ctrl Pts',(180.842633068562,3.38540250062943,48.35));
#77693=CARTESIAN_POINT('Ctrl Pts',(180.656548261642,3.38540250062943,48.5));
#77694=CARTESIAN_POINT('Ctrl Pts',(180.656548261642,3.38540250062943,48.35));
#77695=CARTESIAN_POINT('Ctrl Pts',(180.545497953892,3.22783091664314,48.5));
#77696=CARTESIAN_POINT('Ctrl Pts',(180.545497953892,3.22783091664314,48.35));
#77697=CARTESIAN_POINT('',(180.842633068562,3.38540250062943,48.5));
#77698=CARTESIAN_POINT('',(180.545497953892,3.22783091664314,48.5));
#77699=CARTESIAN_POINT('Ctrl Pts',(180.842633068562,3.38540250062943,48.5));
#77700=CARTESIAN_POINT('Ctrl Pts',(180.656548261642,3.38540250062943,48.5));
#77701=CARTESIAN_POINT('Ctrl Pts',(180.545497953892,3.22783091664314,48.5));
#77702=CARTESIAN_POINT('',(180.842633068562,3.38540250062943,48.35));
#77703=CARTESIAN_POINT('',(180.842633068562,3.38540250062943,48.5));
#77704=CARTESIAN_POINT('',(180.545497953892,3.22783091664314,48.35));
#77705=CARTESIAN_POINT('Ctrl Pts',(180.842633068562,3.38540250062943,48.35));
#77706=CARTESIAN_POINT('Ctrl Pts',(180.656548261642,3.38540250062943,48.35));
#77707=CARTESIAN_POINT('Ctrl Pts',(180.545497953892,3.22783091664314,48.35));
#77708=CARTESIAN_POINT('',(180.545497953892,3.22783091664314,48.5));
#77709=CARTESIAN_POINT('Ctrl Pts',(181.158526360989,3.2068213224411,48.5));
#77710=CARTESIAN_POINT('Ctrl Pts',(181.158526360989,3.2068213224411,48.35));
#77711=CARTESIAN_POINT('Ctrl Pts',(181.031718671322,3.38540250062943,48.5));
#77712=CARTESIAN_POINT('Ctrl Pts',(181.031718671322,3.38540250062943,48.35));
#77713=CARTESIAN_POINT('Ctrl Pts',(180.842633068562,3.38540250062943,48.5));
#77714=CARTESIAN_POINT('Ctrl Pts',(180.842633068562,3.38540250062943,48.35));
#77715=CARTESIAN_POINT('',(181.158526360989,3.2068213224411,48.5));
#77716=CARTESIAN_POINT('Ctrl Pts',(181.158526360989,3.2068213224411,48.5));
#77717=CARTESIAN_POINT('Ctrl Pts',(181.031718671322,3.38540250062943,48.5));
#77718=CARTESIAN_POINT('Ctrl Pts',(180.842633068562,3.38540250062943,48.5));
#77719=CARTESIAN_POINT('',(181.158526360989,3.2068213224411,48.35));
#77720=CARTESIAN_POINT('',(181.158526360989,3.2068213224411,48.5));
#77721=CARTESIAN_POINT('Ctrl Pts',(181.158526360989,3.2068213224411,48.35));
#77722=CARTESIAN_POINT('Ctrl Pts',(181.031718671322,3.38540250062943,48.35));
#77723=CARTESIAN_POINT('Ctrl Pts',(180.842633068562,3.38540250062943,48.35));
#77724=CARTESIAN_POINT('Ctrl Pts',(181.285334050655,2.48499327898026,48.5));
#77725=CARTESIAN_POINT('Ctrl Pts',(181.285334050655,2.48499327898026,48.35));
#77726=CARTESIAN_POINT('Ctrl Pts',(181.285334050655,3.02824014425278,48.5));
#77727=CARTESIAN_POINT('Ctrl Pts',(181.285334050655,3.02824014425278,48.35));
#77728=CARTESIAN_POINT('Ctrl Pts',(181.158526360989,3.2068213224411,48.5));
#77729=CARTESIAN_POINT('Ctrl Pts',(181.158526360989,3.2068213224411,48.35));
#77730=CARTESIAN_POINT('',(181.285334050655,2.48499327898026,48.5));
#77731=CARTESIAN_POINT('Ctrl Pts',(181.285334050655,2.48499327898026,48.5));
#77732=CARTESIAN_POINT('Ctrl Pts',(181.285334050655,3.02824014425278,48.5));
#77733=CARTESIAN_POINT('Ctrl Pts',(181.158526360989,3.2068213224411,48.5));
#77734=CARTESIAN_POINT('',(181.285334050655,2.48499327898026,48.35));
#77735=CARTESIAN_POINT('',(181.285334050655,2.48499327898026,48.5));
#77736=CARTESIAN_POINT('Ctrl Pts',(181.285334050655,2.48499327898026,48.35));
#77737=CARTESIAN_POINT('Ctrl Pts',(181.285334050655,3.02824014425278,48.35));
#77738=CARTESIAN_POINT('Ctrl Pts',(181.158526360989,3.2068213224411,48.35));
#77739=CARTESIAN_POINT('Ctrl Pts',(181.158526360989,1.76466578245163,48.5));
#77740=CARTESIAN_POINT('Ctrl Pts',(181.158526360989,1.76466578245163,48.35));
#77741=CARTESIAN_POINT('Ctrl Pts',(181.285334050655,1.9447478055954,48.5));
#77742=CARTESIAN_POINT('Ctrl Pts',(181.285334050655,1.9447478055954,48.35));
#77743=CARTESIAN_POINT('Ctrl Pts',(181.285334050655,2.48499327898026,48.5));
#77744=CARTESIAN_POINT('Ctrl Pts',(181.285334050655,2.48499327898026,48.35));
#77745=CARTESIAN_POINT('',(181.158526360989,1.76466578245163,48.5));
#77746=CARTESIAN_POINT('Ctrl Pts',(181.158526360989,1.76466578245163,48.5));
#77747=CARTESIAN_POINT('Ctrl Pts',(181.285334050655,1.9447478055954,48.5));
#77748=CARTESIAN_POINT('Ctrl Pts',(181.285334050655,2.48499327898026,48.5));
#77749=CARTESIAN_POINT('',(181.158526360989,1.76466578245163,48.35));
#77750=CARTESIAN_POINT('',(181.158526360989,1.76466578245163,48.5));
#77751=CARTESIAN_POINT('Ctrl Pts',(181.158526360989,1.76466578245163,48.35));
#77752=CARTESIAN_POINT('Ctrl Pts',(181.285334050655,1.9447478055954,48.35));
#77753=CARTESIAN_POINT('Ctrl Pts',(181.285334050655,2.48499327898026,48.35));
#77754=CARTESIAN_POINT('Ctrl Pts',(180.845634162426,1.58458405733109,48.5));
#77755=CARTESIAN_POINT('Ctrl Pts',(180.845634162426,1.58458405733109,48.35));
#77756=CARTESIAN_POINT('Ctrl Pts',(181.031718671322,1.58458405733109,48.5));
#77757=CARTESIAN_POINT('Ctrl Pts',(181.031718671322,1.58458405733109,48.35));
#77758=CARTESIAN_POINT('Ctrl Pts',(181.158526360989,1.76466578245163,48.5));
#77759=CARTESIAN_POINT('Ctrl Pts',(181.158526360989,1.76466578245163,48.35));
#77760=CARTESIAN_POINT('',(180.845634162426,1.58458405733109,48.5));
#77761=CARTESIAN_POINT('Ctrl Pts',(180.845634162426,1.58458405733109,48.5));
#77762=CARTESIAN_POINT('Ctrl Pts',(181.031718671322,1.58458405733109,48.5));
#77763=CARTESIAN_POINT('Ctrl Pts',(181.158526360989,1.76466578245163,48.5));
#77764=CARTESIAN_POINT('',(180.845634162426,1.58458405733109,48.35));
#77765=CARTESIAN_POINT('',(180.845634162426,1.58458405733109,48.5));
#77766=CARTESIAN_POINT('Ctrl Pts',(180.845634162426,1.58458405733109,48.35));
#77767=CARTESIAN_POINT('Ctrl Pts',(181.031718671322,1.58458405733109,48.35));
#77768=CARTESIAN_POINT('Ctrl Pts',(181.158526360989,1.76466578245163,48.35));
#77769=CARTESIAN_POINT('Ctrl Pts',(180.532741963863,1.76391565799713,48.5));
#77770=CARTESIAN_POINT('Ctrl Pts',(180.532741963863,1.76391565799713,48.35));
#77771=CARTESIAN_POINT('Ctrl Pts',(180.65954965353,1.58458405733109,48.5));
#77772=CARTESIAN_POINT('Ctrl Pts',(180.65954965353,1.58458405733109,48.35));
#77773=CARTESIAN_POINT('Ctrl Pts',(180.845634162426,1.58458405733109,48.5));
#77774=CARTESIAN_POINT('Ctrl Pts',(180.845634162426,1.58458405733109,48.35));
#77775=CARTESIAN_POINT('',(180.532741963863,1.76391565799713,48.5));
#77776=CARTESIAN_POINT('Ctrl Pts',(180.532741963863,1.76391565799713,48.5));
#77777=CARTESIAN_POINT('Ctrl Pts',(180.65954965353,1.58458405733109,48.5));
#77778=CARTESIAN_POINT('Ctrl Pts',(180.845634162426,1.58458405733109,48.5));
#77779=CARTESIAN_POINT('',(180.532741963863,1.76391565799713,48.35));
#77780=CARTESIAN_POINT('',(180.532741963863,1.76391565799713,48.5));
#77781=CARTESIAN_POINT('Ctrl Pts',(180.532741963863,1.76391565799713,48.35));
#77782=CARTESIAN_POINT('Ctrl Pts',(180.65954965353,1.58458405733109,48.35));
#77783=CARTESIAN_POINT('Ctrl Pts',(180.845634162426,1.58458405733109,48.35));
#77784=CARTESIAN_POINT('Ctrl Pts',(180.405934274197,2.48499327898026,48.5));
#77785=CARTESIAN_POINT('Ctrl Pts',(180.405934274197,2.48499327898026,48.35));
#77786=CARTESIAN_POINT('Ctrl Pts',(180.405934274197,1.94324696063995,48.5));
#77787=CARTESIAN_POINT('Ctrl Pts',(180.405934274197,1.94324696063995,48.35));
#77788=CARTESIAN_POINT('Ctrl Pts',(180.532741963863,1.76391565799713,48.5));
#77789=CARTESIAN_POINT('Ctrl Pts',(180.532741963863,1.76391565799713,48.35));
#77790=CARTESIAN_POINT('',(180.405934274197,2.48499327898026,48.5));
#77791=CARTESIAN_POINT('Ctrl Pts',(180.405934274197,2.48499327898026,48.5));
#77792=CARTESIAN_POINT('Ctrl Pts',(180.405934274197,1.94324696063995,48.5));
#77793=CARTESIAN_POINT('Ctrl Pts',(180.532741963863,1.76391565799713,48.5));
#77794=CARTESIAN_POINT('',(180.405934274197,2.48499327898026,48.35));
#77795=CARTESIAN_POINT('',(180.405934274197,2.48499327898026,48.5));
#77796=CARTESIAN_POINT('Ctrl Pts',(180.405934274197,2.48499327898026,48.35));
#77797=CARTESIAN_POINT('Ctrl Pts',(180.405934274197,1.94324696063995,48.35));
#77798=CARTESIAN_POINT('Ctrl Pts',(180.532741963863,1.76391565799713,48.35));
#77799=CARTESIAN_POINT('Ctrl Pts',(180.545497953892,3.22783091664314,48.5));
#77800=CARTESIAN_POINT('Ctrl Pts',(180.545497953892,3.22783091664314,48.35));
#77801=CARTESIAN_POINT('Ctrl Pts',(180.405934274197,3.02673944830894,48.5));
#77802=CARTESIAN_POINT('Ctrl Pts',(180.405934274197,3.02673944830894,48.35));
#77803=CARTESIAN_POINT('Ctrl Pts',(180.405934274197,2.48499327898026,48.5));
#77804=CARTESIAN_POINT('Ctrl Pts',(180.405934274197,2.48499327898026,48.35));
#77805=CARTESIAN_POINT('Ctrl Pts',(180.545497953892,3.22783091664314,48.5));
#77806=CARTESIAN_POINT('Ctrl Pts',(180.405934274197,3.02673944830894,48.5));
#77807=CARTESIAN_POINT('Ctrl Pts',(180.405934274197,2.48499327898026,48.5));
#77808=CARTESIAN_POINT('Ctrl Pts',(180.545497953892,3.22783091664314,48.35));
#77809=CARTESIAN_POINT('Ctrl Pts',(180.405934274197,3.02673944830894,48.35));
#77810=CARTESIAN_POINT('Ctrl Pts',(180.405934274197,2.48499327898026,48.35));
#77811=CARTESIAN_POINT('Ctrl Pts',(180.845634162426,1.36248314380646,48.5));
#77812=CARTESIAN_POINT('Ctrl Pts',(180.845634162426,1.36248314380646,48.35));
#77813=CARTESIAN_POINT('Ctrl Pts',(180.527489602566,1.36248314380646,48.5));
#77814=CARTESIAN_POINT('Ctrl Pts',(180.527489602566,1.36248314380646,48.35));
#77815=CARTESIAN_POINT('Ctrl Pts',(180.34590703249,1.59058684110642,48.5));
#77816=CARTESIAN_POINT('Ctrl Pts',(180.34590703249,1.59058684110642,48.35));
#77817=CARTESIAN_POINT('',(180.845634162426,1.36248314380646,48.5));
#77818=CARTESIAN_POINT('',(180.34590703249,1.59058684110642,48.5));
#77819=CARTESIAN_POINT('Ctrl Pts',(180.845634162426,1.36248314380646,48.5));
#77820=CARTESIAN_POINT('Ctrl Pts',(180.527489602566,1.36248314380646,48.5));
#77821=CARTESIAN_POINT('Ctrl Pts',(180.34590703249,1.59058684110642,48.5));
#77822=CARTESIAN_POINT('',(180.845634162426,1.36248314380646,48.35));
#77823=CARTESIAN_POINT('',(180.845634162426,1.36248314380646,48.5));
#77824=CARTESIAN_POINT('',(180.34590703249,1.59058684110642,48.35));
#77825=CARTESIAN_POINT('Ctrl Pts',(180.845634162426,1.36248314380646,48.35));
#77826=CARTESIAN_POINT('Ctrl Pts',(180.527489602566,1.36248314380646,48.35));
#77827=CARTESIAN_POINT('Ctrl Pts',(180.34590703249,1.59058684110642,48.35));
#77828=CARTESIAN_POINT('',(180.34590703249,1.59058684110642,48.5));
#77829=CARTESIAN_POINT('Ctrl Pts',(181.245565831661,1.49229192733765,48.5));
#77830=CARTESIAN_POINT('Ctrl Pts',(181.245565831661,1.49229192733765,48.35));
#77831=CARTESIAN_POINT('Ctrl Pts',(181.087243974209,1.36248314380646,48.5));
#77832=CARTESIAN_POINT('Ctrl Pts',(181.087243974209,1.36248314380646,48.35));
#77833=CARTESIAN_POINT('Ctrl Pts',(180.845634162426,1.36248314380646,48.5));
#77834=CARTESIAN_POINT('Ctrl Pts',(180.845634162426,1.36248314380646,48.35));
#77835=CARTESIAN_POINT('',(181.245565831661,1.49229192733765,48.5));
#77836=CARTESIAN_POINT('Ctrl Pts',(181.245565831661,1.49229192733765,48.5));
#77837=CARTESIAN_POINT('Ctrl Pts',(181.087243974209,1.36248314380646,48.5));
#77838=CARTESIAN_POINT('Ctrl Pts',(180.845634162426,1.36248314380646,48.5));
#77839=CARTESIAN_POINT('',(181.245565831661,1.49229192733765,48.35));
#77840=CARTESIAN_POINT('',(181.245565831661,1.49229192733765,48.5));
#77841=CARTESIAN_POINT('Ctrl Pts',(181.245565831661,1.49229192733765,48.35));
#77842=CARTESIAN_POINT('Ctrl Pts',(181.087243974209,1.36248314380646,48.35));
#77843=CARTESIAN_POINT('Ctrl Pts',(180.845634162426,1.36248314380646,48.35));
#77844=CARTESIAN_POINT('Ctrl Pts',(181.483424127102,1.85995900630951,48.5));
#77845=CARTESIAN_POINT('Ctrl Pts',(181.483424127102,1.85995900630951,48.35));
#77846=CARTESIAN_POINT('Ctrl Pts',(181.403887689114,1.62210100889206,48.5));
#77847=CARTESIAN_POINT('Ctrl Pts',(181.403887689114,1.62210100889206,48.35));
#77848=CARTESIAN_POINT('Ctrl Pts',(181.245565831661,1.49229192733765,48.5));
#77849=CARTESIAN_POINT('Ctrl Pts',(181.245565831661,1.49229192733765,48.35));
#77850=CARTESIAN_POINT('',(181.483424127102,1.85995900630951,48.5));
#77851=CARTESIAN_POINT('Ctrl Pts',(181.483424127102,1.85995900630951,48.5));
#77852=CARTESIAN_POINT('Ctrl Pts',(181.403887689114,1.62210100889206,48.5));
#77853=CARTESIAN_POINT('Ctrl Pts',(181.245565831661,1.49229192733765,48.5));
#77854=CARTESIAN_POINT('',(181.483424127102,1.85995900630951,48.35));
#77855=CARTESIAN_POINT('',(181.483424127102,1.85995900630951,48.5));
#77856=CARTESIAN_POINT('Ctrl Pts',(181.483424127102,1.85995900630951,48.35));
#77857=CARTESIAN_POINT('Ctrl Pts',(181.403887689114,1.62210100889206,48.35));
#77858=CARTESIAN_POINT('Ctrl Pts',(181.245565831661,1.49229192733765,48.35));
#77859=CARTESIAN_POINT('Ctrl Pts',(181.562959969044,2.48499327898026,48.5));
#77860=CARTESIAN_POINT('Ctrl Pts',(181.562959969044,2.48499327898026,48.35));
#77861=CARTESIAN_POINT('Ctrl Pts',(181.562959969044,2.09781730175018,48.5));
#77862=CARTESIAN_POINT('Ctrl Pts',(181.562959969044,2.09781730175018,48.35));
#77863=CARTESIAN_POINT('Ctrl Pts',(181.483424127102,1.85995900630951,48.5));
#77864=CARTESIAN_POINT('Ctrl Pts',(181.483424127102,1.85995900630951,48.35));
#77865=CARTESIAN_POINT('',(181.562959969044,2.48499327898026,48.5));
#77866=CARTESIAN_POINT('Ctrl Pts',(181.562959969044,2.48499327898026,48.5));
#77867=CARTESIAN_POINT('Ctrl Pts',(181.562959969044,2.09781730175018,48.5));
#77868=CARTESIAN_POINT('Ctrl Pts',(181.483424127102,1.85995900630951,48.5));
#77869=CARTESIAN_POINT('',(181.562959969044,2.48499327898026,48.35));
#77870=CARTESIAN_POINT('',(181.562959969044,2.48499327898026,48.5));
#77871=CARTESIAN_POINT('Ctrl Pts',(181.562959969044,2.48499327898026,48.35));
#77872=CARTESIAN_POINT('Ctrl Pts',(181.562959969044,2.09781730175018,48.35));
#77873=CARTESIAN_POINT('Ctrl Pts',(181.483424127102,1.85995900630951,48.35));
#77874=CARTESIAN_POINT('Ctrl Pts',(181.513437449932,3.00497958064079,48.5));
#77875=CARTESIAN_POINT('Ctrl Pts',(181.513437449932,3.00497958064079,48.35));
#77876=CARTESIAN_POINT('Ctrl Pts',(181.562959969044,2.81214186549187,48.5));
#77877=CARTESIAN_POINT('Ctrl Pts',(181.562959969044,2.81214186549187,48.35));
#77878=CARTESIAN_POINT('Ctrl Pts',(181.562959969044,2.48499327898026,48.5));
#77879=CARTESIAN_POINT('Ctrl Pts',(181.562959969044,2.48499327898026,48.35));
#77880=CARTESIAN_POINT('',(181.513437449932,3.00497958064079,48.5));
#77881=CARTESIAN_POINT('Ctrl Pts',(181.513437449932,3.00497958064079,48.5));
#77882=CARTESIAN_POINT('Ctrl Pts',(181.562959969044,2.81214186549187,48.5));
#77883=CARTESIAN_POINT('Ctrl Pts',(181.562959969044,2.48499327898026,48.5));
#77884=CARTESIAN_POINT('',(181.513437449932,3.00497958064079,48.35));
#77885=CARTESIAN_POINT('',(181.513437449932,3.00497958064079,48.5));
#77886=CARTESIAN_POINT('Ctrl Pts',(181.513437449932,3.00497958064079,48.35));
#77887=CARTESIAN_POINT('Ctrl Pts',(181.562959969044,2.81214186549187,48.35));
#77888=CARTESIAN_POINT('Ctrl Pts',(181.562959969044,2.48499327898026,48.35));
#77889=CARTESIAN_POINT('Ctrl Pts',(181.376875460148,3.33212831616402,48.5));
#77890=CARTESIAN_POINT('Ctrl Pts',(181.376875460148,3.33212831616402,48.35));
#77891=CARTESIAN_POINT('Ctrl Pts',(181.46391493082,3.19781729578972,48.5));
#77892=CARTESIAN_POINT('Ctrl Pts',(181.46391493082,3.19781729578972,48.35));
#77893=CARTESIAN_POINT('Ctrl Pts',(181.513437449932,3.00497958064079,48.5));
#77894=CARTESIAN_POINT('Ctrl Pts',(181.513437449932,3.00497958064079,48.35));
#77895=CARTESIAN_POINT('',(181.376875460148,3.33212831616402,48.5));
#77896=CARTESIAN_POINT('Ctrl Pts',(181.376875460148,3.33212831616402,48.5));
#77897=CARTESIAN_POINT('Ctrl Pts',(181.46391493082,3.19781729578972,48.5));
#77898=CARTESIAN_POINT('Ctrl Pts',(181.513437449932,3.00497958064079,48.5));
#77899=CARTESIAN_POINT('',(181.376875460148,3.33212831616402,48.35));
#77900=CARTESIAN_POINT('',(181.376875460148,3.33212831616402,48.5));
#77901=CARTESIAN_POINT('Ctrl Pts',(181.376875460148,3.33212831616402,48.35));
#77902=CARTESIAN_POINT('Ctrl Pts',(181.46391493082,3.19781729578972,48.35));
#77903=CARTESIAN_POINT('Ctrl Pts',(181.513437449932,3.00497958064079,48.35));
#77904=CARTESIAN_POINT('Ctrl Pts',(181.156275689602,3.5377217233181,48.5));
#77905=CARTESIAN_POINT('Ctrl Pts',(181.156275689602,3.5377217233181,48.35));
#77906=CARTESIAN_POINT('Ctrl Pts',(181.289835989475,3.46643933653831,48.5));
#77907=CARTESIAN_POINT('Ctrl Pts',(181.289835989475,3.46643933653831,48.35));
#77908=CARTESIAN_POINT('Ctrl Pts',(181.376875460148,3.33212831616402,48.5));
#77909=CARTESIAN_POINT('Ctrl Pts',(181.376875460148,3.33212831616402,48.35));
#77910=CARTESIAN_POINT('',(181.156275689602,3.5377217233181,48.5));
#77911=CARTESIAN_POINT('Ctrl Pts',(181.156275689602,3.5377217233181,48.5));
#77912=CARTESIAN_POINT('Ctrl Pts',(181.289835989475,3.46643933653831,48.5));
#77913=CARTESIAN_POINT('Ctrl Pts',(181.376875460148,3.33212831616402,48.5));
#77914=CARTESIAN_POINT('',(181.156275689602,3.5377217233181,48.35));
#77915=CARTESIAN_POINT('',(181.156275689602,3.5377217233181,48.5));
#77916=CARTESIAN_POINT('Ctrl Pts',(181.156275689602,3.5377217233181,48.35));
#77917=CARTESIAN_POINT('Ctrl Pts',(181.289835989475,3.46643933653831,48.35));
#77918=CARTESIAN_POINT('Ctrl Pts',(181.376875460148,3.33212831616402,48.35));
#77919=CARTESIAN_POINT('Ctrl Pts',(180.845634162426,3.60900411009789,48.5));
#77920=CARTESIAN_POINT('Ctrl Pts',(180.845634162426,3.60900411009789,48.35));
#77921=CARTESIAN_POINT('Ctrl Pts',(181.022714793682,3.60900411009789,48.5));
#77922=CARTESIAN_POINT('Ctrl Pts',(181.022714793682,3.60900411009789,48.35));
#77923=CARTESIAN_POINT('Ctrl Pts',(181.156275689602,3.5377217233181,48.5));
#77924=CARTESIAN_POINT('Ctrl Pts',(181.156275689602,3.5377217233181,48.35));
#77925=CARTESIAN_POINT('',(180.845634162426,3.60900411009789,48.5));
#77926=CARTESIAN_POINT('Ctrl Pts',(180.845634162426,3.60900411009789,48.5));
#77927=CARTESIAN_POINT('Ctrl Pts',(181.022714793682,3.60900411009789,48.5));
#77928=CARTESIAN_POINT('Ctrl Pts',(181.156275689602,3.5377217233181,48.5));
#77929=CARTESIAN_POINT('',(180.845634162426,3.60900411009789,48.35));
#77930=CARTESIAN_POINT('',(180.845634162426,3.60900411009789,48.5));
#77931=CARTESIAN_POINT('Ctrl Pts',(180.845634162426,3.60900411009789,48.35));
#77932=CARTESIAN_POINT('Ctrl Pts',(181.022714793682,3.60900411009789,48.35));
#77933=CARTESIAN_POINT('Ctrl Pts',(181.156275689602,3.5377217233181,48.35));
#77934=CARTESIAN_POINT('Ctrl Pts',(180.447203338146,3.47994545102119,48.5));
#77935=CARTESIAN_POINT('Ctrl Pts',(180.447203338146,3.47994545102119,48.35));
#77936=CARTESIAN_POINT('Ctrl Pts',(180.605525195599,3.60900411009789,48.5));
#77937=CARTESIAN_POINT('Ctrl Pts',(180.605525195599,3.60900411009789,48.35));
#77938=CARTESIAN_POINT('Ctrl Pts',(180.845634162426,3.60900411009789,48.5));
#77939=CARTESIAN_POINT('Ctrl Pts',(180.845634162426,3.60900411009789,48.35));
#77940=CARTESIAN_POINT('',(180.447203338146,3.47994545102119,48.5));
#77941=CARTESIAN_POINT('Ctrl Pts',(180.447203338146,3.47994545102119,48.5));
#77942=CARTESIAN_POINT('Ctrl Pts',(180.605525195599,3.60900411009789,48.5));
#77943=CARTESIAN_POINT('Ctrl Pts',(180.845634162426,3.60900411009789,48.5));
#77944=CARTESIAN_POINT('',(180.447203338146,3.47994545102119,48.35));
#77945=CARTESIAN_POINT('',(180.447203338146,3.47994545102119,48.5));
#77946=CARTESIAN_POINT('Ctrl Pts',(180.447203338146,3.47994545102119,48.35));
#77947=CARTESIAN_POINT('Ctrl Pts',(180.605525195599,3.60900411009789,48.35));
#77948=CARTESIAN_POINT('Ctrl Pts',(180.845634162426,3.60900411009789,48.35));
#77949=CARTESIAN_POINT('Ctrl Pts',(180.208594620228,3.11302864551544,48.5));
#77950=CARTESIAN_POINT('Ctrl Pts',(180.208594620228,3.11302864551544,48.35));
#77951=CARTESIAN_POINT('Ctrl Pts',(180.288881182671,3.3508867919445,48.5));
#77952=CARTESIAN_POINT('Ctrl Pts',(180.288881182671,3.3508867919445,48.35));
#77953=CARTESIAN_POINT('Ctrl Pts',(180.447203338146,3.47994545102119,48.5));
#77954=CARTESIAN_POINT('Ctrl Pts',(180.447203338146,3.47994545102119,48.35));
#77955=CARTESIAN_POINT('',(180.208594620228,3.11302864551544,48.5));
#77956=CARTESIAN_POINT('Ctrl Pts',(180.208594620228,3.11302864551544,48.5));
#77957=CARTESIAN_POINT('Ctrl Pts',(180.288881182671,3.3508867919445,48.5));
#77958=CARTESIAN_POINT('Ctrl Pts',(180.447203338146,3.47994545102119,48.5));
#77959=CARTESIAN_POINT('',(180.208594620228,3.11302864551544,48.35));
#77960=CARTESIAN_POINT('',(180.208594620228,3.11302864551544,48.5));
#77961=CARTESIAN_POINT('Ctrl Pts',(180.208594620228,3.11302864551544,48.35));
#77962=CARTESIAN_POINT('Ctrl Pts',(180.288881182671,3.3508867919445,48.35));
#77963=CARTESIAN_POINT('Ctrl Pts',(180.447203338146,3.47994545102119,48.35));
#77964=CARTESIAN_POINT('Ctrl Pts',(180.128308355808,2.48499327898026,48.5));
#77965=CARTESIAN_POINT('Ctrl Pts',(180.128308355808,2.48499327898026,48.35));
#77966=CARTESIAN_POINT('Ctrl Pts',(180.128308355808,2.87517049908638,48.5));
#77967=CARTESIAN_POINT('Ctrl Pts',(180.128308355808,2.87517049908638,48.35));
#77968=CARTESIAN_POINT('Ctrl Pts',(180.208594620228,3.11302864551544,48.5));
#77969=CARTESIAN_POINT('Ctrl Pts',(180.208594620228,3.11302864551544,48.35));
#77970=CARTESIAN_POINT('',(180.128308355808,2.48499327898026,48.5));
#77971=CARTESIAN_POINT('Ctrl Pts',(180.128308355808,2.48499327898026,48.5));
#77972=CARTESIAN_POINT('Ctrl Pts',(180.128308355808,2.87517049908638,48.5));
#77973=CARTESIAN_POINT('Ctrl Pts',(180.208594620228,3.11302864551544,48.5));
#77974=CARTESIAN_POINT('',(180.128308355808,2.48499327898026,48.35));
#77975=CARTESIAN_POINT('',(180.128308355808,2.48499327898026,48.5));
#77976=CARTESIAN_POINT('Ctrl Pts',(180.128308355808,2.48499327898026,48.35));
#77977=CARTESIAN_POINT('Ctrl Pts',(180.128308355808,2.87517049908638,48.35));
#77978=CARTESIAN_POINT('Ctrl Pts',(180.208594620228,3.11302864551544,48.35));
#77979=CARTESIAN_POINT('Ctrl Pts',(180.34590703249,1.59058684110642,48.5));
#77980=CARTESIAN_POINT('Ctrl Pts',(180.34590703249,1.59058684110642,48.35));
#77981=CARTESIAN_POINT('Ctrl Pts',(180.128308355808,1.86521166563034,48.5));
#77982=CARTESIAN_POINT('Ctrl Pts',(180.128308355808,1.86521166563034,48.35));
#77983=CARTESIAN_POINT('Ctrl Pts',(180.128308355808,2.48499327898026,48.5));
#77984=CARTESIAN_POINT('Ctrl Pts',(180.128308355808,2.48499327898026,48.35));
#77985=CARTESIAN_POINT('Ctrl Pts',(180.34590703249,1.59058684110642,48.5));
#77986=CARTESIAN_POINT('Ctrl Pts',(180.128308355808,1.86521166563034,48.5));
#77987=CARTESIAN_POINT('Ctrl Pts',(180.128308355808,2.48499327898026,48.5));
#77988=CARTESIAN_POINT('Ctrl Pts',(180.34590703249,1.59058684110642,48.35));
#77989=CARTESIAN_POINT('Ctrl Pts',(180.128308355808,1.86521166563034,48.35));
#77990=CARTESIAN_POINT('Ctrl Pts',(180.128308355808,2.48499327898026,48.35));
#77991=CARTESIAN_POINT('Origin',(179.99999974668,2.48574362695217,48.35));
#77992=CARTESIAN_POINT('Ctrl Pts',(179.126602977514,2.7363575398922,48.5));
#77993=CARTESIAN_POINT('Ctrl Pts',(179.126602977514,2.7363575398922,48.35));
#77994=CARTESIAN_POINT('Ctrl Pts',(179.308935821056,3.07776266336441,48.5));
#77995=CARTESIAN_POINT('Ctrl Pts',(179.308935821056,3.07776266336441,48.35));
#77996=CARTESIAN_POINT('Ctrl Pts',(179.51452922821,3.3118691444397,48.5));
#77997=CARTESIAN_POINT('Ctrl Pts',(179.51452922821,3.3118691444397,48.35));
#77998=CARTESIAN_POINT('',(179.126602977514,2.7363575398922,48.5));
#77999=CARTESIAN_POINT('',(179.51452922821,3.3118691444397,48.5));
#78000=CARTESIAN_POINT('Ctrl Pts',(179.126602977514,2.7363575398922,48.5));
#78001=CARTESIAN_POINT('Ctrl Pts',(179.308935821056,3.07776266336441,48.5));
#78002=CARTESIAN_POINT('Ctrl Pts',(179.51452922821,3.3118691444397,48.5));
#78003=CARTESIAN_POINT('',(179.126602977514,2.7363575398922,48.35));
#78004=CARTESIAN_POINT('',(179.126602977514,2.7363575398922,48.5));
#78005=CARTESIAN_POINT('',(179.51452922821,3.3118691444397,48.35));
#78006=CARTESIAN_POINT('Ctrl Pts',(179.126602977514,2.7363575398922,48.35));
#78007=CARTESIAN_POINT('Ctrl Pts',(179.308935821056,3.07776266336441,48.35));
#78008=CARTESIAN_POINT('Ctrl Pts',(179.51452922821,3.3118691444397,48.35));
#78009=CARTESIAN_POINT('',(179.51452922821,3.3118691444397,48.5));
#78010=CARTESIAN_POINT('Ctrl Pts',(178.846725791693,2.02728533744812,48.5));
#78011=CARTESIAN_POINT('Ctrl Pts',(178.846725791693,2.02728533744812,48.35));
#78012=CARTESIAN_POINT('Ctrl Pts',(178.944270133972,2.39495241641998,48.5));
#78013=CARTESIAN_POINT('Ctrl Pts',(178.944270133972,2.39495241641998,48.35));
#78014=CARTESIAN_POINT('Ctrl Pts',(179.126602977514,2.7363575398922,48.5));
#78015=CARTESIAN_POINT('Ctrl Pts',(179.126602977514,2.7363575398922,48.35));
#78016=CARTESIAN_POINT('',(178.846725791693,2.02728533744812,48.5));
#78017=CARTESIAN_POINT('Ctrl Pts',(178.846725791693,2.02728533744812,48.5));
#78018=CARTESIAN_POINT('Ctrl Pts',(178.944270133972,2.39495241641998,48.5));
#78019=CARTESIAN_POINT('Ctrl Pts',(179.126602977514,2.7363575398922,48.5));
#78020=CARTESIAN_POINT('',(178.846725791693,2.02728533744812,48.35));
#78021=CARTESIAN_POINT('',(178.846725791693,2.02728533744812,48.5));
#78022=CARTESIAN_POINT('Ctrl Pts',(178.846725791693,2.02728533744812,48.35));
#78023=CARTESIAN_POINT('Ctrl Pts',(178.944270133972,2.39495241641998,48.35));
#78024=CARTESIAN_POINT('Ctrl Pts',(179.126602977514,2.7363575398922,48.35));
#78025=CARTESIAN_POINT('Ctrl Pts',(178.744679361582,1.40000009536743,48.5));
#78026=CARTESIAN_POINT('Ctrl Pts',(178.744679361582,1.40000009536743,48.35));
#78027=CARTESIAN_POINT('Ctrl Pts',(178.749181449413,1.65961825847626,48.5));
#78028=CARTESIAN_POINT('Ctrl Pts',(178.749181449413,1.65961825847626,48.35));
#78029=CARTESIAN_POINT('Ctrl Pts',(178.846725791693,2.02728533744812,48.5));
#78030=CARTESIAN_POINT('Ctrl Pts',(178.846725791693,2.02728533744812,48.35));
#78031=CARTESIAN_POINT('',(178.744679361582,1.40000009536743,48.5));
#78032=CARTESIAN_POINT('Ctrl Pts',(178.744679361582,1.40000009536743,48.5));
#78033=CARTESIAN_POINT('Ctrl Pts',(178.749181449413,1.65961825847626,48.5));
#78034=CARTESIAN_POINT('Ctrl Pts',(178.846725791693,2.02728533744812,48.5));
#78035=CARTESIAN_POINT('',(178.744679361582,1.40000009536743,48.35));
#78036=CARTESIAN_POINT('',(178.744679361582,1.40000009536743,48.5));
#78037=CARTESIAN_POINT('Ctrl Pts',(178.744679361582,1.40000009536743,48.35));
#78038=CARTESIAN_POINT('Ctrl Pts',(178.749181449413,1.65961825847626,48.35));
#78039=CARTESIAN_POINT('Ctrl Pts',(178.846725791693,2.02728533744812,48.35));
#78040=CARTESIAN_POINT('Origin',(179.022305577993,1.40000009536743,48.5));
#78041=CARTESIAN_POINT('',(179.022305577993,1.40000009536743,48.5));
#78042=CARTESIAN_POINT('',(89.5111527889967,1.40000009536743,48.5));
#78043=CARTESIAN_POINT('',(179.022305577993,1.40000009536743,48.35));
#78044=CARTESIAN_POINT('',(179.022305577993,1.40000009536743,48.5));
#78045=CARTESIAN_POINT('',(179.022305577993,1.40000009536743,48.35));
#78046=CARTESIAN_POINT('Ctrl Pts',(179.125852704048,2.00477504730225,48.5));
#78047=CARTESIAN_POINT('Ctrl Pts',(179.125852704048,2.00477504730225,48.35));
#78048=CARTESIAN_POINT('Ctrl Pts',(179.044815719128,1.72864937782288,48.5));
#78049=CARTESIAN_POINT('Ctrl Pts',(179.044815719128,1.72864937782288,48.35));
#78050=CARTESIAN_POINT('Ctrl Pts',(179.022305577993,1.40000009536743,48.5));
#78051=CARTESIAN_POINT('Ctrl Pts',(179.022305577993,1.40000009536743,48.35));
#78052=CARTESIAN_POINT('',(179.125852704048,2.00477504730225,48.5));
#78053=CARTESIAN_POINT('Ctrl Pts',(179.125852704048,2.00477504730225,48.5));
#78054=CARTESIAN_POINT('Ctrl Pts',(179.044815719128,1.72864937782288,48.5));
#78055=CARTESIAN_POINT('Ctrl Pts',(179.022305577993,1.40000009536743,48.5));
#78056=CARTESIAN_POINT('',(179.125852704048,2.00477504730225,48.35));
#78057=CARTESIAN_POINT('',(179.125852704048,2.00477504730225,48.5));
#78058=CARTESIAN_POINT('Ctrl Pts',(179.125852704048,2.00477504730225,48.35));
#78059=CARTESIAN_POINT('Ctrl Pts',(179.044815719128,1.72864937782288,48.35));
#78060=CARTESIAN_POINT('Ctrl Pts',(179.022305577993,1.40000009536743,48.35));
#78061=CARTESIAN_POINT('Ctrl Pts',(179.444747388363,2.76712143421173,48.5));
#78062=CARTESIAN_POINT('Ctrl Pts',(179.444747388363,2.76712143421173,48.35));
#78063=CARTESIAN_POINT('Ctrl Pts',(179.238403856754,2.3964529633522,48.5));
#78064=CARTESIAN_POINT('Ctrl Pts',(179.238403856754,2.3964529633522,48.35));
#78065=CARTESIAN_POINT('Ctrl Pts',(179.125852704048,2.00477504730225,48.5));
#78066=CARTESIAN_POINT('Ctrl Pts',(179.125852704048,2.00477504730225,48.35));
#78067=CARTESIAN_POINT('',(179.444747388363,2.76712143421173,48.5));
#78068=CARTESIAN_POINT('Ctrl Pts',(179.444747388363,2.76712143421173,48.5));
#78069=CARTESIAN_POINT('Ctrl Pts',(179.238403856754,2.3964529633522,48.5));
#78070=CARTESIAN_POINT('Ctrl Pts',(179.125852704048,2.00477504730225,48.5));
#78071=CARTESIAN_POINT('',(179.444747388363,2.76712143421173,48.35));
#78072=CARTESIAN_POINT('',(179.444747388363,2.76712143421173,48.5));
#78073=CARTESIAN_POINT('Ctrl Pts',(179.444747388363,2.76712143421173,48.35));
#78074=CARTESIAN_POINT('Ctrl Pts',(179.238403856754,2.3964529633522,48.35));
#78075=CARTESIAN_POINT('Ctrl Pts',(179.125852704048,2.00477504730225,48.35));
#78076=CARTESIAN_POINT('Ctrl Pts',(179.861186861992,3.36139166355133,48.5));
#78077=CARTESIAN_POINT('Ctrl Pts',(179.861186861992,3.36139166355133,48.35));
#78078=CARTESIAN_POINT('Ctrl Pts',(179.651091516018,3.13779005408287,48.5));
#78079=CARTESIAN_POINT('Ctrl Pts',(179.651091516018,3.13779005408287,48.35));
#78080=CARTESIAN_POINT('Ctrl Pts',(179.444747388363,2.76712143421173,48.5));
#78081=CARTESIAN_POINT('Ctrl Pts',(179.444747388363,2.76712143421173,48.35));
#78082=CARTESIAN_POINT('',(179.861186861992,3.36139166355133,48.5));
#78083=CARTESIAN_POINT('Ctrl Pts',(179.861186861992,3.36139166355133,48.5));
#78084=CARTESIAN_POINT('Ctrl Pts',(179.651091516018,3.13779005408287,48.5));
#78085=CARTESIAN_POINT('Ctrl Pts',(179.444747388363,2.76712143421173,48.5));
#78086=CARTESIAN_POINT('',(179.861186861992,3.36139166355133,48.35));
#78087=CARTESIAN_POINT('',(179.861186861992,3.36139166355133,48.5));
#78088=CARTESIAN_POINT('Ctrl Pts',(179.861186861992,3.36139166355133,48.35));
#78089=CARTESIAN_POINT('Ctrl Pts',(179.651091516018,3.13779005408287,48.35));
#78090=CARTESIAN_POINT('Ctrl Pts',(179.444747388363,2.76712143421173,48.35));
#78091=CARTESIAN_POINT('Origin',(179.861186861992,3.57148715853691,48.5));
#78092=CARTESIAN_POINT('',(179.861186861992,3.57148715853691,48.5));
#78093=CARTESIAN_POINT('',(179.861186861992,5.78574357926846,48.5));
#78094=CARTESIAN_POINT('',(179.861186861992,3.57148715853691,48.35));
#78095=CARTESIAN_POINT('',(179.861186861992,3.57148715853691,48.5));
#78096=CARTESIAN_POINT('',(179.861186861992,3.57148715853691,48.35));
#78097=CARTESIAN_POINT('Origin',(178.437039524317,3.57148715853691,48.5));
#78098=CARTESIAN_POINT('',(178.437039524317,3.57148715853691,48.5));
#78099=CARTESIAN_POINT('',(89.2185197621584,3.57148715853691,48.5));
#78100=CARTESIAN_POINT('',(178.437039524317,3.57148715853691,48.35));
#78101=CARTESIAN_POINT('',(178.437039524317,3.57148715853691,48.5));
#78102=CARTESIAN_POINT('',(178.437039524317,3.57148715853691,48.35));
#78103=CARTESIAN_POINT('Origin',(178.437039524317,3.3118691444397,48.5));
#78104=CARTESIAN_POINT('',(178.437039524317,3.3118691444397,48.5));
#78105=CARTESIAN_POINT('',(178.437039524317,5.65593457221985,48.5));
#78106=CARTESIAN_POINT('',(178.437039524317,3.3118691444397,48.35));
#78107=CARTESIAN_POINT('',(178.437039524317,3.3118691444397,48.5));
#78108=CARTESIAN_POINT('',(178.437039524317,3.3118691444397,48.35));
#78109=CARTESIAN_POINT('Origin',(179.51452922821,3.3118691444397,48.5));
#78110=CARTESIAN_POINT('',(89.7572646141052,3.3118691444397,48.5));
#78111=CARTESIAN_POINT('',(179.51452922821,3.3118691444397,48.35));
#78112=CARTESIAN_POINT('Origin',(179.99999974668,2.48574362695217,48.35));
#78113=CARTESIAN_POINT('Origin',(0.,8.,48.5));
#78114=CARTESIAN_POINT('Ctrl Pts',(170.857640046626,3.38540250062943,48.5));
#78115=CARTESIAN_POINT('Ctrl Pts',(170.857640046626,3.38540250062943,48.35));
#78116=CARTESIAN_POINT('Ctrl Pts',(170.671555239707,3.38540250062943,48.5));
#78117=CARTESIAN_POINT('Ctrl Pts',(170.671555239707,3.38540250062943,48.35));
#78118=CARTESIAN_POINT('Ctrl Pts',(170.560504931957,3.22783091664314,48.5));
#78119=CARTESIAN_POINT('Ctrl Pts',(170.560504931957,3.22783091664314,48.35));
#78120=CARTESIAN_POINT('',(170.857640046626,3.38540250062943,48.5));
#78121=CARTESIAN_POINT('',(170.560504931957,3.22783091664314,48.5));
#78122=CARTESIAN_POINT('Ctrl Pts',(170.857640046626,3.38540250062943,48.5));
#78123=CARTESIAN_POINT('Ctrl Pts',(170.671555239707,3.38540250062943,48.5));
#78124=CARTESIAN_POINT('Ctrl Pts',(170.560504931957,3.22783091664314,48.5));
#78125=CARTESIAN_POINT('',(170.857640046626,3.38540250062943,48.35));
#78126=CARTESIAN_POINT('',(170.857640046626,3.38540250062943,48.5));
#78127=CARTESIAN_POINT('',(170.560504931957,3.22783091664314,48.35));
#78128=CARTESIAN_POINT('Ctrl Pts',(170.857640046626,3.38540250062943,48.35));
#78129=CARTESIAN_POINT('Ctrl Pts',(170.671555239707,3.38540250062943,48.35));
#78130=CARTESIAN_POINT('Ctrl Pts',(170.560504931957,3.22783091664314,48.35));
#78131=CARTESIAN_POINT('',(170.560504931957,3.22783091664314,48.5));
#78132=CARTESIAN_POINT('Ctrl Pts',(171.173533339053,3.2068213224411,48.5));
#78133=CARTESIAN_POINT('Ctrl Pts',(171.173533339053,3.2068213224411,48.35));
#78134=CARTESIAN_POINT('Ctrl Pts',(171.046725649387,3.38540250062943,48.5));
#78135=CARTESIAN_POINT('Ctrl Pts',(171.046725649387,3.38540250062943,48.35));
#78136=CARTESIAN_POINT('Ctrl Pts',(170.857640046626,3.38540250062943,48.5));
#78137=CARTESIAN_POINT('Ctrl Pts',(170.857640046626,3.38540250062943,48.35));
#78138=CARTESIAN_POINT('',(171.173533339053,3.2068213224411,48.5));
#78139=CARTESIAN_POINT('Ctrl Pts',(171.173533339053,3.2068213224411,48.5));
#78140=CARTESIAN_POINT('Ctrl Pts',(171.046725649387,3.38540250062943,48.5));
#78141=CARTESIAN_POINT('Ctrl Pts',(170.857640046626,3.38540250062943,48.5));
#78142=CARTESIAN_POINT('',(171.173533339053,3.2068213224411,48.35));
#78143=CARTESIAN_POINT('',(171.173533339053,3.2068213224411,48.5));
#78144=CARTESIAN_POINT('Ctrl Pts',(171.173533339053,3.2068213224411,48.35));
#78145=CARTESIAN_POINT('Ctrl Pts',(171.046725649387,3.38540250062943,48.35));
#78146=CARTESIAN_POINT('Ctrl Pts',(170.857640046626,3.38540250062943,48.35));
#78147=CARTESIAN_POINT('Ctrl Pts',(171.30034102872,2.48499327898026,48.5));
#78148=CARTESIAN_POINT('Ctrl Pts',(171.30034102872,2.48499327898026,48.35));
#78149=CARTESIAN_POINT('Ctrl Pts',(171.30034102872,3.02824014425278,48.5));
#78150=CARTESIAN_POINT('Ctrl Pts',(171.30034102872,3.02824014425278,48.35));
#78151=CARTESIAN_POINT('Ctrl Pts',(171.173533339053,3.2068213224411,48.5));
#78152=CARTESIAN_POINT('Ctrl Pts',(171.173533339053,3.2068213224411,48.35));
#78153=CARTESIAN_POINT('',(171.30034102872,2.48499327898026,48.5));
#78154=CARTESIAN_POINT('Ctrl Pts',(171.30034102872,2.48499327898026,48.5));
#78155=CARTESIAN_POINT('Ctrl Pts',(171.30034102872,3.02824014425278,48.5));
#78156=CARTESIAN_POINT('Ctrl Pts',(171.173533339053,3.2068213224411,48.5));
#78157=CARTESIAN_POINT('',(171.30034102872,2.48499327898026,48.35));
#78158=CARTESIAN_POINT('',(171.30034102872,2.48499327898026,48.5));
#78159=CARTESIAN_POINT('Ctrl Pts',(171.30034102872,2.48499327898026,48.35));
#78160=CARTESIAN_POINT('Ctrl Pts',(171.30034102872,3.02824014425278,48.35));
#78161=CARTESIAN_POINT('Ctrl Pts',(171.173533339053,3.2068213224411,48.35));
#78162=CARTESIAN_POINT('Ctrl Pts',(171.173533339053,1.76466578245163,48.5));
#78163=CARTESIAN_POINT('Ctrl Pts',(171.173533339053,1.76466578245163,48.35));
#78164=CARTESIAN_POINT('Ctrl Pts',(171.30034102872,1.9447478055954,48.5));
#78165=CARTESIAN_POINT('Ctrl Pts',(171.30034102872,1.9447478055954,48.35));
#78166=CARTESIAN_POINT('Ctrl Pts',(171.30034102872,2.48499327898026,48.5));
#78167=CARTESIAN_POINT('Ctrl Pts',(171.30034102872,2.48499327898026,48.35));
#78168=CARTESIAN_POINT('',(171.173533339053,1.76466578245163,48.5));
#78169=CARTESIAN_POINT('Ctrl Pts',(171.173533339053,1.76466578245163,48.5));
#78170=CARTESIAN_POINT('Ctrl Pts',(171.30034102872,1.9447478055954,48.5));
#78171=CARTESIAN_POINT('Ctrl Pts',(171.30034102872,2.48499327898026,48.5));
#78172=CARTESIAN_POINT('',(171.173533339053,1.76466578245163,48.35));
#78173=CARTESIAN_POINT('',(171.173533339053,1.76466578245163,48.5));
#78174=CARTESIAN_POINT('Ctrl Pts',(171.173533339053,1.76466578245163,48.35));
#78175=CARTESIAN_POINT('Ctrl Pts',(171.30034102872,1.9447478055954,48.35));
#78176=CARTESIAN_POINT('Ctrl Pts',(171.30034102872,2.48499327898026,48.35));
#78177=CARTESIAN_POINT('Ctrl Pts',(170.860641140491,1.58458405733109,48.5));
#78178=CARTESIAN_POINT('Ctrl Pts',(170.860641140491,1.58458405733109,48.35));
#78179=CARTESIAN_POINT('Ctrl Pts',(171.046725649387,1.58458405733109,48.5));
#78180=CARTESIAN_POINT('Ctrl Pts',(171.046725649387,1.58458405733109,48.35));
#78181=CARTESIAN_POINT('Ctrl Pts',(171.173533339053,1.76466578245163,48.5));
#78182=CARTESIAN_POINT('Ctrl Pts',(171.173533339053,1.76466578245163,48.35));
#78183=CARTESIAN_POINT('',(170.860641140491,1.58458405733109,48.5));
#78184=CARTESIAN_POINT('Ctrl Pts',(170.860641140491,1.58458405733109,48.5));
#78185=CARTESIAN_POINT('Ctrl Pts',(171.046725649387,1.58458405733109,48.5));
#78186=CARTESIAN_POINT('Ctrl Pts',(171.173533339053,1.76466578245163,48.5));
#78187=CARTESIAN_POINT('',(170.860641140491,1.58458405733109,48.35));
#78188=CARTESIAN_POINT('',(170.860641140491,1.58458405733109,48.5));
#78189=CARTESIAN_POINT('Ctrl Pts',(170.860641140491,1.58458405733109,48.35));
#78190=CARTESIAN_POINT('Ctrl Pts',(171.046725649387,1.58458405733109,48.35));
#78191=CARTESIAN_POINT('Ctrl Pts',(171.173533339053,1.76466578245163,48.35));
#78192=CARTESIAN_POINT('Ctrl Pts',(170.547748941928,1.76391565799713,48.5));
#78193=CARTESIAN_POINT('Ctrl Pts',(170.547748941928,1.76391565799713,48.35));
#78194=CARTESIAN_POINT('Ctrl Pts',(170.674556631595,1.58458405733109,48.5));
#78195=CARTESIAN_POINT('Ctrl Pts',(170.674556631595,1.58458405733109,48.35));
#78196=CARTESIAN_POINT('Ctrl Pts',(170.860641140491,1.58458405733109,48.5));
#78197=CARTESIAN_POINT('Ctrl Pts',(170.860641140491,1.58458405733109,48.35));
#78198=CARTESIAN_POINT('',(170.547748941928,1.76391565799713,48.5));
#78199=CARTESIAN_POINT('Ctrl Pts',(170.547748941928,1.76391565799713,48.5));
#78200=CARTESIAN_POINT('Ctrl Pts',(170.674556631595,1.58458405733109,48.5));
#78201=CARTESIAN_POINT('Ctrl Pts',(170.860641140491,1.58458405733109,48.5));
#78202=CARTESIAN_POINT('',(170.547748941928,1.76391565799713,48.35));
#78203=CARTESIAN_POINT('',(170.547748941928,1.76391565799713,48.5));
#78204=CARTESIAN_POINT('Ctrl Pts',(170.547748941928,1.76391565799713,48.35));
#78205=CARTESIAN_POINT('Ctrl Pts',(170.674556631595,1.58458405733109,48.35));
#78206=CARTESIAN_POINT('Ctrl Pts',(170.860641140491,1.58458405733109,48.35));
#78207=CARTESIAN_POINT('Ctrl Pts',(170.420941252261,2.48499327898026,48.5));
#78208=CARTESIAN_POINT('Ctrl Pts',(170.420941252261,2.48499327898026,48.35));
#78209=CARTESIAN_POINT('Ctrl Pts',(170.420941252261,1.94324696063995,48.5));
#78210=CARTESIAN_POINT('Ctrl Pts',(170.420941252261,1.94324696063995,48.35));
#78211=CARTESIAN_POINT('Ctrl Pts',(170.547748941928,1.76391565799713,48.5));
#78212=CARTESIAN_POINT('Ctrl Pts',(170.547748941928,1.76391565799713,48.35));
#78213=CARTESIAN_POINT('',(170.420941252261,2.48499327898026,48.5));
#78214=CARTESIAN_POINT('Ctrl Pts',(170.420941252261,2.48499327898026,48.5));
#78215=CARTESIAN_POINT('Ctrl Pts',(170.420941252261,1.94324696063995,48.5));
#78216=CARTESIAN_POINT('Ctrl Pts',(170.547748941928,1.76391565799713,48.5));
#78217=CARTESIAN_POINT('',(170.420941252261,2.48499327898026,48.35));
#78218=CARTESIAN_POINT('',(170.420941252261,2.48499327898026,48.5));
#78219=CARTESIAN_POINT('Ctrl Pts',(170.420941252261,2.48499327898026,48.35));
#78220=CARTESIAN_POINT('Ctrl Pts',(170.420941252261,1.94324696063995,48.35));
#78221=CARTESIAN_POINT('Ctrl Pts',(170.547748941928,1.76391565799713,48.35));
#78222=CARTESIAN_POINT('Ctrl Pts',(170.560504931957,3.22783091664314,48.5));
#78223=CARTESIAN_POINT('Ctrl Pts',(170.560504931957,3.22783091664314,48.35));
#78224=CARTESIAN_POINT('Ctrl Pts',(170.420941252261,3.02673944830894,48.5));
#78225=CARTESIAN_POINT('Ctrl Pts',(170.420941252261,3.02673944830894,48.35));
#78226=CARTESIAN_POINT('Ctrl Pts',(170.420941252261,2.48499327898026,48.5));
#78227=CARTESIAN_POINT('Ctrl Pts',(170.420941252261,2.48499327898026,48.35));
#78228=CARTESIAN_POINT('Ctrl Pts',(170.560504931957,3.22783091664314,48.5));
#78229=CARTESIAN_POINT('Ctrl Pts',(170.420941252261,3.02673944830894,48.5));
#78230=CARTESIAN_POINT('Ctrl Pts',(170.420941252261,2.48499327898026,48.5));
#78231=CARTESIAN_POINT('Ctrl Pts',(170.560504931957,3.22783091664314,48.35));
#78232=CARTESIAN_POINT('Ctrl Pts',(170.420941252261,3.02673944830894,48.35));
#78233=CARTESIAN_POINT('Ctrl Pts',(170.420941252261,2.48499327898026,48.35));
#78234=CARTESIAN_POINT('Ctrl Pts',(170.860641140491,1.36248314380646,48.5));
#78235=CARTESIAN_POINT('Ctrl Pts',(170.860641140491,1.36248314380646,48.35));
#78236=CARTESIAN_POINT('Ctrl Pts',(170.542496580631,1.36248314380646,48.5));
#78237=CARTESIAN_POINT('Ctrl Pts',(170.542496580631,1.36248314380646,48.35));
#78238=CARTESIAN_POINT('Ctrl Pts',(170.360914010555,1.59058684110642,48.5));
#78239=CARTESIAN_POINT('Ctrl Pts',(170.360914010555,1.59058684110642,48.35));
#78240=CARTESIAN_POINT('',(170.860641140491,1.36248314380646,48.5));
#78241=CARTESIAN_POINT('',(170.360914010555,1.59058684110642,48.5));
#78242=CARTESIAN_POINT('Ctrl Pts',(170.860641140491,1.36248314380646,48.5));
#78243=CARTESIAN_POINT('Ctrl Pts',(170.542496580631,1.36248314380646,48.5));
#78244=CARTESIAN_POINT('Ctrl Pts',(170.360914010555,1.59058684110642,48.5));
#78245=CARTESIAN_POINT('',(170.860641140491,1.36248314380646,48.35));
#78246=CARTESIAN_POINT('',(170.860641140491,1.36248314380646,48.5));
#78247=CARTESIAN_POINT('',(170.360914010555,1.59058684110642,48.35));
#78248=CARTESIAN_POINT('Ctrl Pts',(170.860641140491,1.36248314380646,48.35));
#78249=CARTESIAN_POINT('Ctrl Pts',(170.542496580631,1.36248314380646,48.35));
#78250=CARTESIAN_POINT('Ctrl Pts',(170.360914010555,1.59058684110642,48.35));
#78251=CARTESIAN_POINT('',(170.360914010555,1.59058684110642,48.5));
#78252=CARTESIAN_POINT('Ctrl Pts',(171.260572809726,1.49229192733765,48.5));
#78253=CARTESIAN_POINT('Ctrl Pts',(171.260572809726,1.49229192733765,48.35));
#78254=CARTESIAN_POINT('Ctrl Pts',(171.102250952274,1.36248314380646,48.5));
#78255=CARTESIAN_POINT('Ctrl Pts',(171.102250952274,1.36248314380646,48.35));
#78256=CARTESIAN_POINT('Ctrl Pts',(170.860641140491,1.36248314380646,48.5));
#78257=CARTESIAN_POINT('Ctrl Pts',(170.860641140491,1.36248314380646,48.35));
#78258=CARTESIAN_POINT('',(171.260572809726,1.49229192733765,48.5));
#78259=CARTESIAN_POINT('Ctrl Pts',(171.260572809726,1.49229192733765,48.5));
#78260=CARTESIAN_POINT('Ctrl Pts',(171.102250952274,1.36248314380646,48.5));
#78261=CARTESIAN_POINT('Ctrl Pts',(170.860641140491,1.36248314380646,48.5));
#78262=CARTESIAN_POINT('',(171.260572809726,1.49229192733765,48.35));
#78263=CARTESIAN_POINT('',(171.260572809726,1.49229192733765,48.5));
#78264=CARTESIAN_POINT('Ctrl Pts',(171.260572809726,1.49229192733765,48.35));
#78265=CARTESIAN_POINT('Ctrl Pts',(171.102250952274,1.36248314380646,48.35));
#78266=CARTESIAN_POINT('Ctrl Pts',(170.860641140491,1.36248314380646,48.35));
#78267=CARTESIAN_POINT('Ctrl Pts',(171.498431105167,1.85995900630951,48.5));
#78268=CARTESIAN_POINT('Ctrl Pts',(171.498431105167,1.85995900630951,48.35));
#78269=CARTESIAN_POINT('Ctrl Pts',(171.418894667178,1.62210100889206,48.5));
#78270=CARTESIAN_POINT('Ctrl Pts',(171.418894667178,1.62210100889206,48.35));
#78271=CARTESIAN_POINT('Ctrl Pts',(171.260572809726,1.49229192733765,48.5));
#78272=CARTESIAN_POINT('Ctrl Pts',(171.260572809726,1.49229192733765,48.35));
#78273=CARTESIAN_POINT('',(171.498431105167,1.85995900630951,48.5));
#78274=CARTESIAN_POINT('Ctrl Pts',(171.498431105167,1.85995900630951,48.5));
#78275=CARTESIAN_POINT('Ctrl Pts',(171.418894667178,1.62210100889206,48.5));
#78276=CARTESIAN_POINT('Ctrl Pts',(171.260572809726,1.49229192733765,48.5));
#78277=CARTESIAN_POINT('',(171.498431105167,1.85995900630951,48.35));
#78278=CARTESIAN_POINT('',(171.498431105167,1.85995900630951,48.5));
#78279=CARTESIAN_POINT('Ctrl Pts',(171.498431105167,1.85995900630951,48.35));
#78280=CARTESIAN_POINT('Ctrl Pts',(171.418894667178,1.62210100889206,48.35));
#78281=CARTESIAN_POINT('Ctrl Pts',(171.260572809726,1.49229192733765,48.35));
#78282=CARTESIAN_POINT('Ctrl Pts',(171.577966947109,2.48499327898026,48.5));
#78283=CARTESIAN_POINT('Ctrl Pts',(171.577966947109,2.48499327898026,48.35));
#78284=CARTESIAN_POINT('Ctrl Pts',(171.577966947109,2.09781730175018,48.5));
#78285=CARTESIAN_POINT('Ctrl Pts',(171.577966947109,2.09781730175018,48.35));
#78286=CARTESIAN_POINT('Ctrl Pts',(171.498431105167,1.85995900630951,48.5));
#78287=CARTESIAN_POINT('Ctrl Pts',(171.498431105167,1.85995900630951,48.35));
#78288=CARTESIAN_POINT('',(171.577966947109,2.48499327898026,48.5));
#78289=CARTESIAN_POINT('Ctrl Pts',(171.577966947109,2.48499327898026,48.5));
#78290=CARTESIAN_POINT('Ctrl Pts',(171.577966947109,2.09781730175018,48.5));
#78291=CARTESIAN_POINT('Ctrl Pts',(171.498431105167,1.85995900630951,48.5));
#78292=CARTESIAN_POINT('',(171.577966947109,2.48499327898026,48.35));
#78293=CARTESIAN_POINT('',(171.577966947109,2.48499327898026,48.5));
#78294=CARTESIAN_POINT('Ctrl Pts',(171.577966947109,2.48499327898026,48.35));
#78295=CARTESIAN_POINT('Ctrl Pts',(171.577966947109,2.09781730175018,48.35));
#78296=CARTESIAN_POINT('Ctrl Pts',(171.498431105167,1.85995900630951,48.35));
#78297=CARTESIAN_POINT('Ctrl Pts',(171.528444427997,3.00497958064079,48.5));
#78298=CARTESIAN_POINT('Ctrl Pts',(171.528444427997,3.00497958064079,48.35));
#78299=CARTESIAN_POINT('Ctrl Pts',(171.577966947109,2.81214186549187,48.5));
#78300=CARTESIAN_POINT('Ctrl Pts',(171.577966947109,2.81214186549187,48.35));
#78301=CARTESIAN_POINT('Ctrl Pts',(171.577966947109,2.48499327898026,48.5));
#78302=CARTESIAN_POINT('Ctrl Pts',(171.577966947109,2.48499327898026,48.35));
#78303=CARTESIAN_POINT('',(171.528444427997,3.00497958064079,48.5));
#78304=CARTESIAN_POINT('Ctrl Pts',(171.528444427997,3.00497958064079,48.5));
#78305=CARTESIAN_POINT('Ctrl Pts',(171.577966947109,2.81214186549187,48.5));
#78306=CARTESIAN_POINT('Ctrl Pts',(171.577966947109,2.48499327898026,48.5));
#78307=CARTESIAN_POINT('',(171.528444427997,3.00497958064079,48.35));
#78308=CARTESIAN_POINT('',(171.528444427997,3.00497958064079,48.5));
#78309=CARTESIAN_POINT('Ctrl Pts',(171.528444427997,3.00497958064079,48.35));
#78310=CARTESIAN_POINT('Ctrl Pts',(171.577966947109,2.81214186549187,48.35));
#78311=CARTESIAN_POINT('Ctrl Pts',(171.577966947109,2.48499327898026,48.35));
#78312=CARTESIAN_POINT('Ctrl Pts',(171.391882438213,3.33212831616402,48.5));
#78313=CARTESIAN_POINT('Ctrl Pts',(171.391882438213,3.33212831616402,48.35));
#78314=CARTESIAN_POINT('Ctrl Pts',(171.478921908885,3.19781729578972,48.5));
#78315=CARTESIAN_POINT('Ctrl Pts',(171.478921908885,3.19781729578972,48.35));
#78316=CARTESIAN_POINT('Ctrl Pts',(171.528444427997,3.00497958064079,48.5));
#78317=CARTESIAN_POINT('Ctrl Pts',(171.528444427997,3.00497958064079,48.35));
#78318=CARTESIAN_POINT('',(171.391882438213,3.33212831616402,48.5));
#78319=CARTESIAN_POINT('Ctrl Pts',(171.391882438213,3.33212831616402,48.5));
#78320=CARTESIAN_POINT('Ctrl Pts',(171.478921908885,3.19781729578972,48.5));
#78321=CARTESIAN_POINT('Ctrl Pts',(171.528444427997,3.00497958064079,48.5));
#78322=CARTESIAN_POINT('',(171.391882438213,3.33212831616402,48.35));
#78323=CARTESIAN_POINT('',(171.391882438213,3.33212831616402,48.5));
#78324=CARTESIAN_POINT('Ctrl Pts',(171.391882438213,3.33212831616402,48.35));
#78325=CARTESIAN_POINT('Ctrl Pts',(171.478921908885,3.19781729578972,48.35));
#78326=CARTESIAN_POINT('Ctrl Pts',(171.528444427997,3.00497958064079,48.35));
#78327=CARTESIAN_POINT('Ctrl Pts',(171.171282667667,3.5377217233181,48.5));
#78328=CARTESIAN_POINT('Ctrl Pts',(171.171282667667,3.5377217233181,48.35));
#78329=CARTESIAN_POINT('Ctrl Pts',(171.30484296754,3.46643933653831,48.5));
#78330=CARTESIAN_POINT('Ctrl Pts',(171.30484296754,3.46643933653831,48.35));
#78331=CARTESIAN_POINT('Ctrl Pts',(171.391882438213,3.33212831616402,48.5));
#78332=CARTESIAN_POINT('Ctrl Pts',(171.391882438213,3.33212831616402,48.35));
#78333=CARTESIAN_POINT('',(171.171282667667,3.5377217233181,48.5));
#78334=CARTESIAN_POINT('Ctrl Pts',(171.171282667667,3.5377217233181,48.5));
#78335=CARTESIAN_POINT('Ctrl Pts',(171.30484296754,3.46643933653831,48.5));
#78336=CARTESIAN_POINT('Ctrl Pts',(171.391882438213,3.33212831616402,48.5));
#78337=CARTESIAN_POINT('',(171.171282667667,3.5377217233181,48.35));
#78338=CARTESIAN_POINT('',(171.171282667667,3.5377217233181,48.5));
#78339=CARTESIAN_POINT('Ctrl Pts',(171.171282667667,3.5377217233181,48.35));
#78340=CARTESIAN_POINT('Ctrl Pts',(171.30484296754,3.46643933653831,48.35));
#78341=CARTESIAN_POINT('Ctrl Pts',(171.391882438213,3.33212831616402,48.35));
#78342=CARTESIAN_POINT('Ctrl Pts',(170.860641140491,3.60900411009789,48.5));
#78343=CARTESIAN_POINT('Ctrl Pts',(170.860641140491,3.60900411009789,48.35));
#78344=CARTESIAN_POINT('Ctrl Pts',(171.037721771747,3.60900411009789,48.5));
#78345=CARTESIAN_POINT('Ctrl Pts',(171.037721771747,3.60900411009789,48.35));
#78346=CARTESIAN_POINT('Ctrl Pts',(171.171282667667,3.5377217233181,48.5));
#78347=CARTESIAN_POINT('Ctrl Pts',(171.171282667667,3.5377217233181,48.35));
#78348=CARTESIAN_POINT('',(170.860641140491,3.60900411009789,48.5));
#78349=CARTESIAN_POINT('Ctrl Pts',(170.860641140491,3.60900411009789,48.5));
#78350=CARTESIAN_POINT('Ctrl Pts',(171.037721771747,3.60900411009789,48.5));
#78351=CARTESIAN_POINT('Ctrl Pts',(171.171282667667,3.5377217233181,48.5));
#78352=CARTESIAN_POINT('',(170.860641140491,3.60900411009789,48.35));
#78353=CARTESIAN_POINT('',(170.860641140491,3.60900411009789,48.5));
#78354=CARTESIAN_POINT('Ctrl Pts',(170.860641140491,3.60900411009789,48.35));
#78355=CARTESIAN_POINT('Ctrl Pts',(171.037721771747,3.60900411009789,48.35));
#78356=CARTESIAN_POINT('Ctrl Pts',(171.171282667667,3.5377217233181,48.35));
#78357=CARTESIAN_POINT('Ctrl Pts',(170.462210316211,3.47994545102119,48.5));
#78358=CARTESIAN_POINT('Ctrl Pts',(170.462210316211,3.47994545102119,48.35));
#78359=CARTESIAN_POINT('Ctrl Pts',(170.620532173663,3.60900411009789,48.5));
#78360=CARTESIAN_POINT('Ctrl Pts',(170.620532173663,3.60900411009789,48.35));
#78361=CARTESIAN_POINT('Ctrl Pts',(170.860641140491,3.60900411009789,48.5));
#78362=CARTESIAN_POINT('Ctrl Pts',(170.860641140491,3.60900411009789,48.35));
#78363=CARTESIAN_POINT('',(170.462210316211,3.47994545102119,48.5));
#78364=CARTESIAN_POINT('Ctrl Pts',(170.462210316211,3.47994545102119,48.5));
#78365=CARTESIAN_POINT('Ctrl Pts',(170.620532173663,3.60900411009789,48.5));
#78366=CARTESIAN_POINT('Ctrl Pts',(170.860641140491,3.60900411009789,48.5));
#78367=CARTESIAN_POINT('',(170.462210316211,3.47994545102119,48.35));
#78368=CARTESIAN_POINT('',(170.462210316211,3.47994545102119,48.5));
#78369=CARTESIAN_POINT('Ctrl Pts',(170.462210316211,3.47994545102119,48.35));
#78370=CARTESIAN_POINT('Ctrl Pts',(170.620532173663,3.60900411009789,48.35));
#78371=CARTESIAN_POINT('Ctrl Pts',(170.860641140491,3.60900411009789,48.35));
#78372=CARTESIAN_POINT('Ctrl Pts',(170.223601598293,3.11302864551544,48.5));
#78373=CARTESIAN_POINT('Ctrl Pts',(170.223601598293,3.11302864551544,48.35));
#78374=CARTESIAN_POINT('Ctrl Pts',(170.303888160735,3.3508867919445,48.5));
#78375=CARTESIAN_POINT('Ctrl Pts',(170.303888160735,3.3508867919445,48.35));
#78376=CARTESIAN_POINT('Ctrl Pts',(170.462210316211,3.47994545102119,48.5));
#78377=CARTESIAN_POINT('Ctrl Pts',(170.462210316211,3.47994545102119,48.35));
#78378=CARTESIAN_POINT('',(170.223601598293,3.11302864551544,48.5));
#78379=CARTESIAN_POINT('Ctrl Pts',(170.223601598293,3.11302864551544,48.5));
#78380=CARTESIAN_POINT('Ctrl Pts',(170.303888160735,3.3508867919445,48.5));
#78381=CARTESIAN_POINT('Ctrl Pts',(170.462210316211,3.47994545102119,48.5));
#78382=CARTESIAN_POINT('',(170.223601598293,3.11302864551544,48.35));
#78383=CARTESIAN_POINT('',(170.223601598293,3.11302864551544,48.5));
#78384=CARTESIAN_POINT('Ctrl Pts',(170.223601598293,3.11302864551544,48.35));
#78385=CARTESIAN_POINT('Ctrl Pts',(170.303888160735,3.3508867919445,48.35));
#78386=CARTESIAN_POINT('Ctrl Pts',(170.462210316211,3.47994545102119,48.35));
#78387=CARTESIAN_POINT('Ctrl Pts',(170.143315333873,2.48499327898026,48.5));
#78388=CARTESIAN_POINT('Ctrl Pts',(170.143315333873,2.48499327898026,48.35));
#78389=CARTESIAN_POINT('Ctrl Pts',(170.143315333873,2.87517049908638,48.5));
#78390=CARTESIAN_POINT('Ctrl Pts',(170.143315333873,2.87517049908638,48.35));
#78391=CARTESIAN_POINT('Ctrl Pts',(170.223601598293,3.11302864551544,48.5));
#78392=CARTESIAN_POINT('Ctrl Pts',(170.223601598293,3.11302864551544,48.35));
#78393=CARTESIAN_POINT('',(170.143315333873,2.48499327898026,48.5));
#78394=CARTESIAN_POINT('Ctrl Pts',(170.143315333873,2.48499327898026,48.5));
#78395=CARTESIAN_POINT('Ctrl Pts',(170.143315333873,2.87517049908638,48.5));
#78396=CARTESIAN_POINT('Ctrl Pts',(170.223601598293,3.11302864551544,48.5));
#78397=CARTESIAN_POINT('',(170.143315333873,2.48499327898026,48.35));
#78398=CARTESIAN_POINT('',(170.143315333873,2.48499327898026,48.5));
#78399=CARTESIAN_POINT('Ctrl Pts',(170.143315333873,2.48499327898026,48.35));
#78400=CARTESIAN_POINT('Ctrl Pts',(170.143315333873,2.87517049908638,48.35));
#78401=CARTESIAN_POINT('Ctrl Pts',(170.223601598293,3.11302864551544,48.35));
#78402=CARTESIAN_POINT('Ctrl Pts',(170.360914010555,1.59058684110642,48.5));
#78403=CARTESIAN_POINT('Ctrl Pts',(170.360914010555,1.59058684110642,48.35));
#78404=CARTESIAN_POINT('Ctrl Pts',(170.143315333873,1.86521166563034,48.5));
#78405=CARTESIAN_POINT('Ctrl Pts',(170.143315333873,1.86521166563034,48.35));
#78406=CARTESIAN_POINT('Ctrl Pts',(170.143315333873,2.48499327898026,48.5));
#78407=CARTESIAN_POINT('Ctrl Pts',(170.143315333873,2.48499327898026,48.35));
#78408=CARTESIAN_POINT('Ctrl Pts',(170.360914010555,1.59058684110642,48.5));
#78409=CARTESIAN_POINT('Ctrl Pts',(170.143315333873,1.86521166563034,48.5));
#78410=CARTESIAN_POINT('Ctrl Pts',(170.143315333873,2.48499327898026,48.5));
#78411=CARTESIAN_POINT('Ctrl Pts',(170.360914010555,1.59058684110642,48.35));
#78412=CARTESIAN_POINT('Ctrl Pts',(170.143315333873,1.86521166563034,48.35));
#78413=CARTESIAN_POINT('Ctrl Pts',(170.143315333873,2.48499327898026,48.35));
#78414=CARTESIAN_POINT('Origin',(169.999999914318,2.48574362695217,48.35));
#78415=CARTESIAN_POINT('Ctrl Pts',(169.170873302966,2.58854025602341,48.5));
#78416=CARTESIAN_POINT('Ctrl Pts',(169.170873302966,2.58854025602341,48.35));
#78417=CARTESIAN_POINT('Ctrl Pts',(168.987790036947,2.58854025602341,48.5));
#78418=CARTESIAN_POINT('Ctrl Pts',(168.987790036947,2.58854025602341,48.35));
#78419=CARTESIAN_POINT('Ctrl Pts',(168.860232073814,2.45723062753677,48.5));
#78420=CARTESIAN_POINT('Ctrl Pts',(168.860232073814,2.45723062753677,48.35));
#78421=CARTESIAN_POINT('',(169.170873302966,2.58854025602341,48.5));
#78422=CARTESIAN_POINT('',(168.860232073814,2.45723062753677,48.5));
#78423=CARTESIAN_POINT('Ctrl Pts',(169.170873302966,2.58854025602341,48.5));
#78424=CARTESIAN_POINT('Ctrl Pts',(168.987790036947,2.58854025602341,48.5));
#78425=CARTESIAN_POINT('Ctrl Pts',(168.860232073814,2.45723062753677,48.5));
#78426=CARTESIAN_POINT('',(169.170873302966,2.58854025602341,48.35));
#78427=CARTESIAN_POINT('',(169.170873302966,2.58854025602341,48.5));
#78428=CARTESIAN_POINT('',(168.860232073814,2.45723062753677,48.35));
#78429=CARTESIAN_POINT('Ctrl Pts',(169.170873302966,2.58854025602341,48.35));
#78430=CARTESIAN_POINT('Ctrl Pts',(168.987790036947,2.58854025602341,48.35));
#78431=CARTESIAN_POINT('Ctrl Pts',(168.860232073814,2.45723062753677,48.35));
#78432=CARTESIAN_POINT('',(168.860232073814,2.45723062753677,48.5));
#78433=CARTESIAN_POINT('Ctrl Pts',(169.477012295276,2.45723062753677,48.5));
#78434=CARTESIAN_POINT('Ctrl Pts',(169.477012295276,2.45723062753677,48.35));
#78435=CARTESIAN_POINT('Ctrl Pts',(169.35545726493,2.58854025602341,48.5));
#78436=CARTESIAN_POINT('Ctrl Pts',(169.35545726493,2.58854025602341,48.35));
#78437=CARTESIAN_POINT('Ctrl Pts',(169.170873302966,2.58854025602341,48.5));
#78438=CARTESIAN_POINT('Ctrl Pts',(169.170873302966,2.58854025602341,48.35));
#78439=CARTESIAN_POINT('',(169.477012295276,2.45723062753677,48.5));
#78440=CARTESIAN_POINT('Ctrl Pts',(169.477012295276,2.45723062753677,48.5));
#78441=CARTESIAN_POINT('Ctrl Pts',(169.35545726493,2.58854025602341,48.5));
#78442=CARTESIAN_POINT('Ctrl Pts',(169.170873302966,2.58854025602341,48.5));
#78443=CARTESIAN_POINT('',(169.477012295276,2.45723062753677,48.35));
#78444=CARTESIAN_POINT('',(169.477012295276,2.45723062753677,48.5));
#78445=CARTESIAN_POINT('Ctrl Pts',(169.477012295276,2.45723062753677,48.35));
#78446=CARTESIAN_POINT('Ctrl Pts',(169.35545726493,2.58854025602341,48.35));
#78447=CARTESIAN_POINT('Ctrl Pts',(169.170873302966,2.58854025602341,48.35));
#78448=CARTESIAN_POINT('Ctrl Pts',(169.598567623645,2.09781730175018,48.5));
#78449=CARTESIAN_POINT('Ctrl Pts',(169.598567623645,2.09781730175018,48.35));
#78450=CARTESIAN_POINT('Ctrl Pts',(169.598567623645,2.32592099905014,48.5));
#78451=CARTESIAN_POINT('Ctrl Pts',(169.598567623645,2.32592099905014,48.35));
#78452=CARTESIAN_POINT('Ctrl Pts',(169.477012295276,2.45723062753677,48.5));
#78453=CARTESIAN_POINT('Ctrl Pts',(169.477012295276,2.45723062753677,48.35));
#78454=CARTESIAN_POINT('',(169.598567623645,2.09781730175018,48.5));
#78455=CARTESIAN_POINT('Ctrl Pts',(169.598567623645,2.09781730175018,48.5));
#78456=CARTESIAN_POINT('Ctrl Pts',(169.598567623645,2.32592099905014,48.5));
#78457=CARTESIAN_POINT('Ctrl Pts',(169.477012295276,2.45723062753677,48.5));
#78458=CARTESIAN_POINT('',(169.598567623645,2.09781730175018,48.35));
#78459=CARTESIAN_POINT('',(169.598567623645,2.09781730175018,48.5));
#78460=CARTESIAN_POINT('Ctrl Pts',(169.598567623645,2.09781730175018,48.35));
#78461=CARTESIAN_POINT('Ctrl Pts',(169.598567623645,2.32592099905014,48.35));
#78462=CARTESIAN_POINT('Ctrl Pts',(169.477012295276,2.45723062753677,48.35));
#78463=CARTESIAN_POINT('Ctrl Pts',(169.475511748344,1.72264659404755,48.5));
#78464=CARTESIAN_POINT('Ctrl Pts',(169.475511748344,1.72264659404755,48.35));
#78465=CARTESIAN_POINT('Ctrl Pts',(169.598567623645,1.86070942878723,48.5));
#78466=CARTESIAN_POINT('Ctrl Pts',(169.598567623645,1.86070942878723,48.35));
#78467=CARTESIAN_POINT('Ctrl Pts',(169.598567623645,2.09781730175018,48.5));
#78468=CARTESIAN_POINT('Ctrl Pts',(169.598567623645,2.09781730175018,48.35));
#78469=CARTESIAN_POINT('',(169.475511748344,1.72264659404755,48.5));
#78470=CARTESIAN_POINT('Ctrl Pts',(169.475511748344,1.72264659404755,48.5));
#78471=CARTESIAN_POINT('Ctrl Pts',(169.598567623645,1.86070942878723,48.5));
#78472=CARTESIAN_POINT('Ctrl Pts',(169.598567623645,2.09781730175018,48.5));
#78473=CARTESIAN_POINT('',(169.475511748344,1.72264659404755,48.35));
#78474=CARTESIAN_POINT('',(169.475511748344,1.72264659404755,48.5));
#78475=CARTESIAN_POINT('Ctrl Pts',(169.475511748344,1.72264659404755,48.35));
#78476=CARTESIAN_POINT('Ctrl Pts',(169.598567623645,1.86070942878723,48.35));
#78477=CARTESIAN_POINT('Ctrl Pts',(169.598567623645,2.09781730175018,48.35));
#78478=CARTESIAN_POINT('Ctrl Pts',(169.181378025562,1.58458405733109,48.5));
#78479=CARTESIAN_POINT('Ctrl Pts',(169.181378025562,1.58458405733109,48.35));
#78480=CARTESIAN_POINT('Ctrl Pts',(169.352455873042,1.58458405733109,48.5));
#78481=CARTESIAN_POINT('Ctrl Pts',(169.352455873042,1.58458405733109,48.35));
#78482=CARTESIAN_POINT('Ctrl Pts',(169.475511748344,1.72264659404755,48.5));
#78483=CARTESIAN_POINT('Ctrl Pts',(169.475511748344,1.72264659404755,48.35));
#78484=CARTESIAN_POINT('',(169.181378025562,1.58458405733109,48.5));
#78485=CARTESIAN_POINT('Ctrl Pts',(169.181378025562,1.58458405733109,48.5));
#78486=CARTESIAN_POINT('Ctrl Pts',(169.352455873042,1.58458405733109,48.5));
#78487=CARTESIAN_POINT('Ctrl Pts',(169.475511748344,1.72264659404755,48.5));
#78488=CARTESIAN_POINT('',(169.181378025562,1.58458405733109,48.35));
#78489=CARTESIAN_POINT('',(169.181378025562,1.58458405733109,48.5));
#78490=CARTESIAN_POINT('Ctrl Pts',(169.181378025562,1.58458405733109,48.35));
#78491=CARTESIAN_POINT('Ctrl Pts',(169.352455873042,1.58458405733109,48.35));
#78492=CARTESIAN_POINT('Ctrl Pts',(169.475511748344,1.72264659404755,48.35));
#78493=CARTESIAN_POINT('Ctrl Pts',(168.957776416093,1.65136420726776,48.5));
#78494=CARTESIAN_POINT('Ctrl Pts',(168.957776416093,1.65136420726776,48.35));
#78495=CARTESIAN_POINT('Ctrl Pts',(169.064324934036,1.58458405733109,48.5));
#78496=CARTESIAN_POINT('Ctrl Pts',(169.064324934036,1.58458405733109,48.35));
#78497=CARTESIAN_POINT('Ctrl Pts',(169.181378025562,1.58458405733109,48.5));
#78498=CARTESIAN_POINT('Ctrl Pts',(169.181378025562,1.58458405733109,48.35));
#78499=CARTESIAN_POINT('',(168.957776416093,1.65136420726776,48.5));
#78500=CARTESIAN_POINT('Ctrl Pts',(168.957776416093,1.65136420726776,48.5));
#78501=CARTESIAN_POINT('Ctrl Pts',(169.064324934036,1.58458405733109,48.5));
#78502=CARTESIAN_POINT('Ctrl Pts',(169.181378025562,1.58458405733109,48.5));
#78503=CARTESIAN_POINT('',(168.957776416093,1.65136420726776,48.35));
#78504=CARTESIAN_POINT('',(168.957776416093,1.65136420726776,48.5));
#78505=CARTESIAN_POINT('Ctrl Pts',(168.957776416093,1.65136420726776,48.35));
#78506=CARTESIAN_POINT('Ctrl Pts',(169.064324934036,1.58458405733109,48.35));
#78507=CARTESIAN_POINT('Ctrl Pts',(169.181378025562,1.58458405733109,48.35));
#78508=CARTESIAN_POINT('Ctrl Pts',(168.791951078922,1.84570276737213,48.5));
#78509=CARTESIAN_POINT('Ctrl Pts',(168.791951078922,1.84570276737213,48.35));
#78510=CARTESIAN_POINT('Ctrl Pts',(168.851227898151,1.71814465522766,48.5));
#78511=CARTESIAN_POINT('Ctrl Pts',(168.851227898151,1.71814465522766,48.35));
#78512=CARTESIAN_POINT('Ctrl Pts',(168.957776416093,1.65136420726776,48.5));
#78513=CARTESIAN_POINT('Ctrl Pts',(168.957776416093,1.65136420726776,48.35));
#78514=CARTESIAN_POINT('',(168.791951078922,1.84570276737213,48.5));
#78515=CARTESIAN_POINT('Ctrl Pts',(168.791951078922,1.84570276737213,48.5));
#78516=CARTESIAN_POINT('Ctrl Pts',(168.851227898151,1.71814465522766,48.5));
#78517=CARTESIAN_POINT('Ctrl Pts',(168.957776416093,1.65136420726776,48.5));
#78518=CARTESIAN_POINT('',(168.791951078922,1.84570276737213,48.35));
#78519=CARTESIAN_POINT('',(168.791951078922,1.84570276737213,48.5));
#78520=CARTESIAN_POINT('Ctrl Pts',(168.791951078922,1.84570276737213,48.35));
#78521=CARTESIAN_POINT('Ctrl Pts',(168.851227898151,1.71814465522766,48.35));
#78522=CARTESIAN_POINT('Ctrl Pts',(168.957776416093,1.65136420726776,48.35));
#78523=CARTESIAN_POINT('Ctrl Pts',(168.732673961669,2.1128241121769,48.5));
#78524=CARTESIAN_POINT('Ctrl Pts',(168.732673961669,2.1128241121769,48.35));
#78525=CARTESIAN_POINT('Ctrl Pts',(168.732673961669,1.97326058149338,48.5));
#78526=CARTESIAN_POINT('Ctrl Pts',(168.732673961669,1.97326058149338,48.35));
#78527=CARTESIAN_POINT('Ctrl Pts',(168.791951078922,1.84570276737213,48.5));
#78528=CARTESIAN_POINT('Ctrl Pts',(168.791951078922,1.84570276737213,48.35));
#78529=CARTESIAN_POINT('',(168.732673961669,2.1128241121769,48.5));
#78530=CARTESIAN_POINT('Ctrl Pts',(168.732673961669,2.1128241121769,48.5));
#78531=CARTESIAN_POINT('Ctrl Pts',(168.732673961669,1.97326058149338,48.5));
#78532=CARTESIAN_POINT('Ctrl Pts',(168.791951078922,1.84570276737213,48.5));
#78533=CARTESIAN_POINT('',(168.732673961669,2.1128241121769,48.35));
#78534=CARTESIAN_POINT('',(168.732673961669,2.1128241121769,48.5));
#78535=CARTESIAN_POINT('Ctrl Pts',(168.732673961669,2.1128241121769,48.35));
#78536=CARTESIAN_POINT('Ctrl Pts',(168.732673961669,1.97326058149338,48.35));
#78537=CARTESIAN_POINT('Ctrl Pts',(168.791951078922,1.84570276737213,48.35));
#78538=CARTESIAN_POINT('Ctrl Pts',(168.860232073814,2.45723062753677,48.5));
#78539=CARTESIAN_POINT('Ctrl Pts',(168.860232073814,2.45723062753677,48.35));
#78540=CARTESIAN_POINT('Ctrl Pts',(168.732673961669,2.32592099905014,48.5));
#78541=CARTESIAN_POINT('Ctrl Pts',(168.732673961669,2.32592099905014,48.35));
#78542=CARTESIAN_POINT('Ctrl Pts',(168.732673961669,2.1128241121769,48.5));
#78543=CARTESIAN_POINT('Ctrl Pts',(168.732673961669,2.1128241121769,48.35));
#78544=CARTESIAN_POINT('Ctrl Pts',(168.860232073814,2.45723062753677,48.5));
#78545=CARTESIAN_POINT('Ctrl Pts',(168.732673961669,2.32592099905014,48.5));
#78546=CARTESIAN_POINT('Ctrl Pts',(168.732673961669,2.1128241121769,48.5));
#78547=CARTESIAN_POINT('Ctrl Pts',(168.860232073814,2.45723062753677,48.35));
#78548=CARTESIAN_POINT('Ctrl Pts',(168.732673961669,2.32592099905014,48.35));
#78549=CARTESIAN_POINT('Ctrl Pts',(168.732673961669,2.1128241121769,48.35));
#78550=CARTESIAN_POINT('Ctrl Pts',(169.211391646415,3.60900411009789,48.5));
#78551=CARTESIAN_POINT('Ctrl Pts',(169.211391646415,3.60900411009789,48.35));
#78552=CARTESIAN_POINT('Ctrl Pts',(169.471009511501,3.60900411009789,48.5));
#78553=CARTESIAN_POINT('Ctrl Pts',(169.471009511501,3.60900411009789,48.35));
#78554=CARTESIAN_POINT('Ctrl Pts',(169.636834997684,3.46343794465065,48.5));
#78555=CARTESIAN_POINT('Ctrl Pts',(169.636834997684,3.46343794465065,48.35));
#78556=CARTESIAN_POINT('',(169.211391646415,3.60900411009789,48.5));
#78557=CARTESIAN_POINT('',(169.636834997684,3.46343794465065,48.5));
#78558=CARTESIAN_POINT('Ctrl Pts',(169.211391646415,3.60900411009789,48.5));
#78559=CARTESIAN_POINT('Ctrl Pts',(169.471009511501,3.60900411009789,48.5));
#78560=CARTESIAN_POINT('Ctrl Pts',(169.636834997684,3.46343794465065,48.5));
#78561=CARTESIAN_POINT('',(169.211391646415,3.60900411009789,48.35));
#78562=CARTESIAN_POINT('',(169.211391646415,3.60900411009789,48.5));
#78563=CARTESIAN_POINT('',(169.636834997684,3.46343794465065,48.35));
#78564=CARTESIAN_POINT('Ctrl Pts',(169.211391646415,3.60900411009789,48.35));
#78565=CARTESIAN_POINT('Ctrl Pts',(169.471009511501,3.60900411009789,48.35));
#78566=CARTESIAN_POINT('Ctrl Pts',(169.636834997684,3.46343794465065,48.35));
#78567=CARTESIAN_POINT('',(169.636834997684,3.46343794465065,48.5));
#78568=CARTESIAN_POINT('Ctrl Pts',(168.657639909536,3.35688957571983,48.5));
#78569=CARTESIAN_POINT('Ctrl Pts',(168.657639909536,3.35688957571983,48.35));
#78570=CARTESIAN_POINT('Ctrl Pts',(168.863233465701,3.60900411009789,48.5));
#78571=CARTESIAN_POINT('Ctrl Pts',(168.863233465701,3.60900411009789,48.35));
#78572=CARTESIAN_POINT('Ctrl Pts',(169.211391646415,3.60900411009789,48.5));
#78573=CARTESIAN_POINT('Ctrl Pts',(169.211391646415,3.60900411009789,48.35));
#78574=CARTESIAN_POINT('',(168.657639909536,3.35688957571983,48.5));
#78575=CARTESIAN_POINT('Ctrl Pts',(168.657639909536,3.35688957571983,48.5));
#78576=CARTESIAN_POINT('Ctrl Pts',(168.863233465701,3.60900411009789,48.5));
#78577=CARTESIAN_POINT('Ctrl Pts',(169.211391646415,3.60900411009789,48.5));
#78578=CARTESIAN_POINT('',(168.657639909536,3.35688957571983,48.35));
#78579=CARTESIAN_POINT('',(168.657639909536,3.35688957571983,48.5));
#78580=CARTESIAN_POINT('Ctrl Pts',(168.657639909536,3.35688957571983,48.35));
#78581=CARTESIAN_POINT('Ctrl Pts',(168.863233465701,3.60900411009789,48.35));
#78582=CARTESIAN_POINT('Ctrl Pts',(169.211391646415,3.60900411009789,48.35));
#78583=CARTESIAN_POINT('Ctrl Pts',(168.422032881528,2.42946797609329,48.5));
#78584=CARTESIAN_POINT('Ctrl Pts',(168.422032881528,2.42946797609329,48.35));
#78585=CARTESIAN_POINT('Ctrl Pts',(168.422032881528,3.0672579407692,48.5));
#78586=CARTESIAN_POINT('Ctrl Pts',(168.422032881528,3.0672579407692,48.35));
#78587=CARTESIAN_POINT('Ctrl Pts',(168.657639909536,3.35688957571983,48.5));
#78588=CARTESIAN_POINT('Ctrl Pts',(168.657639909536,3.35688957571983,48.35));
#78589=CARTESIAN_POINT('',(168.422032881528,2.42946797609329,48.5));
#78590=CARTESIAN_POINT('Ctrl Pts',(168.422032881528,2.42946797609329,48.5));
#78591=CARTESIAN_POINT('Ctrl Pts',(168.422032881528,3.0672579407692,48.5));
#78592=CARTESIAN_POINT('Ctrl Pts',(168.657639909536,3.35688957571983,48.5));
#78593=CARTESIAN_POINT('',(168.422032881528,2.42946797609329,48.35));
#78594=CARTESIAN_POINT('',(168.422032881528,2.42946797609329,48.5));
#78595=CARTESIAN_POINT('Ctrl Pts',(168.422032881528,2.42946797609329,48.35));
#78596=CARTESIAN_POINT('Ctrl Pts',(168.422032881528,3.0672579407692,48.35));
#78597=CARTESIAN_POINT('Ctrl Pts',(168.657639909536,3.35688957571983,48.35));
#78598=CARTESIAN_POINT('Ctrl Pts',(168.635129768401,1.61084586381912,48.5));
#78599=CARTESIAN_POINT('Ctrl Pts',(168.635129768401,1.61084586381912,48.35));
#78600=CARTESIAN_POINT('Ctrl Pts',(168.422032881528,1.85920888185501,48.5));
#78601=CARTESIAN_POINT('Ctrl Pts',(168.422032881528,1.85920888185501,48.35));
#78602=CARTESIAN_POINT('Ctrl Pts',(168.422032881528,2.42946797609329,48.5));
#78603=CARTESIAN_POINT('Ctrl Pts',(168.422032881528,2.42946797609329,48.35));
#78604=CARTESIAN_POINT('',(168.635129768401,1.61084586381912,48.5));
#78605=CARTESIAN_POINT('Ctrl Pts',(168.635129768401,1.61084586381912,48.5));
#78606=CARTESIAN_POINT('Ctrl Pts',(168.422032881528,1.85920888185501,48.5));
#78607=CARTESIAN_POINT('Ctrl Pts',(168.422032881528,2.42946797609329,48.5));
#78608=CARTESIAN_POINT('',(168.635129768401,1.61084586381912,48.35));
#78609=CARTESIAN_POINT('',(168.635129768401,1.61084586381912,48.5));
#78610=CARTESIAN_POINT('Ctrl Pts',(168.635129768401,1.61084586381912,48.35));
#78611=CARTESIAN_POINT('Ctrl Pts',(168.422032881528,1.85920888185501,48.35));
#78612=CARTESIAN_POINT('Ctrl Pts',(168.422032881528,2.42946797609329,48.35));
#78613=CARTESIAN_POINT('Ctrl Pts',(169.185880113393,1.36248314380646,48.5));
#78614=CARTESIAN_POINT('Ctrl Pts',(169.185880113393,1.36248314380646,48.35));
#78615=CARTESIAN_POINT('Ctrl Pts',(168.848226506263,1.36248314380646,48.5));
#78616=CARTESIAN_POINT('Ctrl Pts',(168.848226506263,1.36248314380646,48.35));
#78617=CARTESIAN_POINT('Ctrl Pts',(168.635129768401,1.61084586381912,48.5));
#78618=CARTESIAN_POINT('Ctrl Pts',(168.635129768401,1.61084586381912,48.35));
#78619=CARTESIAN_POINT('',(169.185880113393,1.36248314380646,48.5));
#78620=CARTESIAN_POINT('Ctrl Pts',(169.185880113393,1.36248314380646,48.5));
#78621=CARTESIAN_POINT('Ctrl Pts',(168.848226506263,1.36248314380646,48.5));
#78622=CARTESIAN_POINT('Ctrl Pts',(168.635129768401,1.61084586381912,48.5));
#78623=CARTESIAN_POINT('',(169.185880113393,1.36248314380646,48.35));
#78624=CARTESIAN_POINT('',(169.185880113393,1.36248314380646,48.5));
#78625=CARTESIAN_POINT('Ctrl Pts',(169.185880113393,1.36248314380646,48.35));
#78626=CARTESIAN_POINT('Ctrl Pts',(168.848226506263,1.36248314380646,48.35));
#78627=CARTESIAN_POINT('Ctrl Pts',(168.635129768401,1.61084586381912,48.35));
#78628=CARTESIAN_POINT('Ctrl Pts',(169.540041226894,1.45702594518662,48.5));
#78629=CARTESIAN_POINT('Ctrl Pts',(169.540041226894,1.45702594518662,48.35));
#78630=CARTESIAN_POINT('Ctrl Pts',(169.383970040828,1.36248314380646,48.5));
#78631=CARTESIAN_POINT('Ctrl Pts',(169.383970040828,1.36248314380646,48.35));
#78632=CARTESIAN_POINT('Ctrl Pts',(169.185880113393,1.36248314380646,48.5));
#78633=CARTESIAN_POINT('Ctrl Pts',(169.185880113393,1.36248314380646,48.35));
#78634=CARTESIAN_POINT('',(169.540041226894,1.45702594518662,48.5));
#78635=CARTESIAN_POINT('Ctrl Pts',(169.540041226894,1.45702594518662,48.5));
#78636=CARTESIAN_POINT('Ctrl Pts',(169.383970040828,1.36248314380646,48.5));
#78637=CARTESIAN_POINT('Ctrl Pts',(169.185880113393,1.36248314380646,48.5));
#78638=CARTESIAN_POINT('',(169.540041226894,1.45702594518662,48.35));
#78639=CARTESIAN_POINT('',(169.540041226894,1.45702594518662,48.5));
#78640=CARTESIAN_POINT('Ctrl Pts',(169.540041226894,1.45702594518662,48.35));
#78641=CARTESIAN_POINT('Ctrl Pts',(169.383970040828,1.36248314380646,48.35));
#78642=CARTESIAN_POINT('Ctrl Pts',(169.185880113393,1.36248314380646,48.35));
#78643=CARTESIAN_POINT('Ctrl Pts',(169.785402555019,1.7293998003006,48.5));
#78644=CARTESIAN_POINT('Ctrl Pts',(169.785402555019,1.7293998003006,48.35));
#78645=CARTESIAN_POINT('Ctrl Pts',(169.696111816913,1.55156904459,48.5));
#78646=CARTESIAN_POINT('Ctrl Pts',(169.696111816913,1.55156904459,48.35));
#78647=CARTESIAN_POINT('Ctrl Pts',(169.540041226894,1.45702594518662,48.5));
#78648=CARTESIAN_POINT('Ctrl Pts',(169.540041226894,1.45702594518662,48.35));
#78649=CARTESIAN_POINT('',(169.785402555019,1.7293998003006,48.5));
#78650=CARTESIAN_POINT('Ctrl Pts',(169.785402555019,1.7293998003006,48.5));
#78651=CARTESIAN_POINT('Ctrl Pts',(169.696111816913,1.55156904459,48.5));
#78652=CARTESIAN_POINT('Ctrl Pts',(169.540041226894,1.45702594518662,48.5));
#78653=CARTESIAN_POINT('',(169.785402555019,1.7293998003006,48.35));
#78654=CARTESIAN_POINT('',(169.785402555019,1.7293998003006,48.5));
#78655=CARTESIAN_POINT('Ctrl Pts',(169.785402555019,1.7293998003006,48.35));
#78656=CARTESIAN_POINT('Ctrl Pts',(169.696111816913,1.55156904459,48.35));
#78657=CARTESIAN_POINT('Ctrl Pts',(169.540041226894,1.45702594518662,48.35));
#78658=CARTESIAN_POINT('Ctrl Pts',(169.874693293124,2.11432480812073,48.5));
#78659=CARTESIAN_POINT('Ctrl Pts',(169.874693293124,2.11432480812073,48.35));
#78660=CARTESIAN_POINT('Ctrl Pts',(169.874693293124,1.9072305560112,48.5));
#78661=CARTESIAN_POINT('Ctrl Pts',(169.874693293124,1.9072305560112,48.35));
#78662=CARTESIAN_POINT('Ctrl Pts',(169.785402555019,1.7293998003006,48.5));
#78663=CARTESIAN_POINT('Ctrl Pts',(169.785402555019,1.7293998003006,48.35));
#78664=CARTESIAN_POINT('',(169.874693293124,2.11432480812073,48.5));
#78665=CARTESIAN_POINT('Ctrl Pts',(169.874693293124,2.11432480812073,48.5));
#78666=CARTESIAN_POINT('Ctrl Pts',(169.874693293124,1.9072305560112,48.5));
#78667=CARTESIAN_POINT('Ctrl Pts',(169.785402555019,1.7293998003006,48.5));
#78668=CARTESIAN_POINT('',(169.874693293124,2.11432480812073,48.35));
#78669=CARTESIAN_POINT('',(169.874693293124,2.11432480812073,48.5));
#78670=CARTESIAN_POINT('Ctrl Pts',(169.874693293124,2.11432480812073,48.35));
#78671=CARTESIAN_POINT('Ctrl Pts',(169.874693293124,1.9072305560112,48.35));
#78672=CARTESIAN_POINT('Ctrl Pts',(169.785402555019,1.7293998003006,48.35));
#78673=CARTESIAN_POINT('Ctrl Pts',(169.68485667184,2.62830847501755,48.5));
#78674=CARTESIAN_POINT('Ctrl Pts',(169.68485667184,2.62830847501755,48.35));
#78675=CARTESIAN_POINT('Ctrl Pts',(169.874693293124,2.42946797609329,48.5));
#78676=CARTESIAN_POINT('Ctrl Pts',(169.874693293124,2.42946797609329,48.35));
#78677=CARTESIAN_POINT('Ctrl Pts',(169.874693293124,2.11432480812073,48.5));
#78678=CARTESIAN_POINT('Ctrl Pts',(169.874693293124,2.11432480812073,48.35));
#78679=CARTESIAN_POINT('',(169.68485667184,2.62830847501755,48.5));
#78680=CARTESIAN_POINT('Ctrl Pts',(169.68485667184,2.62830847501755,48.5));
#78681=CARTESIAN_POINT('Ctrl Pts',(169.874693293124,2.42946797609329,48.5));
#78682=CARTESIAN_POINT('Ctrl Pts',(169.874693293124,2.11432480812073,48.5));
#78683=CARTESIAN_POINT('',(169.68485667184,2.62830847501755,48.35));
#78684=CARTESIAN_POINT('',(169.68485667184,2.62830847501755,48.5));
#78685=CARTESIAN_POINT('Ctrl Pts',(169.68485667184,2.62830847501755,48.35));
#78686=CARTESIAN_POINT('Ctrl Pts',(169.874693293124,2.42946797609329,48.35));
#78687=CARTESIAN_POINT('Ctrl Pts',(169.874693293124,2.11432480812073,48.35));
#78688=CARTESIAN_POINT('Ctrl Pts',(169.224897760898,2.82714867591858,48.5));
#78689=CARTESIAN_POINT('Ctrl Pts',(169.224897760898,2.82714867591858,48.35));
#78690=CARTESIAN_POINT('Ctrl Pts',(169.495020646602,2.82714867591858,48.5));
#78691=CARTESIAN_POINT('Ctrl Pts',(169.495020646602,2.82714867591858,48.35));
#78692=CARTESIAN_POINT('Ctrl Pts',(169.68485667184,2.62830847501755,48.5));
#78693=CARTESIAN_POINT('Ctrl Pts',(169.68485667184,2.62830847501755,48.35));
#78694=CARTESIAN_POINT('',(169.224897760898,2.82714867591858,48.5));
#78695=CARTESIAN_POINT('Ctrl Pts',(169.224897760898,2.82714867591858,48.5));
#78696=CARTESIAN_POINT('Ctrl Pts',(169.495020646602,2.82714867591858,48.5));
#78697=CARTESIAN_POINT('Ctrl Pts',(169.68485667184,2.62830847501755,48.5));
#78698=CARTESIAN_POINT('',(169.224897760898,2.82714867591858,48.35));
#78699=CARTESIAN_POINT('',(169.224897760898,2.82714867591858,48.5));
#78700=CARTESIAN_POINT('Ctrl Pts',(169.224897760898,2.82714867591858,48.35));
#78701=CARTESIAN_POINT('Ctrl Pts',(169.495020646602,2.82714867591858,48.35));
#78702=CARTESIAN_POINT('Ctrl Pts',(169.68485667184,2.62830847501755,48.35));
#78703=CARTESIAN_POINT('Ctrl Pts',(168.929263491184,2.75511601567268,48.5));
#78704=CARTESIAN_POINT('Ctrl Pts',(168.929263491184,2.75511601567268,48.35));
#78705=CARTESIAN_POINT('Ctrl Pts',(169.070327568799,2.82714867591858,48.5));
#78706=CARTESIAN_POINT('Ctrl Pts',(169.070327568799,2.82714867591858,48.35));
#78707=CARTESIAN_POINT('Ctrl Pts',(169.224897760898,2.82714867591858,48.5));
#78708=CARTESIAN_POINT('Ctrl Pts',(169.224897760898,2.82714867591858,48.35));
#78709=CARTESIAN_POINT('',(168.929263491184,2.75511601567268,48.5));
#78710=CARTESIAN_POINT('Ctrl Pts',(168.929263491184,2.75511601567268,48.5));
#78711=CARTESIAN_POINT('Ctrl Pts',(169.070327568799,2.82714867591858,48.5));
#78712=CARTESIAN_POINT('Ctrl Pts',(169.224897760898,2.82714867591858,48.5));
#78713=CARTESIAN_POINT('',(168.929263491184,2.75511601567268,48.35));
#78714=CARTESIAN_POINT('',(168.929263491184,2.75511601567268,48.5));
#78715=CARTESIAN_POINT('Ctrl Pts',(168.929263491184,2.75511601567268,48.35));
#78716=CARTESIAN_POINT('Ctrl Pts',(169.070327568799,2.82714867591858,48.35));
#78717=CARTESIAN_POINT('Ctrl Pts',(169.224897760898,2.82714867591858,48.35));
#78718=CARTESIAN_POINT('Ctrl Pts',(168.690654922277,2.53451579809189,48.5));
#78719=CARTESIAN_POINT('Ctrl Pts',(168.690654922277,2.53451579809189,48.35));
#78720=CARTESIAN_POINT('Ctrl Pts',(168.788199264556,2.68308320641518,48.5));
#78721=CARTESIAN_POINT('Ctrl Pts',(168.788199264556,2.68308320641518,48.35));
#78722=CARTESIAN_POINT('Ctrl Pts',(168.929263491184,2.75511601567268,48.5));
#78723=CARTESIAN_POINT('Ctrl Pts',(168.929263491184,2.75511601567268,48.35));
#78724=CARTESIAN_POINT('',(168.690654922277,2.53451579809189,48.5));
#78725=CARTESIAN_POINT('Ctrl Pts',(168.690654922277,2.53451579809189,48.5));
#78726=CARTESIAN_POINT('Ctrl Pts',(168.788199264556,2.68308320641518,48.5));
#78727=CARTESIAN_POINT('Ctrl Pts',(168.929263491184,2.75511601567268,48.5));
#78728=CARTESIAN_POINT('',(168.690654922277,2.53451579809189,48.35));
#78729=CARTESIAN_POINT('',(168.690654922277,2.53451579809189,48.5));
#78730=CARTESIAN_POINT('Ctrl Pts',(168.690654922277,2.53451579809189,48.35));
#78731=CARTESIAN_POINT('Ctrl Pts',(168.788199264556,2.68308320641518,48.35));
#78732=CARTESIAN_POINT('Ctrl Pts',(168.929263491184,2.75511601567268,48.35));
#78733=CARTESIAN_POINT('Ctrl Pts',(168.767189819366,3.04324695467949,48.5));
#78734=CARTESIAN_POINT('Ctrl Pts',(168.767189819366,3.04324695467949,48.35));
#78735=CARTESIAN_POINT('Ctrl Pts',(168.693656314164,2.86466577649117,48.5));
#78736=CARTESIAN_POINT('Ctrl Pts',(168.693656314164,2.86466577649117,48.35));
#78737=CARTESIAN_POINT('Ctrl Pts',(168.690654922277,2.53451579809189,48.5));
#78738=CARTESIAN_POINT('Ctrl Pts',(168.690654922277,2.53451579809189,48.35));
#78739=CARTESIAN_POINT('',(168.767189819366,3.04324695467949,48.5));
#78740=CARTESIAN_POINT('Ctrl Pts',(168.767189819366,3.04324695467949,48.5));
#78741=CARTESIAN_POINT('Ctrl Pts',(168.693656314164,2.86466577649117,48.5));
#78742=CARTESIAN_POINT('Ctrl Pts',(168.690654922277,2.53451579809189,48.5));
#78743=CARTESIAN_POINT('',(168.767189819366,3.04324695467949,48.35));
#78744=CARTESIAN_POINT('',(168.767189819366,3.04324695467949,48.5));
#78745=CARTESIAN_POINT('Ctrl Pts',(168.767189819366,3.04324695467949,48.35));
#78746=CARTESIAN_POINT('Ctrl Pts',(168.693656314164,2.86466577649117,48.35));
#78747=CARTESIAN_POINT('Ctrl Pts',(168.690654922277,2.53451579809189,48.35));
#78748=CARTESIAN_POINT('Ctrl Pts',(168.968281138688,3.31487038731575,48.5));
#78749=CARTESIAN_POINT('Ctrl Pts',(168.968281138688,3.31487038731575,48.35));
#78750=CARTESIAN_POINT('Ctrl Pts',(168.840723175555,3.22182813286781,48.5));
#78751=CARTESIAN_POINT('Ctrl Pts',(168.840723175555,3.22182813286781,48.35));
#78752=CARTESIAN_POINT('Ctrl Pts',(168.767189819366,3.04324695467949,48.5));
#78753=CARTESIAN_POINT('Ctrl Pts',(168.767189819366,3.04324695467949,48.35));
#78754=CARTESIAN_POINT('',(168.968281138688,3.31487038731575,48.5));
#78755=CARTESIAN_POINT('Ctrl Pts',(168.968281138688,3.31487038731575,48.5));
#78756=CARTESIAN_POINT('Ctrl Pts',(168.840723175555,3.22182813286781,48.5));
#78757=CARTESIAN_POINT('Ctrl Pts',(168.767189819366,3.04324695467949,48.5));
#78758=CARTESIAN_POINT('',(168.968281138688,3.31487038731575,48.35));
#78759=CARTESIAN_POINT('',(168.968281138688,3.31487038731575,48.5));
#78760=CARTESIAN_POINT('Ctrl Pts',(168.968281138688,3.31487038731575,48.35));
#78761=CARTESIAN_POINT('Ctrl Pts',(168.840723175555,3.22182813286781,48.35));
#78762=CARTESIAN_POINT('Ctrl Pts',(168.767189819366,3.04324695467949,48.35));
#78763=CARTESIAN_POINT('Ctrl Pts',(169.194884140044,3.38690319657326,48.5));
#78764=CARTESIAN_POINT('Ctrl Pts',(169.194884140044,3.38690319657326,48.35));
#78765=CARTESIAN_POINT('Ctrl Pts',(169.065825480968,3.38690319657326,48.5));
#78766=CARTESIAN_POINT('Ctrl Pts',(169.065825480968,3.38690319657326,48.35));
#78767=CARTESIAN_POINT('Ctrl Pts',(168.968281138688,3.31487038731575,48.5));
#78768=CARTESIAN_POINT('Ctrl Pts',(168.968281138688,3.31487038731575,48.35));
#78769=CARTESIAN_POINT('',(169.194884140044,3.38690319657326,48.5));
#78770=CARTESIAN_POINT('Ctrl Pts',(169.194884140044,3.38690319657326,48.5));
#78771=CARTESIAN_POINT('Ctrl Pts',(169.065825480968,3.38690319657326,48.5));
#78772=CARTESIAN_POINT('Ctrl Pts',(168.968281138688,3.31487038731575,48.5));
#78773=CARTESIAN_POINT('',(169.194884140044,3.38690319657326,48.35));
#78774=CARTESIAN_POINT('',(169.194884140044,3.38690319657326,48.5));
#78775=CARTESIAN_POINT('Ctrl Pts',(169.194884140044,3.38690319657326,48.35));
#78776=CARTESIAN_POINT('Ctrl Pts',(169.065825480968,3.38690319657326,48.35));
#78777=CARTESIAN_POINT('Ctrl Pts',(168.968281138688,3.31487038731575,48.35));
#78778=CARTESIAN_POINT('Ctrl Pts',(169.465007025748,3.27135065197945,48.5));
#78779=CARTESIAN_POINT('Ctrl Pts',(169.465007025748,3.27135065197945,48.35));
#78780=CARTESIAN_POINT('Ctrl Pts',(169.35545726493,3.38690319657326,48.5));
#78781=CARTESIAN_POINT('Ctrl Pts',(169.35545726493,3.38690319657326,48.35));
#78782=CARTESIAN_POINT('Ctrl Pts',(169.194884140044,3.38690319657326,48.5));
#78783=CARTESIAN_POINT('Ctrl Pts',(169.194884140044,3.38690319657326,48.35));
#78784=CARTESIAN_POINT('',(169.465007025748,3.27135065197945,48.5));
#78785=CARTESIAN_POINT('Ctrl Pts',(169.465007025748,3.27135065197945,48.5));
#78786=CARTESIAN_POINT('Ctrl Pts',(169.35545726493,3.38690319657326,48.5));
#78787=CARTESIAN_POINT('Ctrl Pts',(169.194884140044,3.38690319657326,48.5));
#78788=CARTESIAN_POINT('',(169.465007025748,3.27135065197945,48.35));
#78789=CARTESIAN_POINT('',(169.465007025748,3.27135065197945,48.5));
#78790=CARTESIAN_POINT('Ctrl Pts',(169.465007025748,3.27135065197945,48.35));
#78791=CARTESIAN_POINT('Ctrl Pts',(169.35545726493,3.38690319657326,48.35));
#78792=CARTESIAN_POINT('Ctrl Pts',(169.194884140044,3.38690319657326,48.35));
#78793=CARTESIAN_POINT('Ctrl Pts',(169.567053455859,3.04024556279182,48.5));
#78794=CARTESIAN_POINT('Ctrl Pts',(169.567053455859,3.04024556279182,48.35));
#78795=CARTESIAN_POINT('Ctrl Pts',(169.531037051231,3.19931784272194,48.5));
#78796=CARTESIAN_POINT('Ctrl Pts',(169.531037051231,3.19931784272194,48.35));
#78797=CARTESIAN_POINT('Ctrl Pts',(169.465007025748,3.27135065197945,48.5));
#78798=CARTESIAN_POINT('Ctrl Pts',(169.465007025748,3.27135065197945,48.35));
#78799=CARTESIAN_POINT('',(169.567053455859,3.04024556279182,48.5));
#78800=CARTESIAN_POINT('Ctrl Pts',(169.567053455859,3.04024556279182,48.5));
#78801=CARTESIAN_POINT('Ctrl Pts',(169.531037051231,3.19931784272194,48.5));
#78802=CARTESIAN_POINT('Ctrl Pts',(169.465007025748,3.27135065197945,48.5));
#78803=CARTESIAN_POINT('',(169.567053455859,3.04024556279182,48.35));
#78804=CARTESIAN_POINT('',(169.567053455859,3.04024556279182,48.5));
#78805=CARTESIAN_POINT('Ctrl Pts',(169.567053455859,3.04024556279182,48.35));
#78806=CARTESIAN_POINT('Ctrl Pts',(169.531037051231,3.19931784272194,48.35));
#78807=CARTESIAN_POINT('Ctrl Pts',(169.465007025748,3.27135065197945,48.35));
#78808=CARTESIAN_POINT('Origin',(169.835675496608,3.06125515699387,48.5));
#78809=CARTESIAN_POINT('',(169.835675496608,3.06125515699387,48.5));
#78810=CARTESIAN_POINT('',(85.6260995320938,-3.52498405855974,48.5));
#78811=CARTESIAN_POINT('',(169.835675496608,3.06125515699387,48.35));
#78812=CARTESIAN_POINT('',(169.835675496608,3.06125515699387,48.5));
#78813=CARTESIAN_POINT('',(169.835675496608,3.06125515699387,48.35));
#78814=CARTESIAN_POINT('Ctrl Pts',(169.636834997684,3.46343794465065,48.5));
#78815=CARTESIAN_POINT('Ctrl Pts',(169.636834997684,3.46343794465065,48.35));
#78816=CARTESIAN_POINT('Ctrl Pts',(169.802660483867,3.31787177920341,48.5));
#78817=CARTESIAN_POINT('Ctrl Pts',(169.802660483867,3.31787177920341,48.35));
#78818=CARTESIAN_POINT('Ctrl Pts',(169.835675496608,3.06125515699387,48.5));
#78819=CARTESIAN_POINT('Ctrl Pts',(169.835675496608,3.06125515699387,48.35));
#78820=CARTESIAN_POINT('Ctrl Pts',(169.636834997684,3.46343794465065,48.5));
#78821=CARTESIAN_POINT('Ctrl Pts',(169.802660483867,3.31787177920341,48.5));
#78822=CARTESIAN_POINT('Ctrl Pts',(169.835675496608,3.06125515699387,48.5));
#78823=CARTESIAN_POINT('Ctrl Pts',(169.636834997684,3.46343794465065,48.35));
#78824=CARTESIAN_POINT('Ctrl Pts',(169.802660483867,3.31787177920341,48.35));
#78825=CARTESIAN_POINT('Ctrl Pts',(169.835675496608,3.06125515699387,48.35));
#78826=CARTESIAN_POINT('Origin',(169.999999914318,2.48574362695217,48.35));
#78827=CARTESIAN_POINT('Origin',(0.,8.,48.5));
#78828=CARTESIAN_POINT('Origin',(0.,8.,48.5));
#78829=CARTESIAN_POINT('Ctrl Pts',(160.85163737461,3.38540250062943,48.5));
#78830=CARTESIAN_POINT('Ctrl Pts',(160.85163737461,3.38540250062943,48.35));
#78831=CARTESIAN_POINT('Ctrl Pts',(160.665552567691,3.38540250062943,48.5));
#78832=CARTESIAN_POINT('Ctrl Pts',(160.665552567691,3.38540250062943,48.35));
#78833=CARTESIAN_POINT('Ctrl Pts',(160.55450225994,3.22783091664314,48.5));
#78834=CARTESIAN_POINT('Ctrl Pts',(160.55450225994,3.22783091664314,48.35));
#78835=CARTESIAN_POINT('',(160.85163737461,3.38540250062943,48.5));
#78836=CARTESIAN_POINT('',(160.55450225994,3.22783091664314,48.5));
#78837=CARTESIAN_POINT('Ctrl Pts',(160.85163737461,3.38540250062943,48.5));
#78838=CARTESIAN_POINT('Ctrl Pts',(160.665552567691,3.38540250062943,48.5));
#78839=CARTESIAN_POINT('Ctrl Pts',(160.55450225994,3.22783091664314,48.5));
#78840=CARTESIAN_POINT('',(160.85163737461,3.38540250062943,48.35));
#78841=CARTESIAN_POINT('',(160.85163737461,3.38540250062943,48.5));
#78842=CARTESIAN_POINT('',(160.55450225994,3.22783091664314,48.35));
#78843=CARTESIAN_POINT('Ctrl Pts',(160.85163737461,3.38540250062943,48.35));
#78844=CARTESIAN_POINT('Ctrl Pts',(160.665552567691,3.38540250062943,48.35));
#78845=CARTESIAN_POINT('Ctrl Pts',(160.55450225994,3.22783091664314,48.35));
#78846=CARTESIAN_POINT('',(160.55450225994,3.22783091664314,48.5));
#78847=CARTESIAN_POINT('Ctrl Pts',(161.167530667037,3.2068213224411,48.5));
#78848=CARTESIAN_POINT('Ctrl Pts',(161.167530667037,3.2068213224411,48.35));
#78849=CARTESIAN_POINT('Ctrl Pts',(161.04072297737,3.38540250062943,48.5));
#78850=CARTESIAN_POINT('Ctrl Pts',(161.04072297737,3.38540250062943,48.35));
#78851=CARTESIAN_POINT('Ctrl Pts',(160.85163737461,3.38540250062943,48.5));
#78852=CARTESIAN_POINT('Ctrl Pts',(160.85163737461,3.38540250062943,48.35));
#78853=CARTESIAN_POINT('',(161.167530667037,3.2068213224411,48.5));
#78854=CARTESIAN_POINT('Ctrl Pts',(161.167530667037,3.2068213224411,48.5));
#78855=CARTESIAN_POINT('Ctrl Pts',(161.04072297737,3.38540250062943,48.5));
#78856=CARTESIAN_POINT('Ctrl Pts',(160.85163737461,3.38540250062943,48.5));
#78857=CARTESIAN_POINT('',(161.167530667037,3.2068213224411,48.35));
#78858=CARTESIAN_POINT('',(161.167530667037,3.2068213224411,48.5));
#78859=CARTESIAN_POINT('Ctrl Pts',(161.167530667037,3.2068213224411,48.35));
#78860=CARTESIAN_POINT('Ctrl Pts',(161.04072297737,3.38540250062943,48.35));
#78861=CARTESIAN_POINT('Ctrl Pts',(160.85163737461,3.38540250062943,48.35));
#78862=CARTESIAN_POINT('Ctrl Pts',(161.294338356704,2.48499327898026,48.5));
#78863=CARTESIAN_POINT('Ctrl Pts',(161.294338356704,2.48499327898026,48.35));
#78864=CARTESIAN_POINT('Ctrl Pts',(161.294338356704,3.02824014425278,48.5));
#78865=CARTESIAN_POINT('Ctrl Pts',(161.294338356704,3.02824014425278,48.35));
#78866=CARTESIAN_POINT('Ctrl Pts',(161.167530667037,3.2068213224411,48.5));
#78867=CARTESIAN_POINT('Ctrl Pts',(161.167530667037,3.2068213224411,48.35));
#78868=CARTESIAN_POINT('',(161.294338356704,2.48499327898026,48.5));
#78869=CARTESIAN_POINT('Ctrl Pts',(161.294338356704,2.48499327898026,48.5));
#78870=CARTESIAN_POINT('Ctrl Pts',(161.294338356704,3.02824014425278,48.5));
#78871=CARTESIAN_POINT('Ctrl Pts',(161.167530667037,3.2068213224411,48.5));
#78872=CARTESIAN_POINT('',(161.294338356704,2.48499327898026,48.35));
#78873=CARTESIAN_POINT('',(161.294338356704,2.48499327898026,48.5));
#78874=CARTESIAN_POINT('Ctrl Pts',(161.294338356704,2.48499327898026,48.35));
#78875=CARTESIAN_POINT('Ctrl Pts',(161.294338356704,3.02824014425278,48.35));
#78876=CARTESIAN_POINT('Ctrl Pts',(161.167530667037,3.2068213224411,48.35));
#78877=CARTESIAN_POINT('Ctrl Pts',(161.167530667037,1.76466578245163,48.5));
#78878=CARTESIAN_POINT('Ctrl Pts',(161.167530667037,1.76466578245163,48.35));
#78879=CARTESIAN_POINT('Ctrl Pts',(161.294338356704,1.9447478055954,48.5));
#78880=CARTESIAN_POINT('Ctrl Pts',(161.294338356704,1.9447478055954,48.35));
#78881=CARTESIAN_POINT('Ctrl Pts',(161.294338356704,2.48499327898026,48.5));
#78882=CARTESIAN_POINT('Ctrl Pts',(161.294338356704,2.48499327898026,48.35));
#78883=CARTESIAN_POINT('',(161.167530667037,1.76466578245163,48.5));
#78884=CARTESIAN_POINT('Ctrl Pts',(161.167530667037,1.76466578245163,48.5));
#78885=CARTESIAN_POINT('Ctrl Pts',(161.294338356704,1.9447478055954,48.5));
#78886=CARTESIAN_POINT('Ctrl Pts',(161.294338356704,2.48499327898026,48.5));
#78887=CARTESIAN_POINT('',(161.167530667037,1.76466578245163,48.35));
#78888=CARTESIAN_POINT('',(161.167530667037,1.76466578245163,48.5));
#78889=CARTESIAN_POINT('Ctrl Pts',(161.167530667037,1.76466578245163,48.35));
#78890=CARTESIAN_POINT('Ctrl Pts',(161.294338356704,1.9447478055954,48.35));
#78891=CARTESIAN_POINT('Ctrl Pts',(161.294338356704,2.48499327898026,48.35));
#78892=CARTESIAN_POINT('Ctrl Pts',(160.854638468474,1.58458405733109,48.5));
#78893=CARTESIAN_POINT('Ctrl Pts',(160.854638468474,1.58458405733109,48.35));
#78894=CARTESIAN_POINT('Ctrl Pts',(161.04072297737,1.58458405733109,48.5));
#78895=CARTESIAN_POINT('Ctrl Pts',(161.04072297737,1.58458405733109,48.35));
#78896=CARTESIAN_POINT('Ctrl Pts',(161.167530667037,1.76466578245163,48.5));
#78897=CARTESIAN_POINT('Ctrl Pts',(161.167530667037,1.76466578245163,48.35));
#78898=CARTESIAN_POINT('',(160.854638468474,1.58458405733109,48.5));
#78899=CARTESIAN_POINT('Ctrl Pts',(160.854638468474,1.58458405733109,48.5));
#78900=CARTESIAN_POINT('Ctrl Pts',(161.04072297737,1.58458405733109,48.5));
#78901=CARTESIAN_POINT('Ctrl Pts',(161.167530667037,1.76466578245163,48.5));
#78902=CARTESIAN_POINT('',(160.854638468474,1.58458405733109,48.35));
#78903=CARTESIAN_POINT('',(160.854638468474,1.58458405733109,48.5));
#78904=CARTESIAN_POINT('Ctrl Pts',(160.854638468474,1.58458405733109,48.35));
#78905=CARTESIAN_POINT('Ctrl Pts',(161.04072297737,1.58458405733109,48.35));
#78906=CARTESIAN_POINT('Ctrl Pts',(161.167530667037,1.76466578245163,48.35));
#78907=CARTESIAN_POINT('Ctrl Pts',(160.541746269912,1.76391565799713,48.5));
#78908=CARTESIAN_POINT('Ctrl Pts',(160.541746269912,1.76391565799713,48.35));
#78909=CARTESIAN_POINT('Ctrl Pts',(160.668553959578,1.58458405733109,48.5));
#78910=CARTESIAN_POINT('Ctrl Pts',(160.668553959578,1.58458405733109,48.35));
#78911=CARTESIAN_POINT('Ctrl Pts',(160.854638468474,1.58458405733109,48.5));
#78912=CARTESIAN_POINT('Ctrl Pts',(160.854638468474,1.58458405733109,48.35));
#78913=CARTESIAN_POINT('',(160.541746269912,1.76391565799713,48.5));
#78914=CARTESIAN_POINT('Ctrl Pts',(160.541746269912,1.76391565799713,48.5));
#78915=CARTESIAN_POINT('Ctrl Pts',(160.668553959578,1.58458405733109,48.5));
#78916=CARTESIAN_POINT('Ctrl Pts',(160.854638468474,1.58458405733109,48.5));
#78917=CARTESIAN_POINT('',(160.541746269912,1.76391565799713,48.35));
#78918=CARTESIAN_POINT('',(160.541746269912,1.76391565799713,48.5));
#78919=CARTESIAN_POINT('Ctrl Pts',(160.541746269912,1.76391565799713,48.35));
#78920=CARTESIAN_POINT('Ctrl Pts',(160.668553959578,1.58458405733109,48.35));
#78921=CARTESIAN_POINT('Ctrl Pts',(160.854638468474,1.58458405733109,48.35));
#78922=CARTESIAN_POINT('Ctrl Pts',(160.414938580245,2.48499327898026,48.5));
#78923=CARTESIAN_POINT('Ctrl Pts',(160.414938580245,2.48499327898026,48.35));
#78924=CARTESIAN_POINT('Ctrl Pts',(160.414938580245,1.94324696063995,48.5));
#78925=CARTESIAN_POINT('Ctrl Pts',(160.414938580245,1.94324696063995,48.35));
#78926=CARTESIAN_POINT('Ctrl Pts',(160.541746269912,1.76391565799713,48.5));
#78927=CARTESIAN_POINT('Ctrl Pts',(160.541746269912,1.76391565799713,48.35));
#78928=CARTESIAN_POINT('',(160.414938580245,2.48499327898026,48.5));
#78929=CARTESIAN_POINT('Ctrl Pts',(160.414938580245,2.48499327898026,48.5));
#78930=CARTESIAN_POINT('Ctrl Pts',(160.414938580245,1.94324696063995,48.5));
#78931=CARTESIAN_POINT('Ctrl Pts',(160.541746269912,1.76391565799713,48.5));
#78932=CARTESIAN_POINT('',(160.414938580245,2.48499327898026,48.35));
#78933=CARTESIAN_POINT('',(160.414938580245,2.48499327898026,48.5));
#78934=CARTESIAN_POINT('Ctrl Pts',(160.414938580245,2.48499327898026,48.35));
#78935=CARTESIAN_POINT('Ctrl Pts',(160.414938580245,1.94324696063995,48.35));
#78936=CARTESIAN_POINT('Ctrl Pts',(160.541746269912,1.76391565799713,48.35));
#78937=CARTESIAN_POINT('Ctrl Pts',(160.55450225994,3.22783091664314,48.5));
#78938=CARTESIAN_POINT('Ctrl Pts',(160.55450225994,3.22783091664314,48.35));
#78939=CARTESIAN_POINT('Ctrl Pts',(160.414938580245,3.02673944830894,48.5));
#78940=CARTESIAN_POINT('Ctrl Pts',(160.414938580245,3.02673944830894,48.35));
#78941=CARTESIAN_POINT('Ctrl Pts',(160.414938580245,2.48499327898026,48.5));
#78942=CARTESIAN_POINT('Ctrl Pts',(160.414938580245,2.48499327898026,48.35));
#78943=CARTESIAN_POINT('Ctrl Pts',(160.55450225994,3.22783091664314,48.5));
#78944=CARTESIAN_POINT('Ctrl Pts',(160.414938580245,3.02673944830894,48.5));
#78945=CARTESIAN_POINT('Ctrl Pts',(160.414938580245,2.48499327898026,48.5));
#78946=CARTESIAN_POINT('Ctrl Pts',(160.55450225994,3.22783091664314,48.35));
#78947=CARTESIAN_POINT('Ctrl Pts',(160.414938580245,3.02673944830894,48.35));
#78948=CARTESIAN_POINT('Ctrl Pts',(160.414938580245,2.48499327898026,48.35));
#78949=CARTESIAN_POINT('Ctrl Pts',(160.854638468474,1.36248314380646,48.5));
#78950=CARTESIAN_POINT('Ctrl Pts',(160.854638468474,1.36248314380646,48.35));
#78951=CARTESIAN_POINT('Ctrl Pts',(160.536493908614,1.36248314380646,48.5));
#78952=CARTESIAN_POINT('Ctrl Pts',(160.536493908614,1.36248314380646,48.35));
#78953=CARTESIAN_POINT('Ctrl Pts',(160.354911338538,1.59058684110642,48.5));
#78954=CARTESIAN_POINT('Ctrl Pts',(160.354911338538,1.59058684110642,48.35));
#78955=CARTESIAN_POINT('',(160.854638468474,1.36248314380646,48.5));
#78956=CARTESIAN_POINT('',(160.354911338538,1.59058684110642,48.5));
#78957=CARTESIAN_POINT('Ctrl Pts',(160.854638468474,1.36248314380646,48.5));
#78958=CARTESIAN_POINT('Ctrl Pts',(160.536493908614,1.36248314380646,48.5));
#78959=CARTESIAN_POINT('Ctrl Pts',(160.354911338538,1.59058684110642,48.5));
#78960=CARTESIAN_POINT('',(160.854638468474,1.36248314380646,48.35));
#78961=CARTESIAN_POINT('',(160.854638468474,1.36248314380646,48.5));
#78962=CARTESIAN_POINT('',(160.354911338538,1.59058684110642,48.35));
#78963=CARTESIAN_POINT('Ctrl Pts',(160.854638468474,1.36248314380646,48.35));
#78964=CARTESIAN_POINT('Ctrl Pts',(160.536493908614,1.36248314380646,48.35));
#78965=CARTESIAN_POINT('Ctrl Pts',(160.354911338538,1.59058684110642,48.35));
#78966=CARTESIAN_POINT('',(160.354911338538,1.59058684110642,48.5));
#78967=CARTESIAN_POINT('Ctrl Pts',(161.254570137709,1.49229192733765,48.5));
#78968=CARTESIAN_POINT('Ctrl Pts',(161.254570137709,1.49229192733765,48.35));
#78969=CARTESIAN_POINT('Ctrl Pts',(161.096248280257,1.36248314380646,48.5));
#78970=CARTESIAN_POINT('Ctrl Pts',(161.096248280257,1.36248314380646,48.35));
#78971=CARTESIAN_POINT('Ctrl Pts',(160.854638468474,1.36248314380646,48.5));
#78972=CARTESIAN_POINT('Ctrl Pts',(160.854638468474,1.36248314380646,48.35));
#78973=CARTESIAN_POINT('',(161.254570137709,1.49229192733765,48.5));
#78974=CARTESIAN_POINT('Ctrl Pts',(161.254570137709,1.49229192733765,48.5));
#78975=CARTESIAN_POINT('Ctrl Pts',(161.096248280257,1.36248314380646,48.5));
#78976=CARTESIAN_POINT('Ctrl Pts',(160.854638468474,1.36248314380646,48.5));
#78977=CARTESIAN_POINT('',(161.254570137709,1.49229192733765,48.35));
#78978=CARTESIAN_POINT('',(161.254570137709,1.49229192733765,48.5));
#78979=CARTESIAN_POINT('Ctrl Pts',(161.254570137709,1.49229192733765,48.35));
#78980=CARTESIAN_POINT('Ctrl Pts',(161.096248280257,1.36248314380646,48.35));
#78981=CARTESIAN_POINT('Ctrl Pts',(160.854638468474,1.36248314380646,48.35));
#78982=CARTESIAN_POINT('Ctrl Pts',(161.49242843315,1.85995900630951,48.5));
#78983=CARTESIAN_POINT('Ctrl Pts',(161.49242843315,1.85995900630951,48.35));
#78984=CARTESIAN_POINT('Ctrl Pts',(161.412891995162,1.62210100889206,48.5));
#78985=CARTESIAN_POINT('Ctrl Pts',(161.412891995162,1.62210100889206,48.35));
#78986=CARTESIAN_POINT('Ctrl Pts',(161.254570137709,1.49229192733765,48.5));
#78987=CARTESIAN_POINT('Ctrl Pts',(161.254570137709,1.49229192733765,48.35));
#78988=CARTESIAN_POINT('',(161.49242843315,1.85995900630951,48.5));
#78989=CARTESIAN_POINT('Ctrl Pts',(161.49242843315,1.85995900630951,48.5));
#78990=CARTESIAN_POINT('Ctrl Pts',(161.412891995162,1.62210100889206,48.5));
#78991=CARTESIAN_POINT('Ctrl Pts',(161.254570137709,1.49229192733765,48.5));
#78992=CARTESIAN_POINT('',(161.49242843315,1.85995900630951,48.35));
#78993=CARTESIAN_POINT('',(161.49242843315,1.85995900630951,48.5));
#78994=CARTESIAN_POINT('Ctrl Pts',(161.49242843315,1.85995900630951,48.35));
#78995=CARTESIAN_POINT('Ctrl Pts',(161.412891995162,1.62210100889206,48.35));
#78996=CARTESIAN_POINT('Ctrl Pts',(161.254570137709,1.49229192733765,48.35));
#78997=CARTESIAN_POINT('Ctrl Pts',(161.571964275092,2.48499327898026,48.5));
#78998=CARTESIAN_POINT('Ctrl Pts',(161.571964275092,2.48499327898026,48.35));
#78999=CARTESIAN_POINT('Ctrl Pts',(161.571964275092,2.09781730175018,48.5));
#79000=CARTESIAN_POINT('Ctrl Pts',(161.571964275092,2.09781730175018,48.35));
#79001=CARTESIAN_POINT('Ctrl Pts',(161.49242843315,1.85995900630951,48.5));
#79002=CARTESIAN_POINT('Ctrl Pts',(161.49242843315,1.85995900630951,48.35));
#79003=CARTESIAN_POINT('',(161.571964275092,2.48499327898026,48.5));
#79004=CARTESIAN_POINT('Ctrl Pts',(161.571964275092,2.48499327898026,48.5));
#79005=CARTESIAN_POINT('Ctrl Pts',(161.571964275092,2.09781730175018,48.5));
#79006=CARTESIAN_POINT('Ctrl Pts',(161.49242843315,1.85995900630951,48.5));
#79007=CARTESIAN_POINT('',(161.571964275092,2.48499327898026,48.35));
#79008=CARTESIAN_POINT('',(161.571964275092,2.48499327898026,48.5));
#79009=CARTESIAN_POINT('Ctrl Pts',(161.571964275092,2.48499327898026,48.35));
#79010=CARTESIAN_POINT('Ctrl Pts',(161.571964275092,2.09781730175018,48.35));
#79011=CARTESIAN_POINT('Ctrl Pts',(161.49242843315,1.85995900630951,48.35));
#79012=CARTESIAN_POINT('Ctrl Pts',(161.52244175598,3.00497958064079,48.5));
#79013=CARTESIAN_POINT('Ctrl Pts',(161.52244175598,3.00497958064079,48.35));
#79014=CARTESIAN_POINT('Ctrl Pts',(161.571964275092,2.81214186549187,48.5));
#79015=CARTESIAN_POINT('Ctrl Pts',(161.571964275092,2.81214186549187,48.35));
#79016=CARTESIAN_POINT('Ctrl Pts',(161.571964275092,2.48499327898026,48.5));
#79017=CARTESIAN_POINT('Ctrl Pts',(161.571964275092,2.48499327898026,48.35));
#79018=CARTESIAN_POINT('',(161.52244175598,3.00497958064079,48.5));
#79019=CARTESIAN_POINT('Ctrl Pts',(161.52244175598,3.00497958064079,48.5));
#79020=CARTESIAN_POINT('Ctrl Pts',(161.571964275092,2.81214186549187,48.5));
#79021=CARTESIAN_POINT('Ctrl Pts',(161.571964275092,2.48499327898026,48.5));
#79022=CARTESIAN_POINT('',(161.52244175598,3.00497958064079,48.35));
#79023=CARTESIAN_POINT('',(161.52244175598,3.00497958064079,48.5));
#79024=CARTESIAN_POINT('Ctrl Pts',(161.52244175598,3.00497958064079,48.35));
#79025=CARTESIAN_POINT('Ctrl Pts',(161.571964275092,2.81214186549187,48.35));
#79026=CARTESIAN_POINT('Ctrl Pts',(161.571964275092,2.48499327898026,48.35));
#79027=CARTESIAN_POINT('Ctrl Pts',(161.385879766196,3.33212831616402,48.5));
#79028=CARTESIAN_POINT('Ctrl Pts',(161.385879766196,3.33212831616402,48.35));
#79029=CARTESIAN_POINT('Ctrl Pts',(161.472919236869,3.19781729578972,48.5));
#79030=CARTESIAN_POINT('Ctrl Pts',(161.472919236869,3.19781729578972,48.35));
#79031=CARTESIAN_POINT('Ctrl Pts',(161.52244175598,3.00497958064079,48.5));
#79032=CARTESIAN_POINT('Ctrl Pts',(161.52244175598,3.00497958064079,48.35));
#79033=CARTESIAN_POINT('',(161.385879766196,3.33212831616402,48.5));
#79034=CARTESIAN_POINT('Ctrl Pts',(161.385879766196,3.33212831616402,48.5));
#79035=CARTESIAN_POINT('Ctrl Pts',(161.472919236869,3.19781729578972,48.5));
#79036=CARTESIAN_POINT('Ctrl Pts',(161.52244175598,3.00497958064079,48.5));
#79037=CARTESIAN_POINT('',(161.385879766196,3.33212831616402,48.35));
#79038=CARTESIAN_POINT('',(161.385879766196,3.33212831616402,48.5));
#79039=CARTESIAN_POINT('Ctrl Pts',(161.385879766196,3.33212831616402,48.35));
#79040=CARTESIAN_POINT('Ctrl Pts',(161.472919236869,3.19781729578972,48.35));
#79041=CARTESIAN_POINT('Ctrl Pts',(161.52244175598,3.00497958064079,48.35));
#79042=CARTESIAN_POINT('Ctrl Pts',(161.16527999565,3.5377217233181,48.5));
#79043=CARTESIAN_POINT('Ctrl Pts',(161.16527999565,3.5377217233181,48.35));
#79044=CARTESIAN_POINT('Ctrl Pts',(161.298840295523,3.46643933653831,48.5));
#79045=CARTESIAN_POINT('Ctrl Pts',(161.298840295523,3.46643933653831,48.35));
#79046=CARTESIAN_POINT('Ctrl Pts',(161.385879766196,3.33212831616402,48.5));
#79047=CARTESIAN_POINT('Ctrl Pts',(161.385879766196,3.33212831616402,48.35));
#79048=CARTESIAN_POINT('',(161.16527999565,3.5377217233181,48.5));
#79049=CARTESIAN_POINT('Ctrl Pts',(161.16527999565,3.5377217233181,48.5));
#79050=CARTESIAN_POINT('Ctrl Pts',(161.298840295523,3.46643933653831,48.5));
#79051=CARTESIAN_POINT('Ctrl Pts',(161.385879766196,3.33212831616402,48.5));
#79052=CARTESIAN_POINT('',(161.16527999565,3.5377217233181,48.35));
#79053=CARTESIAN_POINT('',(161.16527999565,3.5377217233181,48.5));
#79054=CARTESIAN_POINT('Ctrl Pts',(161.16527999565,3.5377217233181,48.35));
#79055=CARTESIAN_POINT('Ctrl Pts',(161.298840295523,3.46643933653831,48.35));
#79056=CARTESIAN_POINT('Ctrl Pts',(161.385879766196,3.33212831616402,48.35));
#79057=CARTESIAN_POINT('Ctrl Pts',(160.854638468474,3.60900411009789,48.5));
#79058=CARTESIAN_POINT('Ctrl Pts',(160.854638468474,3.60900411009789,48.35));
#79059=CARTESIAN_POINT('Ctrl Pts',(161.03171909973,3.60900411009789,48.5));
#79060=CARTESIAN_POINT('Ctrl Pts',(161.03171909973,3.60900411009789,48.35));
#79061=CARTESIAN_POINT('Ctrl Pts',(161.16527999565,3.5377217233181,48.5));
#79062=CARTESIAN_POINT('Ctrl Pts',(161.16527999565,3.5377217233181,48.35));
#79063=CARTESIAN_POINT('',(160.854638468474,3.60900411009789,48.5));
#79064=CARTESIAN_POINT('Ctrl Pts',(160.854638468474,3.60900411009789,48.5));
#79065=CARTESIAN_POINT('Ctrl Pts',(161.03171909973,3.60900411009789,48.5));
#79066=CARTESIAN_POINT('Ctrl Pts',(161.16527999565,3.5377217233181,48.5));
#79067=CARTESIAN_POINT('',(160.854638468474,3.60900411009789,48.35));
#79068=CARTESIAN_POINT('',(160.854638468474,3.60900411009789,48.5));
#79069=CARTESIAN_POINT('Ctrl Pts',(160.854638468474,3.60900411009789,48.35));
#79070=CARTESIAN_POINT('Ctrl Pts',(161.03171909973,3.60900411009789,48.35));
#79071=CARTESIAN_POINT('Ctrl Pts',(161.16527999565,3.5377217233181,48.35));
#79072=CARTESIAN_POINT('Ctrl Pts',(160.456207644194,3.47994545102119,48.5));
#79073=CARTESIAN_POINT('Ctrl Pts',(160.456207644194,3.47994545102119,48.35));
#79074=CARTESIAN_POINT('Ctrl Pts',(160.614529501647,3.60900411009789,48.5));
#79075=CARTESIAN_POINT('Ctrl Pts',(160.614529501647,3.60900411009789,48.35));
#79076=CARTESIAN_POINT('Ctrl Pts',(160.854638468474,3.60900411009789,48.5));
#79077=CARTESIAN_POINT('Ctrl Pts',(160.854638468474,3.60900411009789,48.35));
#79078=CARTESIAN_POINT('',(160.456207644194,3.47994545102119,48.5));
#79079=CARTESIAN_POINT('Ctrl Pts',(160.456207644194,3.47994545102119,48.5));
#79080=CARTESIAN_POINT('Ctrl Pts',(160.614529501647,3.60900411009789,48.5));
#79081=CARTESIAN_POINT('Ctrl Pts',(160.854638468474,3.60900411009789,48.5));
#79082=CARTESIAN_POINT('',(160.456207644194,3.47994545102119,48.35));
#79083=CARTESIAN_POINT('',(160.456207644194,3.47994545102119,48.5));
#79084=CARTESIAN_POINT('Ctrl Pts',(160.456207644194,3.47994545102119,48.35));
#79085=CARTESIAN_POINT('Ctrl Pts',(160.614529501647,3.60900411009789,48.35));
#79086=CARTESIAN_POINT('Ctrl Pts',(160.854638468474,3.60900411009789,48.35));
#79087=CARTESIAN_POINT('Ctrl Pts',(160.217598926276,3.11302864551544,48.5));
#79088=CARTESIAN_POINT('Ctrl Pts',(160.217598926276,3.11302864551544,48.35));
#79089=CARTESIAN_POINT('Ctrl Pts',(160.297885488719,3.3508867919445,48.5));
#79090=CARTESIAN_POINT('Ctrl Pts',(160.297885488719,3.3508867919445,48.35));
#79091=CARTESIAN_POINT('Ctrl Pts',(160.456207644194,3.47994545102119,48.5));
#79092=CARTESIAN_POINT('Ctrl Pts',(160.456207644194,3.47994545102119,48.35));
#79093=CARTESIAN_POINT('',(160.217598926276,3.11302864551544,48.5));
#79094=CARTESIAN_POINT('Ctrl Pts',(160.217598926276,3.11302864551544,48.5));
#79095=CARTESIAN_POINT('Ctrl Pts',(160.297885488719,3.3508867919445,48.5));
#79096=CARTESIAN_POINT('Ctrl Pts',(160.456207644194,3.47994545102119,48.5));
#79097=CARTESIAN_POINT('',(160.217598926276,3.11302864551544,48.35));
#79098=CARTESIAN_POINT('',(160.217598926276,3.11302864551544,48.5));
#79099=CARTESIAN_POINT('Ctrl Pts',(160.217598926276,3.11302864551544,48.35));
#79100=CARTESIAN_POINT('Ctrl Pts',(160.297885488719,3.3508867919445,48.35));
#79101=CARTESIAN_POINT('Ctrl Pts',(160.456207644194,3.47994545102119,48.35));
#79102=CARTESIAN_POINT('Ctrl Pts',(160.137312661856,2.48499327898026,48.5));
#79103=CARTESIAN_POINT('Ctrl Pts',(160.137312661856,2.48499327898026,48.35));
#79104=CARTESIAN_POINT('Ctrl Pts',(160.137312661856,2.87517049908638,48.5));
#79105=CARTESIAN_POINT('Ctrl Pts',(160.137312661856,2.87517049908638,48.35));
#79106=CARTESIAN_POINT('Ctrl Pts',(160.217598926276,3.11302864551544,48.5));
#79107=CARTESIAN_POINT('Ctrl Pts',(160.217598926276,3.11302864551544,48.35));
#79108=CARTESIAN_POINT('',(160.137312661856,2.48499327898026,48.5));
#79109=CARTESIAN_POINT('Ctrl Pts',(160.137312661856,2.48499327898026,48.5));
#79110=CARTESIAN_POINT('Ctrl Pts',(160.137312661856,2.87517049908638,48.5));
#79111=CARTESIAN_POINT('Ctrl Pts',(160.217598926276,3.11302864551544,48.5));
#79112=CARTESIAN_POINT('',(160.137312661856,2.48499327898026,48.35));
#79113=CARTESIAN_POINT('',(160.137312661856,2.48499327898026,48.5));
#79114=CARTESIAN_POINT('Ctrl Pts',(160.137312661856,2.48499327898026,48.35));
#79115=CARTESIAN_POINT('Ctrl Pts',(160.137312661856,2.87517049908638,48.35));
#79116=CARTESIAN_POINT('Ctrl Pts',(160.217598926276,3.11302864551544,48.35));
#79117=CARTESIAN_POINT('Ctrl Pts',(160.354911338538,1.59058684110642,48.5));
#79118=CARTESIAN_POINT('Ctrl Pts',(160.354911338538,1.59058684110642,48.35));
#79119=CARTESIAN_POINT('Ctrl Pts',(160.137312661856,1.86521166563034,48.5));
#79120=CARTESIAN_POINT('Ctrl Pts',(160.137312661856,1.86521166563034,48.35));
#79121=CARTESIAN_POINT('Ctrl Pts',(160.137312661856,2.48499327898026,48.5));
#79122=CARTESIAN_POINT('Ctrl Pts',(160.137312661856,2.48499327898026,48.35));
#79123=CARTESIAN_POINT('Ctrl Pts',(160.354911338538,1.59058684110642,48.5));
#79124=CARTESIAN_POINT('Ctrl Pts',(160.137312661856,1.86521166563034,48.5));
#79125=CARTESIAN_POINT('Ctrl Pts',(160.137312661856,2.48499327898026,48.5));
#79126=CARTESIAN_POINT('Ctrl Pts',(160.354911338538,1.59058684110642,48.35));
#79127=CARTESIAN_POINT('Ctrl Pts',(160.137312661856,1.86521166563034,48.35));
#79128=CARTESIAN_POINT('Ctrl Pts',(160.137312661856,2.48499327898026,48.35));
#79129=CARTESIAN_POINT('Origin',(159.999999951571,2.48574362695217,48.35));
#79130=CARTESIAN_POINT('Ctrl Pts',(159.134857010096,1.36248314380646,48.5));
#79131=CARTESIAN_POINT('Ctrl Pts',(159.134857010096,1.36248314380646,48.35));
#79132=CARTESIAN_POINT('Ctrl Pts',(158.834720503539,1.36248314380646,48.5));
#79133=CARTESIAN_POINT('Ctrl Pts',(158.834720503539,1.36248314380646,48.35));
#79134=CARTESIAN_POINT('Ctrl Pts',(158.644884180278,1.53055930137634,48.5));
#79135=CARTESIAN_POINT('Ctrl Pts',(158.644884180278,1.53055930137634,48.35));
#79136=CARTESIAN_POINT('',(159.134857010096,1.36248314380646,48.5));
#79137=CARTESIAN_POINT('',(158.644884180278,1.53055930137634,48.5));
#79138=CARTESIAN_POINT('Ctrl Pts',(159.134857010096,1.36248314380646,48.5));
#79139=CARTESIAN_POINT('Ctrl Pts',(158.834720503539,1.36248314380646,48.5));
#79140=CARTESIAN_POINT('Ctrl Pts',(158.644884180278,1.53055930137634,48.5));
#79141=CARTESIAN_POINT('',(159.134857010096,1.36248314380646,48.35));
#79142=CARTESIAN_POINT('',(159.134857010096,1.36248314380646,48.5));
#79143=CARTESIAN_POINT('',(158.644884180278,1.53055930137634,48.35));
#79144=CARTESIAN_POINT('Ctrl Pts',(159.134857010096,1.36248314380646,48.35));
#79145=CARTESIAN_POINT('Ctrl Pts',(158.834720503539,1.36248314380646,48.35));
#79146=CARTESIAN_POINT('Ctrl Pts',(158.644884180278,1.53055930137634,48.35));
#79147=CARTESIAN_POINT('',(158.644884180278,1.53055930137634,48.5));
#79148=CARTESIAN_POINT('Ctrl Pts',(159.712619435042,1.62960433959961,48.5));
#79149=CARTESIAN_POINT('Ctrl Pts',(159.712619435042,1.62960433959961,48.35));
#79150=CARTESIAN_POINT('Ctrl Pts',(159.501023244113,1.36248314380646,48.5));
#79151=CARTESIAN_POINT('Ctrl Pts',(159.501023244113,1.36248314380646,48.35));
#79152=CARTESIAN_POINT('Ctrl Pts',(159.134857010096,1.36248314380646,48.5));
#79153=CARTESIAN_POINT('Ctrl Pts',(159.134857010096,1.36248314380646,48.35));
#79154=CARTESIAN_POINT('',(159.712619435042,1.62960433959961,48.5));
#79155=CARTESIAN_POINT('Ctrl Pts',(159.712619435042,1.62960433959961,48.5));
#79156=CARTESIAN_POINT('Ctrl Pts',(159.501023244113,1.36248314380646,48.5));
#79157=CARTESIAN_POINT('Ctrl Pts',(159.134857010096,1.36248314380646,48.5));
#79158=CARTESIAN_POINT('',(159.712619435042,1.62960433959961,48.35));
#79159=CARTESIAN_POINT('',(159.712619435042,1.62960433959961,48.5));
#79160=CARTESIAN_POINT('Ctrl Pts',(159.712619435042,1.62960433959961,48.35));
#79161=CARTESIAN_POINT('Ctrl Pts',(159.501023244113,1.36248314380646,48.35));
#79162=CARTESIAN_POINT('Ctrl Pts',(159.134857010096,1.36248314380646,48.35));
#79163=CARTESIAN_POINT('Ctrl Pts',(159.886698674411,2.14583912491798,48.5));
#79164=CARTESIAN_POINT('Ctrl Pts',(159.886698674411,2.14583912491798,48.35));
#79165=CARTESIAN_POINT('Ctrl Pts',(159.886698674411,1.84720331430435,48.5));
#79166=CARTESIAN_POINT('Ctrl Pts',(159.886698674411,1.84720331430435,48.35));
#79167=CARTESIAN_POINT('Ctrl Pts',(159.712619435042,1.62960433959961,48.5));
#79168=CARTESIAN_POINT('Ctrl Pts',(159.712619435042,1.62960433959961,48.35));
#79169=CARTESIAN_POINT('',(159.886698674411,2.14583912491798,48.5));
#79170=CARTESIAN_POINT('Ctrl Pts',(159.886698674411,2.14583912491798,48.5));
#79171=CARTESIAN_POINT('Ctrl Pts',(159.886698674411,1.84720331430435,48.5));
#79172=CARTESIAN_POINT('Ctrl Pts',(159.712619435042,1.62960433959961,48.5));
#79173=CARTESIAN_POINT('',(159.886698674411,2.14583912491798,48.35));
#79174=CARTESIAN_POINT('',(159.886698674411,2.14583912491798,48.5));
#79175=CARTESIAN_POINT('Ctrl Pts',(159.886698674411,2.14583912491798,48.35));
#79176=CARTESIAN_POINT('Ctrl Pts',(159.886698674411,1.84720331430435,48.35));
#79177=CARTESIAN_POINT('Ctrl Pts',(159.712619435042,1.62960433959961,48.35));
#79178=CARTESIAN_POINT('Ctrl Pts',(159.688608597964,2.65907236933708,48.5));
#79179=CARTESIAN_POINT('Ctrl Pts',(159.688608597964,2.65907236933708,48.35));
#79180=CARTESIAN_POINT('Ctrl Pts',(159.886698674411,2.45948159694672,48.5));
#79181=CARTESIAN_POINT('Ctrl Pts',(159.886698674411,2.45948159694672,48.35));
#79182=CARTESIAN_POINT('Ctrl Pts',(159.886698674411,2.14583912491798,48.5));
#79183=CARTESIAN_POINT('Ctrl Pts',(159.886698674411,2.14583912491798,48.35));
#79184=CARTESIAN_POINT('',(159.688608597964,2.65907236933708,48.5));
#79185=CARTESIAN_POINT('Ctrl Pts',(159.688608597964,2.65907236933708,48.5));
#79186=CARTESIAN_POINT('Ctrl Pts',(159.886698674411,2.45948159694672,48.5));
#79187=CARTESIAN_POINT('Ctrl Pts',(159.886698674411,2.14583912491798,48.5));
#79188=CARTESIAN_POINT('',(159.688608597964,2.65907236933708,48.35));
#79189=CARTESIAN_POINT('',(159.688608597964,2.65907236933708,48.5));
#79190=CARTESIAN_POINT('Ctrl Pts',(159.688608597964,2.65907236933708,48.35));
#79191=CARTESIAN_POINT('Ctrl Pts',(159.886698674411,2.45948159694672,48.35));
#79192=CARTESIAN_POINT('Ctrl Pts',(159.886698674411,2.14583912491798,48.35));
#79193=CARTESIAN_POINT('Ctrl Pts',(159.202387582511,2.85866314172745,48.5));
#79194=CARTESIAN_POINT('Ctrl Pts',(159.202387582511,2.85866314172745,48.35));
#79195=CARTESIAN_POINT('Ctrl Pts',(159.490518521518,2.85866314172745,48.5));
#79196=CARTESIAN_POINT('Ctrl Pts',(159.490518521518,2.85866314172745,48.35));
#79197=CARTESIAN_POINT('Ctrl Pts',(159.688608597964,2.65907236933708,48.5));
#79198=CARTESIAN_POINT('Ctrl Pts',(159.688608597964,2.65907236933708,48.35));
#79199=CARTESIAN_POINT('',(159.202387582511,2.85866314172745,48.5));
#79200=CARTESIAN_POINT('Ctrl Pts',(159.202387582511,2.85866314172745,48.5));
#79201=CARTESIAN_POINT('Ctrl Pts',(159.490518521518,2.85866314172745,48.5));
#79202=CARTESIAN_POINT('Ctrl Pts',(159.688608597964,2.65907236933708,48.5));
#79203=CARTESIAN_POINT('',(159.202387582511,2.85866314172745,48.35));
#79204=CARTESIAN_POINT('',(159.202387582511,2.85866314172745,48.5));
#79205=CARTESIAN_POINT('Ctrl Pts',(159.202387582511,2.85866314172745,48.35));
#79206=CARTESIAN_POINT('Ctrl Pts',(159.490518521518,2.85866314172745,48.35));
#79207=CARTESIAN_POINT('Ctrl Pts',(159.688608597964,2.65907236933708,48.35));
#79208=CARTESIAN_POINT('Ctrl Pts',(158.786698680371,2.72060030698776,48.5));
#79209=CARTESIAN_POINT('Ctrl Pts',(158.786698680371,2.72060030698776,48.35));
#79210=CARTESIAN_POINT('Ctrl Pts',(158.984788607806,2.85866314172745,48.5));
#79211=CARTESIAN_POINT('Ctrl Pts',(158.984788607806,2.85866314172745,48.35));
#79212=CARTESIAN_POINT('Ctrl Pts',(159.202387582511,2.85866314172745,48.5));
#79213=CARTESIAN_POINT('Ctrl Pts',(159.202387582511,2.85866314172745,48.35));
#79214=CARTESIAN_POINT('',(158.786698680371,2.72060030698776,48.5));
#79215=CARTESIAN_POINT('Ctrl Pts',(158.786698680371,2.72060030698776,48.5));
#79216=CARTESIAN_POINT('Ctrl Pts',(158.984788607806,2.85866314172745,48.5));
#79217=CARTESIAN_POINT('Ctrl Pts',(159.202387582511,2.85866314172745,48.5));
#79218=CARTESIAN_POINT('',(158.786698680371,2.72060030698776,48.35));
#79219=CARTESIAN_POINT('',(158.786698680371,2.72060030698776,48.5));
#79220=CARTESIAN_POINT('Ctrl Pts',(158.786698680371,2.72060030698776,48.35));
#79221=CARTESIAN_POINT('Ctrl Pts',(158.984788607806,2.85866314172745,48.35));
#79222=CARTESIAN_POINT('Ctrl Pts',(159.202387582511,2.85866314172745,48.35));
#79223=CARTESIAN_POINT('Origin',(158.905252467841,3.31186899542809,48.5));
#79224=CARTESIAN_POINT('',(158.905252467841,3.31186899542809,48.5));
#79225=CARTESIAN_POINT('',(156.286292429022,-9.74978934782317,48.5));
#79226=CARTESIAN_POINT('',(158.905252467841,3.31186899542809,48.35));
#79227=CARTESIAN_POINT('',(158.905252467841,3.31186899542809,48.5));
#79228=CARTESIAN_POINT('',(158.905252467841,3.31186899542809,48.35));
#79229=CARTESIAN_POINT('Origin',(159.783151399344,3.31186899542809,48.5));
#79230=CARTESIAN_POINT('',(159.783151399344,3.31186899542809,48.5));
#79231=CARTESIAN_POINT('',(79.8915756996721,3.31186899542809,48.5));
#79232=CARTESIAN_POINT('',(159.783151399344,3.31186899542809,48.35));
#79233=CARTESIAN_POINT('',(159.783151399344,3.31186899542809,48.5));
#79234=CARTESIAN_POINT('',(159.783151399344,3.31186899542809,48.35));
#79235=CARTESIAN_POINT('Origin',(159.783151399344,3.56998646259308,48.5));
#79236=CARTESIAN_POINT('',(159.783151399344,3.56998646259308,48.5));
#79237=CARTESIAN_POINT('',(159.783151399344,5.78499323129654,48.5));
#79238=CARTESIAN_POINT('',(159.783151399344,3.56998646259308,48.35));
#79239=CARTESIAN_POINT('',(159.783151399344,3.56998646259308,48.5));
#79240=CARTESIAN_POINT('',(159.783151399344,3.56998646259308,48.35));
#79241=CARTESIAN_POINT('Origin',(158.689154338092,3.56998646259308,48.5));
#79242=CARTESIAN_POINT('',(158.689154338092,3.56998646259308,48.5));
#79243=CARTESIAN_POINT('',(79.3445771690458,3.56998646259308,48.5));
#79244=CARTESIAN_POINT('',(158.689154338092,3.56998646259308,48.35));
#79245=CARTESIAN_POINT('',(158.689154338092,3.56998646259308,48.5));
#79246=CARTESIAN_POINT('',(158.689154338092,3.56998646259308,48.35));
#79247=CARTESIAN_POINT('Origin',(158.476057451218,2.43997284770012,48.5));
#79248=CARTESIAN_POINT('',(158.476057451218,2.43997284770012,48.5));
#79249=CARTESIAN_POINT('',(156.261207188242,-9.30497091396423,48.5));
#79250=CARTESIAN_POINT('',(158.476057451218,2.43997284770012,48.35));
#79251=CARTESIAN_POINT('',(158.476057451218,2.43997284770012,48.5));
#79252=CARTESIAN_POINT('',(158.476057451218,2.43997284770012,48.35));
#79253=CARTESIAN_POINT('Origin',(158.72967268154,2.40695783495903,48.5));
#79254=CARTESIAN_POINT('',(158.72967268154,2.40695783495903,48.5));
#79255=CARTESIAN_POINT('',(80.3293789433537,12.6129170487894,48.5));
#79256=CARTESIAN_POINT('',(158.72967268154,2.40695783495903,48.35));
#79257=CARTESIAN_POINT('',(158.72967268154,2.40695783495903,48.5));
#79258=CARTESIAN_POINT('',(158.72967268154,2.40695783495903,48.35));
#79259=CARTESIAN_POINT('Ctrl Pts',(158.894747745246,2.56077775359154,48.5));
#79260=CARTESIAN_POINT('Ctrl Pts',(158.894747745246,2.56077775359154,48.35));
#79261=CARTESIAN_POINT('Ctrl Pts',(158.789700072259,2.5015007853508,48.5));
#79262=CARTESIAN_POINT('Ctrl Pts',(158.789700072259,2.5015007853508,48.35));
#79263=CARTESIAN_POINT('Ctrl Pts',(158.72967268154,2.40695783495903,48.5));
#79264=CARTESIAN_POINT('Ctrl Pts',(158.72967268154,2.40695783495903,48.35));
#79265=CARTESIAN_POINT('',(158.894747745246,2.56077775359154,48.5));
#79266=CARTESIAN_POINT('Ctrl Pts',(158.894747745246,2.56077775359154,48.5));
#79267=CARTESIAN_POINT('Ctrl Pts',(158.789700072259,2.5015007853508,48.5));
#79268=CARTESIAN_POINT('Ctrl Pts',(158.72967268154,2.40695783495903,48.5));
#79269=CARTESIAN_POINT('',(158.894747745246,2.56077775359154,48.35));
#79270=CARTESIAN_POINT('',(158.894747745246,2.56077775359154,48.5));
#79271=CARTESIAN_POINT('Ctrl Pts',(158.894747745246,2.56077775359154,48.35));
#79272=CARTESIAN_POINT('Ctrl Pts',(158.789700072259,2.5015007853508,48.35));
#79273=CARTESIAN_POINT('Ctrl Pts',(158.72967268154,2.40695783495903,48.35));
#79274=CARTESIAN_POINT('Ctrl Pts',(159.130354773253,2.62005472183228,48.5));
#79275=CARTESIAN_POINT('Ctrl Pts',(159.130354773253,2.62005472183228,48.35));
#79276=CARTESIAN_POINT('Ctrl Pts',(158.999795567244,2.62005472183228,48.5));
#79277=CARTESIAN_POINT('Ctrl Pts',(158.999795567244,2.62005472183228,48.35));
#79278=CARTESIAN_POINT('Ctrl Pts',(158.894747745246,2.56077775359154,48.5));
#79279=CARTESIAN_POINT('Ctrl Pts',(158.894747745246,2.56077775359154,48.35));
#79280=CARTESIAN_POINT('',(159.130354773253,2.62005472183228,48.5));
#79281=CARTESIAN_POINT('Ctrl Pts',(159.130354773253,2.62005472183228,48.5));
#79282=CARTESIAN_POINT('Ctrl Pts',(158.999795567244,2.62005472183228,48.5));
#79283=CARTESIAN_POINT('Ctrl Pts',(158.894747745246,2.56077775359154,48.5));
#79284=CARTESIAN_POINT('',(159.130354773253,2.62005472183228,48.35));
#79285=CARTESIAN_POINT('',(159.130354773253,2.62005472183228,48.5));
#79286=CARTESIAN_POINT('Ctrl Pts',(159.130354773253,2.62005472183228,48.35));
#79287=CARTESIAN_POINT('Ctrl Pts',(158.999795567244,2.62005472183228,48.35));
#79288=CARTESIAN_POINT('Ctrl Pts',(158.894747745246,2.56077775359154,48.35));
#79289=CARTESIAN_POINT('Ctrl Pts',(159.470259200782,2.48649397492409,48.5));
#79290=CARTESIAN_POINT('Ctrl Pts',(159.470259200782,2.48649397492409,48.35));
#79291=CARTESIAN_POINT('Ctrl Pts',(159.34045041725,2.62005472183228,48.5));
#79292=CARTESIAN_POINT('Ctrl Pts',(159.34045041725,2.62005472183228,48.35));
#79293=CARTESIAN_POINT('Ctrl Pts',(159.130354773253,2.62005472183228,48.5));
#79294=CARTESIAN_POINT('Ctrl Pts',(159.130354773253,2.62005472183228,48.35));
#79295=CARTESIAN_POINT('',(159.470259200782,2.48649397492409,48.5));
#79296=CARTESIAN_POINT('Ctrl Pts',(159.470259200782,2.48649397492409,48.5));
#79297=CARTESIAN_POINT('Ctrl Pts',(159.34045041725,2.62005472183228,48.5));
#79298=CARTESIAN_POINT('Ctrl Pts',(159.130354773253,2.62005472183228,48.5));
#79299=CARTESIAN_POINT('',(159.470259200782,2.48649397492409,48.35));
#79300=CARTESIAN_POINT('',(159.470259200782,2.48649397492409,48.5));
#79301=CARTESIAN_POINT('Ctrl Pts',(159.470259200782,2.48649397492409,48.35));
#79302=CARTESIAN_POINT('Ctrl Pts',(159.34045041725,2.62005472183228,48.35));
#79303=CARTESIAN_POINT('Ctrl Pts',(159.130354773253,2.62005472183228,48.35));
#79304=CARTESIAN_POINT('Ctrl Pts',(159.600068580359,2.12182813882828,48.5));
#79305=CARTESIAN_POINT('Ctrl Pts',(159.600068580359,2.12182813882828,48.35));
#79306=CARTESIAN_POINT('Ctrl Pts',(159.600068580359,2.3529332280159,48.5));
#79307=CARTESIAN_POINT('Ctrl Pts',(159.600068580359,2.3529332280159,48.35));
#79308=CARTESIAN_POINT('Ctrl Pts',(159.470259200782,2.48649397492409,48.5));
#79309=CARTESIAN_POINT('Ctrl Pts',(159.470259200782,2.48649397492409,48.35));
#79310=CARTESIAN_POINT('',(159.600068580359,2.12182813882828,48.5));
#79311=CARTESIAN_POINT('Ctrl Pts',(159.600068580359,2.12182813882828,48.5));
#79312=CARTESIAN_POINT('Ctrl Pts',(159.600068580359,2.3529332280159,48.5));
#79313=CARTESIAN_POINT('Ctrl Pts',(159.470259200782,2.48649397492409,48.5));
#79314=CARTESIAN_POINT('',(159.600068580359,2.12182813882828,48.35));
#79315=CARTESIAN_POINT('',(159.600068580359,2.12182813882828,48.5));
#79316=CARTESIAN_POINT('Ctrl Pts',(159.600068580359,2.12182813882828,48.35));
#79317=CARTESIAN_POINT('Ctrl Pts',(159.600068580359,2.3529332280159,48.35));
#79318=CARTESIAN_POINT('Ctrl Pts',(159.470259200782,2.48649397492409,48.35));
#79319=CARTESIAN_POINT('Ctrl Pts',(159.465006839484,1.73165076971054,48.5));
#79320=CARTESIAN_POINT('Ctrl Pts',(159.465006839484,1.73165076971054,48.35));
#79321=CARTESIAN_POINT('Ctrl Pts',(159.600068580359,1.87871778011322,48.5));
#79322=CARTESIAN_POINT('Ctrl Pts',(159.600068580359,1.87871778011322,48.35));
#79323=CARTESIAN_POINT('Ctrl Pts',(159.600068580359,2.12182813882828,48.5));
#79324=CARTESIAN_POINT('Ctrl Pts',(159.600068580359,2.12182813882828,48.35));
#79325=CARTESIAN_POINT('',(159.465006839484,1.73165076971054,48.5));
#79326=CARTESIAN_POINT('Ctrl Pts',(159.465006839484,1.73165076971054,48.5));
#79327=CARTESIAN_POINT('Ctrl Pts',(159.600068580359,1.87871778011322,48.5));
#79328=CARTESIAN_POINT('Ctrl Pts',(159.600068580359,2.12182813882828,48.5));
#79329=CARTESIAN_POINT('',(159.465006839484,1.73165076971054,48.35));
#79330=CARTESIAN_POINT('',(159.465006839484,1.73165076971054,48.5));
#79331=CARTESIAN_POINT('Ctrl Pts',(159.465006839484,1.73165076971054,48.35));
#79332=CARTESIAN_POINT('Ctrl Pts',(159.600068580359,1.87871778011322,48.35));
#79333=CARTESIAN_POINT('Ctrl Pts',(159.600068580359,2.12182813882828,48.35));
#79334=CARTESIAN_POINT('Ctrl Pts',(159.134857010096,1.58458405733109,48.5));
#79335=CARTESIAN_POINT('Ctrl Pts',(159.134857010096,1.58458405733109,48.35));
#79336=CARTESIAN_POINT('Ctrl Pts',(159.329945545644,1.58458405733109,48.5));
#79337=CARTESIAN_POINT('Ctrl Pts',(159.329945545644,1.58458405733109,48.35));
#79338=CARTESIAN_POINT('Ctrl Pts',(159.465006839484,1.73165076971054,48.5));
#79339=CARTESIAN_POINT('Ctrl Pts',(159.465006839484,1.73165076971054,48.35));
#79340=CARTESIAN_POINT('',(159.134857010096,1.58458405733109,48.5));
#79341=CARTESIAN_POINT('Ctrl Pts',(159.134857010096,1.58458405733109,48.5));
#79342=CARTESIAN_POINT('Ctrl Pts',(159.329945545644,1.58458405733109,48.5));
#79343=CARTESIAN_POINT('Ctrl Pts',(159.465006839484,1.73165076971054,48.5));
#79344=CARTESIAN_POINT('',(159.134857010096,1.58458405733109,48.35));
#79345=CARTESIAN_POINT('',(159.134857010096,1.58458405733109,48.5));
#79346=CARTESIAN_POINT('Ctrl Pts',(159.134857010096,1.58458405733109,48.35));
#79347=CARTESIAN_POINT('Ctrl Pts',(159.329945545644,1.58458405733109,48.35));
#79348=CARTESIAN_POINT('Ctrl Pts',(159.465006839484,1.73165076971054,48.35));
#79349=CARTESIAN_POINT('Ctrl Pts',(158.857981067151,1.68888145685196,48.5));
#79350=CARTESIAN_POINT('Ctrl Pts',(158.857981067151,1.68888145685196,48.35));
#79351=CARTESIAN_POINT('Ctrl Pts',(158.972783338279,1.58458405733109,48.5));
#79352=CARTESIAN_POINT('Ctrl Pts',(158.972783338279,1.58458405733109,48.35));
#79353=CARTESIAN_POINT('Ctrl Pts',(159.134857010096,1.58458405733109,48.5));
#79354=CARTESIAN_POINT('Ctrl Pts',(159.134857010096,1.58458405733109,48.35));
#79355=CARTESIAN_POINT('',(158.857981067151,1.68888145685196,48.5));
#79356=CARTESIAN_POINT('Ctrl Pts',(158.857981067151,1.68888145685196,48.5));
#79357=CARTESIAN_POINT('Ctrl Pts',(158.972783338279,1.58458405733109,48.5));
#79358=CARTESIAN_POINT('Ctrl Pts',(159.134857010096,1.58458405733109,48.5));
#79359=CARTESIAN_POINT('',(158.857981067151,1.68888145685196,48.35));
#79360=CARTESIAN_POINT('',(158.857981067151,1.68888145685196,48.5));
#79361=CARTESIAN_POINT('Ctrl Pts',(158.857981067151,1.68888145685196,48.35));
#79362=CARTESIAN_POINT('Ctrl Pts',(158.972783338279,1.58458405733109,48.35));
#79363=CARTESIAN_POINT('Ctrl Pts',(159.134857010096,1.58458405733109,48.35));
#79364=CARTESIAN_POINT('Ctrl Pts',(158.711664628237,2.00027281045914,48.5));
#79365=CARTESIAN_POINT('Ctrl Pts',(158.711664628237,2.00027281045914,48.35));
#79366=CARTESIAN_POINT('Ctrl Pts',(158.743178796023,1.79317885637283,48.5));
#79367=CARTESIAN_POINT('Ctrl Pts',(158.743178796023,1.79317885637283,48.35));
#79368=CARTESIAN_POINT('Ctrl Pts',(158.857981067151,1.68888145685196,48.5));
#79369=CARTESIAN_POINT('Ctrl Pts',(158.857981067151,1.68888145685196,48.35));
#79370=CARTESIAN_POINT('',(158.711664628237,2.00027281045914,48.5));
#79371=CARTESIAN_POINT('Ctrl Pts',(158.711664628237,2.00027281045914,48.5));
#79372=CARTESIAN_POINT('Ctrl Pts',(158.743178796023,1.79317885637283,48.5));
#79373=CARTESIAN_POINT('Ctrl Pts',(158.857981067151,1.68888145685196,48.5));
#79374=CARTESIAN_POINT('',(158.711664628237,2.00027281045914,48.35));
#79375=CARTESIAN_POINT('',(158.711664628237,2.00027281045914,48.5));
#79376=CARTESIAN_POINT('Ctrl Pts',(158.711664628237,2.00027281045914,48.35));
#79377=CARTESIAN_POINT('Ctrl Pts',(158.743178796023,1.79317885637283,48.35));
#79378=CARTESIAN_POINT('Ctrl Pts',(158.857981067151,1.68888145685196,48.35));
#79379=CARTESIAN_POINT('Origin',(158.428035628051,1.97626197338104,48.5));
#79380=CARTESIAN_POINT('',(158.428035628051,1.97626197338104,48.5));
#79381=CARTESIAN_POINT('',(80.0308315852229,-4.6605152687554,48.5));
#79382=CARTESIAN_POINT('',(158.428035628051,1.97626197338104,48.35));
#79383=CARTESIAN_POINT('',(158.428035628051,1.97626197338104,48.5));
#79384=CARTESIAN_POINT('',(158.428035628051,1.97626197338104,48.35));
#79385=CARTESIAN_POINT('Ctrl Pts',(158.644884180278,1.53055930137634,48.5));
#79386=CARTESIAN_POINT('Ctrl Pts',(158.644884180278,1.53055930137634,48.35));
#79387=CARTESIAN_POINT('Ctrl Pts',(158.455047857016,1.69863575696945,48.5));
#79388=CARTESIAN_POINT('Ctrl Pts',(158.455047857016,1.69863575696945,48.35));
#79389=CARTESIAN_POINT('Ctrl Pts',(158.428035628051,1.97626197338104,48.5));
#79390=CARTESIAN_POINT('Ctrl Pts',(158.428035628051,1.97626197338104,48.35));
#79391=CARTESIAN_POINT('Ctrl Pts',(158.644884180278,1.53055930137634,48.5));
#79392=CARTESIAN_POINT('Ctrl Pts',(158.455047857016,1.69863575696945,48.5));
#79393=CARTESIAN_POINT('Ctrl Pts',(158.428035628051,1.97626197338104,48.5));
#79394=CARTESIAN_POINT('Ctrl Pts',(158.644884180278,1.53055930137634,48.35));
#79395=CARTESIAN_POINT('Ctrl Pts',(158.455047857016,1.69863575696945,48.35));
#79396=CARTESIAN_POINT('Ctrl Pts',(158.428035628051,1.97626197338104,48.35));
#79397=CARTESIAN_POINT('Origin',(159.999999951571,2.48574362695217,48.35));
#79398=CARTESIAN_POINT('Origin',(0.,8.,48.5));
#79399=CARTESIAN_POINT('Ctrl Pts',(150.895907462575,3.38540250062943,48.5));
#79400=CARTESIAN_POINT('Ctrl Pts',(150.895907462575,3.38540250062943,48.35));
#79401=CARTESIAN_POINT('Ctrl Pts',(150.709822655655,3.38540250062943,48.5));
#79402=CARTESIAN_POINT('Ctrl Pts',(150.709822655655,3.38540250062943,48.35));
#79403=CARTESIAN_POINT('Ctrl Pts',(150.598772347905,3.22783091664314,48.5));
#79404=CARTESIAN_POINT('Ctrl Pts',(150.598772347905,3.22783091664314,48.35));
#79405=CARTESIAN_POINT('',(150.895907462575,3.38540250062943,48.5));
#79406=CARTESIAN_POINT('',(150.598772347905,3.22783091664314,48.5));
#79407=CARTESIAN_POINT('Ctrl Pts',(150.895907462575,3.38540250062943,48.5));
#79408=CARTESIAN_POINT('Ctrl Pts',(150.709822655655,3.38540250062943,48.5));
#79409=CARTESIAN_POINT('Ctrl Pts',(150.598772347905,3.22783091664314,48.5));
#79410=CARTESIAN_POINT('',(150.895907462575,3.38540250062943,48.35));
#79411=CARTESIAN_POINT('',(150.895907462575,3.38540250062943,48.5));
#79412=CARTESIAN_POINT('',(150.598772347905,3.22783091664314,48.35));
#79413=CARTESIAN_POINT('Ctrl Pts',(150.895907462575,3.38540250062943,48.35));
#79414=CARTESIAN_POINT('Ctrl Pts',(150.709822655655,3.38540250062943,48.35));
#79415=CARTESIAN_POINT('Ctrl Pts',(150.598772347905,3.22783091664314,48.35));
#79416=CARTESIAN_POINT('',(150.598772347905,3.22783091664314,48.5));
#79417=CARTESIAN_POINT('Ctrl Pts',(151.211800755002,3.2068213224411,48.5));
#79418=CARTESIAN_POINT('Ctrl Pts',(151.211800755002,3.2068213224411,48.35));
#79419=CARTESIAN_POINT('Ctrl Pts',(151.084993065335,3.38540250062943,48.5));
#79420=CARTESIAN_POINT('Ctrl Pts',(151.084993065335,3.38540250062943,48.35));
#79421=CARTESIAN_POINT('Ctrl Pts',(150.895907462575,3.38540250062943,48.5));
#79422=CARTESIAN_POINT('Ctrl Pts',(150.895907462575,3.38540250062943,48.35));
#79423=CARTESIAN_POINT('',(151.211800755002,3.2068213224411,48.5));
#79424=CARTESIAN_POINT('Ctrl Pts',(151.211800755002,3.2068213224411,48.5));
#79425=CARTESIAN_POINT('Ctrl Pts',(151.084993065335,3.38540250062943,48.5));
#79426=CARTESIAN_POINT('Ctrl Pts',(150.895907462575,3.38540250062943,48.5));
#79427=CARTESIAN_POINT('',(151.211800755002,3.2068213224411,48.35));
#79428=CARTESIAN_POINT('',(151.211800755002,3.2068213224411,48.5));
#79429=CARTESIAN_POINT('Ctrl Pts',(151.211800755002,3.2068213224411,48.35));
#79430=CARTESIAN_POINT('Ctrl Pts',(151.084993065335,3.38540250062943,48.35));
#79431=CARTESIAN_POINT('Ctrl Pts',(150.895907462575,3.38540250062943,48.35));
#79432=CARTESIAN_POINT('Ctrl Pts',(151.338608444668,2.48499327898026,48.5));
#79433=CARTESIAN_POINT('Ctrl Pts',(151.338608444668,2.48499327898026,48.35));
#79434=CARTESIAN_POINT('Ctrl Pts',(151.338608444668,3.02824014425278,48.5));
#79435=CARTESIAN_POINT('Ctrl Pts',(151.338608444668,3.02824014425278,48.35));
#79436=CARTESIAN_POINT('Ctrl Pts',(151.211800755002,3.2068213224411,48.5));
#79437=CARTESIAN_POINT('Ctrl Pts',(151.211800755002,3.2068213224411,48.35));
#79438=CARTESIAN_POINT('',(151.338608444668,2.48499327898026,48.5));
#79439=CARTESIAN_POINT('Ctrl Pts',(151.338608444668,2.48499327898026,48.5));
#79440=CARTESIAN_POINT('Ctrl Pts',(151.338608444668,3.02824014425278,48.5));
#79441=CARTESIAN_POINT('Ctrl Pts',(151.211800755002,3.2068213224411,48.5));
#79442=CARTESIAN_POINT('',(151.338608444668,2.48499327898026,48.35));
#79443=CARTESIAN_POINT('',(151.338608444668,2.48499327898026,48.5));
#79444=CARTESIAN_POINT('Ctrl Pts',(151.338608444668,2.48499327898026,48.35));
#79445=CARTESIAN_POINT('Ctrl Pts',(151.338608444668,3.02824014425278,48.35));
#79446=CARTESIAN_POINT('Ctrl Pts',(151.211800755002,3.2068213224411,48.35));
#79447=CARTESIAN_POINT('Ctrl Pts',(151.211800755002,1.76466578245163,48.5));
#79448=CARTESIAN_POINT('Ctrl Pts',(151.211800755002,1.76466578245163,48.35));
#79449=CARTESIAN_POINT('Ctrl Pts',(151.338608444668,1.9447478055954,48.5));
#79450=CARTESIAN_POINT('Ctrl Pts',(151.338608444668,1.9447478055954,48.35));
#79451=CARTESIAN_POINT('Ctrl Pts',(151.338608444668,2.48499327898026,48.5));
#79452=CARTESIAN_POINT('Ctrl Pts',(151.338608444668,2.48499327898026,48.35));
#79453=CARTESIAN_POINT('',(151.211800755002,1.76466578245163,48.5));
#79454=CARTESIAN_POINT('Ctrl Pts',(151.211800755002,1.76466578245163,48.5));
#79455=CARTESIAN_POINT('Ctrl Pts',(151.338608444668,1.9447478055954,48.5));
#79456=CARTESIAN_POINT('Ctrl Pts',(151.338608444668,2.48499327898026,48.5));
#79457=CARTESIAN_POINT('',(151.211800755002,1.76466578245163,48.35));
#79458=CARTESIAN_POINT('',(151.211800755002,1.76466578245163,48.5));
#79459=CARTESIAN_POINT('Ctrl Pts',(151.211800755002,1.76466578245163,48.35));
#79460=CARTESIAN_POINT('Ctrl Pts',(151.338608444668,1.9447478055954,48.35));
#79461=CARTESIAN_POINT('Ctrl Pts',(151.338608444668,2.48499327898026,48.35));
#79462=CARTESIAN_POINT('Ctrl Pts',(150.898908556439,1.58458405733109,48.5));
#79463=CARTESIAN_POINT('Ctrl Pts',(150.898908556439,1.58458405733109,48.35));
#79464=CARTESIAN_POINT('Ctrl Pts',(151.084993065335,1.58458405733109,48.5));
#79465=CARTESIAN_POINT('Ctrl Pts',(151.084993065335,1.58458405733109,48.35));
#79466=CARTESIAN_POINT('Ctrl Pts',(151.211800755002,1.76466578245163,48.5));
#79467=CARTESIAN_POINT('Ctrl Pts',(151.211800755002,1.76466578245163,48.35));
#79468=CARTESIAN_POINT('',(150.898908556439,1.58458405733109,48.5));
#79469=CARTESIAN_POINT('Ctrl Pts',(150.898908556439,1.58458405733109,48.5));
#79470=CARTESIAN_POINT('Ctrl Pts',(151.084993065335,1.58458405733109,48.5));
#79471=CARTESIAN_POINT('Ctrl Pts',(151.211800755002,1.76466578245163,48.5));
#79472=CARTESIAN_POINT('',(150.898908556439,1.58458405733109,48.35));
#79473=CARTESIAN_POINT('',(150.898908556439,1.58458405733109,48.5));
#79474=CARTESIAN_POINT('Ctrl Pts',(150.898908556439,1.58458405733109,48.35));
#79475=CARTESIAN_POINT('Ctrl Pts',(151.084993065335,1.58458405733109,48.35));
#79476=CARTESIAN_POINT('Ctrl Pts',(151.211800755002,1.76466578245163,48.35));
#79477=CARTESIAN_POINT('Ctrl Pts',(150.586016357876,1.76391565799713,48.5));
#79478=CARTESIAN_POINT('Ctrl Pts',(150.586016357876,1.76391565799713,48.35));
#79479=CARTESIAN_POINT('Ctrl Pts',(150.712824047543,1.58458405733109,48.5));
#79480=CARTESIAN_POINT('Ctrl Pts',(150.712824047543,1.58458405733109,48.35));
#79481=CARTESIAN_POINT('Ctrl Pts',(150.898908556439,1.58458405733109,48.5));
#79482=CARTESIAN_POINT('Ctrl Pts',(150.898908556439,1.58458405733109,48.35));
#79483=CARTESIAN_POINT('',(150.586016357876,1.76391565799713,48.5));
#79484=CARTESIAN_POINT('Ctrl Pts',(150.586016357876,1.76391565799713,48.5));
#79485=CARTESIAN_POINT('Ctrl Pts',(150.712824047543,1.58458405733109,48.5));
#79486=CARTESIAN_POINT('Ctrl Pts',(150.898908556439,1.58458405733109,48.5));
#79487=CARTESIAN_POINT('',(150.586016357876,1.76391565799713,48.35));
#79488=CARTESIAN_POINT('',(150.586016357876,1.76391565799713,48.5));
#79489=CARTESIAN_POINT('Ctrl Pts',(150.586016357876,1.76391565799713,48.35));
#79490=CARTESIAN_POINT('Ctrl Pts',(150.712824047543,1.58458405733109,48.35));
#79491=CARTESIAN_POINT('Ctrl Pts',(150.898908556439,1.58458405733109,48.35));
#79492=CARTESIAN_POINT('Ctrl Pts',(150.45920866821,2.48499327898026,48.5));
#79493=CARTESIAN_POINT('Ctrl Pts',(150.45920866821,2.48499327898026,48.35));
#79494=CARTESIAN_POINT('Ctrl Pts',(150.45920866821,1.94324696063995,48.5));
#79495=CARTESIAN_POINT('Ctrl Pts',(150.45920866821,1.94324696063995,48.35));
#79496=CARTESIAN_POINT('Ctrl Pts',(150.586016357876,1.76391565799713,48.5));
#79497=CARTESIAN_POINT('Ctrl Pts',(150.586016357876,1.76391565799713,48.35));
#79498=CARTESIAN_POINT('',(150.45920866821,2.48499327898026,48.5));
#79499=CARTESIAN_POINT('Ctrl Pts',(150.45920866821,2.48499327898026,48.5));
#79500=CARTESIAN_POINT('Ctrl Pts',(150.45920866821,1.94324696063995,48.5));
#79501=CARTESIAN_POINT('Ctrl Pts',(150.586016357876,1.76391565799713,48.5));
#79502=CARTESIAN_POINT('',(150.45920866821,2.48499327898026,48.35));
#79503=CARTESIAN_POINT('',(150.45920866821,2.48499327898026,48.5));
#79504=CARTESIAN_POINT('Ctrl Pts',(150.45920866821,2.48499327898026,48.35));
#79505=CARTESIAN_POINT('Ctrl Pts',(150.45920866821,1.94324696063995,48.35));
#79506=CARTESIAN_POINT('Ctrl Pts',(150.586016357876,1.76391565799713,48.35));
#79507=CARTESIAN_POINT('Ctrl Pts',(150.598772347905,3.22783091664314,48.5));
#79508=CARTESIAN_POINT('Ctrl Pts',(150.598772347905,3.22783091664314,48.35));
#79509=CARTESIAN_POINT('Ctrl Pts',(150.45920866821,3.02673944830894,48.5));
#79510=CARTESIAN_POINT('Ctrl Pts',(150.45920866821,3.02673944830894,48.35));
#79511=CARTESIAN_POINT('Ctrl Pts',(150.45920866821,2.48499327898026,48.5));
#79512=CARTESIAN_POINT('Ctrl Pts',(150.45920866821,2.48499327898026,48.35));
#79513=CARTESIAN_POINT('Ctrl Pts',(150.598772347905,3.22783091664314,48.5));
#79514=CARTESIAN_POINT('Ctrl Pts',(150.45920866821,3.02673944830894,48.5));
#79515=CARTESIAN_POINT('Ctrl Pts',(150.45920866821,2.48499327898026,48.5));
#79516=CARTESIAN_POINT('Ctrl Pts',(150.598772347905,3.22783091664314,48.35));
#79517=CARTESIAN_POINT('Ctrl Pts',(150.45920866821,3.02673944830894,48.35));
#79518=CARTESIAN_POINT('Ctrl Pts',(150.45920866821,2.48499327898026,48.35));
#79519=CARTESIAN_POINT('Ctrl Pts',(150.898908556439,1.36248314380646,48.5));
#79520=CARTESIAN_POINT('Ctrl Pts',(150.898908556439,1.36248314380646,48.35));
#79521=CARTESIAN_POINT('Ctrl Pts',(150.580763996579,1.36248314380646,48.5));
#79522=CARTESIAN_POINT('Ctrl Pts',(150.580763996579,1.36248314380646,48.35));
#79523=CARTESIAN_POINT('Ctrl Pts',(150.399181426503,1.59058684110642,48.5));
#79524=CARTESIAN_POINT('Ctrl Pts',(150.399181426503,1.59058684110642,48.35));
#79525=CARTESIAN_POINT('',(150.898908556439,1.36248314380646,48.5));
#79526=CARTESIAN_POINT('',(150.399181426503,1.59058684110642,48.5));
#79527=CARTESIAN_POINT('Ctrl Pts',(150.898908556439,1.36248314380646,48.5));
#79528=CARTESIAN_POINT('Ctrl Pts',(150.580763996579,1.36248314380646,48.5));
#79529=CARTESIAN_POINT('Ctrl Pts',(150.399181426503,1.59058684110642,48.5));
#79530=CARTESIAN_POINT('',(150.898908556439,1.36248314380646,48.35));
#79531=CARTESIAN_POINT('',(150.898908556439,1.36248314380646,48.5));
#79532=CARTESIAN_POINT('',(150.399181426503,1.59058684110642,48.35));
#79533=CARTESIAN_POINT('Ctrl Pts',(150.898908556439,1.36248314380646,48.35));
#79534=CARTESIAN_POINT('Ctrl Pts',(150.580763996579,1.36248314380646,48.35));
#79535=CARTESIAN_POINT('Ctrl Pts',(150.399181426503,1.59058684110642,48.35));
#79536=CARTESIAN_POINT('',(150.399181426503,1.59058684110642,48.5));
#79537=CARTESIAN_POINT('Ctrl Pts',(151.298840225674,1.49229192733765,48.5));
#79538=CARTESIAN_POINT('Ctrl Pts',(151.298840225674,1.49229192733765,48.35));
#79539=CARTESIAN_POINT('Ctrl Pts',(151.140518368222,1.36248314380646,48.5));
#79540=CARTESIAN_POINT('Ctrl Pts',(151.140518368222,1.36248314380646,48.35));
#79541=CARTESIAN_POINT('Ctrl Pts',(150.898908556439,1.36248314380646,48.5));
#79542=CARTESIAN_POINT('Ctrl Pts',(150.898908556439,1.36248314380646,48.35));
#79543=CARTESIAN_POINT('',(151.298840225674,1.49229192733765,48.5));
#79544=CARTESIAN_POINT('Ctrl Pts',(151.298840225674,1.49229192733765,48.5));
#79545=CARTESIAN_POINT('Ctrl Pts',(151.140518368222,1.36248314380646,48.5));
#79546=CARTESIAN_POINT('Ctrl Pts',(150.898908556439,1.36248314380646,48.5));
#79547=CARTESIAN_POINT('',(151.298840225674,1.49229192733765,48.35));
#79548=CARTESIAN_POINT('',(151.298840225674,1.49229192733765,48.5));
#79549=CARTESIAN_POINT('Ctrl Pts',(151.298840225674,1.49229192733765,48.35));
#79550=CARTESIAN_POINT('Ctrl Pts',(151.140518368222,1.36248314380646,48.35));
#79551=CARTESIAN_POINT('Ctrl Pts',(150.898908556439,1.36248314380646,48.35));
#79552=CARTESIAN_POINT('Ctrl Pts',(151.536698521115,1.85995900630951,48.5));
#79553=CARTESIAN_POINT('Ctrl Pts',(151.536698521115,1.85995900630951,48.35));
#79554=CARTESIAN_POINT('Ctrl Pts',(151.457162083127,1.62210100889206,48.5));
#79555=CARTESIAN_POINT('Ctrl Pts',(151.457162083127,1.62210100889206,48.35));
#79556=CARTESIAN_POINT('Ctrl Pts',(151.298840225674,1.49229192733765,48.5));
#79557=CARTESIAN_POINT('Ctrl Pts',(151.298840225674,1.49229192733765,48.35));
#79558=CARTESIAN_POINT('',(151.536698521115,1.85995900630951,48.5));
#79559=CARTESIAN_POINT('Ctrl Pts',(151.536698521115,1.85995900630951,48.5));
#79560=CARTESIAN_POINT('Ctrl Pts',(151.457162083127,1.62210100889206,48.5));
#79561=CARTESIAN_POINT('Ctrl Pts',(151.298840225674,1.49229192733765,48.5));
#79562=CARTESIAN_POINT('',(151.536698521115,1.85995900630951,48.35));
#79563=CARTESIAN_POINT('',(151.536698521115,1.85995900630951,48.5));
#79564=CARTESIAN_POINT('Ctrl Pts',(151.536698521115,1.85995900630951,48.35));
#79565=CARTESIAN_POINT('Ctrl Pts',(151.457162083127,1.62210100889206,48.35));
#79566=CARTESIAN_POINT('Ctrl Pts',(151.298840225674,1.49229192733765,48.35));
#79567=CARTESIAN_POINT('Ctrl Pts',(151.616234363057,2.48499327898026,48.5));
#79568=CARTESIAN_POINT('Ctrl Pts',(151.616234363057,2.48499327898026,48.35));
#79569=CARTESIAN_POINT('Ctrl Pts',(151.616234363057,2.09781730175018,48.5));
#79570=CARTESIAN_POINT('Ctrl Pts',(151.616234363057,2.09781730175018,48.35));
#79571=CARTESIAN_POINT('Ctrl Pts',(151.536698521115,1.85995900630951,48.5));
#79572=CARTESIAN_POINT('Ctrl Pts',(151.536698521115,1.85995900630951,48.35));
#79573=CARTESIAN_POINT('',(151.616234363057,2.48499327898026,48.5));
#79574=CARTESIAN_POINT('Ctrl Pts',(151.616234363057,2.48499327898026,48.5));
#79575=CARTESIAN_POINT('Ctrl Pts',(151.616234363057,2.09781730175018,48.5));
#79576=CARTESIAN_POINT('Ctrl Pts',(151.536698521115,1.85995900630951,48.5));
#79577=CARTESIAN_POINT('',(151.616234363057,2.48499327898026,48.35));
#79578=CARTESIAN_POINT('',(151.616234363057,2.48499327898026,48.5));
#79579=CARTESIAN_POINT('Ctrl Pts',(151.616234363057,2.48499327898026,48.35));
#79580=CARTESIAN_POINT('Ctrl Pts',(151.616234363057,2.09781730175018,48.35));
#79581=CARTESIAN_POINT('Ctrl Pts',(151.536698521115,1.85995900630951,48.35));
#79582=CARTESIAN_POINT('Ctrl Pts',(151.566711843945,3.00497958064079,48.5));
#79583=CARTESIAN_POINT('Ctrl Pts',(151.566711843945,3.00497958064079,48.35));
#79584=CARTESIAN_POINT('Ctrl Pts',(151.616234363057,2.81214186549187,48.5));
#79585=CARTESIAN_POINT('Ctrl Pts',(151.616234363057,2.81214186549187,48.35));
#79586=CARTESIAN_POINT('Ctrl Pts',(151.616234363057,2.48499327898026,48.5));
#79587=CARTESIAN_POINT('Ctrl Pts',(151.616234363057,2.48499327898026,48.35));
#79588=CARTESIAN_POINT('',(151.566711843945,3.00497958064079,48.5));
#79589=CARTESIAN_POINT('Ctrl Pts',(151.566711843945,3.00497958064079,48.5));
#79590=CARTESIAN_POINT('Ctrl Pts',(151.616234363057,2.81214186549187,48.5));
#79591=CARTESIAN_POINT('Ctrl Pts',(151.616234363057,2.48499327898026,48.5));
#79592=CARTESIAN_POINT('',(151.566711843945,3.00497958064079,48.35));
#79593=CARTESIAN_POINT('',(151.566711843945,3.00497958064079,48.5));
#79594=CARTESIAN_POINT('Ctrl Pts',(151.566711843945,3.00497958064079,48.35));
#79595=CARTESIAN_POINT('Ctrl Pts',(151.616234363057,2.81214186549187,48.35));
#79596=CARTESIAN_POINT('Ctrl Pts',(151.616234363057,2.48499327898026,48.35));
#79597=CARTESIAN_POINT('Ctrl Pts',(151.430149854161,3.33212831616402,48.5));
#79598=CARTESIAN_POINT('Ctrl Pts',(151.430149854161,3.33212831616402,48.35));
#79599=CARTESIAN_POINT('Ctrl Pts',(151.517189324833,3.19781729578972,48.5));
#79600=CARTESIAN_POINT('Ctrl Pts',(151.517189324833,3.19781729578972,48.35));
#79601=CARTESIAN_POINT('Ctrl Pts',(151.566711843945,3.00497958064079,48.5));
#79602=CARTESIAN_POINT('Ctrl Pts',(151.566711843945,3.00497958064079,48.35));
#79603=CARTESIAN_POINT('',(151.430149854161,3.33212831616402,48.5));
#79604=CARTESIAN_POINT('Ctrl Pts',(151.430149854161,3.33212831616402,48.5));
#79605=CARTESIAN_POINT('Ctrl Pts',(151.517189324833,3.19781729578972,48.5));
#79606=CARTESIAN_POINT('Ctrl Pts',(151.566711843945,3.00497958064079,48.5));
#79607=CARTESIAN_POINT('',(151.430149854161,3.33212831616402,48.35));
#79608=CARTESIAN_POINT('',(151.430149854161,3.33212831616402,48.5));
#79609=CARTESIAN_POINT('Ctrl Pts',(151.430149854161,3.33212831616402,48.35));
#79610=CARTESIAN_POINT('Ctrl Pts',(151.517189324833,3.19781729578972,48.35));
#79611=CARTESIAN_POINT('Ctrl Pts',(151.566711843945,3.00497958064079,48.35));
#79612=CARTESIAN_POINT('Ctrl Pts',(151.209550083615,3.5377217233181,48.5));
#79613=CARTESIAN_POINT('Ctrl Pts',(151.209550083615,3.5377217233181,48.35));
#79614=CARTESIAN_POINT('Ctrl Pts',(151.343110383488,3.46643933653831,48.5));
#79615=CARTESIAN_POINT('Ctrl Pts',(151.343110383488,3.46643933653831,48.35));
#79616=CARTESIAN_POINT('Ctrl Pts',(151.430149854161,3.33212831616402,48.5));
#79617=CARTESIAN_POINT('Ctrl Pts',(151.430149854161,3.33212831616402,48.35));
#79618=CARTESIAN_POINT('',(151.209550083615,3.5377217233181,48.5));
#79619=CARTESIAN_POINT('Ctrl Pts',(151.209550083615,3.5377217233181,48.5));
#79620=CARTESIAN_POINT('Ctrl Pts',(151.343110383488,3.46643933653831,48.5));
#79621=CARTESIAN_POINT('Ctrl Pts',(151.430149854161,3.33212831616402,48.5));
#79622=CARTESIAN_POINT('',(151.209550083615,3.5377217233181,48.35));
#79623=CARTESIAN_POINT('',(151.209550083615,3.5377217233181,48.5));
#79624=CARTESIAN_POINT('Ctrl Pts',(151.209550083615,3.5377217233181,48.35));
#79625=CARTESIAN_POINT('Ctrl Pts',(151.343110383488,3.46643933653831,48.35));
#79626=CARTESIAN_POINT('Ctrl Pts',(151.430149854161,3.33212831616402,48.35));
#79627=CARTESIAN_POINT('Ctrl Pts',(150.898908556439,3.60900411009789,48.5));
#79628=CARTESIAN_POINT('Ctrl Pts',(150.898908556439,3.60900411009789,48.35));
#79629=CARTESIAN_POINT('Ctrl Pts',(151.075989187695,3.60900411009789,48.5));
#79630=CARTESIAN_POINT('Ctrl Pts',(151.075989187695,3.60900411009789,48.35));
#79631=CARTESIAN_POINT('Ctrl Pts',(151.209550083615,3.5377217233181,48.5));
#79632=CARTESIAN_POINT('Ctrl Pts',(151.209550083615,3.5377217233181,48.35));
#79633=CARTESIAN_POINT('',(150.898908556439,3.60900411009789,48.5));
#79634=CARTESIAN_POINT('Ctrl Pts',(150.898908556439,3.60900411009789,48.5));
#79635=CARTESIAN_POINT('Ctrl Pts',(151.075989187695,3.60900411009789,48.5));
#79636=CARTESIAN_POINT('Ctrl Pts',(151.209550083615,3.5377217233181,48.5));
#79637=CARTESIAN_POINT('',(150.898908556439,3.60900411009789,48.35));
#79638=CARTESIAN_POINT('',(150.898908556439,3.60900411009789,48.5));
#79639=CARTESIAN_POINT('Ctrl Pts',(150.898908556439,3.60900411009789,48.35));
#79640=CARTESIAN_POINT('Ctrl Pts',(151.075989187695,3.60900411009789,48.35));
#79641=CARTESIAN_POINT('Ctrl Pts',(151.209550083615,3.5377217233181,48.35));
#79642=CARTESIAN_POINT('Ctrl Pts',(150.500477732159,3.47994545102119,48.5));
#79643=CARTESIAN_POINT('Ctrl Pts',(150.500477732159,3.47994545102119,48.35));
#79644=CARTESIAN_POINT('Ctrl Pts',(150.658799589612,3.60900411009789,48.5));
#79645=CARTESIAN_POINT('Ctrl Pts',(150.658799589612,3.60900411009789,48.35));
#79646=CARTESIAN_POINT('Ctrl Pts',(150.898908556439,3.60900411009789,48.5));
#79647=CARTESIAN_POINT('Ctrl Pts',(150.898908556439,3.60900411009789,48.35));
#79648=CARTESIAN_POINT('',(150.500477732159,3.47994545102119,48.5));
#79649=CARTESIAN_POINT('Ctrl Pts',(150.500477732159,3.47994545102119,48.5));
#79650=CARTESIAN_POINT('Ctrl Pts',(150.658799589612,3.60900411009789,48.5));
#79651=CARTESIAN_POINT('Ctrl Pts',(150.898908556439,3.60900411009789,48.5));
#79652=CARTESIAN_POINT('',(150.500477732159,3.47994545102119,48.35));
#79653=CARTESIAN_POINT('',(150.500477732159,3.47994545102119,48.5));
#79654=CARTESIAN_POINT('Ctrl Pts',(150.500477732159,3.47994545102119,48.35));
#79655=CARTESIAN_POINT('Ctrl Pts',(150.658799589612,3.60900411009789,48.35));
#79656=CARTESIAN_POINT('Ctrl Pts',(150.898908556439,3.60900411009789,48.35));
#79657=CARTESIAN_POINT('Ctrl Pts',(150.261869014241,3.11302864551544,48.5));
#79658=CARTESIAN_POINT('Ctrl Pts',(150.261869014241,3.11302864551544,48.35));
#79659=CARTESIAN_POINT('Ctrl Pts',(150.342155576684,3.3508867919445,48.5));
#79660=CARTESIAN_POINT('Ctrl Pts',(150.342155576684,3.3508867919445,48.35));
#79661=CARTESIAN_POINT('Ctrl Pts',(150.500477732159,3.47994545102119,48.5));
#79662=CARTESIAN_POINT('Ctrl Pts',(150.500477732159,3.47994545102119,48.35));
#79663=CARTESIAN_POINT('',(150.261869014241,3.11302864551544,48.5));
#79664=CARTESIAN_POINT('Ctrl Pts',(150.261869014241,3.11302864551544,48.5));
#79665=CARTESIAN_POINT('Ctrl Pts',(150.342155576684,3.3508867919445,48.5));
#79666=CARTESIAN_POINT('Ctrl Pts',(150.500477732159,3.47994545102119,48.5));
#79667=CARTESIAN_POINT('',(150.261869014241,3.11302864551544,48.35));
#79668=CARTESIAN_POINT('',(150.261869014241,3.11302864551544,48.5));
#79669=CARTESIAN_POINT('Ctrl Pts',(150.261869014241,3.11302864551544,48.35));
#79670=CARTESIAN_POINT('Ctrl Pts',(150.342155576684,3.3508867919445,48.35));
#79671=CARTESIAN_POINT('Ctrl Pts',(150.500477732159,3.47994545102119,48.35));
#79672=CARTESIAN_POINT('Ctrl Pts',(150.181582749821,2.48499327898026,48.5));
#79673=CARTESIAN_POINT('Ctrl Pts',(150.181582749821,2.48499327898026,48.35));
#79674=CARTESIAN_POINT('Ctrl Pts',(150.181582749821,2.87517049908638,48.5));
#79675=CARTESIAN_POINT('Ctrl Pts',(150.181582749821,2.87517049908638,48.35));
#79676=CARTESIAN_POINT('Ctrl Pts',(150.261869014241,3.11302864551544,48.5));
#79677=CARTESIAN_POINT('Ctrl Pts',(150.261869014241,3.11302864551544,48.35));
#79678=CARTESIAN_POINT('',(150.181582749821,2.48499327898026,48.5));
#79679=CARTESIAN_POINT('Ctrl Pts',(150.181582749821,2.48499327898026,48.5));
#79680=CARTESIAN_POINT('Ctrl Pts',(150.181582749821,2.87517049908638,48.5));
#79681=CARTESIAN_POINT('Ctrl Pts',(150.261869014241,3.11302864551544,48.5));
#79682=CARTESIAN_POINT('',(150.181582749821,2.48499327898026,48.35));
#79683=CARTESIAN_POINT('',(150.181582749821,2.48499327898026,48.5));
#79684=CARTESIAN_POINT('Ctrl Pts',(150.181582749821,2.48499327898026,48.35));
#79685=CARTESIAN_POINT('Ctrl Pts',(150.181582749821,2.87517049908638,48.35));
#79686=CARTESIAN_POINT('Ctrl Pts',(150.261869014241,3.11302864551544,48.35));
#79687=CARTESIAN_POINT('Ctrl Pts',(150.399181426503,1.59058684110642,48.5));
#79688=CARTESIAN_POINT('Ctrl Pts',(150.399181426503,1.59058684110642,48.35));
#79689=CARTESIAN_POINT('Ctrl Pts',(150.181582749821,1.86521166563034,48.5));
#79690=CARTESIAN_POINT('Ctrl Pts',(150.181582749821,1.86521166563034,48.35));
#79691=CARTESIAN_POINT('Ctrl Pts',(150.181582749821,2.48499327898026,48.5));
#79692=CARTESIAN_POINT('Ctrl Pts',(150.181582749821,2.48499327898026,48.35));
#79693=CARTESIAN_POINT('Ctrl Pts',(150.399181426503,1.59058684110642,48.5));
#79694=CARTESIAN_POINT('Ctrl Pts',(150.181582749821,1.86521166563034,48.5));
#79695=CARTESIAN_POINT('Ctrl Pts',(150.181582749821,2.48499327898026,48.5));
#79696=CARTESIAN_POINT('Ctrl Pts',(150.399181426503,1.59058684110642,48.35));
#79697=CARTESIAN_POINT('Ctrl Pts',(150.181582749821,1.86521166563034,48.35));
#79698=CARTESIAN_POINT('Ctrl Pts',(150.181582749821,2.48499327898026,48.35));
#79699=CARTESIAN_POINT('Origin',(149.999999956228,2.48574362695217,48.35));
#79700=CARTESIAN_POINT('Origin',(149.338199377991,3.16630297899246,48.5));
#79701=CARTESIAN_POINT('',(149.338199377991,3.16630297899246,48.5));
#79702=CARTESIAN_POINT('',(148.64938619826,2.17435204982758,48.5));
#79703=CARTESIAN_POINT('',(126.178769980074,-30.1852910180208,48.5));
#79704=CARTESIAN_POINT('',(149.338199377991,3.16630297899246,48.35));
#79705=CARTESIAN_POINT('',(149.338199377991,3.16630297899246,48.5));
#79706=CARTESIAN_POINT('',(148.64938619826,2.17435204982758,48.35));
#79707=CARTESIAN_POINT('',(149.338199377991,3.16630297899246,48.35));
#79708=CARTESIAN_POINT('',(148.64938619826,2.17435204982758,48.5));
#79709=CARTESIAN_POINT('Origin',(149.338199377991,2.17435204982758,48.5));
#79710=CARTESIAN_POINT('',(149.338199377991,2.17435204982758,48.5));
#79711=CARTESIAN_POINT('',(149.338199377991,5.08717602491379,48.5));
#79712=CARTESIAN_POINT('',(149.338199377991,2.17435204982758,48.35));
#79713=CARTESIAN_POINT('',(149.338199377991,2.17435204982758,48.5));
#79714=CARTESIAN_POINT('',(149.338199377991,2.17435204982758,48.35));
#79715=CARTESIAN_POINT('Origin',(148.64938619826,2.17435204982758,48.5));
#79716=CARTESIAN_POINT('',(74.3246930991299,2.17435204982758,48.5));
#79717=CARTESIAN_POINT('',(148.64938619826,2.17435204982758,48.35));
#79718=CARTESIAN_POINT('Origin',(149.608321965672,1.92673945426941,48.5));
#79719=CARTESIAN_POINT('',(149.608321965672,1.92673945426941,48.5));
#79720=CARTESIAN_POINT('',(149.608321965672,1.40000009536743,48.5));
#79721=CARTESIAN_POINT('',(149.608321965672,4.9633697271347,48.5));
#79722=CARTESIAN_POINT('',(149.608321965672,1.92673945426941,48.35));
#79723=CARTESIAN_POINT('',(149.608321965672,1.92673945426941,48.5));
#79724=CARTESIAN_POINT('',(149.608321965672,1.40000009536743,48.35));
#79725=CARTESIAN_POINT('',(149.608321965672,1.92673945426941,48.35));
#79726=CARTESIAN_POINT('',(149.608321965672,1.40000009536743,48.5));
#79727=CARTESIAN_POINT('Origin',(149.905457080342,1.92673945426941,48.5));
#79728=CARTESIAN_POINT('',(149.905457080342,1.92673945426941,48.5));
#79729=CARTESIAN_POINT('',(74.9527285401709,1.92673945426941,48.5));
#79730=CARTESIAN_POINT('',(149.905457080342,1.92673945426941,48.35));
#79731=CARTESIAN_POINT('',(149.905457080342,1.92673945426941,48.5));
#79732=CARTESIAN_POINT('',(149.905457080342,1.92673945426941,48.35));
#79733=CARTESIAN_POINT('Origin',(149.905457080342,2.17435204982758,48.5));
#79734=CARTESIAN_POINT('',(149.905457080342,2.17435204982758,48.5));
#79735=CARTESIAN_POINT('',(149.905457080342,5.08717602491379,48.5));
#79736=CARTESIAN_POINT('',(149.905457080342,2.17435204982758,48.35));
#79737=CARTESIAN_POINT('',(149.905457080342,2.17435204982758,48.5));
#79738=CARTESIAN_POINT('',(149.905457080342,2.17435204982758,48.35));
#79739=CARTESIAN_POINT('Origin',(149.608321965672,2.17435204982758,48.5));
#79740=CARTESIAN_POINT('',(149.608321965672,2.17435204982758,48.5));
#79741=CARTESIAN_POINT('',(74.804160982836,2.17435204982758,48.5));
#79742=CARTESIAN_POINT('',(149.608321965672,2.17435204982758,48.35));
#79743=CARTESIAN_POINT('',(149.608321965672,2.17435204982758,48.5));
#79744=CARTESIAN_POINT('',(149.608321965672,2.17435204982758,48.35));
#79745=CARTESIAN_POINT('Origin',(149.608321965672,3.6000000834465,48.5));
#79746=CARTESIAN_POINT('',(149.608321965672,3.6000000834465,48.5));
#79747=CARTESIAN_POINT('',(149.608321965672,5.80000004172325,48.5));
#79748=CARTESIAN_POINT('',(149.608321965672,3.6000000834465,48.35));
#79749=CARTESIAN_POINT('',(149.608321965672,3.6000000834465,48.5));
#79750=CARTESIAN_POINT('',(149.608321965672,3.6000000834465,48.35));
#79751=CARTESIAN_POINT('Origin',(149.387721897103,3.6000000834465,48.5));
#79752=CARTESIAN_POINT('',(149.387721897103,3.6000000834465,48.5));
#79753=CARTESIAN_POINT('',(74.6938609485514,3.6000000834465,48.5));
#79754=CARTESIAN_POINT('',(149.387721897103,3.6000000834465,48.35));
#79755=CARTESIAN_POINT('',(149.387721897103,3.6000000834465,48.5));
#79756=CARTESIAN_POINT('',(149.387721897103,3.6000000834465,48.35));
#79757=CARTESIAN_POINT('Origin',(148.383765549399,2.17435204982758,48.5));
#79758=CARTESIAN_POINT('',(148.383765549399,2.17435204982758,48.5));
#79759=CARTESIAN_POINT('',(125.159520291088,-30.8047706585614,48.5));
#79760=CARTESIAN_POINT('',(148.383765549399,2.17435204982758,48.35));
#79761=CARTESIAN_POINT('',(148.383765549399,2.17435204982758,48.5));
#79762=CARTESIAN_POINT('',(148.383765549399,2.17435204982758,48.35));
#79763=CARTESIAN_POINT('Origin',(148.383765549399,1.92673945426941,48.5));
#79764=CARTESIAN_POINT('',(148.383765549399,1.92673945426941,48.5));
#79765=CARTESIAN_POINT('',(148.383765549399,4.9633697271347,48.5));
#79766=CARTESIAN_POINT('',(148.383765549399,1.92673945426941,48.35));
#79767=CARTESIAN_POINT('',(148.383765549399,1.92673945426941,48.5));
#79768=CARTESIAN_POINT('',(148.383765549399,1.92673945426941,48.35));
#79769=CARTESIAN_POINT('Origin',(149.338199377991,1.92673945426941,48.5));
#79770=CARTESIAN_POINT('',(149.338199377991,1.92673945426941,48.5));
#79771=CARTESIAN_POINT('',(74.6690996889956,1.92673945426941,48.5));
#79772=CARTESIAN_POINT('',(149.338199377991,1.92673945426941,48.35));
#79773=CARTESIAN_POINT('',(149.338199377991,1.92673945426941,48.5));
#79774=CARTESIAN_POINT('',(149.338199377991,1.92673945426941,48.35));
#79775=CARTESIAN_POINT('Origin',(149.338199377991,1.40000009536743,48.5));
#79776=CARTESIAN_POINT('',(149.338199377991,1.40000009536743,48.5));
#79777=CARTESIAN_POINT('',(149.338199377991,4.70000004768372,48.5));
#79778=CARTESIAN_POINT('',(149.338199377991,1.40000009536743,48.35));
#79779=CARTESIAN_POINT('',(149.338199377991,1.40000009536743,48.5));
#79780=CARTESIAN_POINT('',(149.338199377991,1.40000009536743,48.35));
#79781=CARTESIAN_POINT('Origin',(149.608321965672,1.40000009536743,48.5));
#79782=CARTESIAN_POINT('',(74.804160982836,1.40000009536743,48.5));
#79783=CARTESIAN_POINT('',(149.608321965672,1.40000009536743,48.35));
#79784=CARTESIAN_POINT('Origin',(149.999999956228,2.48574362695217,48.35));
#79785=CARTESIAN_POINT('Origin',(0.,8.,48.5));
#79786=CARTESIAN_POINT('Origin',(0.,8.,48.5));
#79787=CARTESIAN_POINT('Ctrl Pts',(140.850886523724,3.38540250062943,48.5));
#79788=CARTESIAN_POINT('Ctrl Pts',(140.850886523724,3.38540250062943,48.35));
#79789=CARTESIAN_POINT('Ctrl Pts',(140.664802014828,3.38540250062943,48.5));
#79790=CARTESIAN_POINT('Ctrl Pts',(140.664802014828,3.38540250062943,48.35));
#79791=CARTESIAN_POINT('Ctrl Pts',(140.553751409054,3.22783091664314,48.5));
#79792=CARTESIAN_POINT('Ctrl Pts',(140.553751409054,3.22783091664314,48.35));
#79793=CARTESIAN_POINT('',(140.850886523724,3.38540250062943,48.5));
#79794=CARTESIAN_POINT('',(140.553751409054,3.22783091664314,48.5));
#79795=CARTESIAN_POINT('Ctrl Pts',(140.850886523724,3.38540250062943,48.5));
#79796=CARTESIAN_POINT('Ctrl Pts',(140.664802014828,3.38540250062943,48.5));
#79797=CARTESIAN_POINT('Ctrl Pts',(140.553751409054,3.22783091664314,48.5));
#79798=CARTESIAN_POINT('',(140.850886523724,3.38540250062943,48.35));
#79799=CARTESIAN_POINT('',(140.850886523724,3.38540250062943,48.5));
#79800=CARTESIAN_POINT('',(140.553751409054,3.22783091664314,48.35));
#79801=CARTESIAN_POINT('Ctrl Pts',(140.850886523724,3.38540250062943,48.35));
#79802=CARTESIAN_POINT('Ctrl Pts',(140.664802014828,3.38540250062943,48.35));
#79803=CARTESIAN_POINT('Ctrl Pts',(140.553751409054,3.22783091664314,48.35));
#79804=CARTESIAN_POINT('',(140.553751409054,3.22783091664314,48.5));
#79805=CARTESIAN_POINT('Ctrl Pts',(141.166780412197,3.2068213224411,48.5));
#79806=CARTESIAN_POINT('Ctrl Pts',(141.166780412197,3.2068213224411,48.35));
#79807=CARTESIAN_POINT('Ctrl Pts',(141.03997272253,3.38540250062943,48.5));
#79808=CARTESIAN_POINT('Ctrl Pts',(141.03997272253,3.38540250062943,48.35));
#79809=CARTESIAN_POINT('Ctrl Pts',(140.850886523724,3.38540250062943,48.5));
#79810=CARTESIAN_POINT('Ctrl Pts',(140.850886523724,3.38540250062943,48.35));
#79811=CARTESIAN_POINT('',(141.166780412197,3.2068213224411,48.5));
#79812=CARTESIAN_POINT('Ctrl Pts',(141.166780412197,3.2068213224411,48.5));
#79813=CARTESIAN_POINT('Ctrl Pts',(141.03997272253,3.38540250062943,48.5));
#79814=CARTESIAN_POINT('Ctrl Pts',(140.850886523724,3.38540250062943,48.5));
#79815=CARTESIAN_POINT('',(141.166780412197,3.2068213224411,48.35));
#79816=CARTESIAN_POINT('',(141.166780412197,3.2068213224411,48.5));
#79817=CARTESIAN_POINT('Ctrl Pts',(141.166780412197,3.2068213224411,48.35));
#79818=CARTESIAN_POINT('Ctrl Pts',(141.03997272253,3.38540250062943,48.35));
#79819=CARTESIAN_POINT('Ctrl Pts',(140.850886523724,3.38540250062943,48.35));
#79820=CARTESIAN_POINT('Ctrl Pts',(141.293588101864,2.48499327898026,48.5));
#79821=CARTESIAN_POINT('Ctrl Pts',(141.293588101864,2.48499327898026,48.35));
#79822=CARTESIAN_POINT('Ctrl Pts',(141.293588101864,3.02824014425278,48.5));
#79823=CARTESIAN_POINT('Ctrl Pts',(141.293588101864,3.02824014425278,48.35));
#79824=CARTESIAN_POINT('Ctrl Pts',(141.166780412197,3.2068213224411,48.5));
#79825=CARTESIAN_POINT('Ctrl Pts',(141.166780412197,3.2068213224411,48.35));
#79826=CARTESIAN_POINT('',(141.293588101864,2.48499327898026,48.5));
#79827=CARTESIAN_POINT('Ctrl Pts',(141.293588101864,2.48499327898026,48.5));
#79828=CARTESIAN_POINT('Ctrl Pts',(141.293588101864,3.02824014425278,48.5));
#79829=CARTESIAN_POINT('Ctrl Pts',(141.166780412197,3.2068213224411,48.5));
#79830=CARTESIAN_POINT('',(141.293588101864,2.48499327898026,48.35));
#79831=CARTESIAN_POINT('',(141.293588101864,2.48499327898026,48.5));
#79832=CARTESIAN_POINT('Ctrl Pts',(141.293588101864,2.48499327898026,48.35));
#79833=CARTESIAN_POINT('Ctrl Pts',(141.293588101864,3.02824014425278,48.35));
#79834=CARTESIAN_POINT('Ctrl Pts',(141.166780412197,3.2068213224411,48.35));
#79835=CARTESIAN_POINT('Ctrl Pts',(141.166780412197,1.76466578245163,48.5));
#79836=CARTESIAN_POINT('Ctrl Pts',(141.166780412197,1.76466578245163,48.35));
#79837=CARTESIAN_POINT('Ctrl Pts',(141.293588101864,1.9447478055954,48.5));
#79838=CARTESIAN_POINT('Ctrl Pts',(141.293588101864,1.9447478055954,48.35));
#79839=CARTESIAN_POINT('Ctrl Pts',(141.293588101864,2.48499327898026,48.5));
#79840=CARTESIAN_POINT('Ctrl Pts',(141.293588101864,2.48499327898026,48.35));
#79841=CARTESIAN_POINT('',(141.166780412197,1.76466578245163,48.5));
#79842=CARTESIAN_POINT('Ctrl Pts',(141.166780412197,1.76466578245163,48.5));
#79843=CARTESIAN_POINT('Ctrl Pts',(141.293588101864,1.9447478055954,48.5));
#79844=CARTESIAN_POINT('Ctrl Pts',(141.293588101864,2.48499327898026,48.5));
#79845=CARTESIAN_POINT('',(141.166780412197,1.76466578245163,48.35));
#79846=CARTESIAN_POINT('',(141.166780412197,1.76466578245163,48.5));
#79847=CARTESIAN_POINT('Ctrl Pts',(141.166780412197,1.76466578245163,48.35));
#79848=CARTESIAN_POINT('Ctrl Pts',(141.293588101864,1.9447478055954,48.35));
#79849=CARTESIAN_POINT('Ctrl Pts',(141.293588101864,2.48499327898026,48.35));
#79850=CARTESIAN_POINT('Ctrl Pts',(140.853888213634,1.58458405733109,48.5));
#79851=CARTESIAN_POINT('Ctrl Pts',(140.853888213634,1.58458405733109,48.35));
#79852=CARTESIAN_POINT('Ctrl Pts',(141.03997272253,1.58458405733109,48.5));
#79853=CARTESIAN_POINT('Ctrl Pts',(141.03997272253,1.58458405733109,48.35));
#79854=CARTESIAN_POINT('Ctrl Pts',(141.166780412197,1.76466578245163,48.5));
#79855=CARTESIAN_POINT('Ctrl Pts',(141.166780412197,1.76466578245163,48.35));
#79856=CARTESIAN_POINT('',(140.853888213634,1.58458405733109,48.5));
#79857=CARTESIAN_POINT('Ctrl Pts',(140.853888213634,1.58458405733109,48.5));
#79858=CARTESIAN_POINT('Ctrl Pts',(141.03997272253,1.58458405733109,48.5));
#79859=CARTESIAN_POINT('Ctrl Pts',(141.166780412197,1.76466578245163,48.5));
#79860=CARTESIAN_POINT('',(140.853888213634,1.58458405733109,48.35));
#79861=CARTESIAN_POINT('',(140.853888213634,1.58458405733109,48.5));
#79862=CARTESIAN_POINT('Ctrl Pts',(140.853888213634,1.58458405733109,48.35));
#79863=CARTESIAN_POINT('Ctrl Pts',(141.03997272253,1.58458405733109,48.35));
#79864=CARTESIAN_POINT('Ctrl Pts',(141.166780412197,1.76466578245163,48.35));
#79865=CARTESIAN_POINT('Ctrl Pts',(140.540996015072,1.76391565799713,48.5));
#79866=CARTESIAN_POINT('Ctrl Pts',(140.540996015072,1.76391565799713,48.35));
#79867=CARTESIAN_POINT('Ctrl Pts',(140.667803406715,1.58458405733109,48.5));
#79868=CARTESIAN_POINT('Ctrl Pts',(140.667803406715,1.58458405733109,48.35));
#79869=CARTESIAN_POINT('Ctrl Pts',(140.853888213634,1.58458405733109,48.5));
#79870=CARTESIAN_POINT('Ctrl Pts',(140.853888213634,1.58458405733109,48.35));
#79871=CARTESIAN_POINT('',(140.540996015072,1.76391565799713,48.5));
#79872=CARTESIAN_POINT('Ctrl Pts',(140.540996015072,1.76391565799713,48.5));
#79873=CARTESIAN_POINT('Ctrl Pts',(140.667803406715,1.58458405733109,48.5));
#79874=CARTESIAN_POINT('Ctrl Pts',(140.853888213634,1.58458405733109,48.5));
#79875=CARTESIAN_POINT('',(140.540996015072,1.76391565799713,48.35));
#79876=CARTESIAN_POINT('',(140.540996015072,1.76391565799713,48.5));
#79877=CARTESIAN_POINT('Ctrl Pts',(140.540996015072,1.76391565799713,48.35));
#79878=CARTESIAN_POINT('Ctrl Pts',(140.667803406715,1.58458405733109,48.35));
#79879=CARTESIAN_POINT('Ctrl Pts',(140.853888213634,1.58458405733109,48.35));
#79880=CARTESIAN_POINT('Ctrl Pts',(140.414188325405,2.48499327898026,48.5));
#79881=CARTESIAN_POINT('Ctrl Pts',(140.414188325405,2.48499327898026,48.35));
#79882=CARTESIAN_POINT('Ctrl Pts',(140.414188325405,1.94324696063995,48.5));
#79883=CARTESIAN_POINT('Ctrl Pts',(140.414188325405,1.94324696063995,48.35));
#79884=CARTESIAN_POINT('Ctrl Pts',(140.540996015072,1.76391565799713,48.5));
#79885=CARTESIAN_POINT('Ctrl Pts',(140.540996015072,1.76391565799713,48.35));
#79886=CARTESIAN_POINT('',(140.414188325405,2.48499327898026,48.5));
#79887=CARTESIAN_POINT('Ctrl Pts',(140.414188325405,2.48499327898026,48.5));
#79888=CARTESIAN_POINT('Ctrl Pts',(140.414188325405,1.94324696063995,48.5));
#79889=CARTESIAN_POINT('Ctrl Pts',(140.540996015072,1.76391565799713,48.5));
#79890=CARTESIAN_POINT('',(140.414188325405,2.48499327898026,48.35));
#79891=CARTESIAN_POINT('',(140.414188325405,2.48499327898026,48.5));
#79892=CARTESIAN_POINT('Ctrl Pts',(140.414188325405,2.48499327898026,48.35));
#79893=CARTESIAN_POINT('Ctrl Pts',(140.414188325405,1.94324696063995,48.35));
#79894=CARTESIAN_POINT('Ctrl Pts',(140.540996015072,1.76391565799713,48.35));
#79895=CARTESIAN_POINT('Ctrl Pts',(140.553751409054,3.22783091664314,48.5));
#79896=CARTESIAN_POINT('Ctrl Pts',(140.553751409054,3.22783091664314,48.35));
#79897=CARTESIAN_POINT('Ctrl Pts',(140.414188325405,3.02673944830894,48.5));
#79898=CARTESIAN_POINT('Ctrl Pts',(140.414188325405,3.02673944830894,48.35));
#79899=CARTESIAN_POINT('Ctrl Pts',(140.414188325405,2.48499327898026,48.5));
#79900=CARTESIAN_POINT('Ctrl Pts',(140.414188325405,2.48499327898026,48.35));
#79901=CARTESIAN_POINT('Ctrl Pts',(140.553751409054,3.22783091664314,48.5));
#79902=CARTESIAN_POINT('Ctrl Pts',(140.414188325405,3.02673944830894,48.5));
#79903=CARTESIAN_POINT('Ctrl Pts',(140.414188325405,2.48499327898026,48.5));
#79904=CARTESIAN_POINT('Ctrl Pts',(140.553751409054,3.22783091664314,48.35));
#79905=CARTESIAN_POINT('Ctrl Pts',(140.414188325405,3.02673944830894,48.35));
#79906=CARTESIAN_POINT('Ctrl Pts',(140.414188325405,2.48499327898026,48.35));
#79907=CARTESIAN_POINT('Ctrl Pts',(140.853888213634,1.36248314380646,48.5));
#79908=CARTESIAN_POINT('Ctrl Pts',(140.853888213634,1.36248314380646,48.35));
#79909=CARTESIAN_POINT('Ctrl Pts',(140.535743355751,1.36248314380646,48.5));
#79910=CARTESIAN_POINT('Ctrl Pts',(140.535743355751,1.36248314380646,48.35));
#79911=CARTESIAN_POINT('Ctrl Pts',(140.354161083698,1.59058684110642,48.5));
#79912=CARTESIAN_POINT('Ctrl Pts',(140.354161083698,1.59058684110642,48.35));
#79913=CARTESIAN_POINT('',(140.853888213634,1.36248314380646,48.5));
#79914=CARTESIAN_POINT('',(140.354161083698,1.59058684110642,48.5));
#79915=CARTESIAN_POINT('Ctrl Pts',(140.853888213634,1.36248314380646,48.5));
#79916=CARTESIAN_POINT('Ctrl Pts',(140.535743355751,1.36248314380646,48.5));
#79917=CARTESIAN_POINT('Ctrl Pts',(140.354161083698,1.59058684110642,48.5));
#79918=CARTESIAN_POINT('',(140.853888213634,1.36248314380646,48.35));
#79919=CARTESIAN_POINT('',(140.853888213634,1.36248314380646,48.5));
#79920=CARTESIAN_POINT('',(140.354161083698,1.59058684110642,48.35));
#79921=CARTESIAN_POINT('Ctrl Pts',(140.853888213634,1.36248314380646,48.35));
#79922=CARTESIAN_POINT('Ctrl Pts',(140.535743355751,1.36248314380646,48.35));
#79923=CARTESIAN_POINT('Ctrl Pts',(140.354161083698,1.59058684110642,48.35));
#79924=CARTESIAN_POINT('',(140.354161083698,1.59058684110642,48.5));
#79925=CARTESIAN_POINT('Ctrl Pts',(141.25381988287,1.49229192733765,48.5));
#79926=CARTESIAN_POINT('Ctrl Pts',(141.25381988287,1.49229192733765,48.35));
#79927=CARTESIAN_POINT('Ctrl Pts',(141.095498025417,1.36248314380646,48.5));
#79928=CARTESIAN_POINT('Ctrl Pts',(141.095498025417,1.36248314380646,48.35));
#79929=CARTESIAN_POINT('Ctrl Pts',(140.853888213634,1.36248314380646,48.5));
#79930=CARTESIAN_POINT('Ctrl Pts',(140.853888213634,1.36248314380646,48.35));
#79931=CARTESIAN_POINT('',(141.25381988287,1.49229192733765,48.5));
#79932=CARTESIAN_POINT('Ctrl Pts',(141.25381988287,1.49229192733765,48.5));
#79933=CARTESIAN_POINT('Ctrl Pts',(141.095498025417,1.36248314380646,48.5));
#79934=CARTESIAN_POINT('Ctrl Pts',(140.853888213634,1.36248314380646,48.5));
#79935=CARTESIAN_POINT('',(141.25381988287,1.49229192733765,48.35));
#79936=CARTESIAN_POINT('',(141.25381988287,1.49229192733765,48.5));
#79937=CARTESIAN_POINT('Ctrl Pts',(141.25381988287,1.49229192733765,48.35));
#79938=CARTESIAN_POINT('Ctrl Pts',(141.095498025417,1.36248314380646,48.35));
#79939=CARTESIAN_POINT('Ctrl Pts',(140.853888213634,1.36248314380646,48.35));
#79940=CARTESIAN_POINT('Ctrl Pts',(141.49167817831,1.85995900630951,48.5));
#79941=CARTESIAN_POINT('Ctrl Pts',(141.49167817831,1.85995900630951,48.35));
#79942=CARTESIAN_POINT('Ctrl Pts',(141.412141740322,1.62210100889206,48.5));
#79943=CARTESIAN_POINT('Ctrl Pts',(141.412141740322,1.62210100889206,48.35));
#79944=CARTESIAN_POINT('Ctrl Pts',(141.25381988287,1.49229192733765,48.5));
#79945=CARTESIAN_POINT('Ctrl Pts',(141.25381988287,1.49229192733765,48.35));
#79946=CARTESIAN_POINT('',(141.49167817831,1.85995900630951,48.5));
#79947=CARTESIAN_POINT('Ctrl Pts',(141.49167817831,1.85995900630951,48.5));
#79948=CARTESIAN_POINT('Ctrl Pts',(141.412141740322,1.62210100889206,48.5));
#79949=CARTESIAN_POINT('Ctrl Pts',(141.25381988287,1.49229192733765,48.5));
#79950=CARTESIAN_POINT('',(141.49167817831,1.85995900630951,48.35));
#79951=CARTESIAN_POINT('',(141.49167817831,1.85995900630951,48.5));
#79952=CARTESIAN_POINT('Ctrl Pts',(141.49167817831,1.85995900630951,48.35));
#79953=CARTESIAN_POINT('Ctrl Pts',(141.412141740322,1.62210100889206,48.35));
#79954=CARTESIAN_POINT('Ctrl Pts',(141.25381988287,1.49229192733765,48.35));
#79955=CARTESIAN_POINT('Ctrl Pts',(141.571214020252,2.48499327898026,48.5));
#79956=CARTESIAN_POINT('Ctrl Pts',(141.571214020252,2.48499327898026,48.35));
#79957=CARTESIAN_POINT('Ctrl Pts',(141.571214020252,2.09781730175018,48.5));
#79958=CARTESIAN_POINT('Ctrl Pts',(141.571214020252,2.09781730175018,48.35));
#79959=CARTESIAN_POINT('Ctrl Pts',(141.49167817831,1.85995900630951,48.5));
#79960=CARTESIAN_POINT('Ctrl Pts',(141.49167817831,1.85995900630951,48.35));
#79961=CARTESIAN_POINT('',(141.571214020252,2.48499327898026,48.5));
#79962=CARTESIAN_POINT('Ctrl Pts',(141.571214020252,2.48499327898026,48.5));
#79963=CARTESIAN_POINT('Ctrl Pts',(141.571214020252,2.09781730175018,48.5));
#79964=CARTESIAN_POINT('Ctrl Pts',(141.49167817831,1.85995900630951,48.5));
#79965=CARTESIAN_POINT('',(141.571214020252,2.48499327898026,48.35));
#79966=CARTESIAN_POINT('',(141.571214020252,2.48499327898026,48.5));
#79967=CARTESIAN_POINT('Ctrl Pts',(141.571214020252,2.48499327898026,48.35));
#79968=CARTESIAN_POINT('Ctrl Pts',(141.571214020252,2.09781730175018,48.35));
#79969=CARTESIAN_POINT('Ctrl Pts',(141.49167817831,1.85995900630951,48.35));
#79970=CARTESIAN_POINT('Ctrl Pts',(141.521691501141,3.00497958064079,48.5));
#79971=CARTESIAN_POINT('Ctrl Pts',(141.521691501141,3.00497958064079,48.35));
#79972=CARTESIAN_POINT('Ctrl Pts',(141.571214020252,2.81214186549187,48.5));
#79973=CARTESIAN_POINT('Ctrl Pts',(141.571214020252,2.81214186549187,48.35));
#79974=CARTESIAN_POINT('Ctrl Pts',(141.571214020252,2.48499327898026,48.5));
#79975=CARTESIAN_POINT('Ctrl Pts',(141.571214020252,2.48499327898026,48.35));
#79976=CARTESIAN_POINT('',(141.521691501141,3.00497958064079,48.5));
#79977=CARTESIAN_POINT('Ctrl Pts',(141.521691501141,3.00497958064079,48.5));
#79978=CARTESIAN_POINT('Ctrl Pts',(141.571214020252,2.81214186549187,48.5));
#79979=CARTESIAN_POINT('Ctrl Pts',(141.571214020252,2.48499327898026,48.5));
#79980=CARTESIAN_POINT('',(141.521691501141,3.00497958064079,48.35));
#79981=CARTESIAN_POINT('',(141.521691501141,3.00497958064079,48.5));
#79982=CARTESIAN_POINT('Ctrl Pts',(141.521691501141,3.00497958064079,48.35));
#79983=CARTESIAN_POINT('Ctrl Pts',(141.571214020252,2.81214186549187,48.35));
#79984=CARTESIAN_POINT('Ctrl Pts',(141.571214020252,2.48499327898026,48.35));
#79985=CARTESIAN_POINT('Ctrl Pts',(141.385129511356,3.33212831616402,48.5));
#79986=CARTESIAN_POINT('Ctrl Pts',(141.385129511356,3.33212831616402,48.35));
#79987=CARTESIAN_POINT('Ctrl Pts',(141.472168982029,3.19781729578972,48.5));
#79988=CARTESIAN_POINT('Ctrl Pts',(141.472168982029,3.19781729578972,48.35));
#79989=CARTESIAN_POINT('Ctrl Pts',(141.521691501141,3.00497958064079,48.5));
#79990=CARTESIAN_POINT('Ctrl Pts',(141.521691501141,3.00497958064079,48.35));
#79991=CARTESIAN_POINT('',(141.385129511356,3.33212831616402,48.5));
#79992=CARTESIAN_POINT('Ctrl Pts',(141.385129511356,3.33212831616402,48.5));
#79993=CARTESIAN_POINT('Ctrl Pts',(141.472168982029,3.19781729578972,48.5));
#79994=CARTESIAN_POINT('Ctrl Pts',(141.521691501141,3.00497958064079,48.5));
#79995=CARTESIAN_POINT('',(141.385129511356,3.33212831616402,48.35));
#79996=CARTESIAN_POINT('',(141.385129511356,3.33212831616402,48.5));
#79997=CARTESIAN_POINT('Ctrl Pts',(141.385129511356,3.33212831616402,48.35));
#79998=CARTESIAN_POINT('Ctrl Pts',(141.472168982029,3.19781729578972,48.35));
#79999=CARTESIAN_POINT('Ctrl Pts',(141.521691501141,3.00497958064079,48.35));
#80000=CARTESIAN_POINT('Ctrl Pts',(141.164529144764,3.5377217233181,48.5));
#80001=CARTESIAN_POINT('Ctrl Pts',(141.164529144764,3.5377217233181,48.35));
#80002=CARTESIAN_POINT('Ctrl Pts',(141.298090040684,3.46643933653831,48.5));
#80003=CARTESIAN_POINT('Ctrl Pts',(141.298090040684,3.46643933653831,48.35));
#80004=CARTESIAN_POINT('Ctrl Pts',(141.385129511356,3.33212831616402,48.5));
#80005=CARTESIAN_POINT('Ctrl Pts',(141.385129511356,3.33212831616402,48.35));
#80006=CARTESIAN_POINT('',(141.164529144764,3.5377217233181,48.5));
#80007=CARTESIAN_POINT('Ctrl Pts',(141.164529144764,3.5377217233181,48.5));
#80008=CARTESIAN_POINT('Ctrl Pts',(141.298090040684,3.46643933653831,48.5));
#80009=CARTESIAN_POINT('Ctrl Pts',(141.385129511356,3.33212831616402,48.5));
#80010=CARTESIAN_POINT('',(141.164529144764,3.5377217233181,48.35));
#80011=CARTESIAN_POINT('',(141.164529144764,3.5377217233181,48.5));
#80012=CARTESIAN_POINT('Ctrl Pts',(141.164529144764,3.5377217233181,48.35));
#80013=CARTESIAN_POINT('Ctrl Pts',(141.298090040684,3.46643933653831,48.35));
#80014=CARTESIAN_POINT('Ctrl Pts',(141.385129511356,3.33212831616402,48.35));
#80015=CARTESIAN_POINT('Ctrl Pts',(140.853888213634,3.60900411009789,48.5));
#80016=CARTESIAN_POINT('Ctrl Pts',(140.853888213634,3.60900411009789,48.35));
#80017=CARTESIAN_POINT('Ctrl Pts',(141.030968248844,3.60900411009789,48.5));
#80018=CARTESIAN_POINT('Ctrl Pts',(141.030968248844,3.60900411009789,48.35));
#80019=CARTESIAN_POINT('Ctrl Pts',(141.164529144764,3.5377217233181,48.5));
#80020=CARTESIAN_POINT('Ctrl Pts',(141.164529144764,3.5377217233181,48.35));
#80021=CARTESIAN_POINT('',(140.853888213634,3.60900411009789,48.5));
#80022=CARTESIAN_POINT('Ctrl Pts',(140.853888213634,3.60900411009789,48.5));
#80023=CARTESIAN_POINT('Ctrl Pts',(141.030968248844,3.60900411009789,48.5));
#80024=CARTESIAN_POINT('Ctrl Pts',(141.164529144764,3.5377217233181,48.5));
#80025=CARTESIAN_POINT('',(140.853888213634,3.60900411009789,48.35));
#80026=CARTESIAN_POINT('',(140.853888213634,3.60900411009789,48.5));
#80027=CARTESIAN_POINT('Ctrl Pts',(140.853888213634,3.60900411009789,48.35));
#80028=CARTESIAN_POINT('Ctrl Pts',(141.030968248844,3.60900411009789,48.35));
#80029=CARTESIAN_POINT('Ctrl Pts',(141.164529144764,3.5377217233181,48.35));
#80030=CARTESIAN_POINT('Ctrl Pts',(140.455456793308,3.47994545102119,48.5));
#80031=CARTESIAN_POINT('Ctrl Pts',(140.455456793308,3.47994545102119,48.35));
#80032=CARTESIAN_POINT('Ctrl Pts',(140.613778650761,3.60900411009789,48.5));
#80033=CARTESIAN_POINT('Ctrl Pts',(140.613778650761,3.60900411009789,48.35));
#80034=CARTESIAN_POINT('Ctrl Pts',(140.853888213634,3.60900411009789,48.5));
#80035=CARTESIAN_POINT('Ctrl Pts',(140.853888213634,3.60900411009789,48.35));
#80036=CARTESIAN_POINT('',(140.455456793308,3.47994545102119,48.5));
#80037=CARTESIAN_POINT('Ctrl Pts',(140.455456793308,3.47994545102119,48.5));
#80038=CARTESIAN_POINT('Ctrl Pts',(140.613778650761,3.60900411009789,48.5));
#80039=CARTESIAN_POINT('Ctrl Pts',(140.853888213634,3.60900411009789,48.5));
#80040=CARTESIAN_POINT('',(140.455456793308,3.47994545102119,48.35));
#80041=CARTESIAN_POINT('',(140.455456793308,3.47994545102119,48.5));
#80042=CARTESIAN_POINT('Ctrl Pts',(140.455456793308,3.47994545102119,48.35));
#80043=CARTESIAN_POINT('Ctrl Pts',(140.613778650761,3.60900411009789,48.35));
#80044=CARTESIAN_POINT('Ctrl Pts',(140.853888213634,3.60900411009789,48.35));
#80045=CARTESIAN_POINT('Ctrl Pts',(140.216848671436,3.11302864551544,48.5));
#80046=CARTESIAN_POINT('Ctrl Pts',(140.216848671436,3.11302864551544,48.35));
#80047=CARTESIAN_POINT('Ctrl Pts',(140.297134935856,3.3508867919445,48.5));
#80048=CARTESIAN_POINT('Ctrl Pts',(140.297134935856,3.3508867919445,48.35));
#80049=CARTESIAN_POINT('Ctrl Pts',(140.455456793308,3.47994545102119,48.5));
#80050=CARTESIAN_POINT('Ctrl Pts',(140.455456793308,3.47994545102119,48.35));
#80051=CARTESIAN_POINT('',(140.216848671436,3.11302864551544,48.5));
#80052=CARTESIAN_POINT('Ctrl Pts',(140.216848671436,3.11302864551544,48.5));
#80053=CARTESIAN_POINT('Ctrl Pts',(140.297134935856,3.3508867919445,48.5));
#80054=CARTESIAN_POINT('Ctrl Pts',(140.455456793308,3.47994545102119,48.5));
#80055=CARTESIAN_POINT('',(140.216848671436,3.11302864551544,48.35));
#80056=CARTESIAN_POINT('',(140.216848671436,3.11302864551544,48.5));
#80057=CARTESIAN_POINT('Ctrl Pts',(140.216848671436,3.11302864551544,48.35));
#80058=CARTESIAN_POINT('Ctrl Pts',(140.297134935856,3.3508867919445,48.35));
#80059=CARTESIAN_POINT('Ctrl Pts',(140.455456793308,3.47994545102119,48.35));
#80060=CARTESIAN_POINT('Ctrl Pts',(140.13656181097,2.48499327898026,48.5));
#80061=CARTESIAN_POINT('Ctrl Pts',(140.13656181097,2.48499327898026,48.35));
#80062=CARTESIAN_POINT('Ctrl Pts',(140.13656181097,2.87517049908638,48.5));
#80063=CARTESIAN_POINT('Ctrl Pts',(140.13656181097,2.87517049908638,48.35));
#80064=CARTESIAN_POINT('Ctrl Pts',(140.216848671436,3.11302864551544,48.5));
#80065=CARTESIAN_POINT('Ctrl Pts',(140.216848671436,3.11302864551544,48.35));
#80066=CARTESIAN_POINT('',(140.13656181097,2.48499327898026,48.5));
#80067=CARTESIAN_POINT('Ctrl Pts',(140.13656181097,2.48499327898026,48.5));
#80068=CARTESIAN_POINT('Ctrl Pts',(140.13656181097,2.87517049908638,48.5));
#80069=CARTESIAN_POINT('Ctrl Pts',(140.216848671436,3.11302864551544,48.5));
#80070=CARTESIAN_POINT('',(140.13656181097,2.48499327898026,48.35));
#80071=CARTESIAN_POINT('',(140.13656181097,2.48499327898026,48.5));
#80072=CARTESIAN_POINT('Ctrl Pts',(140.13656181097,2.48499327898026,48.35));
#80073=CARTESIAN_POINT('Ctrl Pts',(140.13656181097,2.87517049908638,48.35));
#80074=CARTESIAN_POINT('Ctrl Pts',(140.216848671436,3.11302864551544,48.35));
#80075=CARTESIAN_POINT('Ctrl Pts',(140.354161083698,1.59058684110642,48.5));
#80076=CARTESIAN_POINT('Ctrl Pts',(140.354161083698,1.59058684110642,48.35));
#80077=CARTESIAN_POINT('Ctrl Pts',(140.13656181097,1.86521166563034,48.5));
#80078=CARTESIAN_POINT('Ctrl Pts',(140.13656181097,1.86521166563034,48.35));
#80079=CARTESIAN_POINT('Ctrl Pts',(140.13656181097,2.48499327898026,48.5));
#80080=CARTESIAN_POINT('Ctrl Pts',(140.13656181097,2.48499327898026,48.35));
#80081=CARTESIAN_POINT('Ctrl Pts',(140.354161083698,1.59058684110642,48.5));
#80082=CARTESIAN_POINT('Ctrl Pts',(140.13656181097,1.86521166563034,48.5));
#80083=CARTESIAN_POINT('Ctrl Pts',(140.13656181097,2.48499327898026,48.5));
#80084=CARTESIAN_POINT('Ctrl Pts',(140.354161083698,1.59058684110642,48.35));
#80085=CARTESIAN_POINT('Ctrl Pts',(140.13656181097,1.86521166563034,48.35));
#80086=CARTESIAN_POINT('Ctrl Pts',(140.13656181097,2.48499327898026,48.35));
#80087=CARTESIAN_POINT('Origin',(139.999999895692,2.48499320447445,48.35));
#80088=CARTESIAN_POINT('Ctrl Pts',(139.128103673458,1.36098229885101,48.5));
#80089=CARTESIAN_POINT('Ctrl Pts',(139.128103673458,1.36098229885101,48.35));
#80090=CARTESIAN_POINT('Ctrl Pts',(138.838472038507,1.36098229885101,48.5));
#80091=CARTESIAN_POINT('Ctrl Pts',(138.838472038507,1.36098229885101,48.35));
#80092=CARTESIAN_POINT('Ctrl Pts',(138.647135019302,1.53356069326401,48.5));
#80093=CARTESIAN_POINT('Ctrl Pts',(138.647135019302,1.53356069326401,48.35));
#80094=CARTESIAN_POINT('',(139.128103673458,1.36098229885101,48.5));
#80095=CARTESIAN_POINT('',(138.647135019302,1.53356069326401,48.5));
#80096=CARTESIAN_POINT('Ctrl Pts',(139.128103673458,1.36098229885101,48.5));
#80097=CARTESIAN_POINT('Ctrl Pts',(138.838472038507,1.36098229885101,48.5));
#80098=CARTESIAN_POINT('Ctrl Pts',(138.647135019302,1.53356069326401,48.5));
#80099=CARTESIAN_POINT('',(139.128103673458,1.36098229885101,48.35));
#80100=CARTESIAN_POINT('',(139.128103673458,1.36098229885101,48.5));
#80101=CARTESIAN_POINT('',(138.647135019302,1.53356069326401,48.35));
#80102=CARTESIAN_POINT('Ctrl Pts',(139.128103673458,1.36098229885101,48.35));
#80103=CARTESIAN_POINT('Ctrl Pts',(138.838472038507,1.36098229885101,48.35));
#80104=CARTESIAN_POINT('Ctrl Pts',(138.647135019302,1.53356069326401,48.35));
#80105=CARTESIAN_POINT('',(138.647135019302,1.53356069326401,48.5));
#80106=CARTESIAN_POINT('Ctrl Pts',(139.65934497118,1.56132334470749,48.5));
#80107=CARTESIAN_POINT('Ctrl Pts',(139.65934497118,1.56132334470749,48.35));
#80108=CARTESIAN_POINT('Ctrl Pts',(139.449249625206,1.36098229885101,48.5));
#80109=CARTESIAN_POINT('Ctrl Pts',(139.449249625206,1.36098229885101,48.35));
#80110=CARTESIAN_POINT('Ctrl Pts',(139.128103673458,1.36098229885101,48.5));
#80111=CARTESIAN_POINT('Ctrl Pts',(139.128103673458,1.36098229885101,48.35));
#80112=CARTESIAN_POINT('',(139.65934497118,1.56132334470749,48.5));
#80113=CARTESIAN_POINT('Ctrl Pts',(139.65934497118,1.56132334470749,48.5));
#80114=CARTESIAN_POINT('Ctrl Pts',(139.449249625206,1.36098229885101,48.5));
#80115=CARTESIAN_POINT('Ctrl Pts',(139.128103673458,1.36098229885101,48.5));
#80116=CARTESIAN_POINT('',(139.65934497118,1.56132334470749,48.35));
#80117=CARTESIAN_POINT('',(139.65934497118,1.56132334470749,48.5));
#80118=CARTESIAN_POINT('Ctrl Pts',(139.65934497118,1.56132334470749,48.35));
#80119=CARTESIAN_POINT('Ctrl Pts',(139.449249625206,1.36098229885101,48.35));
#80120=CARTESIAN_POINT('Ctrl Pts',(139.128103673458,1.36098229885101,48.35));
#80121=CARTESIAN_POINT('Ctrl Pts',(139.869440615177,2.04979562759399,48.5));
#80122=CARTESIAN_POINT('Ctrl Pts',(139.869440615177,2.04979562759399,48.35));
#80123=CARTESIAN_POINT('Ctrl Pts',(139.869440615177,1.76166439056397,48.5));
#80124=CARTESIAN_POINT('Ctrl Pts',(139.869440615177,1.76166439056397,48.35));
#80125=CARTESIAN_POINT('Ctrl Pts',(139.65934497118,1.56132334470749,48.5));
#80126=CARTESIAN_POINT('Ctrl Pts',(139.65934497118,1.56132334470749,48.35));
#80127=CARTESIAN_POINT('',(139.869440615177,2.04979562759399,48.5));
#80128=CARTESIAN_POINT('Ctrl Pts',(139.869440615177,2.04979562759399,48.5));
#80129=CARTESIAN_POINT('Ctrl Pts',(139.869440615177,1.76166439056397,48.5));
#80130=CARTESIAN_POINT('Ctrl Pts',(139.65934497118,1.56132334470749,48.5));
#80131=CARTESIAN_POINT('',(139.869440615177,2.04979562759399,48.35));
#80132=CARTESIAN_POINT('',(139.869440615177,2.04979562759399,48.5));
#80133=CARTESIAN_POINT('Ctrl Pts',(139.869440615177,2.04979562759399,48.35));
#80134=CARTESIAN_POINT('Ctrl Pts',(139.869440615177,1.76166439056397,48.35));
#80135=CARTESIAN_POINT('Ctrl Pts',(139.65934497118,1.56132334470749,48.35));
#80136=CARTESIAN_POINT('Ctrl Pts',(139.761391699314,2.40470671653748,48.5));
#80137=CARTESIAN_POINT('Ctrl Pts',(139.761391699314,2.40470671653748,48.35));
#80138=CARTESIAN_POINT('Ctrl Pts',(139.869440615177,2.26289236545563,48.5));
#80139=CARTESIAN_POINT('Ctrl Pts',(139.869440615177,2.26289236545563,48.35));
#80140=CARTESIAN_POINT('Ctrl Pts',(139.869440615177,2.04979562759399,48.5));
#80141=CARTESIAN_POINT('Ctrl Pts',(139.869440615177,2.04979562759399,48.35));
#80142=CARTESIAN_POINT('',(139.761391699314,2.40470671653748,48.5));
#80143=CARTESIAN_POINT('Ctrl Pts',(139.761391699314,2.40470671653748,48.5));
#80144=CARTESIAN_POINT('Ctrl Pts',(139.869440615177,2.26289236545563,48.5));
#80145=CARTESIAN_POINT('Ctrl Pts',(139.869440615177,2.04979562759399,48.5));
#80146=CARTESIAN_POINT('',(139.761391699314,2.40470671653748,48.35));
#80147=CARTESIAN_POINT('',(139.761391699314,2.40470671653748,48.5));
#80148=CARTESIAN_POINT('Ctrl Pts',(139.761391699314,2.40470671653748,48.35));
#80149=CARTESIAN_POINT('Ctrl Pts',(139.869440615177,2.26289236545563,48.35));
#80150=CARTESIAN_POINT('Ctrl Pts',(139.869440615177,2.04979562759399,48.35));
#80151=CARTESIAN_POINT('Ctrl Pts',(139.458253800869,2.59154164791107,48.5));
#80152=CARTESIAN_POINT('Ctrl Pts',(139.458253800869,2.59154164791107,48.35));
#80153=CARTESIAN_POINT('Ctrl Pts',(139.653342187405,2.54652121663094,48.5));
#80154=CARTESIAN_POINT('Ctrl Pts',(139.653342187405,2.54652121663094,48.35));
#80155=CARTESIAN_POINT('Ctrl Pts',(139.761391699314,2.40470671653748,48.5));
#80156=CARTESIAN_POINT('Ctrl Pts',(139.761391699314,2.40470671653748,48.35));
#80157=CARTESIAN_POINT('',(139.458253800869,2.59154164791107,48.5));
#80158=CARTESIAN_POINT('Ctrl Pts',(139.458253800869,2.59154164791107,48.5));
#80159=CARTESIAN_POINT('Ctrl Pts',(139.653342187405,2.54652121663094,48.5));
#80160=CARTESIAN_POINT('Ctrl Pts',(139.761391699314,2.40470671653748,48.5));
#80161=CARTESIAN_POINT('',(139.458253800869,2.59154164791107,48.35));
#80162=CARTESIAN_POINT('',(139.458253800869,2.59154164791107,48.5));
#80163=CARTESIAN_POINT('Ctrl Pts',(139.458253800869,2.59154164791107,48.35));
#80164=CARTESIAN_POINT('Ctrl Pts',(139.653342187405,2.54652121663094,48.35));
#80165=CARTESIAN_POINT('Ctrl Pts',(139.761391699314,2.40470671653748,48.35));
#80166=CARTESIAN_POINT('Ctrl Pts',(139.684856653214,2.77762615680695,48.5));
#80167=CARTESIAN_POINT('Ctrl Pts',(139.684856653214,2.77762615680695,48.35));
#80168=CARTESIAN_POINT('Ctrl Pts',(139.608321905136,2.66057306528091,48.5));
#80169=CARTESIAN_POINT('Ctrl Pts',(139.608321905136,2.66057306528091,48.35));
#80170=CARTESIAN_POINT('Ctrl Pts',(139.458253800869,2.59154164791107,48.5));
#80171=CARTESIAN_POINT('Ctrl Pts',(139.458253800869,2.59154164791107,48.35));
#80172=CARTESIAN_POINT('',(139.684856653214,2.77762615680695,48.5));
#80173=CARTESIAN_POINT('Ctrl Pts',(139.684856653214,2.77762615680695,48.5));
#80174=CARTESIAN_POINT('Ctrl Pts',(139.608321905136,2.66057306528091,48.5));
#80175=CARTESIAN_POINT('Ctrl Pts',(139.458253800869,2.59154164791107,48.5));
#80176=CARTESIAN_POINT('',(139.684856653214,2.77762615680695,48.35));
#80177=CARTESIAN_POINT('',(139.684856653214,2.77762615680695,48.5));
#80178=CARTESIAN_POINT('Ctrl Pts',(139.684856653214,2.77762615680695,48.35));
#80179=CARTESIAN_POINT('Ctrl Pts',(139.608321905136,2.66057306528091,48.35));
#80180=CARTESIAN_POINT('Ctrl Pts',(139.458253800869,2.59154164791107,48.35));
#80181=CARTESIAN_POINT('Ctrl Pts',(139.761391699314,3.03724417090416,48.5));
#80182=CARTESIAN_POINT('Ctrl Pts',(139.761391699314,3.03724417090416,48.35));
#80183=CARTESIAN_POINT('Ctrl Pts',(139.761391699314,2.89467939734459,48.5));
#80184=CARTESIAN_POINT('Ctrl Pts',(139.761391699314,2.89467939734459,48.35));
#80185=CARTESIAN_POINT('Ctrl Pts',(139.684856653214,2.77762615680695,48.5));
#80186=CARTESIAN_POINT('Ctrl Pts',(139.684856653214,2.77762615680695,48.35));
#80187=CARTESIAN_POINT('',(139.761391699314,3.03724417090416,48.5));
#80188=CARTESIAN_POINT('Ctrl Pts',(139.761391699314,3.03724417090416,48.5));
#80189=CARTESIAN_POINT('Ctrl Pts',(139.761391699314,2.89467939734459,48.5));
#80190=CARTESIAN_POINT('Ctrl Pts',(139.684856653214,2.77762615680695,48.5));
#80191=CARTESIAN_POINT('',(139.761391699314,3.03724417090416,48.35));
#80192=CARTESIAN_POINT('',(139.761391699314,3.03724417090416,48.5));
#80193=CARTESIAN_POINT('Ctrl Pts',(139.761391699314,3.03724417090416,48.35));
#80194=CARTESIAN_POINT('Ctrl Pts',(139.761391699314,2.89467939734459,48.35));
#80195=CARTESIAN_POINT('Ctrl Pts',(139.684856653214,2.77762615680695,48.35));
#80196=CARTESIAN_POINT('Ctrl Pts',(139.681104838848,3.32087317109108,48.5));
#80197=CARTESIAN_POINT('Ctrl Pts',(139.681104838848,3.32087317109108,48.35));
#80198=CARTESIAN_POINT('Ctrl Pts',(139.761391699314,3.18731242418289,48.5));
#80199=CARTESIAN_POINT('Ctrl Pts',(139.761391699314,3.18731242418289,48.35));
#80200=CARTESIAN_POINT('Ctrl Pts',(139.761391699314,3.03724417090416,48.5));
#80201=CARTESIAN_POINT('Ctrl Pts',(139.761391699314,3.03724417090416,48.35));
#80202=CARTESIAN_POINT('',(139.681104838848,3.32087317109108,48.5));
#80203=CARTESIAN_POINT('Ctrl Pts',(139.681104838848,3.32087317109108,48.5));
#80204=CARTESIAN_POINT('Ctrl Pts',(139.761391699314,3.18731242418289,48.5));
#80205=CARTESIAN_POINT('Ctrl Pts',(139.761391699314,3.03724417090416,48.5));
#80206=CARTESIAN_POINT('',(139.681104838848,3.32087317109108,48.35));
#80207=CARTESIAN_POINT('',(139.681104838848,3.32087317109108,48.5));
#80208=CARTESIAN_POINT('Ctrl Pts',(139.681104838848,3.32087317109108,48.35));
#80209=CARTESIAN_POINT('Ctrl Pts',(139.761391699314,3.18731242418289,48.35));
#80210=CARTESIAN_POINT('Ctrl Pts',(139.761391699314,3.03724417090416,48.35));
#80211=CARTESIAN_POINT('Ctrl Pts',(139.449249625206,3.53171893954277,48.5));
#80212=CARTESIAN_POINT('Ctrl Pts',(139.449249625206,3.53171893954277,48.35));
#80213=CARTESIAN_POINT('Ctrl Pts',(139.600818574429,3.45443391799927,48.5));
#80214=CARTESIAN_POINT('Ctrl Pts',(139.600818574429,3.45443391799927,48.35));
#80215=CARTESIAN_POINT('Ctrl Pts',(139.681104838848,3.32087317109108,48.5));
#80216=CARTESIAN_POINT('Ctrl Pts',(139.681104838848,3.32087317109108,48.35));
#80217=CARTESIAN_POINT('',(139.449249625206,3.53171893954277,48.5));
#80218=CARTESIAN_POINT('Ctrl Pts',(139.449249625206,3.53171893954277,48.5));
#80219=CARTESIAN_POINT('Ctrl Pts',(139.600818574429,3.45443391799927,48.5));
#80220=CARTESIAN_POINT('Ctrl Pts',(139.681104838848,3.32087317109108,48.5));
#80221=CARTESIAN_POINT('',(139.449249625206,3.53171893954277,48.35));
#80222=CARTESIAN_POINT('',(139.449249625206,3.53171893954277,48.5));
#80223=CARTESIAN_POINT('Ctrl Pts',(139.449249625206,3.53171893954277,48.35));
#80224=CARTESIAN_POINT('Ctrl Pts',(139.600818574429,3.45443391799927,48.35));
#80225=CARTESIAN_POINT('Ctrl Pts',(139.681104838848,3.32087317109108,48.35));
#80226=CARTESIAN_POINT('Ctrl Pts',(139.117598950863,3.60900411009789,48.5));
#80227=CARTESIAN_POINT('Ctrl Pts',(139.117598950863,3.60900411009789,48.35));
#80228=CARTESIAN_POINT('Ctrl Pts',(139.297680675983,3.60900411009789,48.5));
#80229=CARTESIAN_POINT('Ctrl Pts',(139.297680675983,3.60900411009789,48.35));
#80230=CARTESIAN_POINT('Ctrl Pts',(139.449249625206,3.53171893954277,48.5));
#80231=CARTESIAN_POINT('Ctrl Pts',(139.449249625206,3.53171893954277,48.35));
#80232=CARTESIAN_POINT('',(139.117598950863,3.60900411009789,48.5));
#80233=CARTESIAN_POINT('Ctrl Pts',(139.117598950863,3.60900411009789,48.5));
#80234=CARTESIAN_POINT('Ctrl Pts',(139.297680675983,3.60900411009789,48.5));
#80235=CARTESIAN_POINT('Ctrl Pts',(139.449249625206,3.53171893954277,48.5));
#80236=CARTESIAN_POINT('',(139.117598950863,3.60900411009789,48.35));
#80237=CARTESIAN_POINT('',(139.117598950863,3.60900411009789,48.5));
#80238=CARTESIAN_POINT('Ctrl Pts',(139.117598950863,3.60900411009789,48.35));
#80239=CARTESIAN_POINT('Ctrl Pts',(139.297680675983,3.60900411009789,48.35));
#80240=CARTESIAN_POINT('Ctrl Pts',(139.449249625206,3.53171893954277,48.35));
#80241=CARTESIAN_POINT('Ctrl Pts',(138.680900454521,3.45968627929688,48.5));
#80242=CARTESIAN_POINT('Ctrl Pts',(138.680900454521,3.45968627929688,48.35));
#80243=CARTESIAN_POINT('Ctrl Pts',(138.856480240822,3.60900411009789,48.5));
#80244=CARTESIAN_POINT('Ctrl Pts',(138.856480240822,3.60900411009789,48.35));
#80245=CARTESIAN_POINT('Ctrl Pts',(139.117598950863,3.60900411009789,48.5));
#80246=CARTESIAN_POINT('Ctrl Pts',(139.117598950863,3.60900411009789,48.35));
#80247=CARTESIAN_POINT('',(138.680900454521,3.45968627929688,48.5));
#80248=CARTESIAN_POINT('Ctrl Pts',(138.680900454521,3.45968627929688,48.5));
#80249=CARTESIAN_POINT('Ctrl Pts',(138.856480240822,3.60900411009789,48.5));
#80250=CARTESIAN_POINT('Ctrl Pts',(139.117598950863,3.60900411009789,48.5));
#80251=CARTESIAN_POINT('',(138.680900454521,3.45968627929688,48.35));
#80252=CARTESIAN_POINT('',(138.680900454521,3.45968627929688,48.5));
#80253=CARTESIAN_POINT('Ctrl Pts',(138.680900454521,3.45968627929688,48.35));
#80254=CARTESIAN_POINT('Ctrl Pts',(138.856480240822,3.60900411009789,48.35));
#80255=CARTESIAN_POINT('Ctrl Pts',(139.117598950863,3.60900411009789,48.35));
#80256=CARTESIAN_POINT('Ctrl Pts',(138.455798000097,3.03874486684799,48.5));
#80257=CARTESIAN_POINT('Ctrl Pts',(138.455798000097,3.03874486684799,48.35));
#80258=CARTESIAN_POINT('Ctrl Pts',(138.505320519209,3.31036829948425,48.5));
#80259=CARTESIAN_POINT('Ctrl Pts',(138.505320519209,3.31036829948425,48.35));
#80260=CARTESIAN_POINT('Ctrl Pts',(138.680900454521,3.45968627929688,48.5));
#80261=CARTESIAN_POINT('Ctrl Pts',(138.680900454521,3.45968627929688,48.35));
#80262=CARTESIAN_POINT('',(138.455798000097,3.03874486684799,48.5));
#80263=CARTESIAN_POINT('Ctrl Pts',(138.455798000097,3.03874486684799,48.5));
#80264=CARTESIAN_POINT('Ctrl Pts',(138.505320519209,3.31036829948425,48.5));
#80265=CARTESIAN_POINT('Ctrl Pts',(138.680900454521,3.45968627929688,48.5));
#80266=CARTESIAN_POINT('',(138.455798000097,3.03874486684799,48.35));
#80267=CARTESIAN_POINT('',(138.455798000097,3.03874486684799,48.5));
#80268=CARTESIAN_POINT('Ctrl Pts',(138.455798000097,3.03874486684799,48.35));
#80269=CARTESIAN_POINT('Ctrl Pts',(138.505320519209,3.31036829948425,48.35));
#80270=CARTESIAN_POINT('Ctrl Pts',(138.680900454521,3.45968627929688,48.35));
#80271=CARTESIAN_POINT('Origin',(138.72592073679,2.99072304368019,48.5));
#80272=CARTESIAN_POINT('',(138.72592073679,2.99072304368019,48.5));
#80273=CARTESIAN_POINT('',(71.0563831288241,15.0208638924185,48.5));
#80274=CARTESIAN_POINT('',(138.72592073679,2.99072304368019,48.35));
#80275=CARTESIAN_POINT('',(138.72592073679,2.99072304368019,48.5));
#80276=CARTESIAN_POINT('',(138.72592073679,2.99072304368019,48.35));
#80277=CARTESIAN_POINT('Ctrl Pts',(138.860982179642,3.28785815834999,48.5));
#80278=CARTESIAN_POINT('Ctrl Pts',(138.860982179642,3.28785815834999,48.35));
#80279=CARTESIAN_POINT('Ctrl Pts',(138.755934506655,3.18881312012672,48.5));
#80280=CARTESIAN_POINT('Ctrl Pts',(138.755934506655,3.18881312012672,48.35));
#80281=CARTESIAN_POINT('Ctrl Pts',(138.72592073679,2.99072304368019,48.5));
#80282=CARTESIAN_POINT('Ctrl Pts',(138.72592073679,2.99072304368019,48.35));
#80283=CARTESIAN_POINT('',(138.860982179642,3.28785815834999,48.5));
#80284=CARTESIAN_POINT('Ctrl Pts',(138.860982179642,3.28785815834999,48.5));
#80285=CARTESIAN_POINT('Ctrl Pts',(138.755934506655,3.18881312012672,48.5));
#80286=CARTESIAN_POINT('Ctrl Pts',(138.72592073679,2.99072304368019,48.5));
#80287=CARTESIAN_POINT('',(138.860982179642,3.28785815834999,48.35));
#80288=CARTESIAN_POINT('',(138.860982179642,3.28785815834999,48.5));
#80289=CARTESIAN_POINT('Ctrl Pts',(138.860982179642,3.28785815834999,48.35));
#80290=CARTESIAN_POINT('Ctrl Pts',(138.755934506655,3.18881312012672,48.35));
#80291=CARTESIAN_POINT('Ctrl Pts',(138.72592073679,2.99072304368019,48.35));
#80292=CARTESIAN_POINT('Ctrl Pts',(139.123601585627,3.38690319657326,48.5));
#80293=CARTESIAN_POINT('Ctrl Pts',(139.123601585627,3.38690319657326,48.35));
#80294=CARTESIAN_POINT('Ctrl Pts',(138.96603000164,3.38690319657326,48.5));
#80295=CARTESIAN_POINT('Ctrl Pts',(138.96603000164,3.38690319657326,48.35));
#80296=CARTESIAN_POINT('Ctrl Pts',(138.860982179642,3.28785815834999,48.5));
#80297=CARTESIAN_POINT('Ctrl Pts',(138.860982179642,3.28785815834999,48.35));
#80298=CARTESIAN_POINT('',(139.123601585627,3.38690319657326,48.5));
#80299=CARTESIAN_POINT('Ctrl Pts',(139.123601585627,3.38690319657326,48.5));
#80300=CARTESIAN_POINT('Ctrl Pts',(138.96603000164,3.38690319657326,48.5));
#80301=CARTESIAN_POINT('Ctrl Pts',(138.860982179642,3.28785815834999,48.5));
#80302=CARTESIAN_POINT('',(139.123601585627,3.38690319657326,48.35));
#80303=CARTESIAN_POINT('',(139.123601585627,3.38690319657326,48.5));
#80304=CARTESIAN_POINT('Ctrl Pts',(139.123601585627,3.38690319657326,48.35));
#80305=CARTESIAN_POINT('Ctrl Pts',(138.96603000164,3.38690319657326,48.35));
#80306=CARTESIAN_POINT('Ctrl Pts',(138.860982179642,3.28785815834999,48.35));
#80307=CARTESIAN_POINT('Ctrl Pts',(139.383219599724,3.28935885429382,48.5));
#80308=CARTESIAN_POINT('Ctrl Pts',(139.383219599724,3.28935885429382,48.35));
#80309=CARTESIAN_POINT('Ctrl Pts',(139.282673865557,3.38690319657326,48.5));
#80310=CARTESIAN_POINT('Ctrl Pts',(139.282673865557,3.38690319657326,48.35));
#80311=CARTESIAN_POINT('Ctrl Pts',(139.123601585627,3.38690319657326,48.5));
#80312=CARTESIAN_POINT('Ctrl Pts',(139.123601585627,3.38690319657326,48.35));
#80313=CARTESIAN_POINT('',(139.383219599724,3.28935885429382,48.5));
#80314=CARTESIAN_POINT('Ctrl Pts',(139.383219599724,3.28935885429382,48.5));
#80315=CARTESIAN_POINT('Ctrl Pts',(139.282673865557,3.38690319657326,48.5));
#80316=CARTESIAN_POINT('Ctrl Pts',(139.123601585627,3.38690319657326,48.5));
#80317=CARTESIAN_POINT('',(139.383219599724,3.28935885429382,48.35));
#80318=CARTESIAN_POINT('',(139.383219599724,3.28935885429382,48.5));
#80319=CARTESIAN_POINT('Ctrl Pts',(139.383219599724,3.28935885429382,48.35));
#80320=CARTESIAN_POINT('Ctrl Pts',(139.282673865557,3.38690319657326,48.35));
#80321=CARTESIAN_POINT('Ctrl Pts',(139.123601585627,3.38690319657326,48.35));
#80322=CARTESIAN_POINT('Ctrl Pts',(139.483765184879,3.04324695467949,48.5));
#80323=CARTESIAN_POINT('Ctrl Pts',(139.483765184879,3.04324695467949,48.35));
#80324=CARTESIAN_POINT('Ctrl Pts',(139.483765184879,3.19181451201439,48.5));
#80325=CARTESIAN_POINT('Ctrl Pts',(139.483765184879,3.19181451201439,48.35));
#80326=CARTESIAN_POINT('Ctrl Pts',(139.383219599724,3.28935885429382,48.5));
#80327=CARTESIAN_POINT('Ctrl Pts',(139.383219599724,3.28935885429382,48.35));
#80328=CARTESIAN_POINT('',(139.483765184879,3.04324695467949,48.5));
#80329=CARTESIAN_POINT('Ctrl Pts',(139.483765184879,3.04324695467949,48.5));
#80330=CARTESIAN_POINT('Ctrl Pts',(139.483765184879,3.19181451201439,48.5));
#80331=CARTESIAN_POINT('Ctrl Pts',(139.383219599724,3.28935885429382,48.5));
#80332=CARTESIAN_POINT('',(139.483765184879,3.04324695467949,48.35));
#80333=CARTESIAN_POINT('',(139.483765184879,3.04324695467949,48.5));
#80334=CARTESIAN_POINT('Ctrl Pts',(139.483765184879,3.04324695467949,48.35));
#80335=CARTESIAN_POINT('Ctrl Pts',(139.483765184879,3.19181451201439,48.35));
#80336=CARTESIAN_POINT('Ctrl Pts',(139.383219599724,3.28935885429382,48.35));
#80337=CARTESIAN_POINT('Ctrl Pts',(139.345702648163,2.7656207382679,48.5));
#80338=CARTESIAN_POINT('Ctrl Pts',(139.345702648163,2.7656207382679,48.35));
#80339=CARTESIAN_POINT('Ctrl Pts',(139.483765184879,2.85566174983978,48.5));
#80340=CARTESIAN_POINT('Ctrl Pts',(139.483765184879,2.85566174983978,48.35));
#80341=CARTESIAN_POINT('Ctrl Pts',(139.483765184879,3.04324695467949,48.5));
#80342=CARTESIAN_POINT('Ctrl Pts',(139.483765184879,3.04324695467949,48.35));
#80343=CARTESIAN_POINT('',(139.345702648163,2.7656207382679,48.5));
#80344=CARTESIAN_POINT('Ctrl Pts',(139.345702648163,2.7656207382679,48.5));
#80345=CARTESIAN_POINT('Ctrl Pts',(139.483765184879,2.85566174983978,48.5));
#80346=CARTESIAN_POINT('Ctrl Pts',(139.483765184879,3.04324695467949,48.5));
#80347=CARTESIAN_POINT('',(139.345702648163,2.7656207382679,48.35));
#80348=CARTESIAN_POINT('',(139.345702648163,2.7656207382679,48.5));
#80349=CARTESIAN_POINT('Ctrl Pts',(139.345702648163,2.7656207382679,48.35));
#80350=CARTESIAN_POINT('Ctrl Pts',(139.483765184879,2.85566174983978,48.35));
#80351=CARTESIAN_POINT('Ctrl Pts',(139.483765184879,3.04324695467949,48.35));
#80352=CARTESIAN_POINT('Ctrl Pts',(139.03506141901,2.67557987570763,48.5));
#80353=CARTESIAN_POINT('Ctrl Pts',(139.03506141901,2.67557987570763,48.35));
#80354=CARTESIAN_POINT('Ctrl Pts',(139.207639813423,2.67557987570763,48.5));
#80355=CARTESIAN_POINT('Ctrl Pts',(139.207639813423,2.67557987570763,48.35));
#80356=CARTESIAN_POINT('Ctrl Pts',(139.345702648163,2.7656207382679,48.5));
#80357=CARTESIAN_POINT('Ctrl Pts',(139.345702648163,2.7656207382679,48.35));
#80358=CARTESIAN_POINT('',(139.03506141901,2.67557987570763,48.5));
#80359=CARTESIAN_POINT('Ctrl Pts',(139.03506141901,2.67557987570763,48.5));
#80360=CARTESIAN_POINT('Ctrl Pts',(139.207639813423,2.67557987570763,48.5));
#80361=CARTESIAN_POINT('Ctrl Pts',(139.345702648163,2.7656207382679,48.5));
#80362=CARTESIAN_POINT('',(139.03506141901,2.67557987570763,48.35));
#80363=CARTESIAN_POINT('',(139.03506141901,2.67557987570763,48.5));
#80364=CARTESIAN_POINT('Ctrl Pts',(139.03506141901,2.67557987570763,48.35));
#80365=CARTESIAN_POINT('Ctrl Pts',(139.207639813423,2.67557987570763,48.35));
#80366=CARTESIAN_POINT('Ctrl Pts',(139.345702648163,2.7656207382679,48.35));
#80367=CARTESIAN_POINT('Ctrl Pts',(138.991541534662,2.67858126759529,48.5));
#80368=CARTESIAN_POINT('Ctrl Pts',(138.991541534662,2.67858126759529,48.35));
#80369=CARTESIAN_POINT('Ctrl Pts',(139.01855391264,2.67557987570763,48.5));
#80370=CARTESIAN_POINT('Ctrl Pts',(139.01855391264,2.67557987570763,48.35));
#80371=CARTESIAN_POINT('Ctrl Pts',(139.03506141901,2.67557987570763,48.5));
#80372=CARTESIAN_POINT('Ctrl Pts',(139.03506141901,2.67557987570763,48.35));
#80373=CARTESIAN_POINT('',(138.991541534662,2.67858126759529,48.5));
#80374=CARTESIAN_POINT('Ctrl Pts',(138.991541534662,2.67858126759529,48.5));
#80375=CARTESIAN_POINT('Ctrl Pts',(139.01855391264,2.67557987570763,48.5));
#80376=CARTESIAN_POINT('Ctrl Pts',(139.03506141901,2.67557987570763,48.5));
#80377=CARTESIAN_POINT('',(138.991541534662,2.67858126759529,48.35));
#80378=CARTESIAN_POINT('',(138.991541534662,2.67858126759529,48.5));
#80379=CARTESIAN_POINT('Ctrl Pts',(138.991541534662,2.67858126759529,48.35));
#80380=CARTESIAN_POINT('Ctrl Pts',(139.01855391264,2.67557987570763,48.35));
#80381=CARTESIAN_POINT('Ctrl Pts',(139.03506141901,2.67557987570763,48.35));
#80382=CARTESIAN_POINT('Origin',(138.961527913809,2.44147354364395,48.5));
#80383=CARTESIAN_POINT('',(138.961527913809,2.44147354364395,48.5));
#80384=CARTESIAN_POINT('',(138.212047920404,-3.47942138107244,48.5));
#80385=CARTESIAN_POINT('',(138.961527913809,2.44147354364395,48.35));
#80386=CARTESIAN_POINT('',(138.961527913809,2.44147354364395,48.5));
#80387=CARTESIAN_POINT('',(138.961527913809,2.44147354364395,48.35));
#80388=CARTESIAN_POINT('Ctrl Pts',(139.152114510536,2.47148716449738,48.5));
#80389=CARTESIAN_POINT('Ctrl Pts',(139.152114510536,2.47148716449738,48.35));
#80390=CARTESIAN_POINT('Ctrl Pts',(139.075579762459,2.47148716449738,48.5));
#80391=CARTESIAN_POINT('Ctrl Pts',(139.075579762459,2.47148716449738,48.35));
#80392=CARTESIAN_POINT('Ctrl Pts',(138.961527913809,2.44147354364395,48.5));
#80393=CARTESIAN_POINT('Ctrl Pts',(138.961527913809,2.44147354364395,48.35));
#80394=CARTESIAN_POINT('',(139.152114510536,2.47148716449738,48.5));
#80395=CARTESIAN_POINT('Ctrl Pts',(139.152114510536,2.47148716449738,48.5));
#80396=CARTESIAN_POINT('Ctrl Pts',(139.075579762459,2.47148716449738,48.5));
#80397=CARTESIAN_POINT('Ctrl Pts',(138.961527913809,2.44147354364395,48.5));
#80398=CARTESIAN_POINT('',(139.152114510536,2.47148716449738,48.35));
#80399=CARTESIAN_POINT('',(139.152114510536,2.47148716449738,48.5));
#80400=CARTESIAN_POINT('Ctrl Pts',(139.152114510536,2.47148716449738,48.35));
#80401=CARTESIAN_POINT('Ctrl Pts',(139.075579762459,2.47148716449738,48.35));
#80402=CARTESIAN_POINT('Ctrl Pts',(138.961527913809,2.44147354364395,48.35));
#80403=CARTESIAN_POINT('Ctrl Pts',(139.461254894733,2.35068225860596,48.5));
#80404=CARTESIAN_POINT('Ctrl Pts',(139.461254894733,2.35068225860596,48.35));
#80405=CARTESIAN_POINT('Ctrl Pts',(139.339699864388,2.47148716449738,48.5));
#80406=CARTESIAN_POINT('Ctrl Pts',(139.339699864388,2.47148716449738,48.35));
#80407=CARTESIAN_POINT('Ctrl Pts',(139.152114510536,2.47148716449738,48.5));
#80408=CARTESIAN_POINT('Ctrl Pts',(139.152114510536,2.47148716449738,48.35));
#80409=CARTESIAN_POINT('',(139.461254894733,2.35068225860596,48.5));
#80410=CARTESIAN_POINT('Ctrl Pts',(139.461254894733,2.35068225860596,48.5));
#80411=CARTESIAN_POINT('Ctrl Pts',(139.339699864388,2.47148716449738,48.5));
#80412=CARTESIAN_POINT('Ctrl Pts',(139.152114510536,2.47148716449738,48.5));
#80413=CARTESIAN_POINT('',(139.461254894733,2.35068225860596,48.35));
#80414=CARTESIAN_POINT('',(139.461254894733,2.35068225860596,48.5));
#80415=CARTESIAN_POINT('Ctrl Pts',(139.461254894733,2.35068225860596,48.35));
#80416=CARTESIAN_POINT('Ctrl Pts',(139.339699864388,2.47148716449738,48.35));
#80417=CARTESIAN_POINT('Ctrl Pts',(139.152114510536,2.47148716449738,48.35));
#80418=CARTESIAN_POINT('Ctrl Pts',(139.582810223103,2.04379284381866,48.5));
#80419=CARTESIAN_POINT('Ctrl Pts',(139.582810223103,2.04379284381866,48.35));
#80420=CARTESIAN_POINT('Ctrl Pts',(139.582810223103,2.22987735271454,48.5));
#80421=CARTESIAN_POINT('Ctrl Pts',(139.582810223103,2.22987735271454,48.35));
#80422=CARTESIAN_POINT('Ctrl Pts',(139.461254894733,2.35068225860596,48.5));
#80423=CARTESIAN_POINT('Ctrl Pts',(139.461254894733,2.35068225860596,48.35));
#80424=CARTESIAN_POINT('',(139.582810223103,2.04379284381866,48.5));
#80425=CARTESIAN_POINT('Ctrl Pts',(139.582810223103,2.04379284381866,48.5));
#80426=CARTESIAN_POINT('Ctrl Pts',(139.582810223103,2.22987735271454,48.5));
#80427=CARTESIAN_POINT('Ctrl Pts',(139.461254894733,2.35068225860596,48.5));
#80428=CARTESIAN_POINT('',(139.582810223103,2.04379284381866,48.35));
#80429=CARTESIAN_POINT('',(139.582810223103,2.04379284381866,48.5));
#80430=CARTESIAN_POINT('Ctrl Pts',(139.582810223103,2.04379284381866,48.35));
#80431=CARTESIAN_POINT('Ctrl Pts',(139.582810223103,2.22987735271454,48.35));
#80432=CARTESIAN_POINT('Ctrl Pts',(139.461254894733,2.35068225860596,48.35));
#80433=CARTESIAN_POINT('Ctrl Pts',(139.451500594616,1.71664410829544,48.5));
#80434=CARTESIAN_POINT('Ctrl Pts',(139.451500594616,1.71664410829544,48.35));
#80435=CARTESIAN_POINT('Ctrl Pts',(139.582810223103,1.8487041592598,48.5));
#80436=CARTESIAN_POINT('Ctrl Pts',(139.582810223103,1.8487041592598,48.35));
#80437=CARTESIAN_POINT('Ctrl Pts',(139.582810223103,2.04379284381866,48.5));
#80438=CARTESIAN_POINT('Ctrl Pts',(139.582810223103,2.04379284381866,48.35));
#80439=CARTESIAN_POINT('',(139.451500594616,1.71664410829544,48.5));
#80440=CARTESIAN_POINT('Ctrl Pts',(139.451500594616,1.71664410829544,48.5));
#80441=CARTESIAN_POINT('Ctrl Pts',(139.582810223103,1.8487041592598,48.5));
#80442=CARTESIAN_POINT('Ctrl Pts',(139.582810223103,2.04379284381866,48.5));
#80443=CARTESIAN_POINT('',(139.451500594616,1.71664410829544,48.35));
#80444=CARTESIAN_POINT('',(139.451500594616,1.71664410829544,48.5));
#80445=CARTESIAN_POINT('Ctrl Pts',(139.451500594616,1.71664410829544,48.35));
#80446=CARTESIAN_POINT('Ctrl Pts',(139.582810223103,1.8487041592598,48.35));
#80447=CARTESIAN_POINT('Ctrl Pts',(139.582810223103,2.04379284381866,48.35));
#80448=CARTESIAN_POINT('Ctrl Pts',(139.12960422039,1.58458405733109,48.5));
#80449=CARTESIAN_POINT('Ctrl Pts',(139.12960422039,1.58458405733109,48.35));
#80450=CARTESIAN_POINT('Ctrl Pts',(139.320190966129,1.58458405733109,48.5));
#80451=CARTESIAN_POINT('Ctrl Pts',(139.320190966129,1.58458405733109,48.35));
#80452=CARTESIAN_POINT('Ctrl Pts',(139.451500594616,1.71664410829544,48.5));
#80453=CARTESIAN_POINT('Ctrl Pts',(139.451500594616,1.71664410829544,48.35));
#80454=CARTESIAN_POINT('',(139.12960422039,1.58458405733109,48.5));
#80455=CARTESIAN_POINT('Ctrl Pts',(139.12960422039,1.58458405733109,48.5));
#80456=CARTESIAN_POINT('Ctrl Pts',(139.320190966129,1.58458405733109,48.5));
#80457=CARTESIAN_POINT('Ctrl Pts',(139.451500594616,1.71664410829544,48.5));
#80458=CARTESIAN_POINT('',(139.12960422039,1.58458405733109,48.35));
#80459=CARTESIAN_POINT('',(139.12960422039,1.58458405733109,48.5));
#80460=CARTESIAN_POINT('Ctrl Pts',(139.12960422039,1.58458405733109,48.35));
#80461=CARTESIAN_POINT('Ctrl Pts',(139.320190966129,1.58458405733109,48.35));
#80462=CARTESIAN_POINT('Ctrl Pts',(139.451500594616,1.71664410829544,48.35));
#80463=CARTESIAN_POINT('Ctrl Pts',(138.857230514288,1.68588006496429,48.5));
#80464=CARTESIAN_POINT('Ctrl Pts',(138.857230514288,1.68588006496429,48.35));
#80465=CARTESIAN_POINT('Ctrl Pts',(138.969031393528,1.58458405733109,48.5));
#80466=CARTESIAN_POINT('Ctrl Pts',(138.969031393528,1.58458405733109,48.35));
#80467=CARTESIAN_POINT('Ctrl Pts',(139.12960422039,1.58458405733109,48.5));
#80468=CARTESIAN_POINT('Ctrl Pts',(139.12960422039,1.58458405733109,48.35));
#80469=CARTESIAN_POINT('',(138.857230514288,1.68588006496429,48.5));
#80470=CARTESIAN_POINT('Ctrl Pts',(138.857230514288,1.68588006496429,48.5));
#80471=CARTESIAN_POINT('Ctrl Pts',(138.969031393528,1.58458405733109,48.5));
#80472=CARTESIAN_POINT('Ctrl Pts',(139.12960422039,1.58458405733109,48.5));
#80473=CARTESIAN_POINT('',(138.857230514288,1.68588006496429,48.35));
#80474=CARTESIAN_POINT('',(138.857230514288,1.68588006496429,48.5));
#80475=CARTESIAN_POINT('Ctrl Pts',(138.857230514288,1.68588006496429,48.35));
#80476=CARTESIAN_POINT('Ctrl Pts',(138.969031393528,1.58458405733109,48.35));
#80477=CARTESIAN_POINT('Ctrl Pts',(139.12960422039,1.58458405733109,48.35));
#80478=CARTESIAN_POINT('Ctrl Pts',(138.698908507824,2.01678061485291,48.5));
#80479=CARTESIAN_POINT('Ctrl Pts',(138.698908507824,2.01678061485291,48.35));
#80480=CARTESIAN_POINT('Ctrl Pts',(138.745429635048,1.7871760725975,48.5));
#80481=CARTESIAN_POINT('Ctrl Pts',(138.745429635048,1.7871760725975,48.35));
#80482=CARTESIAN_POINT('Ctrl Pts',(138.857230514288,1.68588006496429,48.5));
#80483=CARTESIAN_POINT('Ctrl Pts',(138.857230514288,1.68588006496429,48.35));
#80484=CARTESIAN_POINT('',(138.698908507824,2.01678061485291,48.5));
#80485=CARTESIAN_POINT('Ctrl Pts',(138.698908507824,2.01678061485291,48.5));
#80486=CARTESIAN_POINT('Ctrl Pts',(138.745429635048,1.7871760725975,48.5));
#80487=CARTESIAN_POINT('Ctrl Pts',(138.857230514288,1.68588006496429,48.5));
#80488=CARTESIAN_POINT('',(138.698908507824,2.01678061485291,48.35));
#80489=CARTESIAN_POINT('',(138.698908507824,2.01678061485291,48.5));
#80490=CARTESIAN_POINT('Ctrl Pts',(138.698908507824,2.01678061485291,48.35));
#80491=CARTESIAN_POINT('Ctrl Pts',(138.745429635048,1.7871760725975,48.35));
#80492=CARTESIAN_POINT('Ctrl Pts',(138.857230514288,1.68588006496429,48.35));
#80493=CARTESIAN_POINT('Origin',(138.428785771132,1.98076421022415,48.5));
#80494=CARTESIAN_POINT('',(138.428785771132,1.98076421022415,48.5));
#80495=CARTESIAN_POINT('',(70.817654041723,-7.03406329963869,48.5));
#80496=CARTESIAN_POINT('',(138.428785771132,1.98076421022415,48.35));
#80497=CARTESIAN_POINT('',(138.428785771132,1.98076421022415,48.5));
#80498=CARTESIAN_POINT('',(138.428785771132,1.98076421022415,48.35));
#80499=CARTESIAN_POINT('Ctrl Pts',(138.647135019302,1.53356069326401,48.5));
#80500=CARTESIAN_POINT('Ctrl Pts',(138.647135019302,1.53356069326401,48.35));
#80501=CARTESIAN_POINT('Ctrl Pts',(138.455798000097,1.70613938570023,48.5));
#80502=CARTESIAN_POINT('Ctrl Pts',(138.455798000097,1.70613938570023,48.35));
#80503=CARTESIAN_POINT('Ctrl Pts',(138.428785771132,1.98076421022415,48.5));
#80504=CARTESIAN_POINT('Ctrl Pts',(138.428785771132,1.98076421022415,48.35));
#80505=CARTESIAN_POINT('Ctrl Pts',(138.647135019302,1.53356069326401,48.5));
#80506=CARTESIAN_POINT('Ctrl Pts',(138.455798000097,1.70613938570023,48.5));
#80507=CARTESIAN_POINT('Ctrl Pts',(138.428785771132,1.98076421022415,48.5));
#80508=CARTESIAN_POINT('Ctrl Pts',(138.647135019302,1.53356069326401,48.35));
#80509=CARTESIAN_POINT('Ctrl Pts',(138.455798000097,1.70613938570023,48.35));
#80510=CARTESIAN_POINT('Ctrl Pts',(138.428785771132,1.98076421022415,48.35));
#80511=CARTESIAN_POINT('Origin',(139.999999895692,2.48499320447445,48.35));
#80512=CARTESIAN_POINT('Origin',(0.,8.,48.5));
#80513=CARTESIAN_POINT('Ctrl Pts',(130.870395654812,3.38540250062943,48.5));
#80514=CARTESIAN_POINT('Ctrl Pts',(130.870395654812,3.38540250062943,48.35));
#80515=CARTESIAN_POINT('Ctrl Pts',(130.684310847893,3.38540250062943,48.5));
#80516=CARTESIAN_POINT('Ctrl Pts',(130.684310847893,3.38540250062943,48.35));
#80517=CARTESIAN_POINT('Ctrl Pts',(130.573260540143,3.22783091664314,48.5));
#80518=CARTESIAN_POINT('Ctrl Pts',(130.573260540143,3.22783091664314,48.35));
#80519=CARTESIAN_POINT('',(130.870395654812,3.38540250062943,48.5));
#80520=CARTESIAN_POINT('',(130.573260540143,3.22783091664314,48.5));
#80521=CARTESIAN_POINT('Ctrl Pts',(130.870395654812,3.38540250062943,48.5));
#80522=CARTESIAN_POINT('Ctrl Pts',(130.684310847893,3.38540250062943,48.5));
#80523=CARTESIAN_POINT('Ctrl Pts',(130.573260540143,3.22783091664314,48.5));
#80524=CARTESIAN_POINT('',(130.870395654812,3.38540250062943,48.35));
#80525=CARTESIAN_POINT('',(130.870395654812,3.38540250062943,48.5));
#80526=CARTESIAN_POINT('',(130.573260540143,3.22783091664314,48.35));
#80527=CARTESIAN_POINT('Ctrl Pts',(130.870395654812,3.38540250062943,48.35));
#80528=CARTESIAN_POINT('Ctrl Pts',(130.684310847893,3.38540250062943,48.35));
#80529=CARTESIAN_POINT('Ctrl Pts',(130.573260540143,3.22783091664314,48.35));
#80530=CARTESIAN_POINT('',(130.573260540143,3.22783091664314,48.5));
#80531=CARTESIAN_POINT('Ctrl Pts',(131.18628894724,3.2068213224411,48.5));
#80532=CARTESIAN_POINT('Ctrl Pts',(131.18628894724,3.2068213224411,48.35));
#80533=CARTESIAN_POINT('Ctrl Pts',(131.059481257573,3.38540250062943,48.5));
#80534=CARTESIAN_POINT('Ctrl Pts',(131.059481257573,3.38540250062943,48.35));
#80535=CARTESIAN_POINT('Ctrl Pts',(130.870395654812,3.38540250062943,48.5));
#80536=CARTESIAN_POINT('Ctrl Pts',(130.870395654812,3.38540250062943,48.35));
#80537=CARTESIAN_POINT('',(131.18628894724,3.2068213224411,48.5));
#80538=CARTESIAN_POINT('Ctrl Pts',(131.18628894724,3.2068213224411,48.5));
#80539=CARTESIAN_POINT('Ctrl Pts',(131.059481257573,3.38540250062943,48.5));
#80540=CARTESIAN_POINT('Ctrl Pts',(130.870395654812,3.38540250062943,48.5));
#80541=CARTESIAN_POINT('',(131.18628894724,3.2068213224411,48.35));
#80542=CARTESIAN_POINT('',(131.18628894724,3.2068213224411,48.5));
#80543=CARTESIAN_POINT('Ctrl Pts',(131.18628894724,3.2068213224411,48.35));
#80544=CARTESIAN_POINT('Ctrl Pts',(131.059481257573,3.38540250062943,48.35));
#80545=CARTESIAN_POINT('Ctrl Pts',(130.870395654812,3.38540250062943,48.35));
#80546=CARTESIAN_POINT('Ctrl Pts',(131.313096636906,2.48499327898026,48.5));
#80547=CARTESIAN_POINT('Ctrl Pts',(131.313096636906,2.48499327898026,48.35));
#80548=CARTESIAN_POINT('Ctrl Pts',(131.313096636906,3.02824014425278,48.5));
#80549=CARTESIAN_POINT('Ctrl Pts',(131.313096636906,3.02824014425278,48.35));
#80550=CARTESIAN_POINT('Ctrl Pts',(131.18628894724,3.2068213224411,48.5));
#80551=CARTESIAN_POINT('Ctrl Pts',(131.18628894724,3.2068213224411,48.35));
#80552=CARTESIAN_POINT('',(131.313096636906,2.48499327898026,48.5));
#80553=CARTESIAN_POINT('Ctrl Pts',(131.313096636906,2.48499327898026,48.5));
#80554=CARTESIAN_POINT('Ctrl Pts',(131.313096636906,3.02824014425278,48.5));
#80555=CARTESIAN_POINT('Ctrl Pts',(131.18628894724,3.2068213224411,48.5));
#80556=CARTESIAN_POINT('',(131.313096636906,2.48499327898026,48.35));
#80557=CARTESIAN_POINT('',(131.313096636906,2.48499327898026,48.5));
#80558=CARTESIAN_POINT('Ctrl Pts',(131.313096636906,2.48499327898026,48.35));
#80559=CARTESIAN_POINT('Ctrl Pts',(131.313096636906,3.02824014425278,48.35));
#80560=CARTESIAN_POINT('Ctrl Pts',(131.18628894724,3.2068213224411,48.35));
#80561=CARTESIAN_POINT('Ctrl Pts',(131.18628894724,1.76466578245163,48.5));
#80562=CARTESIAN_POINT('Ctrl Pts',(131.18628894724,1.76466578245163,48.35));
#80563=CARTESIAN_POINT('Ctrl Pts',(131.313096636906,1.9447478055954,48.5));
#80564=CARTESIAN_POINT('Ctrl Pts',(131.313096636906,1.9447478055954,48.35));
#80565=CARTESIAN_POINT('Ctrl Pts',(131.313096636906,2.48499327898026,48.5));
#80566=CARTESIAN_POINT('Ctrl Pts',(131.313096636906,2.48499327898026,48.35));
#80567=CARTESIAN_POINT('',(131.18628894724,1.76466578245163,48.5));
#80568=CARTESIAN_POINT('Ctrl Pts',(131.18628894724,1.76466578245163,48.5));
#80569=CARTESIAN_POINT('Ctrl Pts',(131.313096636906,1.9447478055954,48.5));
#80570=CARTESIAN_POINT('Ctrl Pts',(131.313096636906,2.48499327898026,48.5));
#80571=CARTESIAN_POINT('',(131.18628894724,1.76466578245163,48.35));
#80572=CARTESIAN_POINT('',(131.18628894724,1.76466578245163,48.5));
#80573=CARTESIAN_POINT('Ctrl Pts',(131.18628894724,1.76466578245163,48.35));
#80574=CARTESIAN_POINT('Ctrl Pts',(131.313096636906,1.9447478055954,48.35));
#80575=CARTESIAN_POINT('Ctrl Pts',(131.313096636906,2.48499327898026,48.35));
#80576=CARTESIAN_POINT('Ctrl Pts',(130.873396748677,1.58458405733109,48.5));
#80577=CARTESIAN_POINT('Ctrl Pts',(130.873396748677,1.58458405733109,48.35));
#80578=CARTESIAN_POINT('Ctrl Pts',(131.059481257573,1.58458405733109,48.5));
#80579=CARTESIAN_POINT('Ctrl Pts',(131.059481257573,1.58458405733109,48.35));
#80580=CARTESIAN_POINT('Ctrl Pts',(131.18628894724,1.76466578245163,48.5));
#80581=CARTESIAN_POINT('Ctrl Pts',(131.18628894724,1.76466578245163,48.35));
#80582=CARTESIAN_POINT('',(130.873396748677,1.58458405733109,48.5));
#80583=CARTESIAN_POINT('Ctrl Pts',(130.873396748677,1.58458405733109,48.5));
#80584=CARTESIAN_POINT('Ctrl Pts',(131.059481257573,1.58458405733109,48.5));
#80585=CARTESIAN_POINT('Ctrl Pts',(131.18628894724,1.76466578245163,48.5));
#80586=CARTESIAN_POINT('',(130.873396748677,1.58458405733109,48.35));
#80587=CARTESIAN_POINT('',(130.873396748677,1.58458405733109,48.5));
#80588=CARTESIAN_POINT('Ctrl Pts',(130.873396748677,1.58458405733109,48.35));
#80589=CARTESIAN_POINT('Ctrl Pts',(131.059481257573,1.58458405733109,48.35));
#80590=CARTESIAN_POINT('Ctrl Pts',(131.18628894724,1.76466578245163,48.35));
#80591=CARTESIAN_POINT('Ctrl Pts',(130.560504550114,1.76391565799713,48.5));
#80592=CARTESIAN_POINT('Ctrl Pts',(130.560504550114,1.76391565799713,48.35));
#80593=CARTESIAN_POINT('Ctrl Pts',(130.687312239781,1.58458405733109,48.5));
#80594=CARTESIAN_POINT('Ctrl Pts',(130.687312239781,1.58458405733109,48.35));
#80595=CARTESIAN_POINT('Ctrl Pts',(130.873396748677,1.58458405733109,48.5));
#80596=CARTESIAN_POINT('Ctrl Pts',(130.873396748677,1.58458405733109,48.35));
#80597=CARTESIAN_POINT('',(130.560504550114,1.76391565799713,48.5));
#80598=CARTESIAN_POINT('Ctrl Pts',(130.560504550114,1.76391565799713,48.5));
#80599=CARTESIAN_POINT('Ctrl Pts',(130.687312239781,1.58458405733109,48.5));
#80600=CARTESIAN_POINT('Ctrl Pts',(130.873396748677,1.58458405733109,48.5));
#80601=CARTESIAN_POINT('',(130.560504550114,1.76391565799713,48.35));
#80602=CARTESIAN_POINT('',(130.560504550114,1.76391565799713,48.5));
#80603=CARTESIAN_POINT('Ctrl Pts',(130.560504550114,1.76391565799713,48.35));
#80604=CARTESIAN_POINT('Ctrl Pts',(130.687312239781,1.58458405733109,48.35));
#80605=CARTESIAN_POINT('Ctrl Pts',(130.873396748677,1.58458405733109,48.35));
#80606=CARTESIAN_POINT('Ctrl Pts',(130.433696860448,2.48499327898026,48.5));
#80607=CARTESIAN_POINT('Ctrl Pts',(130.433696860448,2.48499327898026,48.35));
#80608=CARTESIAN_POINT('Ctrl Pts',(130.433696860448,1.94324696063995,48.5));
#80609=CARTESIAN_POINT('Ctrl Pts',(130.433696860448,1.94324696063995,48.35));
#80610=CARTESIAN_POINT('Ctrl Pts',(130.560504550114,1.76391565799713,48.5));
#80611=CARTESIAN_POINT('Ctrl Pts',(130.560504550114,1.76391565799713,48.35));
#80612=CARTESIAN_POINT('',(130.433696860448,2.48499327898026,48.5));
#80613=CARTESIAN_POINT('Ctrl Pts',(130.433696860448,2.48499327898026,48.5));
#80614=CARTESIAN_POINT('Ctrl Pts',(130.433696860448,1.94324696063995,48.5));
#80615=CARTESIAN_POINT('Ctrl Pts',(130.560504550114,1.76391565799713,48.5));
#80616=CARTESIAN_POINT('',(130.433696860448,2.48499327898026,48.35));
#80617=CARTESIAN_POINT('',(130.433696860448,2.48499327898026,48.5));
#80618=CARTESIAN_POINT('Ctrl Pts',(130.433696860448,2.48499327898026,48.35));
#80619=CARTESIAN_POINT('Ctrl Pts',(130.433696860448,1.94324696063995,48.35));
#80620=CARTESIAN_POINT('Ctrl Pts',(130.560504550114,1.76391565799713,48.35));
#80621=CARTESIAN_POINT('Ctrl Pts',(130.573260540143,3.22783091664314,48.5));
#80622=CARTESIAN_POINT('Ctrl Pts',(130.573260540143,3.22783091664314,48.35));
#80623=CARTESIAN_POINT('Ctrl Pts',(130.433696860448,3.02673944830894,48.5));
#80624=CARTESIAN_POINT('Ctrl Pts',(130.433696860448,3.02673944830894,48.35));
#80625=CARTESIAN_POINT('Ctrl Pts',(130.433696860448,2.48499327898026,48.5));
#80626=CARTESIAN_POINT('Ctrl Pts',(130.433696860448,2.48499327898026,48.35));
#80627=CARTESIAN_POINT('Ctrl Pts',(130.573260540143,3.22783091664314,48.5));
#80628=CARTESIAN_POINT('Ctrl Pts',(130.433696860448,3.02673944830894,48.5));
#80629=CARTESIAN_POINT('Ctrl Pts',(130.433696860448,2.48499327898026,48.5));
#80630=CARTESIAN_POINT('Ctrl Pts',(130.573260540143,3.22783091664314,48.35));
#80631=CARTESIAN_POINT('Ctrl Pts',(130.433696860448,3.02673944830894,48.35));
#80632=CARTESIAN_POINT('Ctrl Pts',(130.433696860448,2.48499327898026,48.35));
#80633=CARTESIAN_POINT('Ctrl Pts',(130.873396748677,1.36248314380646,48.5));
#80634=CARTESIAN_POINT('Ctrl Pts',(130.873396748677,1.36248314380646,48.35));
#80635=CARTESIAN_POINT('Ctrl Pts',(130.555252188817,1.36248314380646,48.5));
#80636=CARTESIAN_POINT('Ctrl Pts',(130.555252188817,1.36248314380646,48.35));
#80637=CARTESIAN_POINT('Ctrl Pts',(130.373669618741,1.59058684110642,48.5));
#80638=CARTESIAN_POINT('Ctrl Pts',(130.373669618741,1.59058684110642,48.35));
#80639=CARTESIAN_POINT('',(130.873396748677,1.36248314380646,48.5));
#80640=CARTESIAN_POINT('',(130.373669618741,1.59058684110642,48.5));
#80641=CARTESIAN_POINT('Ctrl Pts',(130.873396748677,1.36248314380646,48.5));
#80642=CARTESIAN_POINT('Ctrl Pts',(130.555252188817,1.36248314380646,48.5));
#80643=CARTESIAN_POINT('Ctrl Pts',(130.373669618741,1.59058684110642,48.5));
#80644=CARTESIAN_POINT('',(130.873396748677,1.36248314380646,48.35));
#80645=CARTESIAN_POINT('',(130.873396748677,1.36248314380646,48.5));
#80646=CARTESIAN_POINT('',(130.373669618741,1.59058684110642,48.35));
#80647=CARTESIAN_POINT('Ctrl Pts',(130.873396748677,1.36248314380646,48.35));
#80648=CARTESIAN_POINT('Ctrl Pts',(130.555252188817,1.36248314380646,48.35));
#80649=CARTESIAN_POINT('Ctrl Pts',(130.373669618741,1.59058684110642,48.35));
#80650=CARTESIAN_POINT('',(130.373669618741,1.59058684110642,48.5));
#80651=CARTESIAN_POINT('Ctrl Pts',(131.273328417912,1.49229192733765,48.5));
#80652=CARTESIAN_POINT('Ctrl Pts',(131.273328417912,1.49229192733765,48.35));
#80653=CARTESIAN_POINT('Ctrl Pts',(131.11500656046,1.36248314380646,48.5));
#80654=CARTESIAN_POINT('Ctrl Pts',(131.11500656046,1.36248314380646,48.35));
#80655=CARTESIAN_POINT('Ctrl Pts',(130.873396748677,1.36248314380646,48.5));
#80656=CARTESIAN_POINT('Ctrl Pts',(130.873396748677,1.36248314380646,48.35));
#80657=CARTESIAN_POINT('',(131.273328417912,1.49229192733765,48.5));
#80658=CARTESIAN_POINT('Ctrl Pts',(131.273328417912,1.49229192733765,48.5));
#80659=CARTESIAN_POINT('Ctrl Pts',(131.11500656046,1.36248314380646,48.5));
#80660=CARTESIAN_POINT('Ctrl Pts',(130.873396748677,1.36248314380646,48.5));
#80661=CARTESIAN_POINT('',(131.273328417912,1.49229192733765,48.35));
#80662=CARTESIAN_POINT('',(131.273328417912,1.49229192733765,48.5));
#80663=CARTESIAN_POINT('Ctrl Pts',(131.273328417912,1.49229192733765,48.35));
#80664=CARTESIAN_POINT('Ctrl Pts',(131.11500656046,1.36248314380646,48.35));
#80665=CARTESIAN_POINT('Ctrl Pts',(130.873396748677,1.36248314380646,48.35));
#80666=CARTESIAN_POINT('Ctrl Pts',(131.511186713353,1.85995900630951,48.5));
#80667=CARTESIAN_POINT('Ctrl Pts',(131.511186713353,1.85995900630951,48.35));
#80668=CARTESIAN_POINT('Ctrl Pts',(131.431650275365,1.62210100889206,48.5));
#80669=CARTESIAN_POINT('Ctrl Pts',(131.431650275365,1.62210100889206,48.35));
#80670=CARTESIAN_POINT('Ctrl Pts',(131.273328417912,1.49229192733765,48.5));
#80671=CARTESIAN_POINT('Ctrl Pts',(131.273328417912,1.49229192733765,48.35));
#80672=CARTESIAN_POINT('',(131.511186713353,1.85995900630951,48.5));
#80673=CARTESIAN_POINT('Ctrl Pts',(131.511186713353,1.85995900630951,48.5));
#80674=CARTESIAN_POINT('Ctrl Pts',(131.431650275365,1.62210100889206,48.5));
#80675=CARTESIAN_POINT('Ctrl Pts',(131.273328417912,1.49229192733765,48.5));
#80676=CARTESIAN_POINT('',(131.511186713353,1.85995900630951,48.35));
#80677=CARTESIAN_POINT('',(131.511186713353,1.85995900630951,48.5));
#80678=CARTESIAN_POINT('Ctrl Pts',(131.511186713353,1.85995900630951,48.35));
#80679=CARTESIAN_POINT('Ctrl Pts',(131.431650275365,1.62210100889206,48.35));
#80680=CARTESIAN_POINT('Ctrl Pts',(131.273328417912,1.49229192733765,48.35));
#80681=CARTESIAN_POINT('Ctrl Pts',(131.590722555295,2.48499327898026,48.5));
#80682=CARTESIAN_POINT('Ctrl Pts',(131.590722555295,2.48499327898026,48.35));
#80683=CARTESIAN_POINT('Ctrl Pts',(131.590722555295,2.09781730175018,48.5));
#80684=CARTESIAN_POINT('Ctrl Pts',(131.590722555295,2.09781730175018,48.35));
#80685=CARTESIAN_POINT('Ctrl Pts',(131.511186713353,1.85995900630951,48.5));
#80686=CARTESIAN_POINT('Ctrl Pts',(131.511186713353,1.85995900630951,48.35));
#80687=CARTESIAN_POINT('',(131.590722555295,2.48499327898026,48.5));
#80688=CARTESIAN_POINT('Ctrl Pts',(131.590722555295,2.48499327898026,48.5));
#80689=CARTESIAN_POINT('Ctrl Pts',(131.590722555295,2.09781730175018,48.5));
#80690=CARTESIAN_POINT('Ctrl Pts',(131.511186713353,1.85995900630951,48.5));
#80691=CARTESIAN_POINT('',(131.590722555295,2.48499327898026,48.35));
#80692=CARTESIAN_POINT('',(131.590722555295,2.48499327898026,48.5));
#80693=CARTESIAN_POINT('Ctrl Pts',(131.590722555295,2.48499327898026,48.35));
#80694=CARTESIAN_POINT('Ctrl Pts',(131.590722555295,2.09781730175018,48.35));
#80695=CARTESIAN_POINT('Ctrl Pts',(131.511186713353,1.85995900630951,48.35));
#80696=CARTESIAN_POINT('Ctrl Pts',(131.541200036183,3.00497958064079,48.5));
#80697=CARTESIAN_POINT('Ctrl Pts',(131.541200036183,3.00497958064079,48.35));
#80698=CARTESIAN_POINT('Ctrl Pts',(131.590722555295,2.81214186549187,48.5));
#80699=CARTESIAN_POINT('Ctrl Pts',(131.590722555295,2.81214186549187,48.35));
#80700=CARTESIAN_POINT('Ctrl Pts',(131.590722555295,2.48499327898026,48.5));
#80701=CARTESIAN_POINT('Ctrl Pts',(131.590722555295,2.48499327898026,48.35));
#80702=CARTESIAN_POINT('',(131.541200036183,3.00497958064079,48.5));
#80703=CARTESIAN_POINT('Ctrl Pts',(131.541200036183,3.00497958064079,48.5));
#80704=CARTESIAN_POINT('Ctrl Pts',(131.590722555295,2.81214186549187,48.5));
#80705=CARTESIAN_POINT('Ctrl Pts',(131.590722555295,2.48499327898026,48.5));
#80706=CARTESIAN_POINT('',(131.541200036183,3.00497958064079,48.35));
#80707=CARTESIAN_POINT('',(131.541200036183,3.00497958064079,48.5));
#80708=CARTESIAN_POINT('Ctrl Pts',(131.541200036183,3.00497958064079,48.35));
#80709=CARTESIAN_POINT('Ctrl Pts',(131.590722555295,2.81214186549187,48.35));
#80710=CARTESIAN_POINT('Ctrl Pts',(131.590722555295,2.48499327898026,48.35));
#80711=CARTESIAN_POINT('Ctrl Pts',(131.404638046399,3.33212831616402,48.5));
#80712=CARTESIAN_POINT('Ctrl Pts',(131.404638046399,3.33212831616402,48.35));
#80713=CARTESIAN_POINT('Ctrl Pts',(131.491677517071,3.19781729578972,48.5));
#80714=CARTESIAN_POINT('Ctrl Pts',(131.491677517071,3.19781729578972,48.35));
#80715=CARTESIAN_POINT('Ctrl Pts',(131.541200036183,3.00497958064079,48.5));
#80716=CARTESIAN_POINT('Ctrl Pts',(131.541200036183,3.00497958064079,48.35));
#80717=CARTESIAN_POINT('',(131.404638046399,3.33212831616402,48.5));
#80718=CARTESIAN_POINT('Ctrl Pts',(131.404638046399,3.33212831616402,48.5));
#80719=CARTESIAN_POINT('Ctrl Pts',(131.491677517071,3.19781729578972,48.5));
#80720=CARTESIAN_POINT('Ctrl Pts',(131.541200036183,3.00497958064079,48.5));
#80721=CARTESIAN_POINT('',(131.404638046399,3.33212831616402,48.35));
#80722=CARTESIAN_POINT('',(131.404638046399,3.33212831616402,48.5));
#80723=CARTESIAN_POINT('Ctrl Pts',(131.404638046399,3.33212831616402,48.35));
#80724=CARTESIAN_POINT('Ctrl Pts',(131.491677517071,3.19781729578972,48.35));
#80725=CARTESIAN_POINT('Ctrl Pts',(131.541200036183,3.00497958064079,48.35));
#80726=CARTESIAN_POINT('Ctrl Pts',(131.184038275853,3.5377217233181,48.5));
#80727=CARTESIAN_POINT('Ctrl Pts',(131.184038275853,3.5377217233181,48.35));
#80728=CARTESIAN_POINT('Ctrl Pts',(131.317598575726,3.46643933653831,48.5));
#80729=CARTESIAN_POINT('Ctrl Pts',(131.317598575726,3.46643933653831,48.35));
#80730=CARTESIAN_POINT('Ctrl Pts',(131.404638046399,3.33212831616402,48.5));
#80731=CARTESIAN_POINT('Ctrl Pts',(131.404638046399,3.33212831616402,48.35));
#80732=CARTESIAN_POINT('',(131.184038275853,3.5377217233181,48.5));
#80733=CARTESIAN_POINT('Ctrl Pts',(131.184038275853,3.5377217233181,48.5));
#80734=CARTESIAN_POINT('Ctrl Pts',(131.317598575726,3.46643933653831,48.5));
#80735=CARTESIAN_POINT('Ctrl Pts',(131.404638046399,3.33212831616402,48.5));
#80736=CARTESIAN_POINT('',(131.184038275853,3.5377217233181,48.35));
#80737=CARTESIAN_POINT('',(131.184038275853,3.5377217233181,48.5));
#80738=CARTESIAN_POINT('Ctrl Pts',(131.184038275853,3.5377217233181,48.35));
#80739=CARTESIAN_POINT('Ctrl Pts',(131.317598575726,3.46643933653831,48.35));
#80740=CARTESIAN_POINT('Ctrl Pts',(131.404638046399,3.33212831616402,48.35));
#80741=CARTESIAN_POINT('Ctrl Pts',(130.873396748677,3.60900411009789,48.5));
#80742=CARTESIAN_POINT('Ctrl Pts',(130.873396748677,3.60900411009789,48.35));
#80743=CARTESIAN_POINT('Ctrl Pts',(131.050477379933,3.60900411009789,48.5));
#80744=CARTESIAN_POINT('Ctrl Pts',(131.050477379933,3.60900411009789,48.35));
#80745=CARTESIAN_POINT('Ctrl Pts',(131.184038275853,3.5377217233181,48.5));
#80746=CARTESIAN_POINT('Ctrl Pts',(131.184038275853,3.5377217233181,48.35));
#80747=CARTESIAN_POINT('',(130.873396748677,3.60900411009789,48.5));
#80748=CARTESIAN_POINT('Ctrl Pts',(130.873396748677,3.60900411009789,48.5));
#80749=CARTESIAN_POINT('Ctrl Pts',(131.050477379933,3.60900411009789,48.5));
#80750=CARTESIAN_POINT('Ctrl Pts',(131.184038275853,3.5377217233181,48.5));
#80751=CARTESIAN_POINT('',(130.873396748677,3.60900411009789,48.35));
#80752=CARTESIAN_POINT('',(130.873396748677,3.60900411009789,48.5));
#80753=CARTESIAN_POINT('Ctrl Pts',(130.873396748677,3.60900411009789,48.35));
#80754=CARTESIAN_POINT('Ctrl Pts',(131.050477379933,3.60900411009789,48.35));
#80755=CARTESIAN_POINT('Ctrl Pts',(131.184038275853,3.5377217233181,48.35));
#80756=CARTESIAN_POINT('Ctrl Pts',(130.474965924397,3.47994545102119,48.5));
#80757=CARTESIAN_POINT('Ctrl Pts',(130.474965924397,3.47994545102119,48.35));
#80758=CARTESIAN_POINT('Ctrl Pts',(130.63328778185,3.60900411009789,48.5));
#80759=CARTESIAN_POINT('Ctrl Pts',(130.63328778185,3.60900411009789,48.35));
#80760=CARTESIAN_POINT('Ctrl Pts',(130.873396748677,3.60900411009789,48.5));
#80761=CARTESIAN_POINT('Ctrl Pts',(130.873396748677,3.60900411009789,48.35));
#80762=CARTESIAN_POINT('',(130.474965924397,3.47994545102119,48.5));
#80763=CARTESIAN_POINT('Ctrl Pts',(130.474965924397,3.47994545102119,48.5));
#80764=CARTESIAN_POINT('Ctrl Pts',(130.63328778185,3.60900411009789,48.5));
#80765=CARTESIAN_POINT('Ctrl Pts',(130.873396748677,3.60900411009789,48.5));
#80766=CARTESIAN_POINT('',(130.474965924397,3.47994545102119,48.35));
#80767=CARTESIAN_POINT('',(130.474965924397,3.47994545102119,48.5));
#80768=CARTESIAN_POINT('Ctrl Pts',(130.474965924397,3.47994545102119,48.35));
#80769=CARTESIAN_POINT('Ctrl Pts',(130.63328778185,3.60900411009789,48.35));
#80770=CARTESIAN_POINT('Ctrl Pts',(130.873396748677,3.60900411009789,48.35));
#80771=CARTESIAN_POINT('Ctrl Pts',(130.236357206479,3.11302864551544,48.5));
#80772=CARTESIAN_POINT('Ctrl Pts',(130.236357206479,3.11302864551544,48.35));
#80773=CARTESIAN_POINT('Ctrl Pts',(130.316643768921,3.3508867919445,48.5));
#80774=CARTESIAN_POINT('Ctrl Pts',(130.316643768921,3.3508867919445,48.35));
#80775=CARTESIAN_POINT('Ctrl Pts',(130.474965924397,3.47994545102119,48.5));
#80776=CARTESIAN_POINT('Ctrl Pts',(130.474965924397,3.47994545102119,48.35));
#80777=CARTESIAN_POINT('',(130.236357206479,3.11302864551544,48.5));
#80778=CARTESIAN_POINT('Ctrl Pts',(130.236357206479,3.11302864551544,48.5));
#80779=CARTESIAN_POINT('Ctrl Pts',(130.316643768921,3.3508867919445,48.5));
#80780=CARTESIAN_POINT('Ctrl Pts',(130.474965924397,3.47994545102119,48.5));
#80781=CARTESIAN_POINT('',(130.236357206479,3.11302864551544,48.35));
#80782=CARTESIAN_POINT('',(130.236357206479,3.11302864551544,48.5));
#80783=CARTESIAN_POINT('Ctrl Pts',(130.236357206479,3.11302864551544,48.35));
#80784=CARTESIAN_POINT('Ctrl Pts',(130.316643768921,3.3508867919445,48.35));
#80785=CARTESIAN_POINT('Ctrl Pts',(130.474965924397,3.47994545102119,48.35));
#80786=CARTESIAN_POINT('Ctrl Pts',(130.156070942059,2.48499327898026,48.5));
#80787=CARTESIAN_POINT('Ctrl Pts',(130.156070942059,2.48499327898026,48.35));
#80788=CARTESIAN_POINT('Ctrl Pts',(130.156070942059,2.87517049908638,48.5));
#80789=CARTESIAN_POINT('Ctrl Pts',(130.156070942059,2.87517049908638,48.35));
#80790=CARTESIAN_POINT('Ctrl Pts',(130.236357206479,3.11302864551544,48.5));
#80791=CARTESIAN_POINT('Ctrl Pts',(130.236357206479,3.11302864551544,48.35));
#80792=CARTESIAN_POINT('',(130.156070942059,2.48499327898026,48.5));
#80793=CARTESIAN_POINT('Ctrl Pts',(130.156070942059,2.48499327898026,48.5));
#80794=CARTESIAN_POINT('Ctrl Pts',(130.156070942059,2.87517049908638,48.5));
#80795=CARTESIAN_POINT('Ctrl Pts',(130.236357206479,3.11302864551544,48.5));
#80796=CARTESIAN_POINT('',(130.156070942059,2.48499327898026,48.35));
#80797=CARTESIAN_POINT('',(130.156070942059,2.48499327898026,48.5));
#80798=CARTESIAN_POINT('Ctrl Pts',(130.156070942059,2.48499327898026,48.35));
#80799=CARTESIAN_POINT('Ctrl Pts',(130.156070942059,2.87517049908638,48.35));
#80800=CARTESIAN_POINT('Ctrl Pts',(130.236357206479,3.11302864551544,48.35));
#80801=CARTESIAN_POINT('Ctrl Pts',(130.373669618741,1.59058684110642,48.5));
#80802=CARTESIAN_POINT('Ctrl Pts',(130.373669618741,1.59058684110642,48.35));
#80803=CARTESIAN_POINT('Ctrl Pts',(130.156070942059,1.86521166563034,48.5));
#80804=CARTESIAN_POINT('Ctrl Pts',(130.156070942059,1.86521166563034,48.35));
#80805=CARTESIAN_POINT('Ctrl Pts',(130.156070942059,2.48499327898026,48.5));
#80806=CARTESIAN_POINT('Ctrl Pts',(130.156070942059,2.48499327898026,48.35));
#80807=CARTESIAN_POINT('Ctrl Pts',(130.373669618741,1.59058684110642,48.5));
#80808=CARTESIAN_POINT('Ctrl Pts',(130.156070942059,1.86521166563034,48.5));
#80809=CARTESIAN_POINT('Ctrl Pts',(130.156070942059,2.48499327898026,48.5));
#80810=CARTESIAN_POINT('Ctrl Pts',(130.373669618741,1.59058684110642,48.35));
#80811=CARTESIAN_POINT('Ctrl Pts',(130.156070942059,1.86521166563034,48.35));
#80812=CARTESIAN_POINT('Ctrl Pts',(130.156070942059,2.48499327898026,48.35));
#80813=CARTESIAN_POINT('Origin',(129.999999681488,2.48574362695217,48.35));
#80814=CARTESIAN_POINT('Ctrl Pts',(128.901500606909,1.80593454837799,48.5));
#80815=CARTESIAN_POINT('Ctrl Pts',(128.901500606909,1.80593454837799,48.35));
#80816=CARTESIAN_POINT('Ctrl Pts',(128.83246918954,1.73315161466599,48.5));
#80817=CARTESIAN_POINT('Ctrl Pts',(128.83246918954,1.73315161466599,48.35));
#80818=CARTESIAN_POINT('Ctrl Pts',(128.787448758259,1.65961825847626,48.5));
#80819=CARTESIAN_POINT('Ctrl Pts',(128.787448758259,1.65961825847626,48.35));
#80820=CARTESIAN_POINT('',(128.901500606909,1.80593454837799,48.5));
#80821=CARTESIAN_POINT('',(128.787448758259,1.65961825847626,48.5));
#80822=CARTESIAN_POINT('Ctrl Pts',(128.901500606909,1.80593454837799,48.5));
#80823=CARTESIAN_POINT('Ctrl Pts',(128.83246918954,1.73315161466599,48.5));
#80824=CARTESIAN_POINT('Ctrl Pts',(128.787448758259,1.65961825847626,48.5));
#80825=CARTESIAN_POINT('',(128.901500606909,1.80593454837799,48.35));
#80826=CARTESIAN_POINT('',(128.901500606909,1.80593454837799,48.5));
#80827=CARTESIAN_POINT('',(128.787448758259,1.65961825847626,48.35));
#80828=CARTESIAN_POINT('Ctrl Pts',(128.901500606909,1.80593454837799,48.35));
#80829=CARTESIAN_POINT('Ctrl Pts',(128.83246918954,1.73315161466599,48.35));
#80830=CARTESIAN_POINT('Ctrl Pts',(128.787448758259,1.65961825847626,48.35));
#80831=CARTESIAN_POINT('',(128.787448758259,1.65961825847626,48.5));
#80832=CARTESIAN_POINT('Ctrl Pts',(129.213642532006,2.08281049132347,48.5));
#80833=CARTESIAN_POINT('Ctrl Pts',(129.213642532006,2.08281049132347,48.35));
#80834=CARTESIAN_POINT('Ctrl Pts',(128.970531875268,1.87871778011322,48.5));
#80835=CARTESIAN_POINT('Ctrl Pts',(128.970531875268,1.87871778011322,48.35));
#80836=CARTESIAN_POINT('Ctrl Pts',(128.901500606909,1.80593454837799,48.5));
#80837=CARTESIAN_POINT('Ctrl Pts',(128.901500606909,1.80593454837799,48.35));
#80838=CARTESIAN_POINT('',(129.213642532006,2.08281049132347,48.5));
#80839=CARTESIAN_POINT('Ctrl Pts',(129.213642532006,2.08281049132347,48.5));
#80840=CARTESIAN_POINT('Ctrl Pts',(128.970531875268,1.87871778011322,48.5));
#80841=CARTESIAN_POINT('Ctrl Pts',(128.901500606909,1.80593454837799,48.5));
#80842=CARTESIAN_POINT('',(129.213642532006,2.08281049132347,48.35));
#80843=CARTESIAN_POINT('',(129.213642532006,2.08281049132347,48.5));
#80844=CARTESIAN_POINT('Ctrl Pts',(129.213642532006,2.08281049132347,48.35));
#80845=CARTESIAN_POINT('Ctrl Pts',(128.970531875268,1.87871778011322,48.35));
#80846=CARTESIAN_POINT('Ctrl Pts',(128.901500606909,1.80593454837799,48.35));
#80847=CARTESIAN_POINT('Ctrl Pts',(129.630081707612,2.46998646855354,48.5));
#80848=CARTESIAN_POINT('Ctrl Pts',(129.630081707612,2.46998646855354,48.35));
#80849=CARTESIAN_POINT('Ctrl Pts',(129.5047748629,2.32892239093781,48.5));
#80850=CARTESIAN_POINT('Ctrl Pts',(129.5047748629,2.32892239093781,48.35));
#80851=CARTESIAN_POINT('Ctrl Pts',(129.213642532006,2.08281049132347,48.5));
#80852=CARTESIAN_POINT('Ctrl Pts',(129.213642532006,2.08281049132347,48.35));
#80853=CARTESIAN_POINT('',(129.630081707612,2.46998646855354,48.5));
#80854=CARTESIAN_POINT('Ctrl Pts',(129.630081707612,2.46998646855354,48.5));
#80855=CARTESIAN_POINT('Ctrl Pts',(129.5047748629,2.32892239093781,48.5));
#80856=CARTESIAN_POINT('Ctrl Pts',(129.213642532006,2.08281049132347,48.5));
#80857=CARTESIAN_POINT('',(129.630081707612,2.46998646855354,48.35));
#80858=CARTESIAN_POINT('',(129.630081707612,2.46998646855354,48.5));
#80859=CARTESIAN_POINT('Ctrl Pts',(129.630081707612,2.46998646855354,48.35));
#80860=CARTESIAN_POINT('Ctrl Pts',(129.5047748629,2.32892239093781,48.35));
#80861=CARTESIAN_POINT('Ctrl Pts',(129.213642532006,2.08281049132347,48.35));
#80862=CARTESIAN_POINT('Ctrl Pts',(129.809413308278,2.73860850930214,48.5));
#80863=CARTESIAN_POINT('Ctrl Pts',(129.809413308278,2.73860850930214,48.35));
#80864=CARTESIAN_POINT('Ctrl Pts',(129.755388850346,2.61105054616928,48.5));
#80865=CARTESIAN_POINT('Ctrl Pts',(129.755388850346,2.61105054616928,48.35));
#80866=CARTESIAN_POINT('Ctrl Pts',(129.630081707612,2.46998646855354,48.5));
#80867=CARTESIAN_POINT('Ctrl Pts',(129.630081707612,2.46998646855354,48.35));
#80868=CARTESIAN_POINT('',(129.809413308278,2.73860850930214,48.5));
#80869=CARTESIAN_POINT('Ctrl Pts',(129.809413308278,2.73860850930214,48.5));
#80870=CARTESIAN_POINT('Ctrl Pts',(129.755388850346,2.61105054616928,48.5));
#80871=CARTESIAN_POINT('Ctrl Pts',(129.630081707612,2.46998646855354,48.5));
#80872=CARTESIAN_POINT('',(129.809413308278,2.73860850930214,48.35));
#80873=CARTESIAN_POINT('',(129.809413308278,2.73860850930214,48.5));
#80874=CARTESIAN_POINT('Ctrl Pts',(129.809413308278,2.73860850930214,48.35));
#80875=CARTESIAN_POINT('Ctrl Pts',(129.755388850346,2.61105054616928,48.35));
#80876=CARTESIAN_POINT('Ctrl Pts',(129.630081707612,2.46998646855354,48.35));
#80877=CARTESIAN_POINT('Ctrl Pts',(129.863437766209,2.99822652339935,48.5));
#80878=CARTESIAN_POINT('Ctrl Pts',(129.863437766209,2.99822652339935,48.35));
#80879=CARTESIAN_POINT('Ctrl Pts',(129.863437766209,2.866166472435,48.5));
#80880=CARTESIAN_POINT('Ctrl Pts',(129.863437766209,2.866166472435,48.35));
#80881=CARTESIAN_POINT('Ctrl Pts',(129.809413308278,2.73860850930214,48.5));
#80882=CARTESIAN_POINT('Ctrl Pts',(129.809413308278,2.73860850930214,48.35));
#80883=CARTESIAN_POINT('',(129.863437766209,2.99822652339935,48.5));
#80884=CARTESIAN_POINT('Ctrl Pts',(129.863437766209,2.99822652339935,48.5));
#80885=CARTESIAN_POINT('Ctrl Pts',(129.863437766209,2.866166472435,48.5));
#80886=CARTESIAN_POINT('Ctrl Pts',(129.809413308278,2.73860850930214,48.5));
#80887=CARTESIAN_POINT('',(129.863437766209,2.99822652339935,48.35));
#80888=CARTESIAN_POINT('',(129.863437766209,2.99822652339935,48.5));
#80889=CARTESIAN_POINT('Ctrl Pts',(129.863437766209,2.99822652339935,48.35));
#80890=CARTESIAN_POINT('Ctrl Pts',(129.863437766209,2.866166472435,48.35));
#80891=CARTESIAN_POINT('Ctrl Pts',(129.809413308278,2.73860850930214,48.35));
#80892=CARTESIAN_POINT('Ctrl Pts',(129.678854102269,3.43342432379723,48.5));
#80893=CARTESIAN_POINT('Ctrl Pts',(129.678854102269,3.43342432379723,48.35));
#80894=CARTESIAN_POINT('Ctrl Pts',(129.863437766209,3.25784453749657,48.5));
#80895=CARTESIAN_POINT('Ctrl Pts',(129.863437766209,3.25784453749657,48.35));
#80896=CARTESIAN_POINT('Ctrl Pts',(129.863437766209,2.99822652339935,48.5));
#80897=CARTESIAN_POINT('Ctrl Pts',(129.863437766209,2.99822652339935,48.35));
#80898=CARTESIAN_POINT('',(129.678854102269,3.43342432379723,48.5));
#80899=CARTESIAN_POINT('Ctrl Pts',(129.678854102269,3.43342432379723,48.5));
#80900=CARTESIAN_POINT('Ctrl Pts',(129.863437766209,3.25784453749657,48.5));
#80901=CARTESIAN_POINT('Ctrl Pts',(129.863437766209,2.99822652339935,48.5));
#80902=CARTESIAN_POINT('',(129.678854102269,3.43342432379723,48.35));
#80903=CARTESIAN_POINT('',(129.678854102269,3.43342432379723,48.5));
#80904=CARTESIAN_POINT('Ctrl Pts',(129.678854102269,3.43342432379723,48.35));
#80905=CARTESIAN_POINT('Ctrl Pts',(129.863437766209,3.25784453749657,48.35));
#80906=CARTESIAN_POINT('Ctrl Pts',(129.863437766209,2.99822652339935,48.35));
#80907=CARTESIAN_POINT('Ctrl Pts',(129.177626127377,3.60900411009789,48.5));
#80908=CARTESIAN_POINT('Ctrl Pts',(129.177626127377,3.60900411009789,48.35));
#80909=CARTESIAN_POINT('Ctrl Pts',(129.494270140305,3.60900411009789,48.5));
#80910=CARTESIAN_POINT('Ctrl Pts',(129.494270140305,3.60900411009789,48.35));
#80911=CARTESIAN_POINT('Ctrl Pts',(129.678854102269,3.43342432379723,48.5));
#80912=CARTESIAN_POINT('Ctrl Pts',(129.678854102269,3.43342432379723,48.35));
#80913=CARTESIAN_POINT('',(129.177626127377,3.60900411009789,48.5));
#80914=CARTESIAN_POINT('Ctrl Pts',(129.177626127377,3.60900411009789,48.5));
#80915=CARTESIAN_POINT('Ctrl Pts',(129.494270140305,3.60900411009789,48.5));
#80916=CARTESIAN_POINT('Ctrl Pts',(129.678854102269,3.43342432379723,48.5));
#80917=CARTESIAN_POINT('',(129.177626127377,3.60900411009789,48.35));
#80918=CARTESIAN_POINT('',(129.177626127377,3.60900411009789,48.5));
#80919=CARTESIAN_POINT('Ctrl Pts',(129.177626127377,3.60900411009789,48.35));
#80920=CARTESIAN_POINT('Ctrl Pts',(129.494270140305,3.60900411009789,48.35));
#80921=CARTESIAN_POINT('Ctrl Pts',(129.678854102269,3.43342432379723,48.35));
#80922=CARTESIAN_POINT('Ctrl Pts',(128.677898997441,3.446180164814,48.5));
#80923=CARTESIAN_POINT('Ctrl Pts',(128.677898997441,3.446180164814,48.35));
#80924=CARTESIAN_POINT('Ctrl Pts',(128.863983506337,3.60900411009789,48.5));
#80925=CARTESIAN_POINT('Ctrl Pts',(128.863983506337,3.60900411009789,48.35));
#80926=CARTESIAN_POINT('Ctrl Pts',(129.177626127377,3.60900411009789,48.5));
#80927=CARTESIAN_POINT('Ctrl Pts',(129.177626127377,3.60900411009789,48.35));
#80928=CARTESIAN_POINT('',(128.677898997441,3.446180164814,48.5));
#80929=CARTESIAN_POINT('Ctrl Pts',(128.677898997441,3.446180164814,48.5));
#80930=CARTESIAN_POINT('Ctrl Pts',(128.863983506337,3.60900411009789,48.5));
#80931=CARTESIAN_POINT('Ctrl Pts',(129.177626127377,3.60900411009789,48.5));
#80932=CARTESIAN_POINT('',(128.677898997441,3.446180164814,48.35));
#80933=CARTESIAN_POINT('',(128.677898997441,3.446180164814,48.5));
#80934=CARTESIAN_POINT('Ctrl Pts',(128.677898997441,3.446180164814,48.35));
#80935=CARTESIAN_POINT('Ctrl Pts',(128.863983506337,3.60900411009789,48.35));
#80936=CARTESIAN_POINT('Ctrl Pts',(129.177626127377,3.60900411009789,48.35));
#80937=CARTESIAN_POINT('Ctrl Pts',(128.463301414624,2.97271499037743,48.5));
#80938=CARTESIAN_POINT('Ctrl Pts',(128.463301414624,2.97271499037743,48.35));
#80939=CARTESIAN_POINT('Ctrl Pts',(128.491814339533,3.28335621953011,48.5));
#80940=CARTESIAN_POINT('Ctrl Pts',(128.491814339533,3.28335621953011,48.35));
#80941=CARTESIAN_POINT('Ctrl Pts',(128.677898997441,3.446180164814,48.5));
#80942=CARTESIAN_POINT('Ctrl Pts',(128.677898997441,3.446180164814,48.35));
#80943=CARTESIAN_POINT('',(128.463301414624,2.97271499037743,48.5));
#80944=CARTESIAN_POINT('Ctrl Pts',(128.463301414624,2.97271499037743,48.5));
#80945=CARTESIAN_POINT('Ctrl Pts',(128.491814339533,3.28335621953011,48.5));
#80946=CARTESIAN_POINT('Ctrl Pts',(128.677898997441,3.446180164814,48.5));
#80947=CARTESIAN_POINT('',(128.463301414624,2.97271499037743,48.35));
#80948=CARTESIAN_POINT('',(128.463301414624,2.97271499037743,48.5));
#80949=CARTESIAN_POINT('Ctrl Pts',(128.463301414624,2.97271499037743,48.35));
#80950=CARTESIAN_POINT('Ctrl Pts',(128.491814339533,3.28335621953011,48.35));
#80951=CARTESIAN_POINT('Ctrl Pts',(128.677898997441,3.446180164814,48.35));
#80952=CARTESIAN_POINT('Origin',(128.740927631035,2.94420206546783,48.5));
#80953=CARTESIAN_POINT('',(128.740927631035,2.94420206546783,48.5));
#80954=CARTESIAN_POINT('',(64.7854329665245,9.51259549925474,48.5));
#80955=CARTESIAN_POINT('',(128.740927631035,2.94420206546783,48.35));
#80956=CARTESIAN_POINT('',(128.740927631035,2.94420206546783,48.5));
#80957=CARTESIAN_POINT('',(128.740927631035,2.94420206546783,48.35));
#80958=CARTESIAN_POINT('Ctrl Pts',(128.859481567517,3.26834926009178,48.5));
#80959=CARTESIAN_POINT('Ctrl Pts',(128.859481567517,3.26834926009178,48.35));
#80960=CARTESIAN_POINT('Ctrl Pts',(128.742428326979,3.15129616856575,48.5));
#80961=CARTESIAN_POINT('Ctrl Pts',(128.742428326979,3.15129616856575,48.35));
#80962=CARTESIAN_POINT('Ctrl Pts',(128.740927631035,2.94420206546783,48.5));
#80963=CARTESIAN_POINT('Ctrl Pts',(128.740927631035,2.94420206546783,48.35));
#80964=CARTESIAN_POINT('',(128.859481567517,3.26834926009178,48.5));
#80965=CARTESIAN_POINT('Ctrl Pts',(128.859481567517,3.26834926009178,48.5));
#80966=CARTESIAN_POINT('Ctrl Pts',(128.742428326979,3.15129616856575,48.5));
#80967=CARTESIAN_POINT('Ctrl Pts',(128.740927631035,2.94420206546783,48.5));
#80968=CARTESIAN_POINT('',(128.859481567517,3.26834926009178,48.35));
#80969=CARTESIAN_POINT('',(128.859481567517,3.26834926009178,48.5));
#80970=CARTESIAN_POINT('Ctrl Pts',(128.859481567517,3.26834926009178,48.35));
#80971=CARTESIAN_POINT('Ctrl Pts',(128.742428326979,3.15129616856575,48.35));
#80972=CARTESIAN_POINT('Ctrl Pts',(128.740927631035,2.94420206546783,48.35));
#80973=CARTESIAN_POINT('Ctrl Pts',(129.171623343602,3.38540250062943,48.5));
#80974=CARTESIAN_POINT('Ctrl Pts',(129.171623343602,3.38540250062943,48.35));
#80975=CARTESIAN_POINT('Ctrl Pts',(128.976534659043,3.38540250062943,48.5));
#80976=CARTESIAN_POINT('Ctrl Pts',(128.976534659043,3.38540250062943,48.35));
#80977=CARTESIAN_POINT('Ctrl Pts',(128.859481567517,3.26834926009178,48.5));
#80978=CARTESIAN_POINT('Ctrl Pts',(128.859481567517,3.26834926009178,48.35));
#80979=CARTESIAN_POINT('',(129.171623343602,3.38540250062943,48.5));
#80980=CARTESIAN_POINT('Ctrl Pts',(129.171623343602,3.38540250062943,48.5));
#80981=CARTESIAN_POINT('Ctrl Pts',(128.976534659043,3.38540250062943,48.5));
#80982=CARTESIAN_POINT('Ctrl Pts',(128.859481567517,3.26834926009178,48.5));
#80983=CARTESIAN_POINT('',(129.171623343602,3.38540250062943,48.35));
#80984=CARTESIAN_POINT('',(129.171623343602,3.38540250062943,48.5));
#80985=CARTESIAN_POINT('Ctrl Pts',(129.171623343602,3.38540250062943,48.35));
#80986=CARTESIAN_POINT('Ctrl Pts',(128.976534659043,3.38540250062943,48.35));
#80987=CARTESIAN_POINT('Ctrl Pts',(128.859481567517,3.26834926009178,48.35));
#80988=CARTESIAN_POINT('Ctrl Pts',(129.471009427682,3.27510246634483,48.5));
#80989=CARTESIAN_POINT('Ctrl Pts',(129.471009427682,3.27510246634483,48.35));
#80990=CARTESIAN_POINT('Ctrl Pts',(129.356207305565,3.38540250062943,48.5));
#80991=CARTESIAN_POINT('Ctrl Pts',(129.356207305565,3.38540250062943,48.35));
#80992=CARTESIAN_POINT('Ctrl Pts',(129.171623343602,3.38540250062943,48.5));
#80993=CARTESIAN_POINT('Ctrl Pts',(129.171623343602,3.38540250062943,48.35));
#80994=CARTESIAN_POINT('',(129.471009427682,3.27510246634483,48.5));
#80995=CARTESIAN_POINT('Ctrl Pts',(129.471009427682,3.27510246634483,48.5));
#80996=CARTESIAN_POINT('Ctrl Pts',(129.356207305565,3.38540250062943,48.5));
#80997=CARTESIAN_POINT('Ctrl Pts',(129.171623343602,3.38540250062943,48.5));
#80998=CARTESIAN_POINT('',(129.471009427682,3.27510246634483,48.35));
#80999=CARTESIAN_POINT('',(129.471009427682,3.27510246634483,48.5));
#81000=CARTESIAN_POINT('Ctrl Pts',(129.471009427682,3.27510246634483,48.35));
#81001=CARTESIAN_POINT('Ctrl Pts',(129.356207305565,3.38540250062943,48.35));
#81002=CARTESIAN_POINT('Ctrl Pts',(129.171623343602,3.38540250062943,48.35));
#81003=CARTESIAN_POINT('Ctrl Pts',(129.585811847821,3.00422930717468,48.5));
#81004=CARTESIAN_POINT('Ctrl Pts',(129.585811847821,3.00422930717468,48.35));
#81005=CARTESIAN_POINT('Ctrl Pts',(129.585811847821,3.16480228304863,48.5));
#81006=CARTESIAN_POINT('Ctrl Pts',(129.585811847821,3.16480228304863,48.35));
#81007=CARTESIAN_POINT('Ctrl Pts',(129.471009427682,3.27510246634483,48.5));
#81008=CARTESIAN_POINT('Ctrl Pts',(129.471009427682,3.27510246634483,48.35));
#81009=CARTESIAN_POINT('',(129.585811847821,3.00422930717468,48.5));
#81010=CARTESIAN_POINT('Ctrl Pts',(129.585811847821,3.00422930717468,48.5));
#81011=CARTESIAN_POINT('Ctrl Pts',(129.585811847821,3.16480228304863,48.5));
#81012=CARTESIAN_POINT('Ctrl Pts',(129.471009427682,3.27510246634483,48.5));
#81013=CARTESIAN_POINT('',(129.585811847821,3.00422930717468,48.35));
#81014=CARTESIAN_POINT('',(129.585811847821,3.00422930717468,48.5));
#81015=CARTESIAN_POINT('Ctrl Pts',(129.585811847821,3.00422930717468,48.35));
#81016=CARTESIAN_POINT('Ctrl Pts',(129.585811847821,3.16480228304863,48.35));
#81017=CARTESIAN_POINT('Ctrl Pts',(129.471009427682,3.27510246634483,48.35));
#81018=CARTESIAN_POINT('Ctrl Pts',(129.459754282609,2.6793315410614,48.5));
#81019=CARTESIAN_POINT('Ctrl Pts',(129.459754282609,2.6793315410614,48.35));
#81020=CARTESIAN_POINT('Ctrl Pts',(129.585811847821,2.85115966200829,48.5));
#81021=CARTESIAN_POINT('Ctrl Pts',(129.585811847821,2.85115966200829,48.35));
#81022=CARTESIAN_POINT('Ctrl Pts',(129.585811847821,3.00422930717468,48.5));
#81023=CARTESIAN_POINT('Ctrl Pts',(129.585811847821,3.00422930717468,48.35));
#81024=CARTESIAN_POINT('',(129.459754282609,2.6793315410614,48.5));
#81025=CARTESIAN_POINT('Ctrl Pts',(129.459754282609,2.6793315410614,48.5));
#81026=CARTESIAN_POINT('Ctrl Pts',(129.585811847821,2.85115966200829,48.5));
#81027=CARTESIAN_POINT('Ctrl Pts',(129.585811847821,3.00422930717468,48.5));
#81028=CARTESIAN_POINT('',(129.459754282609,2.6793315410614,48.35));
#81029=CARTESIAN_POINT('',(129.459754282609,2.6793315410614,48.5));
#81030=CARTESIAN_POINT('Ctrl Pts',(129.459754282609,2.6793315410614,48.35));
#81031=CARTESIAN_POINT('Ctrl Pts',(129.585811847821,2.85115966200829,48.35));
#81032=CARTESIAN_POINT('Ctrl Pts',(129.585811847821,3.00422930717468,48.35));
#81033=CARTESIAN_POINT('Ctrl Pts',(128.975034112111,2.21336984634399,48.5));
#81034=CARTESIAN_POINT('Ctrl Pts',(128.975034112111,2.21336984634399,48.35));
#81035=CARTESIAN_POINT('Ctrl Pts',(129.33369701542,2.50750356912613,48.5));
#81036=CARTESIAN_POINT('Ctrl Pts',(129.33369701542,2.50750356912613,48.35));
#81037=CARTESIAN_POINT('Ctrl Pts',(129.459754282609,2.6793315410614,48.5));
#81038=CARTESIAN_POINT('Ctrl Pts',(129.459754282609,2.6793315410614,48.35));
#81039=CARTESIAN_POINT('',(128.975034112111,2.21336984634399,48.5));
#81040=CARTESIAN_POINT('Ctrl Pts',(128.975034112111,2.21336984634399,48.5));
#81041=CARTESIAN_POINT('Ctrl Pts',(129.33369701542,2.50750356912613,48.5));
#81042=CARTESIAN_POINT('Ctrl Pts',(129.459754282609,2.6793315410614,48.5));
#81043=CARTESIAN_POINT('',(128.975034112111,2.21336984634399,48.35));
#81044=CARTESIAN_POINT('',(128.975034112111,2.21336984634399,48.5));
#81045=CARTESIAN_POINT('Ctrl Pts',(128.975034112111,2.21336984634399,48.35));
#81046=CARTESIAN_POINT('Ctrl Pts',(129.33369701542,2.50750356912613,48.35));
#81047=CARTESIAN_POINT('Ctrl Pts',(129.459754282609,2.6793315410614,48.35));
#81048=CARTESIAN_POINT('Ctrl Pts',(128.621623421088,1.88021832704544,48.5));
#81049=CARTESIAN_POINT('Ctrl Pts',(128.621623421088,1.88021832704544,48.35));
#81050=CARTESIAN_POINT('Ctrl Pts',(128.743929022923,2.02428394556046,48.5));
#81051=CARTESIAN_POINT('Ctrl Pts',(128.743929022923,2.02428394556046,48.35));
#81052=CARTESIAN_POINT('Ctrl Pts',(128.975034112111,2.21336984634399,48.5));
#81053=CARTESIAN_POINT('Ctrl Pts',(128.975034112111,2.21336984634399,48.35));
#81054=CARTESIAN_POINT('',(128.621623421088,1.88021832704544,48.5));
#81055=CARTESIAN_POINT('Ctrl Pts',(128.621623421088,1.88021832704544,48.5));
#81056=CARTESIAN_POINT('Ctrl Pts',(128.743929022923,2.02428394556046,48.5));
#81057=CARTESIAN_POINT('Ctrl Pts',(128.975034112111,2.21336984634399,48.5));
#81058=CARTESIAN_POINT('',(128.621623421088,1.88021832704544,48.35));
#81059=CARTESIAN_POINT('',(128.621623421088,1.88021832704544,48.5));
#81060=CARTESIAN_POINT('Ctrl Pts',(128.621623421088,1.88021832704544,48.35));
#81061=CARTESIAN_POINT('Ctrl Pts',(128.743929022923,2.02428394556046,48.35));
#81062=CARTESIAN_POINT('Ctrl Pts',(128.975034112111,2.21336984634399,48.35));
#81063=CARTESIAN_POINT('Ctrl Pts',(128.443792516366,1.58758544921875,48.5));
#81064=CARTESIAN_POINT('Ctrl Pts',(128.443792516366,1.58758544921875,48.35));
#81065=CARTESIAN_POINT('Ctrl Pts',(128.499317819253,1.73615300655365,48.5));
#81066=CARTESIAN_POINT('Ctrl Pts',(128.499317819253,1.73615300655365,48.35));
#81067=CARTESIAN_POINT('Ctrl Pts',(128.621623421088,1.88021832704544,48.5));
#81068=CARTESIAN_POINT('Ctrl Pts',(128.621623421088,1.88021832704544,48.35));
#81069=CARTESIAN_POINT('',(128.443792516366,1.58758544921875,48.5));
#81070=CARTESIAN_POINT('Ctrl Pts',(128.443792516366,1.58758544921875,48.5));
#81071=CARTESIAN_POINT('Ctrl Pts',(128.499317819253,1.73615300655365,48.5));
#81072=CARTESIAN_POINT('Ctrl Pts',(128.621623421088,1.88021832704544,48.5));
#81073=CARTESIAN_POINT('',(128.443792516366,1.58758544921875,48.35));
#81074=CARTESIAN_POINT('',(128.443792516366,1.58758544921875,48.5));
#81075=CARTESIAN_POINT('Ctrl Pts',(128.443792516366,1.58758544921875,48.35));
#81076=CARTESIAN_POINT('Ctrl Pts',(128.499317819253,1.73615300655365,48.35));
#81077=CARTESIAN_POINT('Ctrl Pts',(128.621623421088,1.88021832704544,48.35));
#81078=CARTESIAN_POINT('Ctrl Pts',(128.412278199568,1.40000009536743,48.5));
#81079=CARTESIAN_POINT('Ctrl Pts',(128.412278199568,1.40000009536743,48.35));
#81080=CARTESIAN_POINT('Ctrl Pts',(128.409276807681,1.49754428863525,48.5));
#81081=CARTESIAN_POINT('Ctrl Pts',(128.409276807681,1.49754428863525,48.35));
#81082=CARTESIAN_POINT('Ctrl Pts',(128.443792516366,1.58758544921875,48.5));
#81083=CARTESIAN_POINT('Ctrl Pts',(128.443792516366,1.58758544921875,48.35));
#81084=CARTESIAN_POINT('',(128.412278199568,1.40000009536743,48.5));
#81085=CARTESIAN_POINT('Ctrl Pts',(128.412278199568,1.40000009536743,48.5));
#81086=CARTESIAN_POINT('Ctrl Pts',(128.409276807681,1.49754428863525,48.5));
#81087=CARTESIAN_POINT('Ctrl Pts',(128.443792516366,1.58758544921875,48.5));
#81088=CARTESIAN_POINT('',(128.412278199568,1.40000009536743,48.35));
#81089=CARTESIAN_POINT('',(128.412278199568,1.40000009536743,48.5));
#81090=CARTESIAN_POINT('Ctrl Pts',(128.412278199568,1.40000009536743,48.35));
#81091=CARTESIAN_POINT('Ctrl Pts',(128.409276807681,1.49754428863525,48.35));
#81092=CARTESIAN_POINT('Ctrl Pts',(128.443792516366,1.58758544921875,48.35));
#81093=CARTESIAN_POINT('Origin',(129.866439158097,1.40000009536743,48.5));
#81094=CARTESIAN_POINT('',(129.866439158097,1.40000009536743,48.5));
#81095=CARTESIAN_POINT('',(64.9332195790485,1.40000009536743,48.5));
#81096=CARTESIAN_POINT('',(129.866439158097,1.40000009536743,48.35));
#81097=CARTESIAN_POINT('',(129.866439158097,1.40000009536743,48.5));
#81098=CARTESIAN_POINT('',(129.866439158097,1.40000009536743,48.35));
#81099=CARTESIAN_POINT('Origin',(129.866439158097,1.65961825847626,48.5));
#81100=CARTESIAN_POINT('',(129.866439158097,1.65961825847626,48.5));
#81101=CARTESIAN_POINT('',(129.866439158097,4.82980912923813,48.5));
#81102=CARTESIAN_POINT('',(129.866439158097,1.65961825847626,48.35));
#81103=CARTESIAN_POINT('',(129.866439158097,1.65961825847626,48.5));
#81104=CARTESIAN_POINT('',(129.866439158097,1.65961825847626,48.35));
#81105=CARTESIAN_POINT('Origin',(128.787448758259,1.65961825847626,48.5));
#81106=CARTESIAN_POINT('',(64.3937243791297,1.65961825847626,48.5));
#81107=CARTESIAN_POINT('',(128.787448758259,1.65961825847626,48.35));
#81108=CARTESIAN_POINT('Origin',(129.999999681488,2.48574362695217,48.35));
#81109=CARTESIAN_POINT('Origin',(0.,8.,48.5));
#81110=CARTESIAN_POINT('Ctrl Pts',(120.748090229928,3.38540250062943,48.5));
#81111=CARTESIAN_POINT('Ctrl Pts',(120.748090229928,3.38540250062943,48.35));
#81112=CARTESIAN_POINT('Ctrl Pts',(120.562005423009,3.38540250062943,48.5));
#81113=CARTESIAN_POINT('Ctrl Pts',(120.562005423009,3.38540250062943,48.35));
#81114=CARTESIAN_POINT('Ctrl Pts',(120.450955115259,3.22783091664314,48.5));
#81115=CARTESIAN_POINT('Ctrl Pts',(120.450955115259,3.22783091664314,48.35));
#81116=CARTESIAN_POINT('',(120.748090229928,3.38540250062943,48.5));
#81117=CARTESIAN_POINT('',(120.450955115259,3.22783091664314,48.5));
#81118=CARTESIAN_POINT('Ctrl Pts',(120.748090229928,3.38540250062943,48.5));
#81119=CARTESIAN_POINT('Ctrl Pts',(120.562005423009,3.38540250062943,48.5));
#81120=CARTESIAN_POINT('Ctrl Pts',(120.450955115259,3.22783091664314,48.5));
#81121=CARTESIAN_POINT('',(120.748090229928,3.38540250062943,48.35));
#81122=CARTESIAN_POINT('',(120.748090229928,3.38540250062943,48.5));
#81123=CARTESIAN_POINT('',(120.450955115259,3.22783091664314,48.35));
#81124=CARTESIAN_POINT('Ctrl Pts',(120.748090229928,3.38540250062943,48.35));
#81125=CARTESIAN_POINT('Ctrl Pts',(120.562005423009,3.38540250062943,48.35));
#81126=CARTESIAN_POINT('Ctrl Pts',(120.450955115259,3.22783091664314,48.35));
#81127=CARTESIAN_POINT('',(120.450955115259,3.22783091664314,48.5));
#81128=CARTESIAN_POINT('Ctrl Pts',(121.063983522356,3.2068213224411,48.5));
#81129=CARTESIAN_POINT('Ctrl Pts',(121.063983522356,3.2068213224411,48.35));
#81130=CARTESIAN_POINT('Ctrl Pts',(120.937175832689,3.38540250062943,48.5));
#81131=CARTESIAN_POINT('Ctrl Pts',(120.937175832689,3.38540250062943,48.35));
#81132=CARTESIAN_POINT('Ctrl Pts',(120.748090229928,3.38540250062943,48.5));
#81133=CARTESIAN_POINT('Ctrl Pts',(120.748090229928,3.38540250062943,48.35));
#81134=CARTESIAN_POINT('',(121.063983522356,3.2068213224411,48.5));
#81135=CARTESIAN_POINT('Ctrl Pts',(121.063983522356,3.2068213224411,48.5));
#81136=CARTESIAN_POINT('Ctrl Pts',(120.937175832689,3.38540250062943,48.5));
#81137=CARTESIAN_POINT('Ctrl Pts',(120.748090229928,3.38540250062943,48.5));
#81138=CARTESIAN_POINT('',(121.063983522356,3.2068213224411,48.35));
#81139=CARTESIAN_POINT('',(121.063983522356,3.2068213224411,48.5));
#81140=CARTESIAN_POINT('Ctrl Pts',(121.063983522356,3.2068213224411,48.35));
#81141=CARTESIAN_POINT('Ctrl Pts',(120.937175832689,3.38540250062943,48.35));
#81142=CARTESIAN_POINT('Ctrl Pts',(120.748090229928,3.38540250062943,48.35));
#81143=CARTESIAN_POINT('Ctrl Pts',(121.190791212022,2.48499327898026,48.5));
#81144=CARTESIAN_POINT('Ctrl Pts',(121.190791212022,2.48499327898026,48.35));
#81145=CARTESIAN_POINT('Ctrl Pts',(121.190791212022,3.02824014425278,48.5));
#81146=CARTESIAN_POINT('Ctrl Pts',(121.190791212022,3.02824014425278,48.35));
#81147=CARTESIAN_POINT('Ctrl Pts',(121.063983522356,3.2068213224411,48.5));
#81148=CARTESIAN_POINT('Ctrl Pts',(121.063983522356,3.2068213224411,48.35));
#81149=CARTESIAN_POINT('',(121.190791212022,2.48499327898026,48.5));
#81150=CARTESIAN_POINT('Ctrl Pts',(121.190791212022,2.48499327898026,48.5));
#81151=CARTESIAN_POINT('Ctrl Pts',(121.190791212022,3.02824014425278,48.5));
#81152=CARTESIAN_POINT('Ctrl Pts',(121.063983522356,3.2068213224411,48.5));
#81153=CARTESIAN_POINT('',(121.190791212022,2.48499327898026,48.35));
#81154=CARTESIAN_POINT('',(121.190791212022,2.48499327898026,48.5));
#81155=CARTESIAN_POINT('Ctrl Pts',(121.190791212022,2.48499327898026,48.35));
#81156=CARTESIAN_POINT('Ctrl Pts',(121.190791212022,3.02824014425278,48.35));
#81157=CARTESIAN_POINT('Ctrl Pts',(121.063983522356,3.2068213224411,48.35));
#81158=CARTESIAN_POINT('Ctrl Pts',(121.063983522356,1.76466578245163,48.5));
#81159=CARTESIAN_POINT('Ctrl Pts',(121.063983522356,1.76466578245163,48.35));
#81160=CARTESIAN_POINT('Ctrl Pts',(121.190791212022,1.9447478055954,48.5));
#81161=CARTESIAN_POINT('Ctrl Pts',(121.190791212022,1.9447478055954,48.35));
#81162=CARTESIAN_POINT('Ctrl Pts',(121.190791212022,2.48499327898026,48.5));
#81163=CARTESIAN_POINT('Ctrl Pts',(121.190791212022,2.48499327898026,48.35));
#81164=CARTESIAN_POINT('',(121.063983522356,1.76466578245163,48.5));
#81165=CARTESIAN_POINT('Ctrl Pts',(121.063983522356,1.76466578245163,48.5));
#81166=CARTESIAN_POINT('Ctrl Pts',(121.190791212022,1.9447478055954,48.5));
#81167=CARTESIAN_POINT('Ctrl Pts',(121.190791212022,2.48499327898026,48.5));
#81168=CARTESIAN_POINT('',(121.063983522356,1.76466578245163,48.35));
#81169=CARTESIAN_POINT('',(121.063983522356,1.76466578245163,48.5));
#81170=CARTESIAN_POINT('Ctrl Pts',(121.063983522356,1.76466578245163,48.35));
#81171=CARTESIAN_POINT('Ctrl Pts',(121.190791212022,1.9447478055954,48.35));
#81172=CARTESIAN_POINT('Ctrl Pts',(121.190791212022,2.48499327898026,48.35));
#81173=CARTESIAN_POINT('Ctrl Pts',(120.751091323793,1.58458405733109,48.5));
#81174=CARTESIAN_POINT('Ctrl Pts',(120.751091323793,1.58458405733109,48.35));
#81175=CARTESIAN_POINT('Ctrl Pts',(120.937175832689,1.58458405733109,48.5));
#81176=CARTESIAN_POINT('Ctrl Pts',(120.937175832689,1.58458405733109,48.35));
#81177=CARTESIAN_POINT('Ctrl Pts',(121.063983522356,1.76466578245163,48.5));
#81178=CARTESIAN_POINT('Ctrl Pts',(121.063983522356,1.76466578245163,48.35));
#81179=CARTESIAN_POINT('',(120.751091323793,1.58458405733109,48.5));
#81180=CARTESIAN_POINT('Ctrl Pts',(120.751091323793,1.58458405733109,48.5));
#81181=CARTESIAN_POINT('Ctrl Pts',(120.937175832689,1.58458405733109,48.5));
#81182=CARTESIAN_POINT('Ctrl Pts',(121.063983522356,1.76466578245163,48.5));
#81183=CARTESIAN_POINT('',(120.751091323793,1.58458405733109,48.35));
#81184=CARTESIAN_POINT('',(120.751091323793,1.58458405733109,48.5));
#81185=CARTESIAN_POINT('Ctrl Pts',(120.751091323793,1.58458405733109,48.35));
#81186=CARTESIAN_POINT('Ctrl Pts',(120.937175832689,1.58458405733109,48.35));
#81187=CARTESIAN_POINT('Ctrl Pts',(121.063983522356,1.76466578245163,48.35));
#81188=CARTESIAN_POINT('Ctrl Pts',(120.43819912523,1.76391565799713,48.5));
#81189=CARTESIAN_POINT('Ctrl Pts',(120.43819912523,1.76391565799713,48.35));
#81190=CARTESIAN_POINT('Ctrl Pts',(120.565006814897,1.58458405733109,48.5));
#81191=CARTESIAN_POINT('Ctrl Pts',(120.565006814897,1.58458405733109,48.35));
#81192=CARTESIAN_POINT('Ctrl Pts',(120.751091323793,1.58458405733109,48.5));
#81193=CARTESIAN_POINT('Ctrl Pts',(120.751091323793,1.58458405733109,48.35));
#81194=CARTESIAN_POINT('',(120.43819912523,1.76391565799713,48.5));
#81195=CARTESIAN_POINT('Ctrl Pts',(120.43819912523,1.76391565799713,48.5));
#81196=CARTESIAN_POINT('Ctrl Pts',(120.565006814897,1.58458405733109,48.5));
#81197=CARTESIAN_POINT('Ctrl Pts',(120.751091323793,1.58458405733109,48.5));
#81198=CARTESIAN_POINT('',(120.43819912523,1.76391565799713,48.35));
#81199=CARTESIAN_POINT('',(120.43819912523,1.76391565799713,48.5));
#81200=CARTESIAN_POINT('Ctrl Pts',(120.43819912523,1.76391565799713,48.35));
#81201=CARTESIAN_POINT('Ctrl Pts',(120.565006814897,1.58458405733109,48.35));
#81202=CARTESIAN_POINT('Ctrl Pts',(120.751091323793,1.58458405733109,48.35));
#81203=CARTESIAN_POINT('Ctrl Pts',(120.311391435564,2.48499327898026,48.5));
#81204=CARTESIAN_POINT('Ctrl Pts',(120.311391435564,2.48499327898026,48.35));
#81205=CARTESIAN_POINT('Ctrl Pts',(120.311391435564,1.94324696063995,48.5));
#81206=CARTESIAN_POINT('Ctrl Pts',(120.311391435564,1.94324696063995,48.35));
#81207=CARTESIAN_POINT('Ctrl Pts',(120.43819912523,1.76391565799713,48.5));
#81208=CARTESIAN_POINT('Ctrl Pts',(120.43819912523,1.76391565799713,48.35));
#81209=CARTESIAN_POINT('',(120.311391435564,2.48499327898026,48.5));
#81210=CARTESIAN_POINT('Ctrl Pts',(120.311391435564,2.48499327898026,48.5));
#81211=CARTESIAN_POINT('Ctrl Pts',(120.311391435564,1.94324696063995,48.5));
#81212=CARTESIAN_POINT('Ctrl Pts',(120.43819912523,1.76391565799713,48.5));
#81213=CARTESIAN_POINT('',(120.311391435564,2.48499327898026,48.35));
#81214=CARTESIAN_POINT('',(120.311391435564,2.48499327898026,48.5));
#81215=CARTESIAN_POINT('Ctrl Pts',(120.311391435564,2.48499327898026,48.35));
#81216=CARTESIAN_POINT('Ctrl Pts',(120.311391435564,1.94324696063995,48.35));
#81217=CARTESIAN_POINT('Ctrl Pts',(120.43819912523,1.76391565799713,48.35));
#81218=CARTESIAN_POINT('Ctrl Pts',(120.450955115259,3.22783091664314,48.5));
#81219=CARTESIAN_POINT('Ctrl Pts',(120.450955115259,3.22783091664314,48.35));
#81220=CARTESIAN_POINT('Ctrl Pts',(120.311391435564,3.02673944830894,48.5));
#81221=CARTESIAN_POINT('Ctrl Pts',(120.311391435564,3.02673944830894,48.35));
#81222=CARTESIAN_POINT('Ctrl Pts',(120.311391435564,2.48499327898026,48.5));
#81223=CARTESIAN_POINT('Ctrl Pts',(120.311391435564,2.48499327898026,48.35));
#81224=CARTESIAN_POINT('Ctrl Pts',(120.450955115259,3.22783091664314,48.5));
#81225=CARTESIAN_POINT('Ctrl Pts',(120.311391435564,3.02673944830894,48.5));
#81226=CARTESIAN_POINT('Ctrl Pts',(120.311391435564,2.48499327898026,48.5));
#81227=CARTESIAN_POINT('Ctrl Pts',(120.450955115259,3.22783091664314,48.35));
#81228=CARTESIAN_POINT('Ctrl Pts',(120.311391435564,3.02673944830894,48.35));
#81229=CARTESIAN_POINT('Ctrl Pts',(120.311391435564,2.48499327898026,48.35));
#81230=CARTESIAN_POINT('Ctrl Pts',(120.751091323793,1.36248314380646,48.5));
#81231=CARTESIAN_POINT('Ctrl Pts',(120.751091323793,1.36248314380646,48.35));
#81232=CARTESIAN_POINT('Ctrl Pts',(120.432946763933,1.36248314380646,48.5));
#81233=CARTESIAN_POINT('Ctrl Pts',(120.432946763933,1.36248314380646,48.35));
#81234=CARTESIAN_POINT('Ctrl Pts',(120.251364193857,1.59058684110642,48.5));
#81235=CARTESIAN_POINT('Ctrl Pts',(120.251364193857,1.59058684110642,48.35));
#81236=CARTESIAN_POINT('',(120.751091323793,1.36248314380646,48.5));
#81237=CARTESIAN_POINT('',(120.251364193857,1.59058684110642,48.5));
#81238=CARTESIAN_POINT('Ctrl Pts',(120.751091323793,1.36248314380646,48.5));
#81239=CARTESIAN_POINT('Ctrl Pts',(120.432946763933,1.36248314380646,48.5));
#81240=CARTESIAN_POINT('Ctrl Pts',(120.251364193857,1.59058684110642,48.5));
#81241=CARTESIAN_POINT('',(120.751091323793,1.36248314380646,48.35));
#81242=CARTESIAN_POINT('',(120.751091323793,1.36248314380646,48.5));
#81243=CARTESIAN_POINT('',(120.251364193857,1.59058684110642,48.35));
#81244=CARTESIAN_POINT('Ctrl Pts',(120.751091323793,1.36248314380646,48.35));
#81245=CARTESIAN_POINT('Ctrl Pts',(120.432946763933,1.36248314380646,48.35));
#81246=CARTESIAN_POINT('Ctrl Pts',(120.251364193857,1.59058684110642,48.35));
#81247=CARTESIAN_POINT('',(120.251364193857,1.59058684110642,48.5));
#81248=CARTESIAN_POINT('Ctrl Pts',(121.151022993028,1.49229192733765,48.5));
#81249=CARTESIAN_POINT('Ctrl Pts',(121.151022993028,1.49229192733765,48.35));
#81250=CARTESIAN_POINT('Ctrl Pts',(120.992701135576,1.36248314380646,48.5));
#81251=CARTESIAN_POINT('Ctrl Pts',(120.992701135576,1.36248314380646,48.35));
#81252=CARTESIAN_POINT('Ctrl Pts',(120.751091323793,1.36248314380646,48.5));
#81253=CARTESIAN_POINT('Ctrl Pts',(120.751091323793,1.36248314380646,48.35));
#81254=CARTESIAN_POINT('',(121.151022993028,1.49229192733765,48.5));
#81255=CARTESIAN_POINT('Ctrl Pts',(121.151022993028,1.49229192733765,48.5));
#81256=CARTESIAN_POINT('Ctrl Pts',(120.992701135576,1.36248314380646,48.5));
#81257=CARTESIAN_POINT('Ctrl Pts',(120.751091323793,1.36248314380646,48.5));
#81258=CARTESIAN_POINT('',(121.151022993028,1.49229192733765,48.35));
#81259=CARTESIAN_POINT('',(121.151022993028,1.49229192733765,48.5));
#81260=CARTESIAN_POINT('Ctrl Pts',(121.151022993028,1.49229192733765,48.35));
#81261=CARTESIAN_POINT('Ctrl Pts',(120.992701135576,1.36248314380646,48.35));
#81262=CARTESIAN_POINT('Ctrl Pts',(120.751091323793,1.36248314380646,48.35));
#81263=CARTESIAN_POINT('Ctrl Pts',(121.388881288469,1.85995900630951,48.5));
#81264=CARTESIAN_POINT('Ctrl Pts',(121.388881288469,1.85995900630951,48.35));
#81265=CARTESIAN_POINT('Ctrl Pts',(121.309344850481,1.62210100889206,48.5));
#81266=CARTESIAN_POINT('Ctrl Pts',(121.309344850481,1.62210100889206,48.35));
#81267=CARTESIAN_POINT('Ctrl Pts',(121.151022993028,1.49229192733765,48.5));
#81268=CARTESIAN_POINT('Ctrl Pts',(121.151022993028,1.49229192733765,48.35));
#81269=CARTESIAN_POINT('',(121.388881288469,1.85995900630951,48.5));
#81270=CARTESIAN_POINT('Ctrl Pts',(121.388881288469,1.85995900630951,48.5));
#81271=CARTESIAN_POINT('Ctrl Pts',(121.309344850481,1.62210100889206,48.5));
#81272=CARTESIAN_POINT('Ctrl Pts',(121.151022993028,1.49229192733765,48.5));
#81273=CARTESIAN_POINT('',(121.388881288469,1.85995900630951,48.35));
#81274=CARTESIAN_POINT('',(121.388881288469,1.85995900630951,48.5));
#81275=CARTESIAN_POINT('Ctrl Pts',(121.388881288469,1.85995900630951,48.35));
#81276=CARTESIAN_POINT('Ctrl Pts',(121.309344850481,1.62210100889206,48.35));
#81277=CARTESIAN_POINT('Ctrl Pts',(121.151022993028,1.49229192733765,48.35));
#81278=CARTESIAN_POINT('Ctrl Pts',(121.468417130411,2.48499327898026,48.5));
#81279=CARTESIAN_POINT('Ctrl Pts',(121.468417130411,2.48499327898026,48.35));
#81280=CARTESIAN_POINT('Ctrl Pts',(121.468417130411,2.09781730175018,48.5));
#81281=CARTESIAN_POINT('Ctrl Pts',(121.468417130411,2.09781730175018,48.35));
#81282=CARTESIAN_POINT('Ctrl Pts',(121.388881288469,1.85995900630951,48.5));
#81283=CARTESIAN_POINT('Ctrl Pts',(121.388881288469,1.85995900630951,48.35));
#81284=CARTESIAN_POINT('',(121.468417130411,2.48499327898026,48.5));
#81285=CARTESIAN_POINT('Ctrl Pts',(121.468417130411,2.48499327898026,48.5));
#81286=CARTESIAN_POINT('Ctrl Pts',(121.468417130411,2.09781730175018,48.5));
#81287=CARTESIAN_POINT('Ctrl Pts',(121.388881288469,1.85995900630951,48.5));
#81288=CARTESIAN_POINT('',(121.468417130411,2.48499327898026,48.35));
#81289=CARTESIAN_POINT('',(121.468417130411,2.48499327898026,48.5));
#81290=CARTESIAN_POINT('Ctrl Pts',(121.468417130411,2.48499327898026,48.35));
#81291=CARTESIAN_POINT('Ctrl Pts',(121.468417130411,2.09781730175018,48.35));
#81292=CARTESIAN_POINT('Ctrl Pts',(121.388881288469,1.85995900630951,48.35));
#81293=CARTESIAN_POINT('Ctrl Pts',(121.418894611299,3.00497958064079,48.5));
#81294=CARTESIAN_POINT('Ctrl Pts',(121.418894611299,3.00497958064079,48.35));
#81295=CARTESIAN_POINT('Ctrl Pts',(121.468417130411,2.81214186549187,48.5));
#81296=CARTESIAN_POINT('Ctrl Pts',(121.468417130411,2.81214186549187,48.35));
#81297=CARTESIAN_POINT('Ctrl Pts',(121.468417130411,2.48499327898026,48.5));
#81298=CARTESIAN_POINT('Ctrl Pts',(121.468417130411,2.48499327898026,48.35));
#81299=CARTESIAN_POINT('',(121.418894611299,3.00497958064079,48.5));
#81300=CARTESIAN_POINT('Ctrl Pts',(121.418894611299,3.00497958064079,48.5));
#81301=CARTESIAN_POINT('Ctrl Pts',(121.468417130411,2.81214186549187,48.5));
#81302=CARTESIAN_POINT('Ctrl Pts',(121.468417130411,2.48499327898026,48.5));
#81303=CARTESIAN_POINT('',(121.418894611299,3.00497958064079,48.35));
#81304=CARTESIAN_POINT('',(121.418894611299,3.00497958064079,48.5));
#81305=CARTESIAN_POINT('Ctrl Pts',(121.418894611299,3.00497958064079,48.35));
#81306=CARTESIAN_POINT('Ctrl Pts',(121.468417130411,2.81214186549187,48.35));
#81307=CARTESIAN_POINT('Ctrl Pts',(121.468417130411,2.48499327898026,48.35));
#81308=CARTESIAN_POINT('Ctrl Pts',(121.282332621515,3.33212831616402,48.5));
#81309=CARTESIAN_POINT('Ctrl Pts',(121.282332621515,3.33212831616402,48.35));
#81310=CARTESIAN_POINT('Ctrl Pts',(121.369372092187,3.19781729578972,48.5));
#81311=CARTESIAN_POINT('Ctrl Pts',(121.369372092187,3.19781729578972,48.35));
#81312=CARTESIAN_POINT('Ctrl Pts',(121.418894611299,3.00497958064079,48.5));
#81313=CARTESIAN_POINT('Ctrl Pts',(121.418894611299,3.00497958064079,48.35));
#81314=CARTESIAN_POINT('',(121.282332621515,3.33212831616402,48.5));
#81315=CARTESIAN_POINT('Ctrl Pts',(121.282332621515,3.33212831616402,48.5));
#81316=CARTESIAN_POINT('Ctrl Pts',(121.369372092187,3.19781729578972,48.5));
#81317=CARTESIAN_POINT('Ctrl Pts',(121.418894611299,3.00497958064079,48.5));
#81318=CARTESIAN_POINT('',(121.282332621515,3.33212831616402,48.35));
#81319=CARTESIAN_POINT('',(121.282332621515,3.33212831616402,48.5));
#81320=CARTESIAN_POINT('Ctrl Pts',(121.282332621515,3.33212831616402,48.35));
#81321=CARTESIAN_POINT('Ctrl Pts',(121.369372092187,3.19781729578972,48.35));
#81322=CARTESIAN_POINT('Ctrl Pts',(121.418894611299,3.00497958064079,48.35));
#81323=CARTESIAN_POINT('Ctrl Pts',(121.061732850969,3.5377217233181,48.5));
#81324=CARTESIAN_POINT('Ctrl Pts',(121.061732850969,3.5377217233181,48.35));
#81325=CARTESIAN_POINT('Ctrl Pts',(121.195293150842,3.46643933653831,48.5));
#81326=CARTESIAN_POINT('Ctrl Pts',(121.195293150842,3.46643933653831,48.35));
#81327=CARTESIAN_POINT('Ctrl Pts',(121.282332621515,3.33212831616402,48.5));
#81328=CARTESIAN_POINT('Ctrl Pts',(121.282332621515,3.33212831616402,48.35));
#81329=CARTESIAN_POINT('',(121.061732850969,3.5377217233181,48.5));
#81330=CARTESIAN_POINT('Ctrl Pts',(121.061732850969,3.5377217233181,48.5));
#81331=CARTESIAN_POINT('Ctrl Pts',(121.195293150842,3.46643933653831,48.5));
#81332=CARTESIAN_POINT('Ctrl Pts',(121.282332621515,3.33212831616402,48.5));
#81333=CARTESIAN_POINT('',(121.061732850969,3.5377217233181,48.35));
#81334=CARTESIAN_POINT('',(121.061732850969,3.5377217233181,48.5));
#81335=CARTESIAN_POINT('Ctrl Pts',(121.061732850969,3.5377217233181,48.35));
#81336=CARTESIAN_POINT('Ctrl Pts',(121.195293150842,3.46643933653831,48.35));
#81337=CARTESIAN_POINT('Ctrl Pts',(121.282332621515,3.33212831616402,48.35));
#81338=CARTESIAN_POINT('Ctrl Pts',(120.751091323793,3.60900411009789,48.5));
#81339=CARTESIAN_POINT('Ctrl Pts',(120.751091323793,3.60900411009789,48.35));
#81340=CARTESIAN_POINT('Ctrl Pts',(120.928171955049,3.60900411009789,48.5));
#81341=CARTESIAN_POINT('Ctrl Pts',(120.928171955049,3.60900411009789,48.35));
#81342=CARTESIAN_POINT('Ctrl Pts',(121.061732850969,3.5377217233181,48.5));
#81343=CARTESIAN_POINT('Ctrl Pts',(121.061732850969,3.5377217233181,48.35));
#81344=CARTESIAN_POINT('',(120.751091323793,3.60900411009789,48.5));
#81345=CARTESIAN_POINT('Ctrl Pts',(120.751091323793,3.60900411009789,48.5));
#81346=CARTESIAN_POINT('Ctrl Pts',(120.928171955049,3.60900411009789,48.5));
#81347=CARTESIAN_POINT('Ctrl Pts',(121.061732850969,3.5377217233181,48.5));
#81348=CARTESIAN_POINT('',(120.751091323793,3.60900411009789,48.35));
#81349=CARTESIAN_POINT('',(120.751091323793,3.60900411009789,48.5));
#81350=CARTESIAN_POINT('Ctrl Pts',(120.751091323793,3.60900411009789,48.35));
#81351=CARTESIAN_POINT('Ctrl Pts',(120.928171955049,3.60900411009789,48.35));
#81352=CARTESIAN_POINT('Ctrl Pts',(121.061732850969,3.5377217233181,48.35));
#81353=CARTESIAN_POINT('Ctrl Pts',(120.352660499513,3.47994545102119,48.5));
#81354=CARTESIAN_POINT('Ctrl Pts',(120.352660499513,3.47994545102119,48.35));
#81355=CARTESIAN_POINT('Ctrl Pts',(120.510982356966,3.60900411009789,48.5));
#81356=CARTESIAN_POINT('Ctrl Pts',(120.510982356966,3.60900411009789,48.35));
#81357=CARTESIAN_POINT('Ctrl Pts',(120.751091323793,3.60900411009789,48.5));
#81358=CARTESIAN_POINT('Ctrl Pts',(120.751091323793,3.60900411009789,48.35));
#81359=CARTESIAN_POINT('',(120.352660499513,3.47994545102119,48.5));
#81360=CARTESIAN_POINT('Ctrl Pts',(120.352660499513,3.47994545102119,48.5));
#81361=CARTESIAN_POINT('Ctrl Pts',(120.510982356966,3.60900411009789,48.5));
#81362=CARTESIAN_POINT('Ctrl Pts',(120.751091323793,3.60900411009789,48.5));
#81363=CARTESIAN_POINT('',(120.352660499513,3.47994545102119,48.35));
#81364=CARTESIAN_POINT('',(120.352660499513,3.47994545102119,48.5));
#81365=CARTESIAN_POINT('Ctrl Pts',(120.352660499513,3.47994545102119,48.35));
#81366=CARTESIAN_POINT('Ctrl Pts',(120.510982356966,3.60900411009789,48.35));
#81367=CARTESIAN_POINT('Ctrl Pts',(120.751091323793,3.60900411009789,48.35));
#81368=CARTESIAN_POINT('Ctrl Pts',(120.114051781595,3.11302864551544,48.5));
#81369=CARTESIAN_POINT('Ctrl Pts',(120.114051781595,3.11302864551544,48.35));
#81370=CARTESIAN_POINT('Ctrl Pts',(120.194338344038,3.3508867919445,48.5));
#81371=CARTESIAN_POINT('Ctrl Pts',(120.194338344038,3.3508867919445,48.35));
#81372=CARTESIAN_POINT('Ctrl Pts',(120.352660499513,3.47994545102119,48.5));
#81373=CARTESIAN_POINT('Ctrl Pts',(120.352660499513,3.47994545102119,48.35));
#81374=CARTESIAN_POINT('',(120.114051781595,3.11302864551544,48.5));
#81375=CARTESIAN_POINT('Ctrl Pts',(120.114051781595,3.11302864551544,48.5));
#81376=CARTESIAN_POINT('Ctrl Pts',(120.194338344038,3.3508867919445,48.5));
#81377=CARTESIAN_POINT('Ctrl Pts',(120.352660499513,3.47994545102119,48.5));
#81378=CARTESIAN_POINT('',(120.114051781595,3.11302864551544,48.35));
#81379=CARTESIAN_POINT('',(120.114051781595,3.11302864551544,48.5));
#81380=CARTESIAN_POINT('Ctrl Pts',(120.114051781595,3.11302864551544,48.35));
#81381=CARTESIAN_POINT('Ctrl Pts',(120.194338344038,3.3508867919445,48.35));
#81382=CARTESIAN_POINT('Ctrl Pts',(120.352660499513,3.47994545102119,48.35));
#81383=CARTESIAN_POINT('Ctrl Pts',(120.033765517175,2.48499327898026,48.5));
#81384=CARTESIAN_POINT('Ctrl Pts',(120.033765517175,2.48499327898026,48.35));
#81385=CARTESIAN_POINT('Ctrl Pts',(120.033765517175,2.87517049908638,48.5));
#81386=CARTESIAN_POINT('Ctrl Pts',(120.033765517175,2.87517049908638,48.35));
#81387=CARTESIAN_POINT('Ctrl Pts',(120.114051781595,3.11302864551544,48.5));
#81388=CARTESIAN_POINT('Ctrl Pts',(120.114051781595,3.11302864551544,48.35));
#81389=CARTESIAN_POINT('',(120.033765517175,2.48499327898026,48.5));
#81390=CARTESIAN_POINT('Ctrl Pts',(120.033765517175,2.48499327898026,48.5));
#81391=CARTESIAN_POINT('Ctrl Pts',(120.033765517175,2.87517049908638,48.5));
#81392=CARTESIAN_POINT('Ctrl Pts',(120.114051781595,3.11302864551544,48.5));
#81393=CARTESIAN_POINT('',(120.033765517175,2.48499327898026,48.35));
#81394=CARTESIAN_POINT('',(120.033765517175,2.48499327898026,48.5));
#81395=CARTESIAN_POINT('Ctrl Pts',(120.033765517175,2.48499327898026,48.35));
#81396=CARTESIAN_POINT('Ctrl Pts',(120.033765517175,2.87517049908638,48.35));
#81397=CARTESIAN_POINT('Ctrl Pts',(120.114051781595,3.11302864551544,48.35));
#81398=CARTESIAN_POINT('Ctrl Pts',(120.251364193857,1.59058684110642,48.5));
#81399=CARTESIAN_POINT('Ctrl Pts',(120.251364193857,1.59058684110642,48.35));
#81400=CARTESIAN_POINT('Ctrl Pts',(120.033765517175,1.86521166563034,48.5));
#81401=CARTESIAN_POINT('Ctrl Pts',(120.033765517175,1.86521166563034,48.35));
#81402=CARTESIAN_POINT('Ctrl Pts',(120.033765517175,2.48499327898026,48.5));
#81403=CARTESIAN_POINT('Ctrl Pts',(120.033765517175,2.48499327898026,48.35));
#81404=CARTESIAN_POINT('Ctrl Pts',(120.251364193857,1.59058684110642,48.5));
#81405=CARTESIAN_POINT('Ctrl Pts',(120.033765517175,1.86521166563034,48.5));
#81406=CARTESIAN_POINT('Ctrl Pts',(120.033765517175,2.48499327898026,48.5));
#81407=CARTESIAN_POINT('Ctrl Pts',(120.251364193857,1.59058684110642,48.35));
#81408=CARTESIAN_POINT('Ctrl Pts',(120.033765517175,1.86521166563034,48.35));
#81409=CARTESIAN_POINT('Ctrl Pts',(120.033765517175,2.48499327898026,48.35));
#81410=CARTESIAN_POINT('Origin',(119.999999858439,2.48574362695217,48.35));
#81411=CARTESIAN_POINT('Origin',(119.167871855199,3.60900411009789,48.5));
#81412=CARTESIAN_POINT('',(119.167871855199,3.60900411009789,48.5));
#81413=CARTESIAN_POINT('',(119.341951094568,3.60900411009789,48.5));
#81414=CARTESIAN_POINT('',(59.5839359275997,3.60900411009789,48.5));
#81415=CARTESIAN_POINT('',(119.167871855199,3.60900411009789,48.35));
#81416=CARTESIAN_POINT('',(119.167871855199,3.60900411009789,48.5));
#81417=CARTESIAN_POINT('',(119.341951094568,3.60900411009789,48.35));
#81418=CARTESIAN_POINT('',(119.167871855199,3.60900411009789,48.35));
#81419=CARTESIAN_POINT('',(119.341951094568,3.60900411009789,48.5));
#81420=CARTESIAN_POINT('Ctrl Pts',(118.92776273936,3.31487053632736,48.5));
#81421=CARTESIAN_POINT('Ctrl Pts',(118.92776273936,3.31487053632736,48.35));
#81422=CARTESIAN_POINT('Ctrl Pts',(119.097339741886,3.46643933653831,48.5));
#81423=CARTESIAN_POINT('Ctrl Pts',(119.097339741886,3.46643933653831,48.35));
#81424=CARTESIAN_POINT('Ctrl Pts',(119.167871855199,3.60900411009789,48.5));
#81425=CARTESIAN_POINT('Ctrl Pts',(119.167871855199,3.60900411009789,48.35));
#81426=CARTESIAN_POINT('',(118.92776273936,3.31487053632736,48.5));
#81427=CARTESIAN_POINT('Ctrl Pts',(118.92776273936,3.31487053632736,48.5));
#81428=CARTESIAN_POINT('Ctrl Pts',(119.097339741886,3.46643933653831,48.5));
#81429=CARTESIAN_POINT('Ctrl Pts',(119.167871855199,3.60900411009789,48.5));
#81430=CARTESIAN_POINT('',(118.92776273936,3.31487053632736,48.35));
#81431=CARTESIAN_POINT('',(118.92776273936,3.31487053632736,48.5));
#81432=CARTESIAN_POINT('Ctrl Pts',(118.92776273936,3.31487053632736,48.35));
#81433=CARTESIAN_POINT('Ctrl Pts',(119.097339741886,3.46643933653831,48.35));
#81434=CARTESIAN_POINT('Ctrl Pts',(119.167871855199,3.60900411009789,48.35));
#81435=CARTESIAN_POINT('Ctrl Pts',(118.531582586467,3.05675321817398,48.5));
#81436=CARTESIAN_POINT('Ctrl Pts',(118.531582586467,3.05675321817398,48.35));
#81437=CARTESIAN_POINT('Ctrl Pts',(118.758185587823,3.1633015871048,48.5));
#81438=CARTESIAN_POINT('Ctrl Pts',(118.758185587823,3.1633015871048,48.35));
#81439=CARTESIAN_POINT('Ctrl Pts',(118.92776273936,3.31487053632736,48.5));
#81440=CARTESIAN_POINT('Ctrl Pts',(118.92776273936,3.31487053632736,48.35));
#81441=CARTESIAN_POINT('',(118.531582586467,3.05675321817398,48.5));
#81442=CARTESIAN_POINT('Ctrl Pts',(118.531582586467,3.05675321817398,48.5));
#81443=CARTESIAN_POINT('Ctrl Pts',(118.758185587823,3.1633015871048,48.5));
#81444=CARTESIAN_POINT('Ctrl Pts',(118.92776273936,3.31487053632736,48.5));
#81445=CARTESIAN_POINT('',(118.531582586467,3.05675321817398,48.35));
#81446=CARTESIAN_POINT('',(118.531582586467,3.05675321817398,48.5));
#81447=CARTESIAN_POINT('Ctrl Pts',(118.531582586467,3.05675321817398,48.35));
#81448=CARTESIAN_POINT('Ctrl Pts',(118.758185587823,3.1633015871048,48.35));
#81449=CARTESIAN_POINT('Ctrl Pts',(118.92776273936,3.31487053632736,48.35));
#81450=CARTESIAN_POINT('Origin',(118.531582586467,2.79563450813293,48.5));
#81451=CARTESIAN_POINT('',(118.531582586467,2.79563450813293,48.5));
#81452=CARTESIAN_POINT('',(118.531582586467,5.39781725406647,48.5));
#81453=CARTESIAN_POINT('',(118.531582586467,2.79563450813293,48.35));
#81454=CARTESIAN_POINT('',(118.531582586467,2.79563450813293,48.5));
#81455=CARTESIAN_POINT('',(118.531582586467,2.79563450813293,48.35));
#81456=CARTESIAN_POINT('Ctrl Pts',(118.81596186012,2.93519788980484,48.5));
#81457=CARTESIAN_POINT('Ctrl Pts',(118.81596186012,2.93519788980484,48.35));
#81458=CARTESIAN_POINT('Ctrl Pts',(118.657640002668,2.8421556353569,48.5));
#81459=CARTESIAN_POINT('Ctrl Pts',(118.657640002668,2.8421556353569,48.35));
#81460=CARTESIAN_POINT('Ctrl Pts',(118.531582586467,2.79563450813293,48.5));
#81461=CARTESIAN_POINT('Ctrl Pts',(118.531582586467,2.79563450813293,48.35));
#81462=CARTESIAN_POINT('',(118.81596186012,2.93519788980484,48.5));
#81463=CARTESIAN_POINT('Ctrl Pts',(118.81596186012,2.93519788980484,48.5));
#81464=CARTESIAN_POINT('Ctrl Pts',(118.657640002668,2.8421556353569,48.5));
#81465=CARTESIAN_POINT('Ctrl Pts',(118.531582586467,2.79563450813293,48.5));
#81466=CARTESIAN_POINT('',(118.81596186012,2.93519788980484,48.35));
#81467=CARTESIAN_POINT('',(118.81596186012,2.93519788980484,48.5));
#81468=CARTESIAN_POINT('Ctrl Pts',(118.81596186012,2.93519788980484,48.35));
#81469=CARTESIAN_POINT('Ctrl Pts',(118.657640002668,2.8421556353569,48.35));
#81470=CARTESIAN_POINT('Ctrl Pts',(118.531582586467,2.79563450813293,48.35));
#81471=CARTESIAN_POINT('Ctrl Pts',(119.071828208864,3.12128254771233,48.5));
#81472=CARTESIAN_POINT('Ctrl Pts',(119.071828208864,3.12128254771233,48.35));
#81473=CARTESIAN_POINT('Ctrl Pts',(118.974283866584,3.02824014425278,48.5));
#81474=CARTESIAN_POINT('Ctrl Pts',(118.974283866584,3.02824014425278,48.35));
#81475=CARTESIAN_POINT('Ctrl Pts',(118.81596186012,2.93519788980484,48.5));
#81476=CARTESIAN_POINT('Ctrl Pts',(118.81596186012,2.93519788980484,48.35));
#81477=CARTESIAN_POINT('',(119.071828208864,3.12128254771233,48.5));
#81478=CARTESIAN_POINT('Ctrl Pts',(119.071828208864,3.12128254771233,48.5));
#81479=CARTESIAN_POINT('Ctrl Pts',(118.974283866584,3.02824014425278,48.5));
#81480=CARTESIAN_POINT('Ctrl Pts',(118.81596186012,2.93519788980484,48.5));
#81481=CARTESIAN_POINT('',(119.071828208864,3.12128254771233,48.35));
#81482=CARTESIAN_POINT('',(119.071828208864,3.12128254771233,48.5));
#81483=CARTESIAN_POINT('Ctrl Pts',(119.071828208864,3.12128254771233,48.35));
#81484=CARTESIAN_POINT('Ctrl Pts',(118.974283866584,3.02824014425278,48.35));
#81485=CARTESIAN_POINT('Ctrl Pts',(118.81596186012,2.93519788980484,48.35));
#81486=CARTESIAN_POINT('Origin',(119.071828208864,1.40000009536743,48.5));
#81487=CARTESIAN_POINT('',(119.071828208864,1.40000009536743,48.5));
#81488=CARTESIAN_POINT('',(119.071828208864,4.70000004768372,48.5));
#81489=CARTESIAN_POINT('',(119.071828208864,1.40000009536743,48.35));
#81490=CARTESIAN_POINT('',(119.071828208864,1.40000009536743,48.5));
#81491=CARTESIAN_POINT('',(119.071828208864,1.40000009536743,48.35));
#81492=CARTESIAN_POINT('Origin',(119.341951094568,1.40000009536743,48.5));
#81493=CARTESIAN_POINT('',(119.341951094568,1.40000009536743,48.5));
#81494=CARTESIAN_POINT('',(59.6709755472839,1.40000009536743,48.5));
#81495=CARTESIAN_POINT('',(119.341951094568,1.40000009536743,48.35));
#81496=CARTESIAN_POINT('',(119.341951094568,1.40000009536743,48.5));
#81497=CARTESIAN_POINT('',(119.341951094568,1.40000009536743,48.35));
#81498=CARTESIAN_POINT('Origin',(119.341951094568,3.60900411009789,48.5));
#81499=CARTESIAN_POINT('',(119.341951094568,5.80450205504894,48.5));
#81500=CARTESIAN_POINT('',(119.341951094568,3.60900411009789,48.35));
#81501=CARTESIAN_POINT('Origin',(119.999999858439,2.48574362695217,48.35));
#81502=CARTESIAN_POINT('Origin',(0.,8.,48.5));
#81503=CARTESIAN_POINT('Ctrl Pts',(109.996998559684,3.38540250062943,48.5));
#81504=CARTESIAN_POINT('Ctrl Pts',(109.996998559684,3.38540250062943,48.35));
#81505=CARTESIAN_POINT('Ctrl Pts',(109.810914050788,3.38540250062943,48.5));
#81506=CARTESIAN_POINT('Ctrl Pts',(109.810914050788,3.38540250062943,48.35));
#81507=CARTESIAN_POINT('Ctrl Pts',(109.699863743037,3.22783091664314,48.5));
#81508=CARTESIAN_POINT('Ctrl Pts',(109.699863743037,3.22783091664314,48.35));
#81509=CARTESIAN_POINT('',(109.996998559684,3.38540250062943,48.5));
#81510=CARTESIAN_POINT('',(109.699863743037,3.22783091664314,48.5));
#81511=CARTESIAN_POINT('Ctrl Pts',(109.996998559684,3.38540250062943,48.5));
#81512=CARTESIAN_POINT('Ctrl Pts',(109.810914050788,3.38540250062943,48.5));
#81513=CARTESIAN_POINT('Ctrl Pts',(109.699863743037,3.22783091664314,48.5));
#81514=CARTESIAN_POINT('',(109.996998559684,3.38540250062943,48.35));
#81515=CARTESIAN_POINT('',(109.996998559684,3.38540250062943,48.5));
#81516=CARTESIAN_POINT('',(109.699863743037,3.22783091664314,48.35));
#81517=CARTESIAN_POINT('Ctrl Pts',(109.996998559684,3.38540250062943,48.35));
#81518=CARTESIAN_POINT('Ctrl Pts',(109.810914050788,3.38540250062943,48.35));
#81519=CARTESIAN_POINT('Ctrl Pts',(109.699863743037,3.22783091664314,48.35));
#81520=CARTESIAN_POINT('',(109.699863743037,3.22783091664314,48.5));
#81521=CARTESIAN_POINT('Ctrl Pts',(110.312892448157,3.2068213224411,48.5));
#81522=CARTESIAN_POINT('Ctrl Pts',(110.312892448157,3.2068213224411,48.35));
#81523=CARTESIAN_POINT('Ctrl Pts',(110.18608475849,3.38540250062943,48.5));
#81524=CARTESIAN_POINT('Ctrl Pts',(110.18608475849,3.38540250062943,48.35));
#81525=CARTESIAN_POINT('Ctrl Pts',(109.996998559684,3.38540250062943,48.5));
#81526=CARTESIAN_POINT('Ctrl Pts',(109.996998559684,3.38540250062943,48.35));
#81527=CARTESIAN_POINT('',(110.312892448157,3.2068213224411,48.5));
#81528=CARTESIAN_POINT('Ctrl Pts',(110.312892448157,3.2068213224411,48.5));
#81529=CARTESIAN_POINT('Ctrl Pts',(110.18608475849,3.38540250062943,48.5));
#81530=CARTESIAN_POINT('Ctrl Pts',(109.996998559684,3.38540250062943,48.5));
#81531=CARTESIAN_POINT('',(110.312892448157,3.2068213224411,48.35));
#81532=CARTESIAN_POINT('',(110.312892448157,3.2068213224411,48.5));
#81533=CARTESIAN_POINT('Ctrl Pts',(110.312892448157,3.2068213224411,48.35));
#81534=CARTESIAN_POINT('Ctrl Pts',(110.18608475849,3.38540250062943,48.35));
#81535=CARTESIAN_POINT('Ctrl Pts',(109.996998559684,3.38540250062943,48.35));
#81536=CARTESIAN_POINT('Ctrl Pts',(110.439700137824,2.48499327898026,48.5));
#81537=CARTESIAN_POINT('Ctrl Pts',(110.439700137824,2.48499327898026,48.35));
#81538=CARTESIAN_POINT('Ctrl Pts',(110.439700137824,3.02824014425278,48.5));
#81539=CARTESIAN_POINT('Ctrl Pts',(110.439700137824,3.02824014425278,48.35));
#81540=CARTESIAN_POINT('Ctrl Pts',(110.312892448157,3.2068213224411,48.5));
#81541=CARTESIAN_POINT('Ctrl Pts',(110.312892448157,3.2068213224411,48.35));
#81542=CARTESIAN_POINT('',(110.439700137824,2.48499327898026,48.5));
#81543=CARTESIAN_POINT('Ctrl Pts',(110.439700137824,2.48499327898026,48.5));
#81544=CARTESIAN_POINT('Ctrl Pts',(110.439700137824,3.02824014425278,48.5));
#81545=CARTESIAN_POINT('Ctrl Pts',(110.312892448157,3.2068213224411,48.5));
#81546=CARTESIAN_POINT('',(110.439700137824,2.48499327898026,48.35));
#81547=CARTESIAN_POINT('',(110.439700137824,2.48499327898026,48.5));
#81548=CARTESIAN_POINT('Ctrl Pts',(110.439700137824,2.48499327898026,48.35));
#81549=CARTESIAN_POINT('Ctrl Pts',(110.439700137824,3.02824014425278,48.35));
#81550=CARTESIAN_POINT('Ctrl Pts',(110.312892448157,3.2068213224411,48.35));
#81551=CARTESIAN_POINT('Ctrl Pts',(110.312892448157,1.76466578245163,48.5));
#81552=CARTESIAN_POINT('Ctrl Pts',(110.312892448157,1.76466578245163,48.35));
#81553=CARTESIAN_POINT('Ctrl Pts',(110.439700137824,1.9447478055954,48.5));
#81554=CARTESIAN_POINT('Ctrl Pts',(110.439700137824,1.9447478055954,48.35));
#81555=CARTESIAN_POINT('Ctrl Pts',(110.439700137824,2.48499327898026,48.5));
#81556=CARTESIAN_POINT('Ctrl Pts',(110.439700137824,2.48499327898026,48.35));
#81557=CARTESIAN_POINT('',(110.312892448157,1.76466578245163,48.5));
#81558=CARTESIAN_POINT('Ctrl Pts',(110.312892448157,1.76466578245163,48.5));
#81559=CARTESIAN_POINT('Ctrl Pts',(110.439700137824,1.9447478055954,48.5));
#81560=CARTESIAN_POINT('Ctrl Pts',(110.439700137824,2.48499327898026,48.5));
#81561=CARTESIAN_POINT('',(110.312892448157,1.76466578245163,48.35));
#81562=CARTESIAN_POINT('',(110.312892448157,1.76466578245163,48.5));
#81563=CARTESIAN_POINT('Ctrl Pts',(110.312892448157,1.76466578245163,48.35));
#81564=CARTESIAN_POINT('Ctrl Pts',(110.439700137824,1.9447478055954,48.35));
#81565=CARTESIAN_POINT('Ctrl Pts',(110.439700137824,2.48499327898026,48.35));
#81566=CARTESIAN_POINT('Ctrl Pts',(109.999999951571,1.58458405733109,48.5));
#81567=CARTESIAN_POINT('Ctrl Pts',(109.999999951571,1.58458405733109,48.35));
#81568=CARTESIAN_POINT('Ctrl Pts',(110.18608475849,1.58458405733109,48.5));
#81569=CARTESIAN_POINT('Ctrl Pts',(110.18608475849,1.58458405733109,48.35));
#81570=CARTESIAN_POINT('Ctrl Pts',(110.312892448157,1.76466578245163,48.5));
#81571=CARTESIAN_POINT('Ctrl Pts',(110.312892448157,1.76466578245163,48.35));
#81572=CARTESIAN_POINT('',(109.999999951571,1.58458405733109,48.5));
#81573=CARTESIAN_POINT('Ctrl Pts',(109.999999951571,1.58458405733109,48.5));
#81574=CARTESIAN_POINT('Ctrl Pts',(110.18608475849,1.58458405733109,48.5));
#81575=CARTESIAN_POINT('Ctrl Pts',(110.312892448157,1.76466578245163,48.5));
#81576=CARTESIAN_POINT('',(109.999999951571,1.58458405733109,48.35));
#81577=CARTESIAN_POINT('',(109.999999951571,1.58458405733109,48.5));
#81578=CARTESIAN_POINT('Ctrl Pts',(109.999999951571,1.58458405733109,48.35));
#81579=CARTESIAN_POINT('Ctrl Pts',(110.18608475849,1.58458405733109,48.35));
#81580=CARTESIAN_POINT('Ctrl Pts',(110.312892448157,1.76466578245163,48.35));
#81581=CARTESIAN_POINT('Ctrl Pts',(109.687107753009,1.76391565799713,48.5));
#81582=CARTESIAN_POINT('Ctrl Pts',(109.687107753009,1.76391565799713,48.35));
#81583=CARTESIAN_POINT('Ctrl Pts',(109.813915442675,1.58458405733109,48.5));
#81584=CARTESIAN_POINT('Ctrl Pts',(109.813915442675,1.58458405733109,48.35));
#81585=CARTESIAN_POINT('Ctrl Pts',(109.999999951571,1.58458405733109,48.5));
#81586=CARTESIAN_POINT('Ctrl Pts',(109.999999951571,1.58458405733109,48.35));
#81587=CARTESIAN_POINT('',(109.687107753009,1.76391565799713,48.5));
#81588=CARTESIAN_POINT('Ctrl Pts',(109.687107753009,1.76391565799713,48.5));
#81589=CARTESIAN_POINT('Ctrl Pts',(109.813915442675,1.58458405733109,48.5));
#81590=CARTESIAN_POINT('Ctrl Pts',(109.999999951571,1.58458405733109,48.5));
#81591=CARTESIAN_POINT('',(109.687107753009,1.76391565799713,48.35));
#81592=CARTESIAN_POINT('',(109.687107753009,1.76391565799713,48.5));
#81593=CARTESIAN_POINT('Ctrl Pts',(109.687107753009,1.76391565799713,48.35));
#81594=CARTESIAN_POINT('Ctrl Pts',(109.813915442675,1.58458405733109,48.35));
#81595=CARTESIAN_POINT('Ctrl Pts',(109.999999951571,1.58458405733109,48.35));
#81596=CARTESIAN_POINT('Ctrl Pts',(109.560300361365,2.48499327898026,48.5));
#81597=CARTESIAN_POINT('Ctrl Pts',(109.560300361365,2.48499327898026,48.35));
#81598=CARTESIAN_POINT('Ctrl Pts',(109.560300361365,1.94324696063995,48.5));
#81599=CARTESIAN_POINT('Ctrl Pts',(109.560300361365,1.94324696063995,48.35));
#81600=CARTESIAN_POINT('Ctrl Pts',(109.687107753009,1.76391565799713,48.5));
#81601=CARTESIAN_POINT('Ctrl Pts',(109.687107753009,1.76391565799713,48.35));
#81602=CARTESIAN_POINT('',(109.560300361365,2.48499327898026,48.5));
#81603=CARTESIAN_POINT('Ctrl Pts',(109.560300361365,2.48499327898026,48.5));
#81604=CARTESIAN_POINT('Ctrl Pts',(109.560300361365,1.94324696063995,48.5));
#81605=CARTESIAN_POINT('Ctrl Pts',(109.687107753009,1.76391565799713,48.5));
#81606=CARTESIAN_POINT('',(109.560300361365,2.48499327898026,48.35));
#81607=CARTESIAN_POINT('',(109.560300361365,2.48499327898026,48.5));
#81608=CARTESIAN_POINT('Ctrl Pts',(109.560300361365,2.48499327898026,48.35));
#81609=CARTESIAN_POINT('Ctrl Pts',(109.560300361365,1.94324696063995,48.35));
#81610=CARTESIAN_POINT('Ctrl Pts',(109.687107753009,1.76391565799713,48.35));
#81611=CARTESIAN_POINT('Ctrl Pts',(109.699863743037,3.22783091664314,48.5));
#81612=CARTESIAN_POINT('Ctrl Pts',(109.699863743037,3.22783091664314,48.35));
#81613=CARTESIAN_POINT('Ctrl Pts',(109.560300361365,3.02673944830894,48.5));
#81614=CARTESIAN_POINT('Ctrl Pts',(109.560300361365,3.02673944830894,48.35));
#81615=CARTESIAN_POINT('Ctrl Pts',(109.560300361365,2.48499327898026,48.5));
#81616=CARTESIAN_POINT('Ctrl Pts',(109.560300361365,2.48499327898026,48.35));
#81617=CARTESIAN_POINT('Ctrl Pts',(109.699863743037,3.22783091664314,48.5));
#81618=CARTESIAN_POINT('Ctrl Pts',(109.560300361365,3.02673944830894,48.5));
#81619=CARTESIAN_POINT('Ctrl Pts',(109.560300361365,2.48499327898026,48.5));
#81620=CARTESIAN_POINT('Ctrl Pts',(109.699863743037,3.22783091664314,48.35));
#81621=CARTESIAN_POINT('Ctrl Pts',(109.560300361365,3.02673944830894,48.35));
#81622=CARTESIAN_POINT('Ctrl Pts',(109.560300361365,2.48499327898026,48.35));
#81623=CARTESIAN_POINT('Ctrl Pts',(109.999999951571,1.36248314380646,48.5));
#81624=CARTESIAN_POINT('Ctrl Pts',(109.999999951571,1.36248314380646,48.35));
#81625=CARTESIAN_POINT('Ctrl Pts',(109.681855391711,1.36248314380646,48.5));
#81626=CARTESIAN_POINT('Ctrl Pts',(109.681855391711,1.36248314380646,48.35));
#81627=CARTESIAN_POINT('Ctrl Pts',(109.500272821635,1.59058684110642,48.5));
#81628=CARTESIAN_POINT('Ctrl Pts',(109.500272821635,1.59058684110642,48.35));
#81629=CARTESIAN_POINT('',(109.999999951571,1.36248314380646,48.5));
#81630=CARTESIAN_POINT('',(109.500272821635,1.59058684110642,48.5));
#81631=CARTESIAN_POINT('Ctrl Pts',(109.999999951571,1.36248314380646,48.5));
#81632=CARTESIAN_POINT('Ctrl Pts',(109.681855391711,1.36248314380646,48.5));
#81633=CARTESIAN_POINT('Ctrl Pts',(109.500272821635,1.59058684110642,48.5));
#81634=CARTESIAN_POINT('',(109.999999951571,1.36248314380646,48.35));
#81635=CARTESIAN_POINT('',(109.999999951571,1.36248314380646,48.5));
#81636=CARTESIAN_POINT('',(109.500272821635,1.59058684110642,48.35));
#81637=CARTESIAN_POINT('Ctrl Pts',(109.999999951571,1.36248314380646,48.35));
#81638=CARTESIAN_POINT('Ctrl Pts',(109.681855391711,1.36248314380646,48.35));
#81639=CARTESIAN_POINT('Ctrl Pts',(109.500272821635,1.59058684110642,48.35));
#81640=CARTESIAN_POINT('',(109.500272821635,1.59058684110642,48.5));
#81641=CARTESIAN_POINT('Ctrl Pts',(110.39993191883,1.49229192733765,48.5));
#81642=CARTESIAN_POINT('Ctrl Pts',(110.39993191883,1.49229192733765,48.35));
#81643=CARTESIAN_POINT('Ctrl Pts',(110.241609763354,1.36248314380646,48.5));
#81644=CARTESIAN_POINT('Ctrl Pts',(110.241609763354,1.36248314380646,48.35));
#81645=CARTESIAN_POINT('Ctrl Pts',(109.999999951571,1.36248314380646,48.5));
#81646=CARTESIAN_POINT('Ctrl Pts',(109.999999951571,1.36248314380646,48.35));
#81647=CARTESIAN_POINT('',(110.39993191883,1.49229192733765,48.5));
#81648=CARTESIAN_POINT('Ctrl Pts',(110.39993191883,1.49229192733765,48.5));
#81649=CARTESIAN_POINT('Ctrl Pts',(110.241609763354,1.36248314380646,48.5));
#81650=CARTESIAN_POINT('Ctrl Pts',(109.999999951571,1.36248314380646,48.5));
#81651=CARTESIAN_POINT('',(110.39993191883,1.49229192733765,48.35));
#81652=CARTESIAN_POINT('',(110.39993191883,1.49229192733765,48.5));
#81653=CARTESIAN_POINT('Ctrl Pts',(110.39993191883,1.49229192733765,48.35));
#81654=CARTESIAN_POINT('Ctrl Pts',(110.241609763354,1.36248314380646,48.35));
#81655=CARTESIAN_POINT('Ctrl Pts',(109.999999951571,1.36248314380646,48.35));
#81656=CARTESIAN_POINT('Ctrl Pts',(110.637789916247,1.85995900630951,48.5));
#81657=CARTESIAN_POINT('Ctrl Pts',(110.637789916247,1.85995900630951,48.35));
#81658=CARTESIAN_POINT('Ctrl Pts',(110.558253776282,1.62210100889206,48.5));
#81659=CARTESIAN_POINT('Ctrl Pts',(110.558253776282,1.62210100889206,48.35));
#81660=CARTESIAN_POINT('Ctrl Pts',(110.39993191883,1.49229192733765,48.5));
#81661=CARTESIAN_POINT('Ctrl Pts',(110.39993191883,1.49229192733765,48.35));
#81662=CARTESIAN_POINT('',(110.637789916247,1.85995900630951,48.5));
#81663=CARTESIAN_POINT('Ctrl Pts',(110.637789916247,1.85995900630951,48.5));
#81664=CARTESIAN_POINT('Ctrl Pts',(110.558253776282,1.62210100889206,48.5));
#81665=CARTESIAN_POINT('Ctrl Pts',(110.39993191883,1.49229192733765,48.5));
#81666=CARTESIAN_POINT('',(110.637789916247,1.85995900630951,48.35));
#81667=CARTESIAN_POINT('',(110.637789916247,1.85995900630951,48.5));
#81668=CARTESIAN_POINT('Ctrl Pts',(110.637789916247,1.85995900630951,48.35));
#81669=CARTESIAN_POINT('Ctrl Pts',(110.558253776282,1.62210100889206,48.35));
#81670=CARTESIAN_POINT('Ctrl Pts',(110.39993191883,1.49229192733765,48.35));
#81671=CARTESIAN_POINT('Ctrl Pts',(110.717326056212,2.48499327898026,48.5));
#81672=CARTESIAN_POINT('Ctrl Pts',(110.717326056212,2.48499327898026,48.35));
#81673=CARTESIAN_POINT('Ctrl Pts',(110.717326056212,2.09781730175018,48.5));
#81674=CARTESIAN_POINT('Ctrl Pts',(110.717326056212,2.09781730175018,48.35));
#81675=CARTESIAN_POINT('Ctrl Pts',(110.637789916247,1.85995900630951,48.5));
#81676=CARTESIAN_POINT('Ctrl Pts',(110.637789916247,1.85995900630951,48.35));
#81677=CARTESIAN_POINT('',(110.717326056212,2.48499327898026,48.5));
#81678=CARTESIAN_POINT('Ctrl Pts',(110.717326056212,2.48499327898026,48.5));
#81679=CARTESIAN_POINT('Ctrl Pts',(110.717326056212,2.09781730175018,48.5));
#81680=CARTESIAN_POINT('Ctrl Pts',(110.637789916247,1.85995900630951,48.5));
#81681=CARTESIAN_POINT('',(110.717326056212,2.48499327898026,48.35));
#81682=CARTESIAN_POINT('',(110.717326056212,2.48499327898026,48.5));
#81683=CARTESIAN_POINT('Ctrl Pts',(110.717326056212,2.48499327898026,48.35));
#81684=CARTESIAN_POINT('Ctrl Pts',(110.717326056212,2.09781730175018,48.35));
#81685=CARTESIAN_POINT('Ctrl Pts',(110.637789916247,1.85995900630951,48.35));
#81686=CARTESIAN_POINT('Ctrl Pts',(110.667803537101,3.00497958064079,48.5));
#81687=CARTESIAN_POINT('Ctrl Pts',(110.667803537101,3.00497958064079,48.35));
#81688=CARTESIAN_POINT('Ctrl Pts',(110.717326056212,2.81214186549187,48.5));
#81689=CARTESIAN_POINT('Ctrl Pts',(110.717326056212,2.81214186549187,48.35));
#81690=CARTESIAN_POINT('Ctrl Pts',(110.717326056212,2.48499327898026,48.5));
#81691=CARTESIAN_POINT('Ctrl Pts',(110.717326056212,2.48499327898026,48.35));
#81692=CARTESIAN_POINT('',(110.667803537101,3.00497958064079,48.5));
#81693=CARTESIAN_POINT('Ctrl Pts',(110.667803537101,3.00497958064079,48.5));
#81694=CARTESIAN_POINT('Ctrl Pts',(110.717326056212,2.81214186549187,48.5));
#81695=CARTESIAN_POINT('Ctrl Pts',(110.717326056212,2.48499327898026,48.5));
#81696=CARTESIAN_POINT('',(110.667803537101,3.00497958064079,48.35));
#81697=CARTESIAN_POINT('',(110.667803537101,3.00497958064079,48.5));
#81698=CARTESIAN_POINT('Ctrl Pts',(110.667803537101,3.00497958064079,48.35));
#81699=CARTESIAN_POINT('Ctrl Pts',(110.717326056212,2.81214186549187,48.35));
#81700=CARTESIAN_POINT('Ctrl Pts',(110.717326056212,2.48499327898026,48.35));
#81701=CARTESIAN_POINT('Ctrl Pts',(110.531241547316,3.33212831616402,48.5));
#81702=CARTESIAN_POINT('Ctrl Pts',(110.531241547316,3.33212831616402,48.35));
#81703=CARTESIAN_POINT('Ctrl Pts',(110.618281017989,3.19781729578972,48.5));
#81704=CARTESIAN_POINT('Ctrl Pts',(110.618281017989,3.19781729578972,48.35));
#81705=CARTESIAN_POINT('Ctrl Pts',(110.667803537101,3.00497958064079,48.5));
#81706=CARTESIAN_POINT('Ctrl Pts',(110.667803537101,3.00497958064079,48.35));
#81707=CARTESIAN_POINT('',(110.531241547316,3.33212831616402,48.5));
#81708=CARTESIAN_POINT('Ctrl Pts',(110.531241547316,3.33212831616402,48.5));
#81709=CARTESIAN_POINT('Ctrl Pts',(110.618281017989,3.19781729578972,48.5));
#81710=CARTESIAN_POINT('Ctrl Pts',(110.667803537101,3.00497958064079,48.5));
#81711=CARTESIAN_POINT('',(110.531241547316,3.33212831616402,48.35));
#81712=CARTESIAN_POINT('',(110.531241547316,3.33212831616402,48.5));
#81713=CARTESIAN_POINT('Ctrl Pts',(110.531241547316,3.33212831616402,48.35));
#81714=CARTESIAN_POINT('Ctrl Pts',(110.618281017989,3.19781729578972,48.35));
#81715=CARTESIAN_POINT('Ctrl Pts',(110.667803537101,3.00497958064079,48.35));
#81716=CARTESIAN_POINT('Ctrl Pts',(110.310641180724,3.5377217233181,48.5));
#81717=CARTESIAN_POINT('Ctrl Pts',(110.310641180724,3.5377217233181,48.35));
#81718=CARTESIAN_POINT('Ctrl Pts',(110.444202076644,3.46643933653831,48.5));
#81719=CARTESIAN_POINT('Ctrl Pts',(110.444202076644,3.46643933653831,48.35));
#81720=CARTESIAN_POINT('Ctrl Pts',(110.531241547316,3.33212831616402,48.5));
#81721=CARTESIAN_POINT('Ctrl Pts',(110.531241547316,3.33212831616402,48.35));
#81722=CARTESIAN_POINT('',(110.310641180724,3.5377217233181,48.5));
#81723=CARTESIAN_POINT('Ctrl Pts',(110.310641180724,3.5377217233181,48.5));
#81724=CARTESIAN_POINT('Ctrl Pts',(110.444202076644,3.46643933653831,48.5));
#81725=CARTESIAN_POINT('Ctrl Pts',(110.531241547316,3.33212831616402,48.5));
#81726=CARTESIAN_POINT('',(110.310641180724,3.5377217233181,48.35));
#81727=CARTESIAN_POINT('',(110.310641180724,3.5377217233181,48.5));
#81728=CARTESIAN_POINT('Ctrl Pts',(110.310641180724,3.5377217233181,48.35));
#81729=CARTESIAN_POINT('Ctrl Pts',(110.444202076644,3.46643933653831,48.35));
#81730=CARTESIAN_POINT('Ctrl Pts',(110.531241547316,3.33212831616402,48.35));
#81731=CARTESIAN_POINT('Ctrl Pts',(109.999999951571,3.60900411009789,48.5));
#81732=CARTESIAN_POINT('Ctrl Pts',(109.999999951571,3.60900411009789,48.35));
#81733=CARTESIAN_POINT('Ctrl Pts',(110.177080582827,3.60900411009789,48.5));
#81734=CARTESIAN_POINT('Ctrl Pts',(110.177080582827,3.60900411009789,48.35));
#81735=CARTESIAN_POINT('Ctrl Pts',(110.310641180724,3.5377217233181,48.5));
#81736=CARTESIAN_POINT('Ctrl Pts',(110.310641180724,3.5377217233181,48.35));
#81737=CARTESIAN_POINT('',(109.999999951571,3.60900411009789,48.5));
#81738=CARTESIAN_POINT('Ctrl Pts',(109.999999951571,3.60900411009789,48.5));
#81739=CARTESIAN_POINT('Ctrl Pts',(110.177080582827,3.60900411009789,48.5));
#81740=CARTESIAN_POINT('Ctrl Pts',(110.310641180724,3.5377217233181,48.5));
#81741=CARTESIAN_POINT('',(109.999999951571,3.60900411009789,48.35));
#81742=CARTESIAN_POINT('',(109.999999951571,3.60900411009789,48.5));
#81743=CARTESIAN_POINT('Ctrl Pts',(109.999999951571,3.60900411009789,48.35));
#81744=CARTESIAN_POINT('Ctrl Pts',(110.177080582827,3.60900411009789,48.35));
#81745=CARTESIAN_POINT('Ctrl Pts',(110.310641180724,3.5377217233181,48.35));
#81746=CARTESIAN_POINT('Ctrl Pts',(109.601568829268,3.47994545102119,48.5));
#81747=CARTESIAN_POINT('Ctrl Pts',(109.601568829268,3.47994545102119,48.35));
#81748=CARTESIAN_POINT('Ctrl Pts',(109.759890984744,3.60900411009789,48.5));
#81749=CARTESIAN_POINT('Ctrl Pts',(109.759890984744,3.60900411009789,48.35));
#81750=CARTESIAN_POINT('Ctrl Pts',(109.999999951571,3.60900411009789,48.5));
#81751=CARTESIAN_POINT('Ctrl Pts',(109.999999951571,3.60900411009789,48.35));
#81752=CARTESIAN_POINT('',(109.601568829268,3.47994545102119,48.5));
#81753=CARTESIAN_POINT('Ctrl Pts',(109.601568829268,3.47994545102119,48.5));
#81754=CARTESIAN_POINT('Ctrl Pts',(109.759890984744,3.60900411009789,48.5));
#81755=CARTESIAN_POINT('Ctrl Pts',(109.999999951571,3.60900411009789,48.5));
#81756=CARTESIAN_POINT('',(109.601568829268,3.47994545102119,48.35));
#81757=CARTESIAN_POINT('',(109.601568829268,3.47994545102119,48.5));
#81758=CARTESIAN_POINT('Ctrl Pts',(109.601568829268,3.47994545102119,48.35));
#81759=CARTESIAN_POINT('Ctrl Pts',(109.759890984744,3.60900411009789,48.35));
#81760=CARTESIAN_POINT('Ctrl Pts',(109.999999951571,3.60900411009789,48.35));
#81761=CARTESIAN_POINT('Ctrl Pts',(109.362960558385,3.11302864551544,48.5));
#81762=CARTESIAN_POINT('Ctrl Pts',(109.362960558385,3.11302864551544,48.35));
#81763=CARTESIAN_POINT('Ctrl Pts',(109.443246971816,3.3508867919445,48.5));
#81764=CARTESIAN_POINT('Ctrl Pts',(109.443246971816,3.3508867919445,48.35));
#81765=CARTESIAN_POINT('Ctrl Pts',(109.601568829268,3.47994545102119,48.5));
#81766=CARTESIAN_POINT('Ctrl Pts',(109.601568829268,3.47994545102119,48.35));
#81767=CARTESIAN_POINT('',(109.362960558385,3.11302864551544,48.5));
#81768=CARTESIAN_POINT('Ctrl Pts',(109.362960558385,3.11302864551544,48.5));
#81769=CARTESIAN_POINT('Ctrl Pts',(109.443246971816,3.3508867919445,48.5));
#81770=CARTESIAN_POINT('Ctrl Pts',(109.601568829268,3.47994545102119,48.5));
#81771=CARTESIAN_POINT('',(109.362960558385,3.11302864551544,48.35));
#81772=CARTESIAN_POINT('',(109.362960558385,3.11302864551544,48.5));
#81773=CARTESIAN_POINT('Ctrl Pts',(109.362960558385,3.11302864551544,48.35));
#81774=CARTESIAN_POINT('Ctrl Pts',(109.443246971816,3.3508867919445,48.35));
#81775=CARTESIAN_POINT('Ctrl Pts',(109.601568829268,3.47994545102119,48.35));
#81776=CARTESIAN_POINT('Ctrl Pts',(109.282673995942,2.48499327898026,48.5));
#81777=CARTESIAN_POINT('Ctrl Pts',(109.282673995942,2.48499327898026,48.35));
#81778=CARTESIAN_POINT('Ctrl Pts',(109.282673995942,2.87517049908638,48.5));
#81779=CARTESIAN_POINT('Ctrl Pts',(109.282673995942,2.87517049908638,48.35));
#81780=CARTESIAN_POINT('Ctrl Pts',(109.362960558385,3.11302864551544,48.5));
#81781=CARTESIAN_POINT('Ctrl Pts',(109.362960558385,3.11302864551544,48.35));
#81782=CARTESIAN_POINT('',(109.282673995942,2.48499327898026,48.5));
#81783=CARTESIAN_POINT('Ctrl Pts',(109.282673995942,2.48499327898026,48.5));
#81784=CARTESIAN_POINT('Ctrl Pts',(109.282673995942,2.87517049908638,48.5));
#81785=CARTESIAN_POINT('Ctrl Pts',(109.362960558385,3.11302864551544,48.5));
#81786=CARTESIAN_POINT('',(109.282673995942,2.48499327898026,48.35));
#81787=CARTESIAN_POINT('',(109.282673995942,2.48499327898026,48.5));
#81788=CARTESIAN_POINT('Ctrl Pts',(109.282673995942,2.48499327898026,48.35));
#81789=CARTESIAN_POINT('Ctrl Pts',(109.282673995942,2.87517049908638,48.35));
#81790=CARTESIAN_POINT('Ctrl Pts',(109.362960558385,3.11302864551544,48.35));
#81791=CARTESIAN_POINT('Ctrl Pts',(109.500272821635,1.59058684110642,48.5));
#81792=CARTESIAN_POINT('Ctrl Pts',(109.500272821635,1.59058684110642,48.35));
#81793=CARTESIAN_POINT('Ctrl Pts',(109.282673995942,1.86521166563034,48.5));
#81794=CARTESIAN_POINT('Ctrl Pts',(109.282673995942,1.86521166563034,48.35));
#81795=CARTESIAN_POINT('Ctrl Pts',(109.282673995942,2.48499327898026,48.5));
#81796=CARTESIAN_POINT('Ctrl Pts',(109.282673995942,2.48499327898026,48.35));
#81797=CARTESIAN_POINT('Ctrl Pts',(109.500272821635,1.59058684110642,48.5));
#81798=CARTESIAN_POINT('Ctrl Pts',(109.282673995942,1.86521166563034,48.5));
#81799=CARTESIAN_POINT('Ctrl Pts',(109.282673995942,2.48499327898026,48.5));
#81800=CARTESIAN_POINT('Ctrl Pts',(109.500272821635,1.59058684110642,48.35));
#81801=CARTESIAN_POINT('Ctrl Pts',(109.282673995942,1.86521166563034,48.35));
#81802=CARTESIAN_POINT('Ctrl Pts',(109.282673995942,2.48499327898026,48.35));
#81803=CARTESIAN_POINT('Origin',(110.000000026077,2.48574362695217,48.35));
#81804=CARTESIAN_POINT('Origin',(0.,8.,48.5));
#81805=CARTESIAN_POINT('Ctrl Pts',(100.748090229928,3.38540250062943,48.5));
#81806=CARTESIAN_POINT('Ctrl Pts',(100.748090229928,3.38540250062943,48.35));
#81807=CARTESIAN_POINT('Ctrl Pts',(100.562005423009,3.38540250062943,48.5));
#81808=CARTESIAN_POINT('Ctrl Pts',(100.562005423009,3.38540250062943,48.35));
#81809=CARTESIAN_POINT('Ctrl Pts',(100.450955115259,3.22783091664314,48.5));
#81810=CARTESIAN_POINT('Ctrl Pts',(100.450955115259,3.22783091664314,48.35));
#81811=CARTESIAN_POINT('',(100.748090229928,3.38540250062943,48.5));
#81812=CARTESIAN_POINT('',(100.450955115259,3.22783091664314,48.5));
#81813=CARTESIAN_POINT('Ctrl Pts',(100.748090229928,3.38540250062943,48.5));
#81814=CARTESIAN_POINT('Ctrl Pts',(100.562005423009,3.38540250062943,48.5));
#81815=CARTESIAN_POINT('Ctrl Pts',(100.450955115259,3.22783091664314,48.5));
#81816=CARTESIAN_POINT('',(100.748090229928,3.38540250062943,48.35));
#81817=CARTESIAN_POINT('',(100.748090229928,3.38540250062943,48.5));
#81818=CARTESIAN_POINT('',(100.450955115259,3.22783091664314,48.35));
#81819=CARTESIAN_POINT('Ctrl Pts',(100.748090229928,3.38540250062943,48.35));
#81820=CARTESIAN_POINT('Ctrl Pts',(100.562005423009,3.38540250062943,48.35));
#81821=CARTESIAN_POINT('Ctrl Pts',(100.450955115259,3.22783091664314,48.35));
#81822=CARTESIAN_POINT('',(100.450955115259,3.22783091664314,48.5));
#81823=CARTESIAN_POINT('Ctrl Pts',(101.063983522356,3.2068213224411,48.5));
#81824=CARTESIAN_POINT('Ctrl Pts',(101.063983522356,3.2068213224411,48.35));
#81825=CARTESIAN_POINT('Ctrl Pts',(100.937175832689,3.38540250062943,48.5));
#81826=CARTESIAN_POINT('Ctrl Pts',(100.937175832689,3.38540250062943,48.35));
#81827=CARTESIAN_POINT('Ctrl Pts',(100.748090229928,3.38540250062943,48.5));
#81828=CARTESIAN_POINT('Ctrl Pts',(100.748090229928,3.38540250062943,48.35));
#81829=CARTESIAN_POINT('',(101.063983522356,3.2068213224411,48.5));
#81830=CARTESIAN_POINT('Ctrl Pts',(101.063983522356,3.2068213224411,48.5));
#81831=CARTESIAN_POINT('Ctrl Pts',(100.937175832689,3.38540250062943,48.5));
#81832=CARTESIAN_POINT('Ctrl Pts',(100.748090229928,3.38540250062943,48.5));
#81833=CARTESIAN_POINT('',(101.063983522356,3.2068213224411,48.35));
#81834=CARTESIAN_POINT('',(101.063983522356,3.2068213224411,48.5));
#81835=CARTESIAN_POINT('Ctrl Pts',(101.063983522356,3.2068213224411,48.35));
#81836=CARTESIAN_POINT('Ctrl Pts',(100.937175832689,3.38540250062943,48.35));
#81837=CARTESIAN_POINT('Ctrl Pts',(100.748090229928,3.38540250062943,48.35));
#81838=CARTESIAN_POINT('Ctrl Pts',(101.190791212022,2.48499327898026,48.5));
#81839=CARTESIAN_POINT('Ctrl Pts',(101.190791212022,2.48499327898026,48.35));
#81840=CARTESIAN_POINT('Ctrl Pts',(101.190791212022,3.02824014425278,48.5));
#81841=CARTESIAN_POINT('Ctrl Pts',(101.190791212022,3.02824014425278,48.35));
#81842=CARTESIAN_POINT('Ctrl Pts',(101.063983522356,3.2068213224411,48.5));
#81843=CARTESIAN_POINT('Ctrl Pts',(101.063983522356,3.2068213224411,48.35));
#81844=CARTESIAN_POINT('',(101.190791212022,2.48499327898026,48.5));
#81845=CARTESIAN_POINT('Ctrl Pts',(101.190791212022,2.48499327898026,48.5));
#81846=CARTESIAN_POINT('Ctrl Pts',(101.190791212022,3.02824014425278,48.5));
#81847=CARTESIAN_POINT('Ctrl Pts',(101.063983522356,3.2068213224411,48.5));
#81848=CARTESIAN_POINT('',(101.190791212022,2.48499327898026,48.35));
#81849=CARTESIAN_POINT('',(101.190791212022,2.48499327898026,48.5));
#81850=CARTESIAN_POINT('Ctrl Pts',(101.190791212022,2.48499327898026,48.35));
#81851=CARTESIAN_POINT('Ctrl Pts',(101.190791212022,3.02824014425278,48.35));
#81852=CARTESIAN_POINT('Ctrl Pts',(101.063983522356,3.2068213224411,48.35));
#81853=CARTESIAN_POINT('Ctrl Pts',(101.063983522356,1.76466578245163,48.5));
#81854=CARTESIAN_POINT('Ctrl Pts',(101.063983522356,1.76466578245163,48.35));
#81855=CARTESIAN_POINT('Ctrl Pts',(101.190791212022,1.9447478055954,48.5));
#81856=CARTESIAN_POINT('Ctrl Pts',(101.190791212022,1.9447478055954,48.35));
#81857=CARTESIAN_POINT('Ctrl Pts',(101.190791212022,2.48499327898026,48.5));
#81858=CARTESIAN_POINT('Ctrl Pts',(101.190791212022,2.48499327898026,48.35));
#81859=CARTESIAN_POINT('',(101.063983522356,1.76466578245163,48.5));
#81860=CARTESIAN_POINT('Ctrl Pts',(101.063983522356,1.76466578245163,48.5));
#81861=CARTESIAN_POINT('Ctrl Pts',(101.190791212022,1.9447478055954,48.5));
#81862=CARTESIAN_POINT('Ctrl Pts',(101.190791212022,2.48499327898026,48.5));
#81863=CARTESIAN_POINT('',(101.063983522356,1.76466578245163,48.35));
#81864=CARTESIAN_POINT('',(101.063983522356,1.76466578245163,48.5));
#81865=CARTESIAN_POINT('Ctrl Pts',(101.063983522356,1.76466578245163,48.35));
#81866=CARTESIAN_POINT('Ctrl Pts',(101.190791212022,1.9447478055954,48.35));
#81867=CARTESIAN_POINT('Ctrl Pts',(101.190791212022,2.48499327898026,48.35));
#81868=CARTESIAN_POINT('Ctrl Pts',(100.751091323793,1.58458405733109,48.5));
#81869=CARTESIAN_POINT('Ctrl Pts',(100.751091323793,1.58458405733109,48.35));
#81870=CARTESIAN_POINT('Ctrl Pts',(100.937175832689,1.58458405733109,48.5));
#81871=CARTESIAN_POINT('Ctrl Pts',(100.937175832689,1.58458405733109,48.35));
#81872=CARTESIAN_POINT('Ctrl Pts',(101.063983522356,1.76466578245163,48.5));
#81873=CARTESIAN_POINT('Ctrl Pts',(101.063983522356,1.76466578245163,48.35));
#81874=CARTESIAN_POINT('',(100.751091323793,1.58458405733109,48.5));
#81875=CARTESIAN_POINT('Ctrl Pts',(100.751091323793,1.58458405733109,48.5));
#81876=CARTESIAN_POINT('Ctrl Pts',(100.937175832689,1.58458405733109,48.5));
#81877=CARTESIAN_POINT('Ctrl Pts',(101.063983522356,1.76466578245163,48.5));
#81878=CARTESIAN_POINT('',(100.751091323793,1.58458405733109,48.35));
#81879=CARTESIAN_POINT('',(100.751091323793,1.58458405733109,48.5));
#81880=CARTESIAN_POINT('Ctrl Pts',(100.751091323793,1.58458405733109,48.35));
#81881=CARTESIAN_POINT('Ctrl Pts',(100.937175832689,1.58458405733109,48.35));
#81882=CARTESIAN_POINT('Ctrl Pts',(101.063983522356,1.76466578245163,48.35));
#81883=CARTESIAN_POINT('Ctrl Pts',(100.43819912523,1.76391565799713,48.5));
#81884=CARTESIAN_POINT('Ctrl Pts',(100.43819912523,1.76391565799713,48.35));
#81885=CARTESIAN_POINT('Ctrl Pts',(100.565006814897,1.58458405733109,48.5));
#81886=CARTESIAN_POINT('Ctrl Pts',(100.565006814897,1.58458405733109,48.35));
#81887=CARTESIAN_POINT('Ctrl Pts',(100.751091323793,1.58458405733109,48.5));
#81888=CARTESIAN_POINT('Ctrl Pts',(100.751091323793,1.58458405733109,48.35));
#81889=CARTESIAN_POINT('',(100.43819912523,1.76391565799713,48.5));
#81890=CARTESIAN_POINT('Ctrl Pts',(100.43819912523,1.76391565799713,48.5));
#81891=CARTESIAN_POINT('Ctrl Pts',(100.565006814897,1.58458405733109,48.5));
#81892=CARTESIAN_POINT('Ctrl Pts',(100.751091323793,1.58458405733109,48.5));
#81893=CARTESIAN_POINT('',(100.43819912523,1.76391565799713,48.35));
#81894=CARTESIAN_POINT('',(100.43819912523,1.76391565799713,48.5));
#81895=CARTESIAN_POINT('Ctrl Pts',(100.43819912523,1.76391565799713,48.35));
#81896=CARTESIAN_POINT('Ctrl Pts',(100.565006814897,1.58458405733109,48.35));
#81897=CARTESIAN_POINT('Ctrl Pts',(100.751091323793,1.58458405733109,48.35));
#81898=CARTESIAN_POINT('Ctrl Pts',(100.311391435564,2.48499327898026,48.5));
#81899=CARTESIAN_POINT('Ctrl Pts',(100.311391435564,2.48499327898026,48.35));
#81900=CARTESIAN_POINT('Ctrl Pts',(100.311391435564,1.94324696063995,48.5));
#81901=CARTESIAN_POINT('Ctrl Pts',(100.311391435564,1.94324696063995,48.35));
#81902=CARTESIAN_POINT('Ctrl Pts',(100.43819912523,1.76391565799713,48.5));
#81903=CARTESIAN_POINT('Ctrl Pts',(100.43819912523,1.76391565799713,48.35));
#81904=CARTESIAN_POINT('',(100.311391435564,2.48499327898026,48.5));
#81905=CARTESIAN_POINT('Ctrl Pts',(100.311391435564,2.48499327898026,48.5));
#81906=CARTESIAN_POINT('Ctrl Pts',(100.311391435564,1.94324696063995,48.5));
#81907=CARTESIAN_POINT('Ctrl Pts',(100.43819912523,1.76391565799713,48.5));
#81908=CARTESIAN_POINT('',(100.311391435564,2.48499327898026,48.35));
#81909=CARTESIAN_POINT('',(100.311391435564,2.48499327898026,48.5));
#81910=CARTESIAN_POINT('Ctrl Pts',(100.311391435564,2.48499327898026,48.35));
#81911=CARTESIAN_POINT('Ctrl Pts',(100.311391435564,1.94324696063995,48.35));
#81912=CARTESIAN_POINT('Ctrl Pts',(100.43819912523,1.76391565799713,48.35));
#81913=CARTESIAN_POINT('Ctrl Pts',(100.450955115259,3.22783091664314,48.5));
#81914=CARTESIAN_POINT('Ctrl Pts',(100.450955115259,3.22783091664314,48.35));
#81915=CARTESIAN_POINT('Ctrl Pts',(100.311391435564,3.02673944830894,48.5));
#81916=CARTESIAN_POINT('Ctrl Pts',(100.311391435564,3.02673944830894,48.35));
#81917=CARTESIAN_POINT('Ctrl Pts',(100.311391435564,2.48499327898026,48.5));
#81918=CARTESIAN_POINT('Ctrl Pts',(100.311391435564,2.48499327898026,48.35));
#81919=CARTESIAN_POINT('Ctrl Pts',(100.450955115259,3.22783091664314,48.5));
#81920=CARTESIAN_POINT('Ctrl Pts',(100.311391435564,3.02673944830894,48.5));
#81921=CARTESIAN_POINT('Ctrl Pts',(100.311391435564,2.48499327898026,48.5));
#81922=CARTESIAN_POINT('Ctrl Pts',(100.450955115259,3.22783091664314,48.35));
#81923=CARTESIAN_POINT('Ctrl Pts',(100.311391435564,3.02673944830894,48.35));
#81924=CARTESIAN_POINT('Ctrl Pts',(100.311391435564,2.48499327898026,48.35));
#81925=CARTESIAN_POINT('Ctrl Pts',(100.751091323793,1.36248314380646,48.5));
#81926=CARTESIAN_POINT('Ctrl Pts',(100.751091323793,1.36248314380646,48.35));
#81927=CARTESIAN_POINT('Ctrl Pts',(100.432946763933,1.36248314380646,48.5));
#81928=CARTESIAN_POINT('Ctrl Pts',(100.432946763933,1.36248314380646,48.35));
#81929=CARTESIAN_POINT('Ctrl Pts',(100.251364193857,1.59058684110642,48.5));
#81930=CARTESIAN_POINT('Ctrl Pts',(100.251364193857,1.59058684110642,48.35));
#81931=CARTESIAN_POINT('',(100.751091323793,1.36248314380646,48.5));
#81932=CARTESIAN_POINT('',(100.251364193857,1.59058684110642,48.5));
#81933=CARTESIAN_POINT('Ctrl Pts',(100.751091323793,1.36248314380646,48.5));
#81934=CARTESIAN_POINT('Ctrl Pts',(100.432946763933,1.36248314380646,48.5));
#81935=CARTESIAN_POINT('Ctrl Pts',(100.251364193857,1.59058684110642,48.5));
#81936=CARTESIAN_POINT('',(100.751091323793,1.36248314380646,48.35));
#81937=CARTESIAN_POINT('',(100.751091323793,1.36248314380646,48.5));
#81938=CARTESIAN_POINT('',(100.251364193857,1.59058684110642,48.35));
#81939=CARTESIAN_POINT('Ctrl Pts',(100.751091323793,1.36248314380646,48.35));
#81940=CARTESIAN_POINT('Ctrl Pts',(100.432946763933,1.36248314380646,48.35));
#81941=CARTESIAN_POINT('Ctrl Pts',(100.251364193857,1.59058684110642,48.35));
#81942=CARTESIAN_POINT('',(100.251364193857,1.59058684110642,48.5));
#81943=CARTESIAN_POINT('Ctrl Pts',(101.151022993028,1.49229192733765,48.5));
#81944=CARTESIAN_POINT('Ctrl Pts',(101.151022993028,1.49229192733765,48.35));
#81945=CARTESIAN_POINT('Ctrl Pts',(100.992701135576,1.36248314380646,48.5));
#81946=CARTESIAN_POINT('Ctrl Pts',(100.992701135576,1.36248314380646,48.35));
#81947=CARTESIAN_POINT('Ctrl Pts',(100.751091323793,1.36248314380646,48.5));
#81948=CARTESIAN_POINT('Ctrl Pts',(100.751091323793,1.36248314380646,48.35));
#81949=CARTESIAN_POINT('',(101.151022993028,1.49229192733765,48.5));
#81950=CARTESIAN_POINT('Ctrl Pts',(101.151022993028,1.49229192733765,48.5));
#81951=CARTESIAN_POINT('Ctrl Pts',(100.992701135576,1.36248314380646,48.5));
#81952=CARTESIAN_POINT('Ctrl Pts',(100.751091323793,1.36248314380646,48.5));
#81953=CARTESIAN_POINT('',(101.151022993028,1.49229192733765,48.35));
#81954=CARTESIAN_POINT('',(101.151022993028,1.49229192733765,48.5));
#81955=CARTESIAN_POINT('Ctrl Pts',(101.151022993028,1.49229192733765,48.35));
#81956=CARTESIAN_POINT('Ctrl Pts',(100.992701135576,1.36248314380646,48.35));
#81957=CARTESIAN_POINT('Ctrl Pts',(100.751091323793,1.36248314380646,48.35));
#81958=CARTESIAN_POINT('Ctrl Pts',(101.388881288469,1.85995900630951,48.5));
#81959=CARTESIAN_POINT('Ctrl Pts',(101.388881288469,1.85995900630951,48.35));
#81960=CARTESIAN_POINT('Ctrl Pts',(101.309344850481,1.62210100889206,48.5));
#81961=CARTESIAN_POINT('Ctrl Pts',(101.309344850481,1.62210100889206,48.35));
#81962=CARTESIAN_POINT('Ctrl Pts',(101.151022993028,1.49229192733765,48.5));
#81963=CARTESIAN_POINT('Ctrl Pts',(101.151022993028,1.49229192733765,48.35));
#81964=CARTESIAN_POINT('',(101.388881288469,1.85995900630951,48.5));
#81965=CARTESIAN_POINT('Ctrl Pts',(101.388881288469,1.85995900630951,48.5));
#81966=CARTESIAN_POINT('Ctrl Pts',(101.309344850481,1.62210100889206,48.5));
#81967=CARTESIAN_POINT('Ctrl Pts',(101.151022993028,1.49229192733765,48.5));
#81968=CARTESIAN_POINT('',(101.388881288469,1.85995900630951,48.35));
#81969=CARTESIAN_POINT('',(101.388881288469,1.85995900630951,48.5));
#81970=CARTESIAN_POINT('Ctrl Pts',(101.388881288469,1.85995900630951,48.35));
#81971=CARTESIAN_POINT('Ctrl Pts',(101.309344850481,1.62210100889206,48.35));
#81972=CARTESIAN_POINT('Ctrl Pts',(101.151022993028,1.49229192733765,48.35));
#81973=CARTESIAN_POINT('Ctrl Pts',(101.468417130411,2.48499327898026,48.5));
#81974=CARTESIAN_POINT('Ctrl Pts',(101.468417130411,2.48499327898026,48.35));
#81975=CARTESIAN_POINT('Ctrl Pts',(101.468417130411,2.09781730175018,48.5));
#81976=CARTESIAN_POINT('Ctrl Pts',(101.468417130411,2.09781730175018,48.35));
#81977=CARTESIAN_POINT('Ctrl Pts',(101.388881288469,1.85995900630951,48.5));
#81978=CARTESIAN_POINT('Ctrl Pts',(101.388881288469,1.85995900630951,48.35));
#81979=CARTESIAN_POINT('',(101.468417130411,2.48499327898026,48.5));
#81980=CARTESIAN_POINT('Ctrl Pts',(101.468417130411,2.48499327898026,48.5));
#81981=CARTESIAN_POINT('Ctrl Pts',(101.468417130411,2.09781730175018,48.5));
#81982=CARTESIAN_POINT('Ctrl Pts',(101.388881288469,1.85995900630951,48.5));
#81983=CARTESIAN_POINT('',(101.468417130411,2.48499327898026,48.35));
#81984=CARTESIAN_POINT('',(101.468417130411,2.48499327898026,48.5));
#81985=CARTESIAN_POINT('Ctrl Pts',(101.468417130411,2.48499327898026,48.35));
#81986=CARTESIAN_POINT('Ctrl Pts',(101.468417130411,2.09781730175018,48.35));
#81987=CARTESIAN_POINT('Ctrl Pts',(101.388881288469,1.85995900630951,48.35));
#81988=CARTESIAN_POINT('Ctrl Pts',(101.418894611299,3.00497958064079,48.5));
#81989=CARTESIAN_POINT('Ctrl Pts',(101.418894611299,3.00497958064079,48.35));
#81990=CARTESIAN_POINT('Ctrl Pts',(101.468417130411,2.81214186549187,48.5));
#81991=CARTESIAN_POINT('Ctrl Pts',(101.468417130411,2.81214186549187,48.35));
#81992=CARTESIAN_POINT('Ctrl Pts',(101.468417130411,2.48499327898026,48.5));
#81993=CARTESIAN_POINT('Ctrl Pts',(101.468417130411,2.48499327898026,48.35));
#81994=CARTESIAN_POINT('',(101.418894611299,3.00497958064079,48.5));
#81995=CARTESIAN_POINT('Ctrl Pts',(101.418894611299,3.00497958064079,48.5));
#81996=CARTESIAN_POINT('Ctrl Pts',(101.468417130411,2.81214186549187,48.5));
#81997=CARTESIAN_POINT('Ctrl Pts',(101.468417130411,2.48499327898026,48.5));
#81998=CARTESIAN_POINT('',(101.418894611299,3.00497958064079,48.35));
#81999=CARTESIAN_POINT('',(101.418894611299,3.00497958064079,48.5));
#82000=CARTESIAN_POINT('Ctrl Pts',(101.418894611299,3.00497958064079,48.35));
#82001=CARTESIAN_POINT('Ctrl Pts',(101.468417130411,2.81214186549187,48.35));
#82002=CARTESIAN_POINT('Ctrl Pts',(101.468417130411,2.48499327898026,48.35));
#82003=CARTESIAN_POINT('Ctrl Pts',(101.282332621515,3.33212831616402,48.5));
#82004=CARTESIAN_POINT('Ctrl Pts',(101.282332621515,3.33212831616402,48.35));
#82005=CARTESIAN_POINT('Ctrl Pts',(101.369372092187,3.19781729578972,48.5));
#82006=CARTESIAN_POINT('Ctrl Pts',(101.369372092187,3.19781729578972,48.35));
#82007=CARTESIAN_POINT('Ctrl Pts',(101.418894611299,3.00497958064079,48.5));
#82008=CARTESIAN_POINT('Ctrl Pts',(101.418894611299,3.00497958064079,48.35));
#82009=CARTESIAN_POINT('',(101.282332621515,3.33212831616402,48.5));
#82010=CARTESIAN_POINT('Ctrl Pts',(101.282332621515,3.33212831616402,48.5));
#82011=CARTESIAN_POINT('Ctrl Pts',(101.369372092187,3.19781729578972,48.5));
#82012=CARTESIAN_POINT('Ctrl Pts',(101.418894611299,3.00497958064079,48.5));
#82013=CARTESIAN_POINT('',(101.282332621515,3.33212831616402,48.35));
#82014=CARTESIAN_POINT('',(101.282332621515,3.33212831616402,48.5));
#82015=CARTESIAN_POINT('Ctrl Pts',(101.282332621515,3.33212831616402,48.35));
#82016=CARTESIAN_POINT('Ctrl Pts',(101.369372092187,3.19781729578972,48.35));
#82017=CARTESIAN_POINT('Ctrl Pts',(101.418894611299,3.00497958064079,48.35));
#82018=CARTESIAN_POINT('Ctrl Pts',(101.061732850969,3.5377217233181,48.5));
#82019=CARTESIAN_POINT('Ctrl Pts',(101.061732850969,3.5377217233181,48.35));
#82020=CARTESIAN_POINT('Ctrl Pts',(101.195293150842,3.46643933653831,48.5));
#82021=CARTESIAN_POINT('Ctrl Pts',(101.195293150842,3.46643933653831,48.35));
#82022=CARTESIAN_POINT('Ctrl Pts',(101.282332621515,3.33212831616402,48.5));
#82023=CARTESIAN_POINT('Ctrl Pts',(101.282332621515,3.33212831616402,48.35));
#82024=CARTESIAN_POINT('',(101.061732850969,3.5377217233181,48.5));
#82025=CARTESIAN_POINT('Ctrl Pts',(101.061732850969,3.5377217233181,48.5));
#82026=CARTESIAN_POINT('Ctrl Pts',(101.195293150842,3.46643933653831,48.5));
#82027=CARTESIAN_POINT('Ctrl Pts',(101.282332621515,3.33212831616402,48.5));
#82028=CARTESIAN_POINT('',(101.061732850969,3.5377217233181,48.35));
#82029=CARTESIAN_POINT('',(101.061732850969,3.5377217233181,48.5));
#82030=CARTESIAN_POINT('Ctrl Pts',(101.061732850969,3.5377217233181,48.35));
#82031=CARTESIAN_POINT('Ctrl Pts',(101.195293150842,3.46643933653831,48.35));
#82032=CARTESIAN_POINT('Ctrl Pts',(101.282332621515,3.33212831616402,48.35));
#82033=CARTESIAN_POINT('Ctrl Pts',(100.751091323793,3.60900411009789,48.5));
#82034=CARTESIAN_POINT('Ctrl Pts',(100.751091323793,3.60900411009789,48.35));
#82035=CARTESIAN_POINT('Ctrl Pts',(100.928171955049,3.60900411009789,48.5));
#82036=CARTESIAN_POINT('Ctrl Pts',(100.928171955049,3.60900411009789,48.35));
#82037=CARTESIAN_POINT('Ctrl Pts',(101.061732850969,3.5377217233181,48.5));
#82038=CARTESIAN_POINT('Ctrl Pts',(101.061732850969,3.5377217233181,48.35));
#82039=CARTESIAN_POINT('',(100.751091323793,3.60900411009789,48.5));
#82040=CARTESIAN_POINT('Ctrl Pts',(100.751091323793,3.60900411009789,48.5));
#82041=CARTESIAN_POINT('Ctrl Pts',(100.928171955049,3.60900411009789,48.5));
#82042=CARTESIAN_POINT('Ctrl Pts',(101.061732850969,3.5377217233181,48.5));
#82043=CARTESIAN_POINT('',(100.751091323793,3.60900411009789,48.35));
#82044=CARTESIAN_POINT('',(100.751091323793,3.60900411009789,48.5));
#82045=CARTESIAN_POINT('Ctrl Pts',(100.751091323793,3.60900411009789,48.35));
#82046=CARTESIAN_POINT('Ctrl Pts',(100.928171955049,3.60900411009789,48.35));
#82047=CARTESIAN_POINT('Ctrl Pts',(101.061732850969,3.5377217233181,48.35));
#82048=CARTESIAN_POINT('Ctrl Pts',(100.352660499513,3.47994545102119,48.5));
#82049=CARTESIAN_POINT('Ctrl Pts',(100.352660499513,3.47994545102119,48.35));
#82050=CARTESIAN_POINT('Ctrl Pts',(100.510982356966,3.60900411009789,48.5));
#82051=CARTESIAN_POINT('Ctrl Pts',(100.510982356966,3.60900411009789,48.35));
#82052=CARTESIAN_POINT('Ctrl Pts',(100.751091323793,3.60900411009789,48.5));
#82053=CARTESIAN_POINT('Ctrl Pts',(100.751091323793,3.60900411009789,48.35));
#82054=CARTESIAN_POINT('',(100.352660499513,3.47994545102119,48.5));
#82055=CARTESIAN_POINT('Ctrl Pts',(100.352660499513,3.47994545102119,48.5));
#82056=CARTESIAN_POINT('Ctrl Pts',(100.510982356966,3.60900411009789,48.5));
#82057=CARTESIAN_POINT('Ctrl Pts',(100.751091323793,3.60900411009789,48.5));
#82058=CARTESIAN_POINT('',(100.352660499513,3.47994545102119,48.35));
#82059=CARTESIAN_POINT('',(100.352660499513,3.47994545102119,48.5));
#82060=CARTESIAN_POINT('Ctrl Pts',(100.352660499513,3.47994545102119,48.35));
#82061=CARTESIAN_POINT('Ctrl Pts',(100.510982356966,3.60900411009789,48.35));
#82062=CARTESIAN_POINT('Ctrl Pts',(100.751091323793,3.60900411009789,48.35));
#82063=CARTESIAN_POINT('Ctrl Pts',(100.114051781595,3.11302864551544,48.5));
#82064=CARTESIAN_POINT('Ctrl Pts',(100.114051781595,3.11302864551544,48.35));
#82065=CARTESIAN_POINT('Ctrl Pts',(100.194338344038,3.3508867919445,48.5));
#82066=CARTESIAN_POINT('Ctrl Pts',(100.194338344038,3.3508867919445,48.35));
#82067=CARTESIAN_POINT('Ctrl Pts',(100.352660499513,3.47994545102119,48.5));
#82068=CARTESIAN_POINT('Ctrl Pts',(100.352660499513,3.47994545102119,48.35));
#82069=CARTESIAN_POINT('',(100.114051781595,3.11302864551544,48.5));
#82070=CARTESIAN_POINT('Ctrl Pts',(100.114051781595,3.11302864551544,48.5));
#82071=CARTESIAN_POINT('Ctrl Pts',(100.194338344038,3.3508867919445,48.5));
#82072=CARTESIAN_POINT('Ctrl Pts',(100.352660499513,3.47994545102119,48.5));
#82073=CARTESIAN_POINT('',(100.114051781595,3.11302864551544,48.35));
#82074=CARTESIAN_POINT('',(100.114051781595,3.11302864551544,48.5));
#82075=CARTESIAN_POINT('Ctrl Pts',(100.114051781595,3.11302864551544,48.35));
#82076=CARTESIAN_POINT('Ctrl Pts',(100.194338344038,3.3508867919445,48.35));
#82077=CARTESIAN_POINT('Ctrl Pts',(100.352660499513,3.47994545102119,48.35));
#82078=CARTESIAN_POINT('Ctrl Pts',(100.033765517175,2.48499327898026,48.5));
#82079=CARTESIAN_POINT('Ctrl Pts',(100.033765517175,2.48499327898026,48.35));
#82080=CARTESIAN_POINT('Ctrl Pts',(100.033765517175,2.87517049908638,48.5));
#82081=CARTESIAN_POINT('Ctrl Pts',(100.033765517175,2.87517049908638,48.35));
#82082=CARTESIAN_POINT('Ctrl Pts',(100.114051781595,3.11302864551544,48.5));
#82083=CARTESIAN_POINT('Ctrl Pts',(100.114051781595,3.11302864551544,48.35));
#82084=CARTESIAN_POINT('',(100.033765517175,2.48499327898026,48.5));
#82085=CARTESIAN_POINT('Ctrl Pts',(100.033765517175,2.48499327898026,48.5));
#82086=CARTESIAN_POINT('Ctrl Pts',(100.033765517175,2.87517049908638,48.5));
#82087=CARTESIAN_POINT('Ctrl Pts',(100.114051781595,3.11302864551544,48.5));
#82088=CARTESIAN_POINT('',(100.033765517175,2.48499327898026,48.35));
#82089=CARTESIAN_POINT('',(100.033765517175,2.48499327898026,48.5));
#82090=CARTESIAN_POINT('Ctrl Pts',(100.033765517175,2.48499327898026,48.35));
#82091=CARTESIAN_POINT('Ctrl Pts',(100.033765517175,2.87517049908638,48.35));
#82092=CARTESIAN_POINT('Ctrl Pts',(100.114051781595,3.11302864551544,48.35));
#82093=CARTESIAN_POINT('Ctrl Pts',(100.251364193857,1.59058684110642,48.5));
#82094=CARTESIAN_POINT('Ctrl Pts',(100.251364193857,1.59058684110642,48.35));
#82095=CARTESIAN_POINT('Ctrl Pts',(100.033765517175,1.86521166563034,48.5));
#82096=CARTESIAN_POINT('Ctrl Pts',(100.033765517175,1.86521166563034,48.35));
#82097=CARTESIAN_POINT('Ctrl Pts',(100.033765517175,2.48499327898026,48.5));
#82098=CARTESIAN_POINT('Ctrl Pts',(100.033765517175,2.48499327898026,48.35));
#82099=CARTESIAN_POINT('Ctrl Pts',(100.251364193857,1.59058684110642,48.5));
#82100=CARTESIAN_POINT('Ctrl Pts',(100.033765517175,1.86521166563034,48.5));
#82101=CARTESIAN_POINT('Ctrl Pts',(100.033765517175,2.48499327898026,48.5));
#82102=CARTESIAN_POINT('Ctrl Pts',(100.251364193857,1.59058684110642,48.35));
#82103=CARTESIAN_POINT('Ctrl Pts',(100.033765517175,1.86521166563034,48.35));
#82104=CARTESIAN_POINT('Ctrl Pts',(100.033765517175,2.48499327898026,48.35));
#82105=CARTESIAN_POINT('Origin',(99.999999858439,2.48574362695217,48.35));
#82106=CARTESIAN_POINT('Origin',(99.1678718551993,3.60900411009789,48.5));
#82107=CARTESIAN_POINT('',(99.1678718551993,3.60900411009789,48.5));
#82108=CARTESIAN_POINT('',(99.3419510945678,3.60900411009789,48.5));
#82109=CARTESIAN_POINT('',(49.5839359275997,3.60900411009789,48.5));
#82110=CARTESIAN_POINT('',(99.1678718551993,3.60900411009789,48.35));
#82111=CARTESIAN_POINT('',(99.1678718551993,3.60900411009789,48.5));
#82112=CARTESIAN_POINT('',(99.3419510945678,3.60900411009789,48.35));
#82113=CARTESIAN_POINT('',(99.1678718551993,3.60900411009789,48.35));
#82114=CARTESIAN_POINT('',(99.3419510945678,3.60900411009789,48.5));
#82115=CARTESIAN_POINT('Ctrl Pts',(98.9277627393603,3.31487053632736,48.5));
#82116=CARTESIAN_POINT('Ctrl Pts',(98.9277627393603,3.31487053632736,48.35));
#82117=CARTESIAN_POINT('Ctrl Pts',(99.0973397418857,3.46643933653831,48.5));
#82118=CARTESIAN_POINT('Ctrl Pts',(99.0973397418857,3.46643933653831,48.35));
#82119=CARTESIAN_POINT('Ctrl Pts',(99.1678718551993,3.60900411009789,48.5));
#82120=CARTESIAN_POINT('Ctrl Pts',(99.1678718551993,3.60900411009789,48.35));
#82121=CARTESIAN_POINT('',(98.9277627393603,3.31487053632736,48.5));
#82122=CARTESIAN_POINT('Ctrl Pts',(98.9277627393603,3.31487053632736,48.5));
#82123=CARTESIAN_POINT('Ctrl Pts',(99.0973397418857,3.46643933653831,48.5));
#82124=CARTESIAN_POINT('Ctrl Pts',(99.1678718551993,3.60900411009789,48.5));
#82125=CARTESIAN_POINT('',(98.9277627393603,3.31487053632736,48.35));
#82126=CARTESIAN_POINT('',(98.9277627393603,3.31487053632736,48.5));
#82127=CARTESIAN_POINT('Ctrl Pts',(98.9277627393603,3.31487053632736,48.35));
#82128=CARTESIAN_POINT('Ctrl Pts',(99.0973397418857,3.46643933653831,48.35));
#82129=CARTESIAN_POINT('Ctrl Pts',(99.1678718551993,3.60900411009789,48.35));
#82130=CARTESIAN_POINT('Ctrl Pts',(98.5315825864673,3.05675321817398,48.5));
#82131=CARTESIAN_POINT('Ctrl Pts',(98.5315825864673,3.05675321817398,48.35));
#82132=CARTESIAN_POINT('Ctrl Pts',(98.7581855878234,3.1633015871048,48.5));
#82133=CARTESIAN_POINT('Ctrl Pts',(98.7581855878234,3.1633015871048,48.35));
#82134=CARTESIAN_POINT('Ctrl Pts',(98.9277627393603,3.31487053632736,48.5));
#82135=CARTESIAN_POINT('Ctrl Pts',(98.9277627393603,3.31487053632736,48.35));
#82136=CARTESIAN_POINT('',(98.5315825864673,3.05675321817398,48.5));
#82137=CARTESIAN_POINT('Ctrl Pts',(98.5315825864673,3.05675321817398,48.5));
#82138=CARTESIAN_POINT('Ctrl Pts',(98.7581855878234,3.1633015871048,48.5));
#82139=CARTESIAN_POINT('Ctrl Pts',(98.9277627393603,3.31487053632736,48.5));
#82140=CARTESIAN_POINT('',(98.5315825864673,3.05675321817398,48.35));
#82141=CARTESIAN_POINT('',(98.5315825864673,3.05675321817398,48.5));
#82142=CARTESIAN_POINT('Ctrl Pts',(98.5315825864673,3.05675321817398,48.35));
#82143=CARTESIAN_POINT('Ctrl Pts',(98.7581855878234,3.1633015871048,48.35));
#82144=CARTESIAN_POINT('Ctrl Pts',(98.9277627393603,3.31487053632736,48.35));
#82145=CARTESIAN_POINT('Origin',(98.5315825864673,2.79563450813293,48.5));
#82146=CARTESIAN_POINT('',(98.5315825864673,2.79563450813293,48.5));
#82147=CARTESIAN_POINT('',(98.5315825864673,5.39781725406647,48.5));
#82148=CARTESIAN_POINT('',(98.5315825864673,2.79563450813293,48.35));
#82149=CARTESIAN_POINT('',(98.5315825864673,2.79563450813293,48.5));
#82150=CARTESIAN_POINT('',(98.5315825864673,2.79563450813293,48.35));
#82151=CARTESIAN_POINT('Ctrl Pts',(98.8159618601203,2.93519788980484,48.5));
#82152=CARTESIAN_POINT('Ctrl Pts',(98.8159618601203,2.93519788980484,48.35));
#82153=CARTESIAN_POINT('Ctrl Pts',(98.6576400026679,2.8421556353569,48.5));
#82154=CARTESIAN_POINT('Ctrl Pts',(98.6576400026679,2.8421556353569,48.35));
#82155=CARTESIAN_POINT('Ctrl Pts',(98.5315825864673,2.79563450813293,48.5));
#82156=CARTESIAN_POINT('Ctrl Pts',(98.5315825864673,2.79563450813293,48.35));
#82157=CARTESIAN_POINT('',(98.8159618601203,2.93519788980484,48.5));
#82158=CARTESIAN_POINT('Ctrl Pts',(98.8159618601203,2.93519788980484,48.5));
#82159=CARTESIAN_POINT('Ctrl Pts',(98.6576400026679,2.8421556353569,48.5));
#82160=CARTESIAN_POINT('Ctrl Pts',(98.5315825864673,2.79563450813293,48.5));
#82161=CARTESIAN_POINT('',(98.8159618601203,2.93519788980484,48.35));
#82162=CARTESIAN_POINT('',(98.8159618601203,2.93519788980484,48.5));
#82163=CARTESIAN_POINT('Ctrl Pts',(98.8159618601203,2.93519788980484,48.35));
#82164=CARTESIAN_POINT('Ctrl Pts',(98.6576400026679,2.8421556353569,48.35));
#82165=CARTESIAN_POINT('Ctrl Pts',(98.5315825864673,2.79563450813293,48.35));
#82166=CARTESIAN_POINT('Ctrl Pts',(99.0718282088637,3.12128254771233,48.5));
#82167=CARTESIAN_POINT('Ctrl Pts',(99.0718282088637,3.12128254771233,48.35));
#82168=CARTESIAN_POINT('Ctrl Pts',(98.9742838665843,3.02824014425278,48.5));
#82169=CARTESIAN_POINT('Ctrl Pts',(98.9742838665843,3.02824014425278,48.35));
#82170=CARTESIAN_POINT('Ctrl Pts',(98.8159618601203,2.93519788980484,48.5));
#82171=CARTESIAN_POINT('Ctrl Pts',(98.8159618601203,2.93519788980484,48.35));
#82172=CARTESIAN_POINT('',(99.0718282088637,3.12128254771233,48.5));
#82173=CARTESIAN_POINT('Ctrl Pts',(99.0718282088637,3.12128254771233,48.5));
#82174=CARTESIAN_POINT('Ctrl Pts',(98.9742838665843,3.02824014425278,48.5));
#82175=CARTESIAN_POINT('Ctrl Pts',(98.8159618601203,2.93519788980484,48.5));
#82176=CARTESIAN_POINT('',(99.0718282088637,3.12128254771233,48.35));
#82177=CARTESIAN_POINT('',(99.0718282088637,3.12128254771233,48.5));
#82178=CARTESIAN_POINT('Ctrl Pts',(99.0718282088637,3.12128254771233,48.35));
#82179=CARTESIAN_POINT('Ctrl Pts',(98.9742838665843,3.02824014425278,48.35));
#82180=CARTESIAN_POINT('Ctrl Pts',(98.8159618601203,2.93519788980484,48.35));
#82181=CARTESIAN_POINT('Origin',(99.0718282088637,1.40000009536743,48.5));
#82182=CARTESIAN_POINT('',(99.0718282088637,1.40000009536743,48.5));
#82183=CARTESIAN_POINT('',(99.0718282088637,4.70000004768372,48.5));
#82184=CARTESIAN_POINT('',(99.0718282088637,1.40000009536743,48.35));
#82185=CARTESIAN_POINT('',(99.0718282088637,1.40000009536743,48.5));
#82186=CARTESIAN_POINT('',(99.0718282088637,1.40000009536743,48.35));
#82187=CARTESIAN_POINT('Origin',(99.3419510945678,1.40000009536743,48.5));
#82188=CARTESIAN_POINT('',(99.3419510945678,1.40000009536743,48.5));
#82189=CARTESIAN_POINT('',(49.6709755472839,1.40000009536743,48.5));
#82190=CARTESIAN_POINT('',(99.3419510945678,1.40000009536743,48.35));
#82191=CARTESIAN_POINT('',(99.3419510945678,1.40000009536743,48.5));
#82192=CARTESIAN_POINT('',(99.3419510945678,1.40000009536743,48.35));
#82193=CARTESIAN_POINT('Origin',(99.3419510945678,3.60900411009789,48.5));
#82194=CARTESIAN_POINT('',(99.3419510945678,5.80450205504894,48.5));
#82195=CARTESIAN_POINT('',(99.3419510945678,3.60900411009789,48.35));
#82196=CARTESIAN_POINT('Origin',(99.999999858439,2.48574362695217,48.35));
#82197=CARTESIAN_POINT('Origin',(0.,8.,48.5));
#82198=CARTESIAN_POINT('Ctrl Pts',(90.8703956548125,3.38540250062943,48.5));
#82199=CARTESIAN_POINT('Ctrl Pts',(90.8703956548125,3.38540250062943,48.35));
#82200=CARTESIAN_POINT('Ctrl Pts',(90.6843108478934,3.38540250062943,48.5));
#82201=CARTESIAN_POINT('Ctrl Pts',(90.6843108478934,3.38540250062943,48.35));
#82202=CARTESIAN_POINT('Ctrl Pts',(90.5732605401427,3.22783091664314,48.5));
#82203=CARTESIAN_POINT('Ctrl Pts',(90.5732605401427,3.22783091664314,48.35));
#82204=CARTESIAN_POINT('',(90.8703956548125,3.38540250062943,48.5));
#82205=CARTESIAN_POINT('',(90.5732605401427,3.22783091664314,48.5));
#82206=CARTESIAN_POINT('Ctrl Pts',(90.8703956548125,3.38540250062943,48.5));
#82207=CARTESIAN_POINT('Ctrl Pts',(90.6843108478934,3.38540250062943,48.5));
#82208=CARTESIAN_POINT('Ctrl Pts',(90.5732605401427,3.22783091664314,48.5));
#82209=CARTESIAN_POINT('',(90.8703956548125,3.38540250062943,48.35));
#82210=CARTESIAN_POINT('',(90.8703956548125,3.38540250062943,48.5));
#82211=CARTESIAN_POINT('',(90.5732605401427,3.22783091664314,48.35));
#82212=CARTESIAN_POINT('Ctrl Pts',(90.8703956548125,3.38540250062943,48.35));
#82213=CARTESIAN_POINT('Ctrl Pts',(90.6843108478934,3.38540250062943,48.35));
#82214=CARTESIAN_POINT('Ctrl Pts',(90.5732605401427,3.22783091664314,48.35));
#82215=CARTESIAN_POINT('',(90.5732605401427,3.22783091664314,48.5));
#82216=CARTESIAN_POINT('Ctrl Pts',(91.1862889472395,3.2068213224411,48.5));
#82217=CARTESIAN_POINT('Ctrl Pts',(91.1862889472395,3.2068213224411,48.35));
#82218=CARTESIAN_POINT('Ctrl Pts',(91.0594812575728,3.38540250062943,48.5));
#82219=CARTESIAN_POINT('Ctrl Pts',(91.0594812575728,3.38540250062943,48.35));
#82220=CARTESIAN_POINT('Ctrl Pts',(90.8703956548125,3.38540250062943,48.5));
#82221=CARTESIAN_POINT('Ctrl Pts',(90.8703956548125,3.38540250062943,48.35));
#82222=CARTESIAN_POINT('',(91.1862889472395,3.2068213224411,48.5));
#82223=CARTESIAN_POINT('Ctrl Pts',(91.1862889472395,3.2068213224411,48.5));
#82224=CARTESIAN_POINT('Ctrl Pts',(91.0594812575728,3.38540250062943,48.5));
#82225=CARTESIAN_POINT('Ctrl Pts',(90.8703956548125,3.38540250062943,48.5));
#82226=CARTESIAN_POINT('',(91.1862889472395,3.2068213224411,48.35));
#82227=CARTESIAN_POINT('',(91.1862889472395,3.2068213224411,48.5));
#82228=CARTESIAN_POINT('Ctrl Pts',(91.1862889472395,3.2068213224411,48.35));
#82229=CARTESIAN_POINT('Ctrl Pts',(91.0594812575728,3.38540250062943,48.35));
#82230=CARTESIAN_POINT('Ctrl Pts',(90.8703956548125,3.38540250062943,48.35));
#82231=CARTESIAN_POINT('Ctrl Pts',(91.3130966369063,2.48499327898026,48.5));
#82232=CARTESIAN_POINT('Ctrl Pts',(91.3130966369063,2.48499327898026,48.35));
#82233=CARTESIAN_POINT('Ctrl Pts',(91.3130966369063,3.02824014425278,48.5));
#82234=CARTESIAN_POINT('Ctrl Pts',(91.3130966369063,3.02824014425278,48.35));
#82235=CARTESIAN_POINT('Ctrl Pts',(91.1862889472395,3.2068213224411,48.5));
#82236=CARTESIAN_POINT('Ctrl Pts',(91.1862889472395,3.2068213224411,48.35));
#82237=CARTESIAN_POINT('',(91.3130966369063,2.48499327898026,48.5));
#82238=CARTESIAN_POINT('Ctrl Pts',(91.3130966369063,2.48499327898026,48.5));
#82239=CARTESIAN_POINT('Ctrl Pts',(91.3130966369063,3.02824014425278,48.5));
#82240=CARTESIAN_POINT('Ctrl Pts',(91.1862889472395,3.2068213224411,48.5));
#82241=CARTESIAN_POINT('',(91.3130966369063,2.48499327898026,48.35));
#82242=CARTESIAN_POINT('',(91.3130966369063,2.48499327898026,48.5));
#82243=CARTESIAN_POINT('Ctrl Pts',(91.3130966369063,2.48499327898026,48.35));
#82244=CARTESIAN_POINT('Ctrl Pts',(91.3130966369063,3.02824014425278,48.35));
#82245=CARTESIAN_POINT('Ctrl Pts',(91.1862889472395,3.2068213224411,48.35));
#82246=CARTESIAN_POINT('Ctrl Pts',(91.1862889472395,1.76466578245163,48.5));
#82247=CARTESIAN_POINT('Ctrl Pts',(91.1862889472395,1.76466578245163,48.35));
#82248=CARTESIAN_POINT('Ctrl Pts',(91.3130966369063,1.9447478055954,48.5));
#82249=CARTESIAN_POINT('Ctrl Pts',(91.3130966369063,1.9447478055954,48.35));
#82250=CARTESIAN_POINT('Ctrl Pts',(91.3130966369063,2.48499327898026,48.5));
#82251=CARTESIAN_POINT('Ctrl Pts',(91.3130966369063,2.48499327898026,48.35));
#82252=CARTESIAN_POINT('',(91.1862889472395,1.76466578245163,48.5));
#82253=CARTESIAN_POINT('Ctrl Pts',(91.1862889472395,1.76466578245163,48.5));
#82254=CARTESIAN_POINT('Ctrl Pts',(91.3130966369063,1.9447478055954,48.5));
#82255=CARTESIAN_POINT('Ctrl Pts',(91.3130966369063,2.48499327898026,48.5));
#82256=CARTESIAN_POINT('',(91.1862889472395,1.76466578245163,48.35));
#82257=CARTESIAN_POINT('',(91.1862889472395,1.76466578245163,48.5));
#82258=CARTESIAN_POINT('Ctrl Pts',(91.1862889472395,1.76466578245163,48.35));
#82259=CARTESIAN_POINT('Ctrl Pts',(91.3130966369063,1.9447478055954,48.35));
#82260=CARTESIAN_POINT('Ctrl Pts',(91.3130966369063,2.48499327898026,48.35));
#82261=CARTESIAN_POINT('Ctrl Pts',(90.8733967486769,1.58458405733109,48.5));
#82262=CARTESIAN_POINT('Ctrl Pts',(90.8733967486769,1.58458405733109,48.35));
#82263=CARTESIAN_POINT('Ctrl Pts',(91.0594812575728,1.58458405733109,48.5));
#82264=CARTESIAN_POINT('Ctrl Pts',(91.0594812575728,1.58458405733109,48.35));
#82265=CARTESIAN_POINT('Ctrl Pts',(91.1862889472395,1.76466578245163,48.5));
#82266=CARTESIAN_POINT('Ctrl Pts',(91.1862889472395,1.76466578245163,48.35));
#82267=CARTESIAN_POINT('',(90.8733967486769,1.58458405733109,48.5));
#82268=CARTESIAN_POINT('Ctrl Pts',(90.8733967486769,1.58458405733109,48.5));
#82269=CARTESIAN_POINT('Ctrl Pts',(91.0594812575728,1.58458405733109,48.5));
#82270=CARTESIAN_POINT('Ctrl Pts',(91.1862889472395,1.76466578245163,48.5));
#82271=CARTESIAN_POINT('',(90.8733967486769,1.58458405733109,48.35));
#82272=CARTESIAN_POINT('',(90.8733967486769,1.58458405733109,48.5));
#82273=CARTESIAN_POINT('Ctrl Pts',(90.8733967486769,1.58458405733109,48.35));
#82274=CARTESIAN_POINT('Ctrl Pts',(91.0594812575728,1.58458405733109,48.35));
#82275=CARTESIAN_POINT('Ctrl Pts',(91.1862889472395,1.76466578245163,48.35));
#82276=CARTESIAN_POINT('Ctrl Pts',(90.5605045501143,1.76391565799713,48.5));
#82277=CARTESIAN_POINT('Ctrl Pts',(90.5605045501143,1.76391565799713,48.35));
#82278=CARTESIAN_POINT('Ctrl Pts',(90.687312239781,1.58458405733109,48.5));
#82279=CARTESIAN_POINT('Ctrl Pts',(90.687312239781,1.58458405733109,48.35));
#82280=CARTESIAN_POINT('Ctrl Pts',(90.8733967486769,1.58458405733109,48.5));
#82281=CARTESIAN_POINT('Ctrl Pts',(90.8733967486769,1.58458405733109,48.35));
#82282=CARTESIAN_POINT('',(90.5605045501143,1.76391565799713,48.5));
#82283=CARTESIAN_POINT('Ctrl Pts',(90.5605045501143,1.76391565799713,48.5));
#82284=CARTESIAN_POINT('Ctrl Pts',(90.687312239781,1.58458405733109,48.5));
#82285=CARTESIAN_POINT('Ctrl Pts',(90.8733967486769,1.58458405733109,48.5));
#82286=CARTESIAN_POINT('',(90.5605045501143,1.76391565799713,48.35));
#82287=CARTESIAN_POINT('',(90.5605045501143,1.76391565799713,48.5));
#82288=CARTESIAN_POINT('Ctrl Pts',(90.5605045501143,1.76391565799713,48.35));
#82289=CARTESIAN_POINT('Ctrl Pts',(90.687312239781,1.58458405733109,48.35));
#82290=CARTESIAN_POINT('Ctrl Pts',(90.8733967486769,1.58458405733109,48.35));
#82291=CARTESIAN_POINT('Ctrl Pts',(90.4336968604475,2.48499327898026,48.5));
#82292=CARTESIAN_POINT('Ctrl Pts',(90.4336968604475,2.48499327898026,48.35));
#82293=CARTESIAN_POINT('Ctrl Pts',(90.4336968604475,1.94324696063995,48.5));
#82294=CARTESIAN_POINT('Ctrl Pts',(90.4336968604475,1.94324696063995,48.35));
#82295=CARTESIAN_POINT('Ctrl Pts',(90.5605045501143,1.76391565799713,48.5));
#82296=CARTESIAN_POINT('Ctrl Pts',(90.5605045501143,1.76391565799713,48.35));
#82297=CARTESIAN_POINT('',(90.4336968604475,2.48499327898026,48.5));
#82298=CARTESIAN_POINT('Ctrl Pts',(90.4336968604475,2.48499327898026,48.5));
#82299=CARTESIAN_POINT('Ctrl Pts',(90.4336968604475,1.94324696063995,48.5));
#82300=CARTESIAN_POINT('Ctrl Pts',(90.5605045501143,1.76391565799713,48.5));
#82301=CARTESIAN_POINT('',(90.4336968604475,2.48499327898026,48.35));
#82302=CARTESIAN_POINT('',(90.4336968604475,2.48499327898026,48.5));
#82303=CARTESIAN_POINT('Ctrl Pts',(90.4336968604475,2.48499327898026,48.35));
#82304=CARTESIAN_POINT('Ctrl Pts',(90.4336968604475,1.94324696063995,48.35));
#82305=CARTESIAN_POINT('Ctrl Pts',(90.5605045501143,1.76391565799713,48.35));
#82306=CARTESIAN_POINT('Ctrl Pts',(90.5732605401427,3.22783091664314,48.5));
#82307=CARTESIAN_POINT('Ctrl Pts',(90.5732605401427,3.22783091664314,48.35));
#82308=CARTESIAN_POINT('Ctrl Pts',(90.4336968604475,3.02673944830894,48.5));
#82309=CARTESIAN_POINT('Ctrl Pts',(90.4336968604475,3.02673944830894,48.35));
#82310=CARTESIAN_POINT('Ctrl Pts',(90.4336968604475,2.48499327898026,48.5));
#82311=CARTESIAN_POINT('Ctrl Pts',(90.4336968604475,2.48499327898026,48.35));
#82312=CARTESIAN_POINT('Ctrl Pts',(90.5732605401427,3.22783091664314,48.5));
#82313=CARTESIAN_POINT('Ctrl Pts',(90.4336968604475,3.02673944830894,48.5));
#82314=CARTESIAN_POINT('Ctrl Pts',(90.4336968604475,2.48499327898026,48.5));
#82315=CARTESIAN_POINT('Ctrl Pts',(90.5732605401427,3.22783091664314,48.35));
#82316=CARTESIAN_POINT('Ctrl Pts',(90.4336968604475,3.02673944830894,48.35));
#82317=CARTESIAN_POINT('Ctrl Pts',(90.4336968604475,2.48499327898026,48.35));
#82318=CARTESIAN_POINT('Ctrl Pts',(90.8733967486769,1.36248314380646,48.5));
#82319=CARTESIAN_POINT('Ctrl Pts',(90.8733967486769,1.36248314380646,48.35));
#82320=CARTESIAN_POINT('Ctrl Pts',(90.5552521888167,1.36248314380646,48.5));
#82321=CARTESIAN_POINT('Ctrl Pts',(90.5552521888167,1.36248314380646,48.35));
#82322=CARTESIAN_POINT('Ctrl Pts',(90.3736696187407,1.59058684110642,48.5));
#82323=CARTESIAN_POINT('Ctrl Pts',(90.3736696187407,1.59058684110642,48.35));
#82324=CARTESIAN_POINT('',(90.8733967486769,1.36248314380646,48.5));
#82325=CARTESIAN_POINT('',(90.3736696187407,1.59058684110642,48.5));
#82326=CARTESIAN_POINT('Ctrl Pts',(90.8733967486769,1.36248314380646,48.5));
#82327=CARTESIAN_POINT('Ctrl Pts',(90.5552521888167,1.36248314380646,48.5));
#82328=CARTESIAN_POINT('Ctrl Pts',(90.3736696187407,1.59058684110642,48.5));
#82329=CARTESIAN_POINT('',(90.8733967486769,1.36248314380646,48.35));
#82330=CARTESIAN_POINT('',(90.8733967486769,1.36248314380646,48.5));
#82331=CARTESIAN_POINT('',(90.3736696187407,1.59058684110642,48.35));
#82332=CARTESIAN_POINT('Ctrl Pts',(90.8733967486769,1.36248314380646,48.35));
#82333=CARTESIAN_POINT('Ctrl Pts',(90.5552521888167,1.36248314380646,48.35));
#82334=CARTESIAN_POINT('Ctrl Pts',(90.3736696187407,1.59058684110642,48.35));
#82335=CARTESIAN_POINT('',(90.3736696187407,1.59058684110642,48.5));
#82336=CARTESIAN_POINT('Ctrl Pts',(91.2733284179121,1.49229192733765,48.5));
#82337=CARTESIAN_POINT('Ctrl Pts',(91.2733284179121,1.49229192733765,48.35));
#82338=CARTESIAN_POINT('Ctrl Pts',(91.1150065604597,1.36248314380646,48.5));
#82339=CARTESIAN_POINT('Ctrl Pts',(91.1150065604597,1.36248314380646,48.35));
#82340=CARTESIAN_POINT('Ctrl Pts',(90.8733967486769,1.36248314380646,48.5));
#82341=CARTESIAN_POINT('Ctrl Pts',(90.8733967486769,1.36248314380646,48.35));
#82342=CARTESIAN_POINT('',(91.2733284179121,1.49229192733765,48.5));
#82343=CARTESIAN_POINT('Ctrl Pts',(91.2733284179121,1.49229192733765,48.5));
#82344=CARTESIAN_POINT('Ctrl Pts',(91.1150065604597,1.36248314380646,48.5));
#82345=CARTESIAN_POINT('Ctrl Pts',(90.8733967486769,1.36248314380646,48.5));
#82346=CARTESIAN_POINT('',(91.2733284179121,1.49229192733765,48.35));
#82347=CARTESIAN_POINT('',(91.2733284179121,1.49229192733765,48.5));
#82348=CARTESIAN_POINT('Ctrl Pts',(91.2733284179121,1.49229192733765,48.35));
#82349=CARTESIAN_POINT('Ctrl Pts',(91.1150065604597,1.36248314380646,48.35));
#82350=CARTESIAN_POINT('Ctrl Pts',(90.8733967486769,1.36248314380646,48.35));
#82351=CARTESIAN_POINT('Ctrl Pts',(91.5111867133528,1.85995900630951,48.5));
#82352=CARTESIAN_POINT('Ctrl Pts',(91.5111867133528,1.85995900630951,48.35));
#82353=CARTESIAN_POINT('Ctrl Pts',(91.4316502753645,1.62210100889206,48.5));
#82354=CARTESIAN_POINT('Ctrl Pts',(91.4316502753645,1.62210100889206,48.35));
#82355=CARTESIAN_POINT('Ctrl Pts',(91.2733284179121,1.49229192733765,48.5));
#82356=CARTESIAN_POINT('Ctrl Pts',(91.2733284179121,1.49229192733765,48.35));
#82357=CARTESIAN_POINT('',(91.5111867133528,1.85995900630951,48.5));
#82358=CARTESIAN_POINT('Ctrl Pts',(91.5111867133528,1.85995900630951,48.5));
#82359=CARTESIAN_POINT('Ctrl Pts',(91.4316502753645,1.62210100889206,48.5));
#82360=CARTESIAN_POINT('Ctrl Pts',(91.2733284179121,1.49229192733765,48.5));
#82361=CARTESIAN_POINT('',(91.5111867133528,1.85995900630951,48.35));
#82362=CARTESIAN_POINT('',(91.5111867133528,1.85995900630951,48.5));
#82363=CARTESIAN_POINT('Ctrl Pts',(91.5111867133528,1.85995900630951,48.35));
#82364=CARTESIAN_POINT('Ctrl Pts',(91.4316502753645,1.62210100889206,48.35));
#82365=CARTESIAN_POINT('Ctrl Pts',(91.2733284179121,1.49229192733765,48.35));
#82366=CARTESIAN_POINT('Ctrl Pts',(91.5907225552946,2.48499327898026,48.5));
#82367=CARTESIAN_POINT('Ctrl Pts',(91.5907225552946,2.48499327898026,48.35));
#82368=CARTESIAN_POINT('Ctrl Pts',(91.5907225552946,2.09781730175018,48.5));
#82369=CARTESIAN_POINT('Ctrl Pts',(91.5907225552946,2.09781730175018,48.35));
#82370=CARTESIAN_POINT('Ctrl Pts',(91.5111867133528,1.85995900630951,48.5));
#82371=CARTESIAN_POINT('Ctrl Pts',(91.5111867133528,1.85995900630951,48.35));
#82372=CARTESIAN_POINT('',(91.5907225552946,2.48499327898026,48.5));
#82373=CARTESIAN_POINT('Ctrl Pts',(91.5907225552946,2.48499327898026,48.5));
#82374=CARTESIAN_POINT('Ctrl Pts',(91.5907225552946,2.09781730175018,48.5));
#82375=CARTESIAN_POINT('Ctrl Pts',(91.5111867133528,1.85995900630951,48.5));
#82376=CARTESIAN_POINT('',(91.5907225552946,2.48499327898026,48.35));
#82377=CARTESIAN_POINT('',(91.5907225552946,2.48499327898026,48.5));
#82378=CARTESIAN_POINT('Ctrl Pts',(91.5907225552946,2.48499327898026,48.35));
#82379=CARTESIAN_POINT('Ctrl Pts',(91.5907225552946,2.09781730175018,48.35));
#82380=CARTESIAN_POINT('Ctrl Pts',(91.5111867133528,1.85995900630951,48.35));
#82381=CARTESIAN_POINT('Ctrl Pts',(91.541200036183,3.00497958064079,48.5));
#82382=CARTESIAN_POINT('Ctrl Pts',(91.541200036183,3.00497958064079,48.35));
#82383=CARTESIAN_POINT('Ctrl Pts',(91.5907225552946,2.81214186549187,48.5));
#82384=CARTESIAN_POINT('Ctrl Pts',(91.5907225552946,2.81214186549187,48.35));
#82385=CARTESIAN_POINT('Ctrl Pts',(91.5907225552946,2.48499327898026,48.5));
#82386=CARTESIAN_POINT('Ctrl Pts',(91.5907225552946,2.48499327898026,48.35));
#82387=CARTESIAN_POINT('',(91.541200036183,3.00497958064079,48.5));
#82388=CARTESIAN_POINT('Ctrl Pts',(91.541200036183,3.00497958064079,48.5));
#82389=CARTESIAN_POINT('Ctrl Pts',(91.5907225552946,2.81214186549187,48.5));
#82390=CARTESIAN_POINT('Ctrl Pts',(91.5907225552946,2.48499327898026,48.5));
#82391=CARTESIAN_POINT('',(91.541200036183,3.00497958064079,48.35));
#82392=CARTESIAN_POINT('',(91.541200036183,3.00497958064079,48.5));
#82393=CARTESIAN_POINT('Ctrl Pts',(91.541200036183,3.00497958064079,48.35));
#82394=CARTESIAN_POINT('Ctrl Pts',(91.5907225552946,2.81214186549187,48.35));
#82395=CARTESIAN_POINT('Ctrl Pts',(91.5907225552946,2.48499327898026,48.35));
#82396=CARTESIAN_POINT('Ctrl Pts',(91.4046380463988,3.33212831616402,48.5));
#82397=CARTESIAN_POINT('Ctrl Pts',(91.4046380463988,3.33212831616402,48.35));
#82398=CARTESIAN_POINT('Ctrl Pts',(91.4916775170714,3.19781729578972,48.5));
#82399=CARTESIAN_POINT('Ctrl Pts',(91.4916775170714,3.19781729578972,48.35));
#82400=CARTESIAN_POINT('Ctrl Pts',(91.541200036183,3.00497958064079,48.5));
#82401=CARTESIAN_POINT('Ctrl Pts',(91.541200036183,3.00497958064079,48.35));
#82402=CARTESIAN_POINT('',(91.4046380463988,3.33212831616402,48.5));
#82403=CARTESIAN_POINT('Ctrl Pts',(91.4046380463988,3.33212831616402,48.5));
#82404=CARTESIAN_POINT('Ctrl Pts',(91.4916775170714,3.19781729578972,48.5));
#82405=CARTESIAN_POINT('Ctrl Pts',(91.541200036183,3.00497958064079,48.5));
#82406=CARTESIAN_POINT('',(91.4046380463988,3.33212831616402,48.35));
#82407=CARTESIAN_POINT('',(91.4046380463988,3.33212831616402,48.5));
#82408=CARTESIAN_POINT('Ctrl Pts',(91.4046380463988,3.33212831616402,48.35));
#82409=CARTESIAN_POINT('Ctrl Pts',(91.4916775170714,3.19781729578972,48.35));
#82410=CARTESIAN_POINT('Ctrl Pts',(91.541200036183,3.00497958064079,48.35));
#82411=CARTESIAN_POINT('Ctrl Pts',(91.1840382758528,3.5377217233181,48.5));
#82412=CARTESIAN_POINT('Ctrl Pts',(91.1840382758528,3.5377217233181,48.35));
#82413=CARTESIAN_POINT('Ctrl Pts',(91.3175985757262,3.46643933653831,48.5));
#82414=CARTESIAN_POINT('Ctrl Pts',(91.3175985757262,3.46643933653831,48.35));
#82415=CARTESIAN_POINT('Ctrl Pts',(91.4046380463988,3.33212831616402,48.5));
#82416=CARTESIAN_POINT('Ctrl Pts',(91.4046380463988,3.33212831616402,48.35));
#82417=CARTESIAN_POINT('',(91.1840382758528,3.5377217233181,48.5));
#82418=CARTESIAN_POINT('Ctrl Pts',(91.1840382758528,3.5377217233181,48.5));
#82419=CARTESIAN_POINT('Ctrl Pts',(91.3175985757262,3.46643933653831,48.5));
#82420=CARTESIAN_POINT('Ctrl Pts',(91.4046380463988,3.33212831616402,48.5));
#82421=CARTESIAN_POINT('',(91.1840382758528,3.5377217233181,48.35));
#82422=CARTESIAN_POINT('',(91.1840382758528,3.5377217233181,48.5));
#82423=CARTESIAN_POINT('Ctrl Pts',(91.1840382758528,3.5377217233181,48.35));
#82424=CARTESIAN_POINT('Ctrl Pts',(91.3175985757262,3.46643933653831,48.35));
#82425=CARTESIAN_POINT('Ctrl Pts',(91.4046380463988,3.33212831616402,48.35));
#82426=CARTESIAN_POINT('Ctrl Pts',(90.8733967486769,3.60900411009789,48.5));
#82427=CARTESIAN_POINT('Ctrl Pts',(90.8733967486769,3.60900411009789,48.35));
#82428=CARTESIAN_POINT('Ctrl Pts',(91.050477379933,3.60900411009789,48.5));
#82429=CARTESIAN_POINT('Ctrl Pts',(91.050477379933,3.60900411009789,48.35));
#82430=CARTESIAN_POINT('Ctrl Pts',(91.1840382758528,3.5377217233181,48.5));
#82431=CARTESIAN_POINT('Ctrl Pts',(91.1840382758528,3.5377217233181,48.35));
#82432=CARTESIAN_POINT('',(90.8733967486769,3.60900411009789,48.5));
#82433=CARTESIAN_POINT('Ctrl Pts',(90.8733967486769,3.60900411009789,48.5));
#82434=CARTESIAN_POINT('Ctrl Pts',(91.050477379933,3.60900411009789,48.5));
#82435=CARTESIAN_POINT('Ctrl Pts',(91.1840382758528,3.5377217233181,48.5));
#82436=CARTESIAN_POINT('',(90.8733967486769,3.60900411009789,48.35));
#82437=CARTESIAN_POINT('',(90.8733967486769,3.60900411009789,48.5));
#82438=CARTESIAN_POINT('Ctrl Pts',(90.8733967486769,3.60900411009789,48.35));
#82439=CARTESIAN_POINT('Ctrl Pts',(91.050477379933,3.60900411009789,48.35));
#82440=CARTESIAN_POINT('Ctrl Pts',(91.1840382758528,3.5377217233181,48.35));
#82441=CARTESIAN_POINT('Ctrl Pts',(90.4749659243971,3.47994545102119,48.5));
#82442=CARTESIAN_POINT('Ctrl Pts',(90.4749659243971,3.47994545102119,48.35));
#82443=CARTESIAN_POINT('Ctrl Pts',(90.6332877818495,3.60900411009789,48.5));
#82444=CARTESIAN_POINT('Ctrl Pts',(90.6332877818495,3.60900411009789,48.35));
#82445=CARTESIAN_POINT('Ctrl Pts',(90.8733967486769,3.60900411009789,48.5));
#82446=CARTESIAN_POINT('Ctrl Pts',(90.8733967486769,3.60900411009789,48.35));
#82447=CARTESIAN_POINT('',(90.4749659243971,3.47994545102119,48.5));
#82448=CARTESIAN_POINT('Ctrl Pts',(90.4749659243971,3.47994545102119,48.5));
#82449=CARTESIAN_POINT('Ctrl Pts',(90.6332877818495,3.60900411009789,48.5));
#82450=CARTESIAN_POINT('Ctrl Pts',(90.8733967486769,3.60900411009789,48.5));
#82451=CARTESIAN_POINT('',(90.4749659243971,3.47994545102119,48.35));
#82452=CARTESIAN_POINT('',(90.4749659243971,3.47994545102119,48.5));
#82453=CARTESIAN_POINT('Ctrl Pts',(90.4749659243971,3.47994545102119,48.35));
#82454=CARTESIAN_POINT('Ctrl Pts',(90.6332877818495,3.60900411009789,48.35));
#82455=CARTESIAN_POINT('Ctrl Pts',(90.8733967486769,3.60900411009789,48.35));
#82456=CARTESIAN_POINT('Ctrl Pts',(90.2363572064787,3.11302864551544,48.5));
#82457=CARTESIAN_POINT('Ctrl Pts',(90.2363572064787,3.11302864551544,48.35));
#82458=CARTESIAN_POINT('Ctrl Pts',(90.3166437689215,3.3508867919445,48.5));
#82459=CARTESIAN_POINT('Ctrl Pts',(90.3166437689215,3.3508867919445,48.35));
#82460=CARTESIAN_POINT('Ctrl Pts',(90.4749659243971,3.47994545102119,48.5));
#82461=CARTESIAN_POINT('Ctrl Pts',(90.4749659243971,3.47994545102119,48.35));
#82462=CARTESIAN_POINT('',(90.2363572064787,3.11302864551544,48.5));
#82463=CARTESIAN_POINT('Ctrl Pts',(90.2363572064787,3.11302864551544,48.5));
#82464=CARTESIAN_POINT('Ctrl Pts',(90.3166437689215,3.3508867919445,48.5));
#82465=CARTESIAN_POINT('Ctrl Pts',(90.4749659243971,3.47994545102119,48.5));
#82466=CARTESIAN_POINT('',(90.2363572064787,3.11302864551544,48.35));
#82467=CARTESIAN_POINT('',(90.2363572064787,3.11302864551544,48.5));
#82468=CARTESIAN_POINT('Ctrl Pts',(90.2363572064787,3.11302864551544,48.35));
#82469=CARTESIAN_POINT('Ctrl Pts',(90.3166437689215,3.3508867919445,48.35));
#82470=CARTESIAN_POINT('Ctrl Pts',(90.4749659243971,3.47994545102119,48.35));
#82471=CARTESIAN_POINT('Ctrl Pts',(90.1560709420592,2.48499327898026,48.5));
#82472=CARTESIAN_POINT('Ctrl Pts',(90.1560709420592,2.48499327898026,48.35));
#82473=CARTESIAN_POINT('Ctrl Pts',(90.1560709420592,2.87517049908638,48.5));
#82474=CARTESIAN_POINT('Ctrl Pts',(90.1560709420592,2.87517049908638,48.35));
#82475=CARTESIAN_POINT('Ctrl Pts',(90.2363572064787,3.11302864551544,48.5));
#82476=CARTESIAN_POINT('Ctrl Pts',(90.2363572064787,3.11302864551544,48.35));
#82477=CARTESIAN_POINT('',(90.1560709420592,2.48499327898026,48.5));
#82478=CARTESIAN_POINT('Ctrl Pts',(90.1560709420592,2.48499327898026,48.5));
#82479=CARTESIAN_POINT('Ctrl Pts',(90.1560709420592,2.87517049908638,48.5));
#82480=CARTESIAN_POINT('Ctrl Pts',(90.2363572064787,3.11302864551544,48.5));
#82481=CARTESIAN_POINT('',(90.1560709420592,2.48499327898026,48.35));
#82482=CARTESIAN_POINT('',(90.1560709420592,2.48499327898026,48.5));
#82483=CARTESIAN_POINT('Ctrl Pts',(90.1560709420592,2.48499327898026,48.35));
#82484=CARTESIAN_POINT('Ctrl Pts',(90.1560709420592,2.87517049908638,48.35));
#82485=CARTESIAN_POINT('Ctrl Pts',(90.2363572064787,3.11302864551544,48.35));
#82486=CARTESIAN_POINT('Ctrl Pts',(90.3736696187407,1.59058684110642,48.5));
#82487=CARTESIAN_POINT('Ctrl Pts',(90.3736696187407,1.59058684110642,48.35));
#82488=CARTESIAN_POINT('Ctrl Pts',(90.1560709420592,1.86521166563034,48.5));
#82489=CARTESIAN_POINT('Ctrl Pts',(90.1560709420592,1.86521166563034,48.35));
#82490=CARTESIAN_POINT('Ctrl Pts',(90.1560709420592,2.48499327898026,48.5));
#82491=CARTESIAN_POINT('Ctrl Pts',(90.1560709420592,2.48499327898026,48.35));
#82492=CARTESIAN_POINT('Ctrl Pts',(90.3736696187407,1.59058684110642,48.5));
#82493=CARTESIAN_POINT('Ctrl Pts',(90.1560709420592,1.86521166563034,48.5));
#82494=CARTESIAN_POINT('Ctrl Pts',(90.1560709420592,2.48499327898026,48.5));
#82495=CARTESIAN_POINT('Ctrl Pts',(90.3736696187407,1.59058684110642,48.35));
#82496=CARTESIAN_POINT('Ctrl Pts',(90.1560709420592,1.86521166563034,48.35));
#82497=CARTESIAN_POINT('Ctrl Pts',(90.1560709420592,2.48499327898026,48.35));
#82498=CARTESIAN_POINT('Origin',(89.9999996814877,2.48574362695217,48.35));
#82499=CARTESIAN_POINT('Ctrl Pts',(88.9015006069094,1.80593454837799,48.5));
#82500=CARTESIAN_POINT('Ctrl Pts',(88.9015006069094,1.80593454837799,48.35));
#82501=CARTESIAN_POINT('Ctrl Pts',(88.8324691895396,1.73315161466599,48.5));
#82502=CARTESIAN_POINT('Ctrl Pts',(88.8324691895396,1.73315161466599,48.35));
#82503=CARTESIAN_POINT('Ctrl Pts',(88.7874487582594,1.65961825847626,48.5));
#82504=CARTESIAN_POINT('Ctrl Pts',(88.7874487582594,1.65961825847626,48.35));
#82505=CARTESIAN_POINT('',(88.9015006069094,1.80593454837799,48.5));
#82506=CARTESIAN_POINT('',(88.7874487582594,1.65961825847626,48.5));
#82507=CARTESIAN_POINT('Ctrl Pts',(88.9015006069094,1.80593454837799,48.5));
#82508=CARTESIAN_POINT('Ctrl Pts',(88.8324691895396,1.73315161466599,48.5));
#82509=CARTESIAN_POINT('Ctrl Pts',(88.7874487582594,1.65961825847626,48.5));
#82510=CARTESIAN_POINT('',(88.9015006069094,1.80593454837799,48.35));
#82511=CARTESIAN_POINT('',(88.9015006069094,1.80593454837799,48.5));
#82512=CARTESIAN_POINT('',(88.7874487582594,1.65961825847626,48.35));
#82513=CARTESIAN_POINT('Ctrl Pts',(88.9015006069094,1.80593454837799,48.35));
#82514=CARTESIAN_POINT('Ctrl Pts',(88.8324691895396,1.73315161466599,48.35));
#82515=CARTESIAN_POINT('Ctrl Pts',(88.7874487582594,1.65961825847626,48.35));
#82516=CARTESIAN_POINT('',(88.7874487582594,1.65961825847626,48.5));
#82517=CARTESIAN_POINT('Ctrl Pts',(89.2136425320059,2.08281049132347,48.5));
#82518=CARTESIAN_POINT('Ctrl Pts',(89.2136425320059,2.08281049132347,48.35));
#82519=CARTESIAN_POINT('Ctrl Pts',(88.9705318752676,1.87871778011322,48.5));
#82520=CARTESIAN_POINT('Ctrl Pts',(88.9705318752676,1.87871778011322,48.35));
#82521=CARTESIAN_POINT('Ctrl Pts',(88.9015006069094,1.80593454837799,48.5));
#82522=CARTESIAN_POINT('Ctrl Pts',(88.9015006069094,1.80593454837799,48.35));
#82523=CARTESIAN_POINT('',(89.2136425320059,2.08281049132347,48.5));
#82524=CARTESIAN_POINT('Ctrl Pts',(89.2136425320059,2.08281049132347,48.5));
#82525=CARTESIAN_POINT('Ctrl Pts',(88.9705318752676,1.87871778011322,48.5));
#82526=CARTESIAN_POINT('Ctrl Pts',(88.9015006069094,1.80593454837799,48.5));
#82527=CARTESIAN_POINT('',(89.2136425320059,2.08281049132347,48.35));
#82528=CARTESIAN_POINT('',(89.2136425320059,2.08281049132347,48.5));
#82529=CARTESIAN_POINT('Ctrl Pts',(89.2136425320059,2.08281049132347,48.35));
#82530=CARTESIAN_POINT('Ctrl Pts',(88.9705318752676,1.87871778011322,48.35));
#82531=CARTESIAN_POINT('Ctrl Pts',(88.9015006069094,1.80593454837799,48.35));
#82532=CARTESIAN_POINT('Ctrl Pts',(89.6300817076117,2.46998646855354,48.5));
#82533=CARTESIAN_POINT('Ctrl Pts',(89.6300817076117,2.46998646855354,48.35));
#82534=CARTESIAN_POINT('Ctrl Pts',(89.5047748629004,2.32892239093781,48.5));
#82535=CARTESIAN_POINT('Ctrl Pts',(89.5047748629004,2.32892239093781,48.35));
#82536=CARTESIAN_POINT('Ctrl Pts',(89.2136425320059,2.08281049132347,48.5));
#82537=CARTESIAN_POINT('Ctrl Pts',(89.2136425320059,2.08281049132347,48.35));
#82538=CARTESIAN_POINT('',(89.6300817076117,2.46998646855354,48.5));
#82539=CARTESIAN_POINT('Ctrl Pts',(89.6300817076117,2.46998646855354,48.5));
#82540=CARTESIAN_POINT('Ctrl Pts',(89.5047748629004,2.32892239093781,48.5));
#82541=CARTESIAN_POINT('Ctrl Pts',(89.2136425320059,2.08281049132347,48.5));
#82542=CARTESIAN_POINT('',(89.6300817076117,2.46998646855354,48.35));
#82543=CARTESIAN_POINT('',(89.6300817076117,2.46998646855354,48.5));
#82544=CARTESIAN_POINT('Ctrl Pts',(89.6300817076117,2.46998646855354,48.35));
#82545=CARTESIAN_POINT('Ctrl Pts',(89.5047748629004,2.32892239093781,48.35));
#82546=CARTESIAN_POINT('Ctrl Pts',(89.2136425320059,2.08281049132347,48.35));
#82547=CARTESIAN_POINT('Ctrl Pts',(89.8094133082777,2.73860850930214,48.5));
#82548=CARTESIAN_POINT('Ctrl Pts',(89.8094133082777,2.73860850930214,48.35));
#82549=CARTESIAN_POINT('Ctrl Pts',(89.7553888503462,2.61105054616928,48.5));
#82550=CARTESIAN_POINT('Ctrl Pts',(89.7553888503462,2.61105054616928,48.35));
#82551=CARTESIAN_POINT('Ctrl Pts',(89.6300817076117,2.46998646855354,48.5));
#82552=CARTESIAN_POINT('Ctrl Pts',(89.6300817076117,2.46998646855354,48.35));
#82553=CARTESIAN_POINT('',(89.8094133082777,2.73860850930214,48.5));
#82554=CARTESIAN_POINT('Ctrl Pts',(89.8094133082777,2.73860850930214,48.5));
#82555=CARTESIAN_POINT('Ctrl Pts',(89.7553888503462,2.61105054616928,48.5));
#82556=CARTESIAN_POINT('Ctrl Pts',(89.6300817076117,2.46998646855354,48.5));
#82557=CARTESIAN_POINT('',(89.8094133082777,2.73860850930214,48.35));
#82558=CARTESIAN_POINT('',(89.8094133082777,2.73860850930214,48.5));
#82559=CARTESIAN_POINT('Ctrl Pts',(89.8094133082777,2.73860850930214,48.35));
#82560=CARTESIAN_POINT('Ctrl Pts',(89.7553888503462,2.61105054616928,48.35));
#82561=CARTESIAN_POINT('Ctrl Pts',(89.6300817076117,2.46998646855354,48.35));
#82562=CARTESIAN_POINT('Ctrl Pts',(89.8634377662092,2.99822652339935,48.5));
#82563=CARTESIAN_POINT('Ctrl Pts',(89.8634377662092,2.99822652339935,48.35));
#82564=CARTESIAN_POINT('Ctrl Pts',(89.8634377662092,2.866166472435,48.5));
#82565=CARTESIAN_POINT('Ctrl Pts',(89.8634377662092,2.866166472435,48.35));
#82566=CARTESIAN_POINT('Ctrl Pts',(89.8094133082777,2.73860850930214,48.5));
#82567=CARTESIAN_POINT('Ctrl Pts',(89.8094133082777,2.73860850930214,48.35));
#82568=CARTESIAN_POINT('',(89.8634377662092,2.99822652339935,48.5));
#82569=CARTESIAN_POINT('Ctrl Pts',(89.8634377662092,2.99822652339935,48.5));
#82570=CARTESIAN_POINT('Ctrl Pts',(89.8634377662092,2.866166472435,48.5));
#82571=CARTESIAN_POINT('Ctrl Pts',(89.8094133082777,2.73860850930214,48.5));
#82572=CARTESIAN_POINT('',(89.8634377662092,2.99822652339935,48.35));
#82573=CARTESIAN_POINT('',(89.8634377662092,2.99822652339935,48.5));
#82574=CARTESIAN_POINT('Ctrl Pts',(89.8634377662092,2.99822652339935,48.35));
#82575=CARTESIAN_POINT('Ctrl Pts',(89.8634377662092,2.866166472435,48.35));
#82576=CARTESIAN_POINT('Ctrl Pts',(89.8094133082777,2.73860850930214,48.35));
#82577=CARTESIAN_POINT('Ctrl Pts',(89.6788541022688,3.43342432379723,48.5));
#82578=CARTESIAN_POINT('Ctrl Pts',(89.6788541022688,3.43342432379723,48.35));
#82579=CARTESIAN_POINT('Ctrl Pts',(89.8634377662092,3.25784453749657,48.5));
#82580=CARTESIAN_POINT('Ctrl Pts',(89.8634377662092,3.25784453749657,48.35));
#82581=CARTESIAN_POINT('Ctrl Pts',(89.8634377662092,2.99822652339935,48.5));
#82582=CARTESIAN_POINT('Ctrl Pts',(89.8634377662092,2.99822652339935,48.35));
#82583=CARTESIAN_POINT('',(89.6788541022688,3.43342432379723,48.5));
#82584=CARTESIAN_POINT('Ctrl Pts',(89.6788541022688,3.43342432379723,48.5));
#82585=CARTESIAN_POINT('Ctrl Pts',(89.8634377662092,3.25784453749657,48.5));
#82586=CARTESIAN_POINT('Ctrl Pts',(89.8634377662092,2.99822652339935,48.5));
#82587=CARTESIAN_POINT('',(89.6788541022688,3.43342432379723,48.35));
#82588=CARTESIAN_POINT('',(89.6788541022688,3.43342432379723,48.5));
#82589=CARTESIAN_POINT('Ctrl Pts',(89.6788541022688,3.43342432379723,48.35));
#82590=CARTESIAN_POINT('Ctrl Pts',(89.8634377662092,3.25784453749657,48.35));
#82591=CARTESIAN_POINT('Ctrl Pts',(89.8634377662092,2.99822652339935,48.35));
#82592=CARTESIAN_POINT('Ctrl Pts',(89.1776261273772,3.60900411009789,48.5));
#82593=CARTESIAN_POINT('Ctrl Pts',(89.1776261273772,3.60900411009789,48.35));
#82594=CARTESIAN_POINT('Ctrl Pts',(89.4942701403052,3.60900411009789,48.5));
#82595=CARTESIAN_POINT('Ctrl Pts',(89.4942701403052,3.60900411009789,48.35));
#82596=CARTESIAN_POINT('Ctrl Pts',(89.6788541022688,3.43342432379723,48.5));
#82597=CARTESIAN_POINT('Ctrl Pts',(89.6788541022688,3.43342432379723,48.35));
#82598=CARTESIAN_POINT('',(89.1776261273772,3.60900411009789,48.5));
#82599=CARTESIAN_POINT('Ctrl Pts',(89.1776261273772,3.60900411009789,48.5));
#82600=CARTESIAN_POINT('Ctrl Pts',(89.4942701403052,3.60900411009789,48.5));
#82601=CARTESIAN_POINT('Ctrl Pts',(89.6788541022688,3.43342432379723,48.5));
#82602=CARTESIAN_POINT('',(89.1776261273772,3.60900411009789,48.35));
#82603=CARTESIAN_POINT('',(89.1776261273772,3.60900411009789,48.5));
#82604=CARTESIAN_POINT('Ctrl Pts',(89.1776261273772,3.60900411009789,48.35));
#82605=CARTESIAN_POINT('Ctrl Pts',(89.4942701403052,3.60900411009789,48.35));
#82606=CARTESIAN_POINT('Ctrl Pts',(89.6788541022688,3.43342432379723,48.35));
#82607=CARTESIAN_POINT('Ctrl Pts',(88.6778989974409,3.446180164814,48.5));
#82608=CARTESIAN_POINT('Ctrl Pts',(88.6778989974409,3.446180164814,48.35));
#82609=CARTESIAN_POINT('Ctrl Pts',(88.8639835063368,3.60900411009789,48.5));
#82610=CARTESIAN_POINT('Ctrl Pts',(88.8639835063368,3.60900411009789,48.35));
#82611=CARTESIAN_POINT('Ctrl Pts',(89.1776261273772,3.60900411009789,48.5));
#82612=CARTESIAN_POINT('Ctrl Pts',(89.1776261273772,3.60900411009789,48.35));
#82613=CARTESIAN_POINT('',(88.6778989974409,3.446180164814,48.5));
#82614=CARTESIAN_POINT('Ctrl Pts',(88.6778989974409,3.446180164814,48.5));
#82615=CARTESIAN_POINT('Ctrl Pts',(88.8639835063368,3.60900411009789,48.5));
#82616=CARTESIAN_POINT('Ctrl Pts',(89.1776261273772,3.60900411009789,48.5));
#82617=CARTESIAN_POINT('',(88.6778989974409,3.446180164814,48.35));
#82618=CARTESIAN_POINT('',(88.6778989974409,3.446180164814,48.5));
#82619=CARTESIAN_POINT('Ctrl Pts',(88.6778989974409,3.446180164814,48.35));
#82620=CARTESIAN_POINT('Ctrl Pts',(88.8639835063368,3.60900411009789,48.35));
#82621=CARTESIAN_POINT('Ctrl Pts',(89.1776261273772,3.60900411009789,48.35));
#82622=CARTESIAN_POINT('Ctrl Pts',(88.4633014146239,2.97271499037743,48.5));
#82623=CARTESIAN_POINT('Ctrl Pts',(88.4633014146239,2.97271499037743,48.35));
#82624=CARTESIAN_POINT('Ctrl Pts',(88.4918143395334,3.28335621953011,48.5));
#82625=CARTESIAN_POINT('Ctrl Pts',(88.4918143395334,3.28335621953011,48.35));
#82626=CARTESIAN_POINT('Ctrl Pts',(88.6778989974409,3.446180164814,48.5));
#82627=CARTESIAN_POINT('Ctrl Pts',(88.6778989974409,3.446180164814,48.35));
#82628=CARTESIAN_POINT('',(88.4633014146239,2.97271499037743,48.5));
#82629=CARTESIAN_POINT('Ctrl Pts',(88.4633014146239,2.97271499037743,48.5));
#82630=CARTESIAN_POINT('Ctrl Pts',(88.4918143395334,3.28335621953011,48.5));
#82631=CARTESIAN_POINT('Ctrl Pts',(88.6778989974409,3.446180164814,48.5));
#82632=CARTESIAN_POINT('',(88.4633014146239,2.97271499037743,48.35));
#82633=CARTESIAN_POINT('',(88.4633014146239,2.97271499037743,48.5));
#82634=CARTESIAN_POINT('Ctrl Pts',(88.4633014146239,2.97271499037743,48.35));
#82635=CARTESIAN_POINT('Ctrl Pts',(88.4918143395334,3.28335621953011,48.35));
#82636=CARTESIAN_POINT('Ctrl Pts',(88.6778989974409,3.446180164814,48.35));
#82637=CARTESIAN_POINT('Origin',(88.7409276310354,2.94420206546783,48.5));
#82638=CARTESIAN_POINT('',(88.7409276310354,2.94420206546783,48.5));
#82639=CARTESIAN_POINT('',(44.5766785275039,7.47998378901591,48.5));
#82640=CARTESIAN_POINT('',(88.7409276310354,2.94420206546783,48.35));
#82641=CARTESIAN_POINT('',(88.7409276310354,2.94420206546783,48.5));
#82642=CARTESIAN_POINT('',(88.7409276310354,2.94420206546783,48.35));
#82643=CARTESIAN_POINT('Ctrl Pts',(88.8594815675169,3.26834926009178,48.5));
#82644=CARTESIAN_POINT('Ctrl Pts',(88.8594815675169,3.26834926009178,48.35));
#82645=CARTESIAN_POINT('Ctrl Pts',(88.7424283269793,3.15129616856575,48.5));
#82646=CARTESIAN_POINT('Ctrl Pts',(88.7424283269793,3.15129616856575,48.35));
#82647=CARTESIAN_POINT('Ctrl Pts',(88.7409276310354,2.94420206546783,48.5));
#82648=CARTESIAN_POINT('Ctrl Pts',(88.7409276310354,2.94420206546783,48.35));
#82649=CARTESIAN_POINT('',(88.8594815675169,3.26834926009178,48.5));
#82650=CARTESIAN_POINT('Ctrl Pts',(88.8594815675169,3.26834926009178,48.5));
#82651=CARTESIAN_POINT('Ctrl Pts',(88.7424283269793,3.15129616856575,48.5));
#82652=CARTESIAN_POINT('Ctrl Pts',(88.7409276310354,2.94420206546783,48.5));
#82653=CARTESIAN_POINT('',(88.8594815675169,3.26834926009178,48.35));
#82654=CARTESIAN_POINT('',(88.8594815675169,3.26834926009178,48.5));
#82655=CARTESIAN_POINT('Ctrl Pts',(88.8594815675169,3.26834926009178,48.35));
#82656=CARTESIAN_POINT('Ctrl Pts',(88.7424283269793,3.15129616856575,48.35));
#82657=CARTESIAN_POINT('Ctrl Pts',(88.7409276310354,2.94420206546783,48.35));
#82658=CARTESIAN_POINT('Ctrl Pts',(89.1716233436018,3.38540250062943,48.5));
#82659=CARTESIAN_POINT('Ctrl Pts',(89.1716233436018,3.38540250062943,48.35));
#82660=CARTESIAN_POINT('Ctrl Pts',(88.976534659043,3.38540250062943,48.5));
#82661=CARTESIAN_POINT('Ctrl Pts',(88.976534659043,3.38540250062943,48.35));
#82662=CARTESIAN_POINT('Ctrl Pts',(88.8594815675169,3.26834926009178,48.5));
#82663=CARTESIAN_POINT('Ctrl Pts',(88.8594815675169,3.26834926009178,48.35));
#82664=CARTESIAN_POINT('',(89.1716233436018,3.38540250062943,48.5));
#82665=CARTESIAN_POINT('Ctrl Pts',(89.1716233436018,3.38540250062943,48.5));
#82666=CARTESIAN_POINT('Ctrl Pts',(88.976534659043,3.38540250062943,48.5));
#82667=CARTESIAN_POINT('Ctrl Pts',(88.8594815675169,3.26834926009178,48.5));
#82668=CARTESIAN_POINT('',(89.1716233436018,3.38540250062943,48.35));
#82669=CARTESIAN_POINT('',(89.1716233436018,3.38540250062943,48.5));
#82670=CARTESIAN_POINT('Ctrl Pts',(89.1716233436018,3.38540250062943,48.35));
#82671=CARTESIAN_POINT('Ctrl Pts',(88.976534659043,3.38540250062943,48.35));
#82672=CARTESIAN_POINT('Ctrl Pts',(88.8594815675169,3.26834926009178,48.35));
#82673=CARTESIAN_POINT('Ctrl Pts',(89.4710094276816,3.27510246634483,48.5));
#82674=CARTESIAN_POINT('Ctrl Pts',(89.4710094276816,3.27510246634483,48.35));
#82675=CARTESIAN_POINT('Ctrl Pts',(89.3562073055655,3.38540250062943,48.5));
#82676=CARTESIAN_POINT('Ctrl Pts',(89.3562073055655,3.38540250062943,48.35));
#82677=CARTESIAN_POINT('Ctrl Pts',(89.1716233436018,3.38540250062943,48.5));
#82678=CARTESIAN_POINT('Ctrl Pts',(89.1716233436018,3.38540250062943,48.35));
#82679=CARTESIAN_POINT('',(89.4710094276816,3.27510246634483,48.5));
#82680=CARTESIAN_POINT('Ctrl Pts',(89.4710094276816,3.27510246634483,48.5));
#82681=CARTESIAN_POINT('Ctrl Pts',(89.3562073055655,3.38540250062943,48.5));
#82682=CARTESIAN_POINT('Ctrl Pts',(89.1716233436018,3.38540250062943,48.5));
#82683=CARTESIAN_POINT('',(89.4710094276816,3.27510246634483,48.35));
#82684=CARTESIAN_POINT('',(89.4710094276816,3.27510246634483,48.5));
#82685=CARTESIAN_POINT('Ctrl Pts',(89.4710094276816,3.27510246634483,48.35));
#82686=CARTESIAN_POINT('Ctrl Pts',(89.3562073055655,3.38540250062943,48.35));
#82687=CARTESIAN_POINT('Ctrl Pts',(89.1716233436018,3.38540250062943,48.35));
#82688=CARTESIAN_POINT('Ctrl Pts',(89.5858118478209,3.00422930717468,48.5));
#82689=CARTESIAN_POINT('Ctrl Pts',(89.5858118478209,3.00422930717468,48.35));
#82690=CARTESIAN_POINT('Ctrl Pts',(89.5858118478209,3.16480228304863,48.5));
#82691=CARTESIAN_POINT('Ctrl Pts',(89.5858118478209,3.16480228304863,48.35));
#82692=CARTESIAN_POINT('Ctrl Pts',(89.4710094276816,3.27510246634483,48.5));
#82693=CARTESIAN_POINT('Ctrl Pts',(89.4710094276816,3.27510246634483,48.35));
#82694=CARTESIAN_POINT('',(89.5858118478209,3.00422930717468,48.5));
#82695=CARTESIAN_POINT('Ctrl Pts',(89.5858118478209,3.00422930717468,48.5));
#82696=CARTESIAN_POINT('Ctrl Pts',(89.5858118478209,3.16480228304863,48.5));
#82697=CARTESIAN_POINT('Ctrl Pts',(89.4710094276816,3.27510246634483,48.5));
#82698=CARTESIAN_POINT('',(89.5858118478209,3.00422930717468,48.35));
#82699=CARTESIAN_POINT('',(89.5858118478209,3.00422930717468,48.5));
#82700=CARTESIAN_POINT('Ctrl Pts',(89.5858118478209,3.00422930717468,48.35));
#82701=CARTESIAN_POINT('Ctrl Pts',(89.5858118478209,3.16480228304863,48.35));
#82702=CARTESIAN_POINT('Ctrl Pts',(89.4710094276816,3.27510246634483,48.35));
#82703=CARTESIAN_POINT('Ctrl Pts',(89.4597542826086,2.6793315410614,48.5));
#82704=CARTESIAN_POINT('Ctrl Pts',(89.4597542826086,2.6793315410614,48.35));
#82705=CARTESIAN_POINT('Ctrl Pts',(89.5858118478209,2.85115966200829,48.5));
#82706=CARTESIAN_POINT('Ctrl Pts',(89.5858118478209,2.85115966200829,48.35));
#82707=CARTESIAN_POINT('Ctrl Pts',(89.5858118478209,3.00422930717468,48.5));
#82708=CARTESIAN_POINT('Ctrl Pts',(89.5858118478209,3.00422930717468,48.35));
#82709=CARTESIAN_POINT('',(89.4597542826086,2.6793315410614,48.5));
#82710=CARTESIAN_POINT('Ctrl Pts',(89.4597542826086,2.6793315410614,48.5));
#82711=CARTESIAN_POINT('Ctrl Pts',(89.5858118478209,2.85115966200829,48.5));
#82712=CARTESIAN_POINT('Ctrl Pts',(89.5858118478209,3.00422930717468,48.5));
#82713=CARTESIAN_POINT('',(89.4597542826086,2.6793315410614,48.35));
#82714=CARTESIAN_POINT('',(89.4597542826086,2.6793315410614,48.5));
#82715=CARTESIAN_POINT('Ctrl Pts',(89.4597542826086,2.6793315410614,48.35));
#82716=CARTESIAN_POINT('Ctrl Pts',(89.5858118478209,2.85115966200829,48.35));
#82717=CARTESIAN_POINT('Ctrl Pts',(89.5858118478209,3.00422930717468,48.35));
#82718=CARTESIAN_POINT('Ctrl Pts',(88.9750341121107,2.21336984634399,48.5));
#82719=CARTESIAN_POINT('Ctrl Pts',(88.9750341121107,2.21336984634399,48.35));
#82720=CARTESIAN_POINT('Ctrl Pts',(89.3336970154196,2.50750356912613,48.5));
#82721=CARTESIAN_POINT('Ctrl Pts',(89.3336970154196,2.50750356912613,48.35));
#82722=CARTESIAN_POINT('Ctrl Pts',(89.4597542826086,2.6793315410614,48.5));
#82723=CARTESIAN_POINT('Ctrl Pts',(89.4597542826086,2.6793315410614,48.35));
#82724=CARTESIAN_POINT('',(88.9750341121107,2.21336984634399,48.5));
#82725=CARTESIAN_POINT('Ctrl Pts',(88.9750341121107,2.21336984634399,48.5));
#82726=CARTESIAN_POINT('Ctrl Pts',(89.3336970154196,2.50750356912613,48.5));
#82727=CARTESIAN_POINT('Ctrl Pts',(89.4597542826086,2.6793315410614,48.5));
#82728=CARTESIAN_POINT('',(88.9750341121107,2.21336984634399,48.35));
#82729=CARTESIAN_POINT('',(88.9750341121107,2.21336984634399,48.5));
#82730=CARTESIAN_POINT('Ctrl Pts',(88.9750341121107,2.21336984634399,48.35));
#82731=CARTESIAN_POINT('Ctrl Pts',(89.3336970154196,2.50750356912613,48.35));
#82732=CARTESIAN_POINT('Ctrl Pts',(89.4597542826086,2.6793315410614,48.35));
#82733=CARTESIAN_POINT('Ctrl Pts',(88.6216234210879,1.88021832704544,48.5));
#82734=CARTESIAN_POINT('Ctrl Pts',(88.6216234210879,1.88021832704544,48.35));
#82735=CARTESIAN_POINT('Ctrl Pts',(88.7439290229231,2.02428394556046,48.5));
#82736=CARTESIAN_POINT('Ctrl Pts',(88.7439290229231,2.02428394556046,48.35));
#82737=CARTESIAN_POINT('Ctrl Pts',(88.9750341121107,2.21336984634399,48.5));
#82738=CARTESIAN_POINT('Ctrl Pts',(88.9750341121107,2.21336984634399,48.35));
#82739=CARTESIAN_POINT('',(88.6216234210879,1.88021832704544,48.5));
#82740=CARTESIAN_POINT('Ctrl Pts',(88.6216234210879,1.88021832704544,48.5));
#82741=CARTESIAN_POINT('Ctrl Pts',(88.7439290229231,2.02428394556046,48.5));
#82742=CARTESIAN_POINT('Ctrl Pts',(88.9750341121107,2.21336984634399,48.5));
#82743=CARTESIAN_POINT('',(88.6216234210879,1.88021832704544,48.35));
#82744=CARTESIAN_POINT('',(88.6216234210879,1.88021832704544,48.5));
#82745=CARTESIAN_POINT('Ctrl Pts',(88.6216234210879,1.88021832704544,48.35));
#82746=CARTESIAN_POINT('Ctrl Pts',(88.7439290229231,2.02428394556046,48.35));
#82747=CARTESIAN_POINT('Ctrl Pts',(88.9750341121107,2.21336984634399,48.35));
#82748=CARTESIAN_POINT('Ctrl Pts',(88.4437925163656,1.58758544921875,48.5));
#82749=CARTESIAN_POINT('Ctrl Pts',(88.4437925163656,1.58758544921875,48.35));
#82750=CARTESIAN_POINT('Ctrl Pts',(88.4993178192526,1.73615300655365,48.5));
#82751=CARTESIAN_POINT('Ctrl Pts',(88.4993178192526,1.73615300655365,48.35));
#82752=CARTESIAN_POINT('Ctrl Pts',(88.6216234210879,1.88021832704544,48.5));
#82753=CARTESIAN_POINT('Ctrl Pts',(88.6216234210879,1.88021832704544,48.35));
#82754=CARTESIAN_POINT('',(88.4437925163656,1.58758544921875,48.5));
#82755=CARTESIAN_POINT('Ctrl Pts',(88.4437925163656,1.58758544921875,48.5));
#82756=CARTESIAN_POINT('Ctrl Pts',(88.4993178192526,1.73615300655365,48.5));
#82757=CARTESIAN_POINT('Ctrl Pts',(88.6216234210879,1.88021832704544,48.5));
#82758=CARTESIAN_POINT('',(88.4437925163656,1.58758544921875,48.35));
#82759=CARTESIAN_POINT('',(88.4437925163656,1.58758544921875,48.5));
#82760=CARTESIAN_POINT('Ctrl Pts',(88.4437925163656,1.58758544921875,48.35));
#82761=CARTESIAN_POINT('Ctrl Pts',(88.4993178192526,1.73615300655365,48.35));
#82762=CARTESIAN_POINT('Ctrl Pts',(88.6216234210879,1.88021832704544,48.35));
#82763=CARTESIAN_POINT('Ctrl Pts',(88.4122781995684,1.40000009536743,48.5));
#82764=CARTESIAN_POINT('Ctrl Pts',(88.4122781995684,1.40000009536743,48.35));
#82765=CARTESIAN_POINT('Ctrl Pts',(88.4092768076807,1.49754428863525,48.5));
#82766=CARTESIAN_POINT('Ctrl Pts',(88.4092768076807,1.49754428863525,48.35));
#82767=CARTESIAN_POINT('Ctrl Pts',(88.4437925163656,1.58758544921875,48.5));
#82768=CARTESIAN_POINT('Ctrl Pts',(88.4437925163656,1.58758544921875,48.35));
#82769=CARTESIAN_POINT('',(88.4122781995684,1.40000009536743,48.5));
#82770=CARTESIAN_POINT('Ctrl Pts',(88.4122781995684,1.40000009536743,48.5));
#82771=CARTESIAN_POINT('Ctrl Pts',(88.4092768076807,1.49754428863525,48.5));
#82772=CARTESIAN_POINT('Ctrl Pts',(88.4437925163656,1.58758544921875,48.5));
#82773=CARTESIAN_POINT('',(88.4122781995684,1.40000009536743,48.35));
#82774=CARTESIAN_POINT('',(88.4122781995684,1.40000009536743,48.5));
#82775=CARTESIAN_POINT('Ctrl Pts',(88.4122781995684,1.40000009536743,48.35));
#82776=CARTESIAN_POINT('Ctrl Pts',(88.4092768076807,1.49754428863525,48.35));
#82777=CARTESIAN_POINT('Ctrl Pts',(88.4437925163656,1.58758544921875,48.35));
#82778=CARTESIAN_POINT('Origin',(89.8664391580969,1.40000009536743,48.5));
#82779=CARTESIAN_POINT('',(89.8664391580969,1.40000009536743,48.5));
#82780=CARTESIAN_POINT('',(44.9332195790485,1.40000009536743,48.5));
#82781=CARTESIAN_POINT('',(89.8664391580969,1.40000009536743,48.35));
#82782=CARTESIAN_POINT('',(89.8664391580969,1.40000009536743,48.5));
#82783=CARTESIAN_POINT('',(89.8664391580969,1.40000009536743,48.35));
#82784=CARTESIAN_POINT('Origin',(89.8664391580969,1.65961825847626,48.5));
#82785=CARTESIAN_POINT('',(89.8664391580969,1.65961825847626,48.5));
#82786=CARTESIAN_POINT('',(89.8664391580969,4.82980912923813,48.5));
#82787=CARTESIAN_POINT('',(89.8664391580969,1.65961825847626,48.35));
#82788=CARTESIAN_POINT('',(89.8664391580969,1.65961825847626,48.5));
#82789=CARTESIAN_POINT('',(89.8664391580969,1.65961825847626,48.35));
#82790=CARTESIAN_POINT('Origin',(88.7874487582594,1.65961825847626,48.5));
#82791=CARTESIAN_POINT('',(44.3937243791297,1.65961825847626,48.5));
#82792=CARTESIAN_POINT('',(88.7874487582594,1.65961825847626,48.35));
#82793=CARTESIAN_POINT('Origin',(89.9999996814877,2.48574362695217,48.35));
#82794=CARTESIAN_POINT('Origin',(0.,8.,48.5));
#82795=CARTESIAN_POINT('Ctrl Pts',(80.8508865237236,3.38540250062943,48.5));
#82796=CARTESIAN_POINT('Ctrl Pts',(80.8508865237236,3.38540250062943,48.35));
#82797=CARTESIAN_POINT('Ctrl Pts',(80.6648020148277,3.38540250062943,48.5));
#82798=CARTESIAN_POINT('Ctrl Pts',(80.6648020148277,3.38540250062943,48.35));
#82799=CARTESIAN_POINT('Ctrl Pts',(80.5537514090538,3.22783091664314,48.5));
#82800=CARTESIAN_POINT('Ctrl Pts',(80.5537514090538,3.22783091664314,48.35));
#82801=CARTESIAN_POINT('',(80.8508865237236,3.38540250062943,48.5));
#82802=CARTESIAN_POINT('',(80.5537514090538,3.22783091664314,48.5));
#82803=CARTESIAN_POINT('Ctrl Pts',(80.8508865237236,3.38540250062943,48.5));
#82804=CARTESIAN_POINT('Ctrl Pts',(80.6648020148277,3.38540250062943,48.5));
#82805=CARTESIAN_POINT('Ctrl Pts',(80.5537514090538,3.22783091664314,48.5));
#82806=CARTESIAN_POINT('',(80.8508865237236,3.38540250062943,48.35));
#82807=CARTESIAN_POINT('',(80.8508865237236,3.38540250062943,48.5));
#82808=CARTESIAN_POINT('',(80.5537514090538,3.22783091664314,48.35));
#82809=CARTESIAN_POINT('Ctrl Pts',(80.8508865237236,3.38540250062943,48.35));
#82810=CARTESIAN_POINT('Ctrl Pts',(80.6648020148277,3.38540250062943,48.35));
#82811=CARTESIAN_POINT('Ctrl Pts',(80.5537514090538,3.22783091664314,48.35));
#82812=CARTESIAN_POINT('',(80.5537514090538,3.22783091664314,48.5));
#82813=CARTESIAN_POINT('Ctrl Pts',(81.1667804121971,3.2068213224411,48.5));
#82814=CARTESIAN_POINT('Ctrl Pts',(81.1667804121971,3.2068213224411,48.35));
#82815=CARTESIAN_POINT('Ctrl Pts',(81.0399727225304,3.38540250062943,48.5));
#82816=CARTESIAN_POINT('Ctrl Pts',(81.0399727225304,3.38540250062943,48.35));
#82817=CARTESIAN_POINT('Ctrl Pts',(80.8508865237236,3.38540250062943,48.5));
#82818=CARTESIAN_POINT('Ctrl Pts',(80.8508865237236,3.38540250062943,48.35));
#82819=CARTESIAN_POINT('',(81.1667804121971,3.2068213224411,48.5));
#82820=CARTESIAN_POINT('Ctrl Pts',(81.1667804121971,3.2068213224411,48.5));
#82821=CARTESIAN_POINT('Ctrl Pts',(81.0399727225304,3.38540250062943,48.5));
#82822=CARTESIAN_POINT('Ctrl Pts',(80.8508865237236,3.38540250062943,48.5));
#82823=CARTESIAN_POINT('',(81.1667804121971,3.2068213224411,48.35));
#82824=CARTESIAN_POINT('',(81.1667804121971,3.2068213224411,48.5));
#82825=CARTESIAN_POINT('Ctrl Pts',(81.1667804121971,3.2068213224411,48.35));
#82826=CARTESIAN_POINT('Ctrl Pts',(81.0399727225304,3.38540250062943,48.35));
#82827=CARTESIAN_POINT('Ctrl Pts',(80.8508865237236,3.38540250062943,48.35));
#82828=CARTESIAN_POINT('Ctrl Pts',(81.2935881018639,2.48499327898026,48.5));
#82829=CARTESIAN_POINT('Ctrl Pts',(81.2935881018639,2.48499327898026,48.35));
#82830=CARTESIAN_POINT('Ctrl Pts',(81.2935881018639,3.02824014425278,48.5));
#82831=CARTESIAN_POINT('Ctrl Pts',(81.2935881018639,3.02824014425278,48.35));
#82832=CARTESIAN_POINT('Ctrl Pts',(81.1667804121971,3.2068213224411,48.5));
#82833=CARTESIAN_POINT('Ctrl Pts',(81.1667804121971,3.2068213224411,48.35));
#82834=CARTESIAN_POINT('',(81.2935881018639,2.48499327898026,48.5));
#82835=CARTESIAN_POINT('Ctrl Pts',(81.2935881018639,2.48499327898026,48.5));
#82836=CARTESIAN_POINT('Ctrl Pts',(81.2935881018639,3.02824014425278,48.5));
#82837=CARTESIAN_POINT('Ctrl Pts',(81.1667804121971,3.2068213224411,48.5));
#82838=CARTESIAN_POINT('',(81.2935881018639,2.48499327898026,48.35));
#82839=CARTESIAN_POINT('',(81.2935881018639,2.48499327898026,48.5));
#82840=CARTESIAN_POINT('Ctrl Pts',(81.2935881018639,2.48499327898026,48.35));
#82841=CARTESIAN_POINT('Ctrl Pts',(81.2935881018639,3.02824014425278,48.35));
#82842=CARTESIAN_POINT('Ctrl Pts',(81.1667804121971,3.2068213224411,48.35));
#82843=CARTESIAN_POINT('Ctrl Pts',(81.1667804121971,1.76466578245163,48.5));
#82844=CARTESIAN_POINT('Ctrl Pts',(81.1667804121971,1.76466578245163,48.35));
#82845=CARTESIAN_POINT('Ctrl Pts',(81.2935881018639,1.9447478055954,48.5));
#82846=CARTESIAN_POINT('Ctrl Pts',(81.2935881018639,1.9447478055954,48.35));
#82847=CARTESIAN_POINT('Ctrl Pts',(81.2935881018639,2.48499327898026,48.5));
#82848=CARTESIAN_POINT('Ctrl Pts',(81.2935881018639,2.48499327898026,48.35));
#82849=CARTESIAN_POINT('',(81.1667804121971,1.76466578245163,48.5));
#82850=CARTESIAN_POINT('Ctrl Pts',(81.1667804121971,1.76466578245163,48.5));
#82851=CARTESIAN_POINT('Ctrl Pts',(81.2935881018639,1.9447478055954,48.5));
#82852=CARTESIAN_POINT('Ctrl Pts',(81.2935881018639,2.48499327898026,48.5));
#82853=CARTESIAN_POINT('',(81.1667804121971,1.76466578245163,48.35));
#82854=CARTESIAN_POINT('',(81.1667804121971,1.76466578245163,48.5));
#82855=CARTESIAN_POINT('Ctrl Pts',(81.1667804121971,1.76466578245163,48.35));
#82856=CARTESIAN_POINT('Ctrl Pts',(81.2935881018639,1.9447478055954,48.35));
#82857=CARTESIAN_POINT('Ctrl Pts',(81.2935881018639,2.48499327898026,48.35));
#82858=CARTESIAN_POINT('Ctrl Pts',(80.8538882136345,1.58458405733109,48.5));
#82859=CARTESIAN_POINT('Ctrl Pts',(80.8538882136345,1.58458405733109,48.35));
#82860=CARTESIAN_POINT('Ctrl Pts',(81.0399727225304,1.58458405733109,48.5));
#82861=CARTESIAN_POINT('Ctrl Pts',(81.0399727225304,1.58458405733109,48.35));
#82862=CARTESIAN_POINT('Ctrl Pts',(81.1667804121971,1.76466578245163,48.5));
#82863=CARTESIAN_POINT('Ctrl Pts',(81.1667804121971,1.76466578245163,48.35));
#82864=CARTESIAN_POINT('',(80.8538882136345,1.58458405733109,48.5));
#82865=CARTESIAN_POINT('Ctrl Pts',(80.8538882136345,1.58458405733109,48.5));
#82866=CARTESIAN_POINT('Ctrl Pts',(81.0399727225304,1.58458405733109,48.5));
#82867=CARTESIAN_POINT('Ctrl Pts',(81.1667804121971,1.76466578245163,48.5));
#82868=CARTESIAN_POINT('',(80.8538882136345,1.58458405733109,48.35));
#82869=CARTESIAN_POINT('',(80.8538882136345,1.58458405733109,48.5));
#82870=CARTESIAN_POINT('Ctrl Pts',(80.8538882136345,1.58458405733109,48.35));
#82871=CARTESIAN_POINT('Ctrl Pts',(81.0399727225304,1.58458405733109,48.35));
#82872=CARTESIAN_POINT('Ctrl Pts',(81.1667804121971,1.76466578245163,48.35));
#82873=CARTESIAN_POINT('Ctrl Pts',(80.5409960150719,1.76391565799713,48.5));
#82874=CARTESIAN_POINT('Ctrl Pts',(80.5409960150719,1.76391565799713,48.35));
#82875=CARTESIAN_POINT('Ctrl Pts',(80.6678034067154,1.58458405733109,48.5));
#82876=CARTESIAN_POINT('Ctrl Pts',(80.6678034067154,1.58458405733109,48.35));
#82877=CARTESIAN_POINT('Ctrl Pts',(80.8538882136345,1.58458405733109,48.5));
#82878=CARTESIAN_POINT('Ctrl Pts',(80.8538882136345,1.58458405733109,48.35));
#82879=CARTESIAN_POINT('',(80.5409960150719,1.76391565799713,48.5));
#82880=CARTESIAN_POINT('Ctrl Pts',(80.5409960150719,1.76391565799713,48.5));
#82881=CARTESIAN_POINT('Ctrl Pts',(80.6678034067154,1.58458405733109,48.5));
#82882=CARTESIAN_POINT('Ctrl Pts',(80.8538882136345,1.58458405733109,48.5));
#82883=CARTESIAN_POINT('',(80.5409960150719,1.76391565799713,48.35));
#82884=CARTESIAN_POINT('',(80.5409960150719,1.76391565799713,48.5));
#82885=CARTESIAN_POINT('Ctrl Pts',(80.5409960150719,1.76391565799713,48.35));
#82886=CARTESIAN_POINT('Ctrl Pts',(80.6678034067154,1.58458405733109,48.35));
#82887=CARTESIAN_POINT('Ctrl Pts',(80.8538882136345,1.58458405733109,48.35));
#82888=CARTESIAN_POINT('Ctrl Pts',(80.4141883254051,2.48499327898026,48.5));
#82889=CARTESIAN_POINT('Ctrl Pts',(80.4141883254051,2.48499327898026,48.35));
#82890=CARTESIAN_POINT('Ctrl Pts',(80.4141883254051,1.94324696063995,48.5));
#82891=CARTESIAN_POINT('Ctrl Pts',(80.4141883254051,1.94324696063995,48.35));
#82892=CARTESIAN_POINT('Ctrl Pts',(80.5409960150719,1.76391565799713,48.5));
#82893=CARTESIAN_POINT('Ctrl Pts',(80.5409960150719,1.76391565799713,48.35));
#82894=CARTESIAN_POINT('',(80.4141883254051,2.48499327898026,48.5));
#82895=CARTESIAN_POINT('Ctrl Pts',(80.4141883254051,2.48499327898026,48.5));
#82896=CARTESIAN_POINT('Ctrl Pts',(80.4141883254051,1.94324696063995,48.5));
#82897=CARTESIAN_POINT('Ctrl Pts',(80.5409960150719,1.76391565799713,48.5));
#82898=CARTESIAN_POINT('',(80.4141883254051,2.48499327898026,48.35));
#82899=CARTESIAN_POINT('',(80.4141883254051,2.48499327898026,48.5));
#82900=CARTESIAN_POINT('Ctrl Pts',(80.4141883254051,2.48499327898026,48.35));
#82901=CARTESIAN_POINT('Ctrl Pts',(80.4141883254051,1.94324696063995,48.35));
#82902=CARTESIAN_POINT('Ctrl Pts',(80.5409960150719,1.76391565799713,48.35));
#82903=CARTESIAN_POINT('Ctrl Pts',(80.5537514090538,3.22783091664314,48.5));
#82904=CARTESIAN_POINT('Ctrl Pts',(80.5537514090538,3.22783091664314,48.35));
#82905=CARTESIAN_POINT('Ctrl Pts',(80.4141883254051,3.02673944830894,48.5));
#82906=CARTESIAN_POINT('Ctrl Pts',(80.4141883254051,3.02673944830894,48.35));
#82907=CARTESIAN_POINT('Ctrl Pts',(80.4141883254051,2.48499327898026,48.5));
#82908=CARTESIAN_POINT('Ctrl Pts',(80.4141883254051,2.48499327898026,48.35));
#82909=CARTESIAN_POINT('Ctrl Pts',(80.5537514090538,3.22783091664314,48.5));
#82910=CARTESIAN_POINT('Ctrl Pts',(80.4141883254051,3.02673944830894,48.5));
#82911=CARTESIAN_POINT('Ctrl Pts',(80.4141883254051,2.48499327898026,48.5));
#82912=CARTESIAN_POINT('Ctrl Pts',(80.5537514090538,3.22783091664314,48.35));
#82913=CARTESIAN_POINT('Ctrl Pts',(80.4141883254051,3.02673944830894,48.35));
#82914=CARTESIAN_POINT('Ctrl Pts',(80.4141883254051,2.48499327898026,48.35));
#82915=CARTESIAN_POINT('Ctrl Pts',(80.8538882136345,1.36248314380646,48.5));
#82916=CARTESIAN_POINT('Ctrl Pts',(80.8538882136345,1.36248314380646,48.35));
#82917=CARTESIAN_POINT('Ctrl Pts',(80.535743355751,1.36248314380646,48.5));
#82918=CARTESIAN_POINT('Ctrl Pts',(80.535743355751,1.36248314380646,48.35));
#82919=CARTESIAN_POINT('Ctrl Pts',(80.3541610836983,1.59058684110642,48.5));
#82920=CARTESIAN_POINT('Ctrl Pts',(80.3541610836983,1.59058684110642,48.35));
#82921=CARTESIAN_POINT('',(80.8538882136345,1.36248314380646,48.5));
#82922=CARTESIAN_POINT('',(80.3541610836983,1.59058684110642,48.5));
#82923=CARTESIAN_POINT('Ctrl Pts',(80.8538882136345,1.36248314380646,48.5));
#82924=CARTESIAN_POINT('Ctrl Pts',(80.535743355751,1.36248314380646,48.5));
#82925=CARTESIAN_POINT('Ctrl Pts',(80.3541610836983,1.59058684110642,48.5));
#82926=CARTESIAN_POINT('',(80.8538882136345,1.36248314380646,48.35));
#82927=CARTESIAN_POINT('',(80.8538882136345,1.36248314380646,48.5));
#82928=CARTESIAN_POINT('',(80.3541610836983,1.59058684110642,48.35));
#82929=CARTESIAN_POINT('Ctrl Pts',(80.8538882136345,1.36248314380646,48.35));
#82930=CARTESIAN_POINT('Ctrl Pts',(80.535743355751,1.36248314380646,48.35));
#82931=CARTESIAN_POINT('Ctrl Pts',(80.3541610836983,1.59058684110642,48.35));
#82932=CARTESIAN_POINT('',(80.3541610836983,1.59058684110642,48.5));
#82933=CARTESIAN_POINT('Ctrl Pts',(81.2538198828697,1.49229192733765,48.5));
#82934=CARTESIAN_POINT('Ctrl Pts',(81.2538198828697,1.49229192733765,48.35));
#82935=CARTESIAN_POINT('Ctrl Pts',(81.0954980254173,1.36248314380646,48.5));
#82936=CARTESIAN_POINT('Ctrl Pts',(81.0954980254173,1.36248314380646,48.35));
#82937=CARTESIAN_POINT('Ctrl Pts',(80.8538882136345,1.36248314380646,48.5));
#82938=CARTESIAN_POINT('Ctrl Pts',(80.8538882136345,1.36248314380646,48.35));
#82939=CARTESIAN_POINT('',(81.2538198828697,1.49229192733765,48.5));
#82940=CARTESIAN_POINT('Ctrl Pts',(81.2538198828697,1.49229192733765,48.5));
#82941=CARTESIAN_POINT('Ctrl Pts',(81.0954980254173,1.36248314380646,48.5));
#82942=CARTESIAN_POINT('Ctrl Pts',(80.8538882136345,1.36248314380646,48.5));
#82943=CARTESIAN_POINT('',(81.2538198828697,1.49229192733765,48.35));
#82944=CARTESIAN_POINT('',(81.2538198828697,1.49229192733765,48.5));
#82945=CARTESIAN_POINT('Ctrl Pts',(81.2538198828697,1.49229192733765,48.35));
#82946=CARTESIAN_POINT('Ctrl Pts',(81.0954980254173,1.36248314380646,48.35));
#82947=CARTESIAN_POINT('Ctrl Pts',(80.8538882136345,1.36248314380646,48.35));
#82948=CARTESIAN_POINT('Ctrl Pts',(81.4916781783104,1.85995900630951,48.5));
#82949=CARTESIAN_POINT('Ctrl Pts',(81.4916781783104,1.85995900630951,48.35));
#82950=CARTESIAN_POINT('Ctrl Pts',(81.4121417403221,1.62210100889206,48.5));
#82951=CARTESIAN_POINT('Ctrl Pts',(81.4121417403221,1.62210100889206,48.35));
#82952=CARTESIAN_POINT('Ctrl Pts',(81.2538198828697,1.49229192733765,48.5));
#82953=CARTESIAN_POINT('Ctrl Pts',(81.2538198828697,1.49229192733765,48.35));
#82954=CARTESIAN_POINT('',(81.4916781783104,1.85995900630951,48.5));
#82955=CARTESIAN_POINT('Ctrl Pts',(81.4916781783104,1.85995900630951,48.5));
#82956=CARTESIAN_POINT('Ctrl Pts',(81.4121417403221,1.62210100889206,48.5));
#82957=CARTESIAN_POINT('Ctrl Pts',(81.2538198828697,1.49229192733765,48.5));
#82958=CARTESIAN_POINT('',(81.4916781783104,1.85995900630951,48.35));
#82959=CARTESIAN_POINT('',(81.4916781783104,1.85995900630951,48.5));
#82960=CARTESIAN_POINT('Ctrl Pts',(81.4916781783104,1.85995900630951,48.35));
#82961=CARTESIAN_POINT('Ctrl Pts',(81.4121417403221,1.62210100889206,48.35));
#82962=CARTESIAN_POINT('Ctrl Pts',(81.2538198828697,1.49229192733765,48.35));
#82963=CARTESIAN_POINT('Ctrl Pts',(81.5712140202522,2.48499327898026,48.5));
#82964=CARTESIAN_POINT('Ctrl Pts',(81.5712140202522,2.48499327898026,48.35));
#82965=CARTESIAN_POINT('Ctrl Pts',(81.5712140202522,2.09781730175018,48.5));
#82966=CARTESIAN_POINT('Ctrl Pts',(81.5712140202522,2.09781730175018,48.35));
#82967=CARTESIAN_POINT('Ctrl Pts',(81.4916781783104,1.85995900630951,48.5));
#82968=CARTESIAN_POINT('Ctrl Pts',(81.4916781783104,1.85995900630951,48.35));
#82969=CARTESIAN_POINT('',(81.5712140202522,2.48499327898026,48.5));
#82970=CARTESIAN_POINT('Ctrl Pts',(81.5712140202522,2.48499327898026,48.5));
#82971=CARTESIAN_POINT('Ctrl Pts',(81.5712140202522,2.09781730175018,48.5));
#82972=CARTESIAN_POINT('Ctrl Pts',(81.4916781783104,1.85995900630951,48.5));
#82973=CARTESIAN_POINT('',(81.5712140202522,2.48499327898026,48.35));
#82974=CARTESIAN_POINT('',(81.5712140202522,2.48499327898026,48.5));
#82975=CARTESIAN_POINT('Ctrl Pts',(81.5712140202522,2.48499327898026,48.35));
#82976=CARTESIAN_POINT('Ctrl Pts',(81.5712140202522,2.09781730175018,48.35));
#82977=CARTESIAN_POINT('Ctrl Pts',(81.4916781783104,1.85995900630951,48.35));
#82978=CARTESIAN_POINT('Ctrl Pts',(81.5216915011406,3.00497958064079,48.5));
#82979=CARTESIAN_POINT('Ctrl Pts',(81.5216915011406,3.00497958064079,48.35));
#82980=CARTESIAN_POINT('Ctrl Pts',(81.5712140202522,2.81214186549187,48.5));
#82981=CARTESIAN_POINT('Ctrl Pts',(81.5712140202522,2.81214186549187,48.35));
#82982=CARTESIAN_POINT('Ctrl Pts',(81.5712140202522,2.48499327898026,48.5));
#82983=CARTESIAN_POINT('Ctrl Pts',(81.5712140202522,2.48499327898026,48.35));
#82984=CARTESIAN_POINT('',(81.5216915011406,3.00497958064079,48.5));
#82985=CARTESIAN_POINT('Ctrl Pts',(81.5216915011406,3.00497958064079,48.5));
#82986=CARTESIAN_POINT('Ctrl Pts',(81.5712140202522,2.81214186549187,48.5));
#82987=CARTESIAN_POINT('Ctrl Pts',(81.5712140202522,2.48499327898026,48.5));
#82988=CARTESIAN_POINT('',(81.5216915011406,3.00497958064079,48.35));
#82989=CARTESIAN_POINT('',(81.5216915011406,3.00497958064079,48.5));
#82990=CARTESIAN_POINT('Ctrl Pts',(81.5216915011406,3.00497958064079,48.35));
#82991=CARTESIAN_POINT('Ctrl Pts',(81.5712140202522,2.81214186549187,48.35));
#82992=CARTESIAN_POINT('Ctrl Pts',(81.5712140202522,2.48499327898026,48.35));
#82993=CARTESIAN_POINT('Ctrl Pts',(81.3851295113564,3.33212831616402,48.5));
#82994=CARTESIAN_POINT('Ctrl Pts',(81.3851295113564,3.33212831616402,48.35));
#82995=CARTESIAN_POINT('Ctrl Pts',(81.472168982029,3.19781729578972,48.5));
#82996=CARTESIAN_POINT('Ctrl Pts',(81.472168982029,3.19781729578972,48.35));
#82997=CARTESIAN_POINT('Ctrl Pts',(81.5216915011406,3.00497958064079,48.5));
#82998=CARTESIAN_POINT('Ctrl Pts',(81.5216915011406,3.00497958064079,48.35));
#82999=CARTESIAN_POINT('',(81.3851295113564,3.33212831616402,48.5));
#83000=CARTESIAN_POINT('Ctrl Pts',(81.3851295113564,3.33212831616402,48.5));
#83001=CARTESIAN_POINT('Ctrl Pts',(81.472168982029,3.19781729578972,48.5));
#83002=CARTESIAN_POINT('Ctrl Pts',(81.5216915011406,3.00497958064079,48.5));
#83003=CARTESIAN_POINT('',(81.3851295113564,3.33212831616402,48.35));
#83004=CARTESIAN_POINT('',(81.3851295113564,3.33212831616402,48.5));
#83005=CARTESIAN_POINT('Ctrl Pts',(81.3851295113564,3.33212831616402,48.35));
#83006=CARTESIAN_POINT('Ctrl Pts',(81.472168982029,3.19781729578972,48.35));
#83007=CARTESIAN_POINT('Ctrl Pts',(81.5216915011406,3.00497958064079,48.35));
#83008=CARTESIAN_POINT('Ctrl Pts',(81.1645291447639,3.5377217233181,48.5));
#83009=CARTESIAN_POINT('Ctrl Pts',(81.1645291447639,3.5377217233181,48.35));
#83010=CARTESIAN_POINT('Ctrl Pts',(81.2980900406837,3.46643933653831,48.5));
#83011=CARTESIAN_POINT('Ctrl Pts',(81.2980900406837,3.46643933653831,48.35));
#83012=CARTESIAN_POINT('Ctrl Pts',(81.3851295113564,3.33212831616402,48.5));
#83013=CARTESIAN_POINT('Ctrl Pts',(81.3851295113564,3.33212831616402,48.35));
#83014=CARTESIAN_POINT('',(81.1645291447639,3.5377217233181,48.5));
#83015=CARTESIAN_POINT('Ctrl Pts',(81.1645291447639,3.5377217233181,48.5));
#83016=CARTESIAN_POINT('Ctrl Pts',(81.2980900406837,3.46643933653831,48.5));
#83017=CARTESIAN_POINT('Ctrl Pts',(81.3851295113564,3.33212831616402,48.5));
#83018=CARTESIAN_POINT('',(81.1645291447639,3.5377217233181,48.35));
#83019=CARTESIAN_POINT('',(81.1645291447639,3.5377217233181,48.5));
#83020=CARTESIAN_POINT('Ctrl Pts',(81.1645291447639,3.5377217233181,48.35));
#83021=CARTESIAN_POINT('Ctrl Pts',(81.2980900406837,3.46643933653831,48.35));
#83022=CARTESIAN_POINT('Ctrl Pts',(81.3851295113564,3.33212831616402,48.35));
#83023=CARTESIAN_POINT('Ctrl Pts',(80.8538882136345,3.60900411009789,48.5));
#83024=CARTESIAN_POINT('Ctrl Pts',(80.8538882136345,3.60900411009789,48.35));
#83025=CARTESIAN_POINT('Ctrl Pts',(81.0309682488441,3.60900411009789,48.5));
#83026=CARTESIAN_POINT('Ctrl Pts',(81.0309682488441,3.60900411009789,48.35));
#83027=CARTESIAN_POINT('Ctrl Pts',(81.1645291447639,3.5377217233181,48.5));
#83028=CARTESIAN_POINT('Ctrl Pts',(81.1645291447639,3.5377217233181,48.35));
#83029=CARTESIAN_POINT('',(80.8538882136345,3.60900411009789,48.5));
#83030=CARTESIAN_POINT('Ctrl Pts',(80.8538882136345,3.60900411009789,48.5));
#83031=CARTESIAN_POINT('Ctrl Pts',(81.0309682488441,3.60900411009789,48.5));
#83032=CARTESIAN_POINT('Ctrl Pts',(81.1645291447639,3.5377217233181,48.5));
#83033=CARTESIAN_POINT('',(80.8538882136345,3.60900411009789,48.35));
#83034=CARTESIAN_POINT('',(80.8538882136345,3.60900411009789,48.5));
#83035=CARTESIAN_POINT('Ctrl Pts',(80.8538882136345,3.60900411009789,48.35));
#83036=CARTESIAN_POINT('Ctrl Pts',(81.0309682488441,3.60900411009789,48.35));
#83037=CARTESIAN_POINT('Ctrl Pts',(81.1645291447639,3.5377217233181,48.35));
#83038=CARTESIAN_POINT('Ctrl Pts',(80.4554567933083,3.47994545102119,48.5));
#83039=CARTESIAN_POINT('Ctrl Pts',(80.4554567933083,3.47994545102119,48.35));
#83040=CARTESIAN_POINT('Ctrl Pts',(80.6137786507607,3.60900411009789,48.5));
#83041=CARTESIAN_POINT('Ctrl Pts',(80.6137786507607,3.60900411009789,48.35));
#83042=CARTESIAN_POINT('Ctrl Pts',(80.8538882136345,3.60900411009789,48.5));
#83043=CARTESIAN_POINT('Ctrl Pts',(80.8538882136345,3.60900411009789,48.35));
#83044=CARTESIAN_POINT('',(80.4554567933083,3.47994545102119,48.5));
#83045=CARTESIAN_POINT('Ctrl Pts',(80.4554567933083,3.47994545102119,48.5));
#83046=CARTESIAN_POINT('Ctrl Pts',(80.6137786507607,3.60900411009789,48.5));
#83047=CARTESIAN_POINT('Ctrl Pts',(80.8538882136345,3.60900411009789,48.5));
#83048=CARTESIAN_POINT('',(80.4554567933083,3.47994545102119,48.35));
#83049=CARTESIAN_POINT('',(80.4554567933083,3.47994545102119,48.5));
#83050=CARTESIAN_POINT('Ctrl Pts',(80.4554567933083,3.47994545102119,48.35));
#83051=CARTESIAN_POINT('Ctrl Pts',(80.6137786507607,3.60900411009789,48.35));
#83052=CARTESIAN_POINT('Ctrl Pts',(80.8538882136345,3.60900411009789,48.35));
#83053=CARTESIAN_POINT('Ctrl Pts',(80.2168486714363,3.11302864551544,48.5));
#83054=CARTESIAN_POINT('Ctrl Pts',(80.2168486714363,3.11302864551544,48.35));
#83055=CARTESIAN_POINT('Ctrl Pts',(80.2971349358559,3.3508867919445,48.5));
#83056=CARTESIAN_POINT('Ctrl Pts',(80.2971349358559,3.3508867919445,48.35));
#83057=CARTESIAN_POINT('Ctrl Pts',(80.4554567933083,3.47994545102119,48.5));
#83058=CARTESIAN_POINT('Ctrl Pts',(80.4554567933083,3.47994545102119,48.35));
#83059=CARTESIAN_POINT('',(80.2168486714363,3.11302864551544,48.5));
#83060=CARTESIAN_POINT('Ctrl Pts',(80.2168486714363,3.11302864551544,48.5));
#83061=CARTESIAN_POINT('Ctrl Pts',(80.2971349358559,3.3508867919445,48.5));
#83062=CARTESIAN_POINT('Ctrl Pts',(80.4554567933083,3.47994545102119,48.5));
#83063=CARTESIAN_POINT('',(80.2168486714363,3.11302864551544,48.35));
#83064=CARTESIAN_POINT('',(80.2168486714363,3.11302864551544,48.5));
#83065=CARTESIAN_POINT('Ctrl Pts',(80.2168486714363,3.11302864551544,48.35));
#83066=CARTESIAN_POINT('Ctrl Pts',(80.2971349358559,3.3508867919445,48.35));
#83067=CARTESIAN_POINT('Ctrl Pts',(80.4554567933083,3.47994545102119,48.35));
#83068=CARTESIAN_POINT('Ctrl Pts',(80.1365618109703,2.48499327898026,48.5));
#83069=CARTESIAN_POINT('Ctrl Pts',(80.1365618109703,2.48499327898026,48.35));
#83070=CARTESIAN_POINT('Ctrl Pts',(80.1365618109703,2.87517049908638,48.5));
#83071=CARTESIAN_POINT('Ctrl Pts',(80.1365618109703,2.87517049908638,48.35));
#83072=CARTESIAN_POINT('Ctrl Pts',(80.2168486714363,3.11302864551544,48.5));
#83073=CARTESIAN_POINT('Ctrl Pts',(80.2168486714363,3.11302864551544,48.35));
#83074=CARTESIAN_POINT('',(80.1365618109703,2.48499327898026,48.5));
#83075=CARTESIAN_POINT('Ctrl Pts',(80.1365618109703,2.48499327898026,48.5));
#83076=CARTESIAN_POINT('Ctrl Pts',(80.1365618109703,2.87517049908638,48.5));
#83077=CARTESIAN_POINT('Ctrl Pts',(80.2168486714363,3.11302864551544,48.5));
#83078=CARTESIAN_POINT('',(80.1365618109703,2.48499327898026,48.35));
#83079=CARTESIAN_POINT('',(80.1365618109703,2.48499327898026,48.5));
#83080=CARTESIAN_POINT('Ctrl Pts',(80.1365618109703,2.48499327898026,48.35));
#83081=CARTESIAN_POINT('Ctrl Pts',(80.1365618109703,2.87517049908638,48.35));
#83082=CARTESIAN_POINT('Ctrl Pts',(80.2168486714363,3.11302864551544,48.35));
#83083=CARTESIAN_POINT('Ctrl Pts',(80.3541610836983,1.59058684110642,48.5));
#83084=CARTESIAN_POINT('Ctrl Pts',(80.3541610836983,1.59058684110642,48.35));
#83085=CARTESIAN_POINT('Ctrl Pts',(80.1365618109703,1.86521166563034,48.5));
#83086=CARTESIAN_POINT('Ctrl Pts',(80.1365618109703,1.86521166563034,48.35));
#83087=CARTESIAN_POINT('Ctrl Pts',(80.1365618109703,2.48499327898026,48.5));
#83088=CARTESIAN_POINT('Ctrl Pts',(80.1365618109703,2.48499327898026,48.35));
#83089=CARTESIAN_POINT('Ctrl Pts',(80.3541610836983,1.59058684110642,48.5));
#83090=CARTESIAN_POINT('Ctrl Pts',(80.1365618109703,1.86521166563034,48.5));
#83091=CARTESIAN_POINT('Ctrl Pts',(80.1365618109703,2.48499327898026,48.5));
#83092=CARTESIAN_POINT('Ctrl Pts',(80.3541610836983,1.59058684110642,48.35));
#83093=CARTESIAN_POINT('Ctrl Pts',(80.1365618109703,1.86521166563034,48.35));
#83094=CARTESIAN_POINT('Ctrl Pts',(80.1365618109703,2.48499327898026,48.35));
#83095=CARTESIAN_POINT('Origin',(79.9999998956919,2.48499320447445,48.35));
#83096=CARTESIAN_POINT('Ctrl Pts',(79.1281036734581,1.36098229885101,48.5));
#83097=CARTESIAN_POINT('Ctrl Pts',(79.1281036734581,1.36098229885101,48.35));
#83098=CARTESIAN_POINT('Ctrl Pts',(78.8384720385075,1.36098229885101,48.5));
#83099=CARTESIAN_POINT('Ctrl Pts',(78.8384720385075,1.36098229885101,48.35));
#83100=CARTESIAN_POINT('Ctrl Pts',(78.6471350193024,1.53356069326401,48.5));
#83101=CARTESIAN_POINT('Ctrl Pts',(78.6471350193024,1.53356069326401,48.35));
#83102=CARTESIAN_POINT('',(79.1281036734581,1.36098229885101,48.5));
#83103=CARTESIAN_POINT('',(78.6471350193024,1.53356069326401,48.5));
#83104=CARTESIAN_POINT('Ctrl Pts',(79.1281036734581,1.36098229885101,48.5));
#83105=CARTESIAN_POINT('Ctrl Pts',(78.8384720385075,1.36098229885101,48.5));
#83106=CARTESIAN_POINT('Ctrl Pts',(78.6471350193024,1.53356069326401,48.5));
#83107=CARTESIAN_POINT('',(79.1281036734581,1.36098229885101,48.35));
#83108=CARTESIAN_POINT('',(79.1281036734581,1.36098229885101,48.5));
#83109=CARTESIAN_POINT('',(78.6471350193024,1.53356069326401,48.35));
#83110=CARTESIAN_POINT('Ctrl Pts',(79.1281036734581,1.36098229885101,48.35));
#83111=CARTESIAN_POINT('Ctrl Pts',(78.8384720385075,1.36098229885101,48.35));
#83112=CARTESIAN_POINT('Ctrl Pts',(78.6471350193024,1.53356069326401,48.35));
#83113=CARTESIAN_POINT('',(78.6471350193024,1.53356069326401,48.5));
#83114=CARTESIAN_POINT('Ctrl Pts',(79.65934497118,1.56132334470749,48.5));
#83115=CARTESIAN_POINT('Ctrl Pts',(79.65934497118,1.56132334470749,48.35));
#83116=CARTESIAN_POINT('Ctrl Pts',(79.449249625206,1.36098229885101,48.5));
#83117=CARTESIAN_POINT('Ctrl Pts',(79.449249625206,1.36098229885101,48.35));
#83118=CARTESIAN_POINT('Ctrl Pts',(79.1281036734581,1.36098229885101,48.5));
#83119=CARTESIAN_POINT('Ctrl Pts',(79.1281036734581,1.36098229885101,48.35));
#83120=CARTESIAN_POINT('',(79.65934497118,1.56132334470749,48.5));
#83121=CARTESIAN_POINT('Ctrl Pts',(79.65934497118,1.56132334470749,48.5));
#83122=CARTESIAN_POINT('Ctrl Pts',(79.449249625206,1.36098229885101,48.5));
#83123=CARTESIAN_POINT('Ctrl Pts',(79.1281036734581,1.36098229885101,48.5));
#83124=CARTESIAN_POINT('',(79.65934497118,1.56132334470749,48.35));
#83125=CARTESIAN_POINT('',(79.65934497118,1.56132334470749,48.5));
#83126=CARTESIAN_POINT('Ctrl Pts',(79.65934497118,1.56132334470749,48.35));
#83127=CARTESIAN_POINT('Ctrl Pts',(79.449249625206,1.36098229885101,48.35));
#83128=CARTESIAN_POINT('Ctrl Pts',(79.1281036734581,1.36098229885101,48.35));
#83129=CARTESIAN_POINT('Ctrl Pts',(79.8694406151772,2.04979562759399,48.5));
#83130=CARTESIAN_POINT('Ctrl Pts',(79.8694406151772,2.04979562759399,48.35));
#83131=CARTESIAN_POINT('Ctrl Pts',(79.8694406151772,1.76166439056397,48.5));
#83132=CARTESIAN_POINT('Ctrl Pts',(79.8694406151772,1.76166439056397,48.35));
#83133=CARTESIAN_POINT('Ctrl Pts',(79.65934497118,1.56132334470749,48.5));
#83134=CARTESIAN_POINT('Ctrl Pts',(79.65934497118,1.56132334470749,48.35));
#83135=CARTESIAN_POINT('',(79.8694406151772,2.04979562759399,48.5));
#83136=CARTESIAN_POINT('Ctrl Pts',(79.8694406151772,2.04979562759399,48.5));
#83137=CARTESIAN_POINT('Ctrl Pts',(79.8694406151772,1.76166439056397,48.5));
#83138=CARTESIAN_POINT('Ctrl Pts',(79.65934497118,1.56132334470749,48.5));
#83139=CARTESIAN_POINT('',(79.8694406151772,2.04979562759399,48.35));
#83140=CARTESIAN_POINT('',(79.8694406151772,2.04979562759399,48.5));
#83141=CARTESIAN_POINT('Ctrl Pts',(79.8694406151772,2.04979562759399,48.35));
#83142=CARTESIAN_POINT('Ctrl Pts',(79.8694406151772,1.76166439056397,48.35));
#83143=CARTESIAN_POINT('Ctrl Pts',(79.65934497118,1.56132334470749,48.35));
#83144=CARTESIAN_POINT('Ctrl Pts',(79.7613916993141,2.40470671653748,48.5));
#83145=CARTESIAN_POINT('Ctrl Pts',(79.7613916993141,2.40470671653748,48.35));
#83146=CARTESIAN_POINT('Ctrl Pts',(79.8694406151772,2.26289236545563,48.5));
#83147=CARTESIAN_POINT('Ctrl Pts',(79.8694406151772,2.26289236545563,48.35));
#83148=CARTESIAN_POINT('Ctrl Pts',(79.8694406151772,2.04979562759399,48.5));
#83149=CARTESIAN_POINT('Ctrl Pts',(79.8694406151772,2.04979562759399,48.35));
#83150=CARTESIAN_POINT('',(79.7613916993141,2.40470671653748,48.5));
#83151=CARTESIAN_POINT('Ctrl Pts',(79.7613916993141,2.40470671653748,48.5));
#83152=CARTESIAN_POINT('Ctrl Pts',(79.8694406151772,2.26289236545563,48.5));
#83153=CARTESIAN_POINT('Ctrl Pts',(79.8694406151772,2.04979562759399,48.5));
#83154=CARTESIAN_POINT('',(79.7613916993141,2.40470671653748,48.35));
#83155=CARTESIAN_POINT('',(79.7613916993141,2.40470671653748,48.5));
#83156=CARTESIAN_POINT('Ctrl Pts',(79.7613916993141,2.40470671653748,48.35));
#83157=CARTESIAN_POINT('Ctrl Pts',(79.8694406151772,2.26289236545563,48.35));
#83158=CARTESIAN_POINT('Ctrl Pts',(79.8694406151772,2.04979562759399,48.35));
#83159=CARTESIAN_POINT('Ctrl Pts',(79.458253800869,2.59154164791107,48.5));
#83160=CARTESIAN_POINT('Ctrl Pts',(79.458253800869,2.59154164791107,48.35));
#83161=CARTESIAN_POINT('Ctrl Pts',(79.6533421874046,2.54652121663094,48.5));
#83162=CARTESIAN_POINT('Ctrl Pts',(79.6533421874046,2.54652121663094,48.35));
#83163=CARTESIAN_POINT('Ctrl Pts',(79.7613916993141,2.40470671653748,48.5));
#83164=CARTESIAN_POINT('Ctrl Pts',(79.7613916993141,2.40470671653748,48.35));
#83165=CARTESIAN_POINT('',(79.458253800869,2.59154164791107,48.5));
#83166=CARTESIAN_POINT('Ctrl Pts',(79.458253800869,2.59154164791107,48.5));
#83167=CARTESIAN_POINT('Ctrl Pts',(79.6533421874046,2.54652121663094,48.5));
#83168=CARTESIAN_POINT('Ctrl Pts',(79.7613916993141,2.40470671653748,48.5));
#83169=CARTESIAN_POINT('',(79.458253800869,2.59154164791107,48.35));
#83170=CARTESIAN_POINT('',(79.458253800869,2.59154164791107,48.5));
#83171=CARTESIAN_POINT('Ctrl Pts',(79.458253800869,2.59154164791107,48.35));
#83172=CARTESIAN_POINT('Ctrl Pts',(79.6533421874046,2.54652121663094,48.35));
#83173=CARTESIAN_POINT('Ctrl Pts',(79.7613916993141,2.40470671653748,48.35));
#83174=CARTESIAN_POINT('Ctrl Pts',(79.6848566532135,2.77762615680695,48.5));
#83175=CARTESIAN_POINT('Ctrl Pts',(79.6848566532135,2.77762615680695,48.35));
#83176=CARTESIAN_POINT('Ctrl Pts',(79.6083219051361,2.66057306528091,48.5));
#83177=CARTESIAN_POINT('Ctrl Pts',(79.6083219051361,2.66057306528091,48.35));
#83178=CARTESIAN_POINT('Ctrl Pts',(79.458253800869,2.59154164791107,48.5));
#83179=CARTESIAN_POINT('Ctrl Pts',(79.458253800869,2.59154164791107,48.35));
#83180=CARTESIAN_POINT('',(79.6848566532135,2.77762615680695,48.5));
#83181=CARTESIAN_POINT('Ctrl Pts',(79.6848566532135,2.77762615680695,48.5));
#83182=CARTESIAN_POINT('Ctrl Pts',(79.6083219051361,2.66057306528091,48.5));
#83183=CARTESIAN_POINT('Ctrl Pts',(79.458253800869,2.59154164791107,48.5));
#83184=CARTESIAN_POINT('',(79.6848566532135,2.77762615680695,48.35));
#83185=CARTESIAN_POINT('',(79.6848566532135,2.77762615680695,48.5));
#83186=CARTESIAN_POINT('Ctrl Pts',(79.6848566532135,2.77762615680695,48.35));
#83187=CARTESIAN_POINT('Ctrl Pts',(79.6083219051361,2.66057306528091,48.35));
#83188=CARTESIAN_POINT('Ctrl Pts',(79.458253800869,2.59154164791107,48.35));
#83189=CARTESIAN_POINT('Ctrl Pts',(79.7613916993141,3.03724417090416,48.5));
#83190=CARTESIAN_POINT('Ctrl Pts',(79.7613916993141,3.03724417090416,48.35));
#83191=CARTESIAN_POINT('Ctrl Pts',(79.7613916993141,2.89467939734459,48.5));
#83192=CARTESIAN_POINT('Ctrl Pts',(79.7613916993141,2.89467939734459,48.35));
#83193=CARTESIAN_POINT('Ctrl Pts',(79.6848566532135,2.77762615680695,48.5));
#83194=CARTESIAN_POINT('Ctrl Pts',(79.6848566532135,2.77762615680695,48.35));
#83195=CARTESIAN_POINT('',(79.7613916993141,3.03724417090416,48.5));
#83196=CARTESIAN_POINT('Ctrl Pts',(79.7613916993141,3.03724417090416,48.5));
#83197=CARTESIAN_POINT('Ctrl Pts',(79.7613916993141,2.89467939734459,48.5));
#83198=CARTESIAN_POINT('Ctrl Pts',(79.6848566532135,2.77762615680695,48.5));
#83199=CARTESIAN_POINT('',(79.7613916993141,3.03724417090416,48.35));
#83200=CARTESIAN_POINT('',(79.7613916993141,3.03724417090416,48.5));
#83201=CARTESIAN_POINT('Ctrl Pts',(79.7613916993141,3.03724417090416,48.35));
#83202=CARTESIAN_POINT('Ctrl Pts',(79.7613916993141,2.89467939734459,48.35));
#83203=CARTESIAN_POINT('Ctrl Pts',(79.6848566532135,2.77762615680695,48.35));
#83204=CARTESIAN_POINT('Ctrl Pts',(79.6811048388481,3.32087317109108,48.5));
#83205=CARTESIAN_POINT('Ctrl Pts',(79.6811048388481,3.32087317109108,48.35));
#83206=CARTESIAN_POINT('Ctrl Pts',(79.7613916993141,3.18731242418289,48.5));
#83207=CARTESIAN_POINT('Ctrl Pts',(79.7613916993141,3.18731242418289,48.35));
#83208=CARTESIAN_POINT('Ctrl Pts',(79.7613916993141,3.03724417090416,48.5));
#83209=CARTESIAN_POINT('Ctrl Pts',(79.7613916993141,3.03724417090416,48.35));
#83210=CARTESIAN_POINT('',(79.6811048388481,3.32087317109108,48.5));
#83211=CARTESIAN_POINT('Ctrl Pts',(79.6811048388481,3.32087317109108,48.5));
#83212=CARTESIAN_POINT('Ctrl Pts',(79.7613916993141,3.18731242418289,48.5));
#83213=CARTESIAN_POINT('Ctrl Pts',(79.7613916993141,3.03724417090416,48.5));
#83214=CARTESIAN_POINT('',(79.6811048388481,3.32087317109108,48.35));
#83215=CARTESIAN_POINT('',(79.6811048388481,3.32087317109108,48.5));
#83216=CARTESIAN_POINT('Ctrl Pts',(79.6811048388481,3.32087317109108,48.35));
#83217=CARTESIAN_POINT('Ctrl Pts',(79.7613916993141,3.18731242418289,48.35));
#83218=CARTESIAN_POINT('Ctrl Pts',(79.7613916993141,3.03724417090416,48.35));
#83219=CARTESIAN_POINT('Ctrl Pts',(79.449249625206,3.53171893954277,48.5));
#83220=CARTESIAN_POINT('Ctrl Pts',(79.449249625206,3.53171893954277,48.35));
#83221=CARTESIAN_POINT('Ctrl Pts',(79.6008185744286,3.45443391799927,48.5));
#83222=CARTESIAN_POINT('Ctrl Pts',(79.6008185744286,3.45443391799927,48.35));
#83223=CARTESIAN_POINT('Ctrl Pts',(79.6811048388481,3.32087317109108,48.5));
#83224=CARTESIAN_POINT('Ctrl Pts',(79.6811048388481,3.32087317109108,48.35));
#83225=CARTESIAN_POINT('',(79.449249625206,3.53171893954277,48.5));
#83226=CARTESIAN_POINT('Ctrl Pts',(79.449249625206,3.53171893954277,48.5));
#83227=CARTESIAN_POINT('Ctrl Pts',(79.6008185744286,3.45443391799927,48.5));
#83228=CARTESIAN_POINT('Ctrl Pts',(79.6811048388481,3.32087317109108,48.5));
#83229=CARTESIAN_POINT('',(79.449249625206,3.53171893954277,48.35));
#83230=CARTESIAN_POINT('',(79.449249625206,3.53171893954277,48.5));
#83231=CARTESIAN_POINT('Ctrl Pts',(79.449249625206,3.53171893954277,48.35));
#83232=CARTESIAN_POINT('Ctrl Pts',(79.6008185744286,3.45443391799927,48.35));
#83233=CARTESIAN_POINT('Ctrl Pts',(79.6811048388481,3.32087317109108,48.35));
#83234=CARTESIAN_POINT('Ctrl Pts',(79.1175989508629,3.60900411009789,48.5));
#83235=CARTESIAN_POINT('Ctrl Pts',(79.1175989508629,3.60900411009789,48.35));
#83236=CARTESIAN_POINT('Ctrl Pts',(79.2976806759834,3.60900411009789,48.5));
#83237=CARTESIAN_POINT('Ctrl Pts',(79.2976806759834,3.60900411009789,48.35));
#83238=CARTESIAN_POINT('Ctrl Pts',(79.449249625206,3.53171893954277,48.5));
#83239=CARTESIAN_POINT('Ctrl Pts',(79.449249625206,3.53171893954277,48.35));
#83240=CARTESIAN_POINT('',(79.1175989508629,3.60900411009789,48.5));
#83241=CARTESIAN_POINT('Ctrl Pts',(79.1175989508629,3.60900411009789,48.5));
#83242=CARTESIAN_POINT('Ctrl Pts',(79.2976806759834,3.60900411009789,48.5));
#83243=CARTESIAN_POINT('Ctrl Pts',(79.449249625206,3.53171893954277,48.5));
#83244=CARTESIAN_POINT('',(79.1175989508629,3.60900411009789,48.35));
#83245=CARTESIAN_POINT('',(79.1175989508629,3.60900411009789,48.5));
#83246=CARTESIAN_POINT('Ctrl Pts',(79.1175989508629,3.60900411009789,48.35));
#83247=CARTESIAN_POINT('Ctrl Pts',(79.2976806759834,3.60900411009789,48.35));
#83248=CARTESIAN_POINT('Ctrl Pts',(79.449249625206,3.53171893954277,48.35));
#83249=CARTESIAN_POINT('Ctrl Pts',(78.6809004545212,3.45968627929688,48.5));
#83250=CARTESIAN_POINT('Ctrl Pts',(78.6809004545212,3.45968627929688,48.35));
#83251=CARTESIAN_POINT('Ctrl Pts',(78.8564802408218,3.60900411009789,48.5));
#83252=CARTESIAN_POINT('Ctrl Pts',(78.8564802408218,3.60900411009789,48.35));
#83253=CARTESIAN_POINT('Ctrl Pts',(79.1175989508629,3.60900411009789,48.5));
#83254=CARTESIAN_POINT('Ctrl Pts',(79.1175989508629,3.60900411009789,48.35));
#83255=CARTESIAN_POINT('',(78.6809004545212,3.45968627929688,48.5));
#83256=CARTESIAN_POINT('Ctrl Pts',(78.6809004545212,3.45968627929688,48.5));
#83257=CARTESIAN_POINT('Ctrl Pts',(78.8564802408218,3.60900411009789,48.5));
#83258=CARTESIAN_POINT('Ctrl Pts',(79.1175989508629,3.60900411009789,48.5));
#83259=CARTESIAN_POINT('',(78.6809004545212,3.45968627929688,48.35));
#83260=CARTESIAN_POINT('',(78.6809004545212,3.45968627929688,48.5));
#83261=CARTESIAN_POINT('Ctrl Pts',(78.6809004545212,3.45968627929688,48.35));
#83262=CARTESIAN_POINT('Ctrl Pts',(78.8564802408218,3.60900411009789,48.35));
#83263=CARTESIAN_POINT('Ctrl Pts',(79.1175989508629,3.60900411009789,48.35));
#83264=CARTESIAN_POINT('Ctrl Pts',(78.4557980000973,3.03874486684799,48.5));
#83265=CARTESIAN_POINT('Ctrl Pts',(78.4557980000973,3.03874486684799,48.35));
#83266=CARTESIAN_POINT('Ctrl Pts',(78.5053205192089,3.31036829948425,48.5));
#83267=CARTESIAN_POINT('Ctrl Pts',(78.5053205192089,3.31036829948425,48.35));
#83268=CARTESIAN_POINT('Ctrl Pts',(78.6809004545212,3.45968627929688,48.5));
#83269=CARTESIAN_POINT('Ctrl Pts',(78.6809004545212,3.45968627929688,48.35));
#83270=CARTESIAN_POINT('',(78.4557980000973,3.03874486684799,48.5));
#83271=CARTESIAN_POINT('Ctrl Pts',(78.4557980000973,3.03874486684799,48.5));
#83272=CARTESIAN_POINT('Ctrl Pts',(78.5053205192089,3.31036829948425,48.5));
#83273=CARTESIAN_POINT('Ctrl Pts',(78.6809004545212,3.45968627929688,48.5));
#83274=CARTESIAN_POINT('',(78.4557980000973,3.03874486684799,48.35));
#83275=CARTESIAN_POINT('',(78.4557980000973,3.03874486684799,48.5));
#83276=CARTESIAN_POINT('Ctrl Pts',(78.4557980000973,3.03874486684799,48.35));
#83277=CARTESIAN_POINT('Ctrl Pts',(78.5053205192089,3.31036829948425,48.35));
#83278=CARTESIAN_POINT('Ctrl Pts',(78.6809004545212,3.45968627929688,48.35));
#83279=CARTESIAN_POINT('Origin',(78.7259207367897,2.99072304368019,48.5));
#83280=CARTESIAN_POINT('',(78.7259207367897,2.99072304368019,48.5));
#83281=CARTESIAN_POINT('',(40.1372829580836,9.85092578849893,48.5));
#83282=CARTESIAN_POINT('',(78.7259207367897,2.99072304368019,48.35));
#83283=CARTESIAN_POINT('',(78.7259207367897,2.99072304368019,48.5));
#83284=CARTESIAN_POINT('',(78.7259207367897,2.99072304368019,48.35));
#83285=CARTESIAN_POINT('Ctrl Pts',(78.8609821796417,3.28785815834999,48.5));
#83286=CARTESIAN_POINT('Ctrl Pts',(78.8609821796417,3.28785815834999,48.35));
#83287=CARTESIAN_POINT('Ctrl Pts',(78.7559345066547,3.18881312012672,48.5));
#83288=CARTESIAN_POINT('Ctrl Pts',(78.7559345066547,3.18881312012672,48.35));
#83289=CARTESIAN_POINT('Ctrl Pts',(78.7259207367897,2.99072304368019,48.5));
#83290=CARTESIAN_POINT('Ctrl Pts',(78.7259207367897,2.99072304368019,48.35));
#83291=CARTESIAN_POINT('',(78.8609821796417,3.28785815834999,48.5));
#83292=CARTESIAN_POINT('Ctrl Pts',(78.8609821796417,3.28785815834999,48.5));
#83293=CARTESIAN_POINT('Ctrl Pts',(78.7559345066547,3.18881312012672,48.5));
#83294=CARTESIAN_POINT('Ctrl Pts',(78.7259207367897,2.99072304368019,48.5));
#83295=CARTESIAN_POINT('',(78.8609821796417,3.28785815834999,48.35));
#83296=CARTESIAN_POINT('',(78.8609821796417,3.28785815834999,48.5));
#83297=CARTESIAN_POINT('Ctrl Pts',(78.8609821796417,3.28785815834999,48.35));
#83298=CARTESIAN_POINT('Ctrl Pts',(78.7559345066547,3.18881312012672,48.35));
#83299=CARTESIAN_POINT('Ctrl Pts',(78.7259207367897,2.99072304368019,48.35));
#83300=CARTESIAN_POINT('Ctrl Pts',(79.1236015856266,3.38690319657326,48.5));
#83301=CARTESIAN_POINT('Ctrl Pts',(79.1236015856266,3.38690319657326,48.35));
#83302=CARTESIAN_POINT('Ctrl Pts',(78.9660300016403,3.38690319657326,48.5));
#83303=CARTESIAN_POINT('Ctrl Pts',(78.9660300016403,3.38690319657326,48.35));
#83304=CARTESIAN_POINT('Ctrl Pts',(78.8609821796417,3.28785815834999,48.5));
#83305=CARTESIAN_POINT('Ctrl Pts',(78.8609821796417,3.28785815834999,48.35));
#83306=CARTESIAN_POINT('',(79.1236015856266,3.38690319657326,48.5));
#83307=CARTESIAN_POINT('Ctrl Pts',(79.1236015856266,3.38690319657326,48.5));
#83308=CARTESIAN_POINT('Ctrl Pts',(78.9660300016403,3.38690319657326,48.5));
#83309=CARTESIAN_POINT('Ctrl Pts',(78.8609821796417,3.28785815834999,48.5));
#83310=CARTESIAN_POINT('',(79.1236015856266,3.38690319657326,48.35));
#83311=CARTESIAN_POINT('',(79.1236015856266,3.38690319657326,48.5));
#83312=CARTESIAN_POINT('Ctrl Pts',(79.1236015856266,3.38690319657326,48.35));
#83313=CARTESIAN_POINT('Ctrl Pts',(78.9660300016403,3.38690319657326,48.35));
#83314=CARTESIAN_POINT('Ctrl Pts',(78.8609821796417,3.28785815834999,48.35));
#83315=CARTESIAN_POINT('Ctrl Pts',(79.3832195997238,3.28935885429382,48.5));
#83316=CARTESIAN_POINT('Ctrl Pts',(79.3832195997238,3.28935885429382,48.35));
#83317=CARTESIAN_POINT('Ctrl Pts',(79.2826738655567,3.38690319657326,48.5));
#83318=CARTESIAN_POINT('Ctrl Pts',(79.2826738655567,3.38690319657326,48.35));
#83319=CARTESIAN_POINT('Ctrl Pts',(79.1236015856266,3.38690319657326,48.5));
#83320=CARTESIAN_POINT('Ctrl Pts',(79.1236015856266,3.38690319657326,48.35));
#83321=CARTESIAN_POINT('',(79.3832195997238,3.28935885429382,48.5));
#83322=CARTESIAN_POINT('Ctrl Pts',(79.3832195997238,3.28935885429382,48.5));
#83323=CARTESIAN_POINT('Ctrl Pts',(79.2826738655567,3.38690319657326,48.5));
#83324=CARTESIAN_POINT('Ctrl Pts',(79.1236015856266,3.38690319657326,48.5));
#83325=CARTESIAN_POINT('',(79.3832195997238,3.28935885429382,48.35));
#83326=CARTESIAN_POINT('',(79.3832195997238,3.28935885429382,48.5));
#83327=CARTESIAN_POINT('Ctrl Pts',(79.3832195997238,3.28935885429382,48.35));
#83328=CARTESIAN_POINT('Ctrl Pts',(79.2826738655567,3.38690319657326,48.35));
#83329=CARTESIAN_POINT('Ctrl Pts',(79.1236015856266,3.38690319657326,48.35));
#83330=CARTESIAN_POINT('Ctrl Pts',(79.4837651848793,3.04324695467949,48.5));
#83331=CARTESIAN_POINT('Ctrl Pts',(79.4837651848793,3.04324695467949,48.35));
#83332=CARTESIAN_POINT('Ctrl Pts',(79.4837651848793,3.19181451201439,48.5));
#83333=CARTESIAN_POINT('Ctrl Pts',(79.4837651848793,3.19181451201439,48.35));
#83334=CARTESIAN_POINT('Ctrl Pts',(79.3832195997238,3.28935885429382,48.5));
#83335=CARTESIAN_POINT('Ctrl Pts',(79.3832195997238,3.28935885429382,48.35));
#83336=CARTESIAN_POINT('',(79.4837651848793,3.04324695467949,48.5));
#83337=CARTESIAN_POINT('Ctrl Pts',(79.4837651848793,3.04324695467949,48.5));
#83338=CARTESIAN_POINT('Ctrl Pts',(79.4837651848793,3.19181451201439,48.5));
#83339=CARTESIAN_POINT('Ctrl Pts',(79.3832195997238,3.28935885429382,48.5));
#83340=CARTESIAN_POINT('',(79.4837651848793,3.04324695467949,48.35));
#83341=CARTESIAN_POINT('',(79.4837651848793,3.04324695467949,48.5));
#83342=CARTESIAN_POINT('Ctrl Pts',(79.4837651848793,3.04324695467949,48.35));
#83343=CARTESIAN_POINT('Ctrl Pts',(79.4837651848793,3.19181451201439,48.35));
#83344=CARTESIAN_POINT('Ctrl Pts',(79.3832195997238,3.28935885429382,48.35));
#83345=CARTESIAN_POINT('Ctrl Pts',(79.3457026481628,2.7656207382679,48.5));
#83346=CARTESIAN_POINT('Ctrl Pts',(79.3457026481628,2.7656207382679,48.35));
#83347=CARTESIAN_POINT('Ctrl Pts',(79.4837651848793,2.85566174983978,48.5));
#83348=CARTESIAN_POINT('Ctrl Pts',(79.4837651848793,2.85566174983978,48.35));
#83349=CARTESIAN_POINT('Ctrl Pts',(79.4837651848793,3.04324695467949,48.5));
#83350=CARTESIAN_POINT('Ctrl Pts',(79.4837651848793,3.04324695467949,48.35));
#83351=CARTESIAN_POINT('',(79.3457026481628,2.7656207382679,48.5));
#83352=CARTESIAN_POINT('Ctrl Pts',(79.3457026481628,2.7656207382679,48.5));
#83353=CARTESIAN_POINT('Ctrl Pts',(79.4837651848793,2.85566174983978,48.5));
#83354=CARTESIAN_POINT('Ctrl Pts',(79.4837651848793,3.04324695467949,48.5));
#83355=CARTESIAN_POINT('',(79.3457026481628,2.7656207382679,48.35));
#83356=CARTESIAN_POINT('',(79.3457026481628,2.7656207382679,48.5));
#83357=CARTESIAN_POINT('Ctrl Pts',(79.3457026481628,2.7656207382679,48.35));
#83358=CARTESIAN_POINT('Ctrl Pts',(79.4837651848793,2.85566174983978,48.35));
#83359=CARTESIAN_POINT('Ctrl Pts',(79.4837651848793,3.04324695467949,48.35));
#83360=CARTESIAN_POINT('Ctrl Pts',(79.0350614190102,2.67557987570763,48.5));
#83361=CARTESIAN_POINT('Ctrl Pts',(79.0350614190102,2.67557987570763,48.35));
#83362=CARTESIAN_POINT('Ctrl Pts',(79.2076398134232,2.67557987570763,48.5));
#83363=CARTESIAN_POINT('Ctrl Pts',(79.2076398134232,2.67557987570763,48.35));
#83364=CARTESIAN_POINT('Ctrl Pts',(79.3457026481628,2.7656207382679,48.5));
#83365=CARTESIAN_POINT('Ctrl Pts',(79.3457026481628,2.7656207382679,48.35));
#83366=CARTESIAN_POINT('',(79.0350614190102,2.67557987570763,48.5));
#83367=CARTESIAN_POINT('Ctrl Pts',(79.0350614190102,2.67557987570763,48.5));
#83368=CARTESIAN_POINT('Ctrl Pts',(79.2076398134232,2.67557987570763,48.5));
#83369=CARTESIAN_POINT('Ctrl Pts',(79.3457026481628,2.7656207382679,48.5));
#83370=CARTESIAN_POINT('',(79.0350614190102,2.67557987570763,48.35));
#83371=CARTESIAN_POINT('',(79.0350614190102,2.67557987570763,48.5));
#83372=CARTESIAN_POINT('Ctrl Pts',(79.0350614190102,2.67557987570763,48.35));
#83373=CARTESIAN_POINT('Ctrl Pts',(79.2076398134232,2.67557987570763,48.35));
#83374=CARTESIAN_POINT('Ctrl Pts',(79.3457026481628,2.7656207382679,48.35));
#83375=CARTESIAN_POINT('Ctrl Pts',(78.9915415346622,2.67858126759529,48.5));
#83376=CARTESIAN_POINT('Ctrl Pts',(78.9915415346622,2.67858126759529,48.35));
#83377=CARTESIAN_POINT('Ctrl Pts',(79.0185539126396,2.67557987570763,48.5));
#83378=CARTESIAN_POINT('Ctrl Pts',(79.0185539126396,2.67557987570763,48.35));
#83379=CARTESIAN_POINT('Ctrl Pts',(79.0350614190102,2.67557987570763,48.5));
#83380=CARTESIAN_POINT('Ctrl Pts',(79.0350614190102,2.67557987570763,48.35));
#83381=CARTESIAN_POINT('',(78.9915415346622,2.67858126759529,48.5));
#83382=CARTESIAN_POINT('Ctrl Pts',(78.9915415346622,2.67858126759529,48.5));
#83383=CARTESIAN_POINT('Ctrl Pts',(79.0185539126396,2.67557987570763,48.5));
#83384=CARTESIAN_POINT('Ctrl Pts',(79.0350614190102,2.67557987570763,48.5));
#83385=CARTESIAN_POINT('',(78.9915415346622,2.67858126759529,48.35));
#83386=CARTESIAN_POINT('',(78.9915415346622,2.67858126759529,48.5));
#83387=CARTESIAN_POINT('Ctrl Pts',(78.9915415346622,2.67858126759529,48.35));
#83388=CARTESIAN_POINT('Ctrl Pts',(79.0185539126396,2.67557987570763,48.35));
#83389=CARTESIAN_POINT('Ctrl Pts',(79.0350614190102,2.67557987570763,48.35));
#83390=CARTESIAN_POINT('Origin',(78.9615279138088,2.44147354364395,48.5));
#83391=CARTESIAN_POINT('',(78.9615279138088,2.44147354364395,48.5));
#83392=CARTESIAN_POINT('',(78.6851589487883,0.258157622288407,48.5));
#83393=CARTESIAN_POINT('',(78.9615279138088,2.44147354364395,48.35));
#83394=CARTESIAN_POINT('',(78.9615279138088,2.44147354364395,48.5));
#83395=CARTESIAN_POINT('',(78.9615279138088,2.44147354364395,48.35));
#83396=CARTESIAN_POINT('Ctrl Pts',(79.1521145105362,2.47148716449738,48.5));
#83397=CARTESIAN_POINT('Ctrl Pts',(79.1521145105362,2.47148716449738,48.35));
#83398=CARTESIAN_POINT('Ctrl Pts',(79.0755797624588,2.47148716449738,48.5));
#83399=CARTESIAN_POINT('Ctrl Pts',(79.0755797624588,2.47148716449738,48.35));
#83400=CARTESIAN_POINT('Ctrl Pts',(78.9615279138088,2.44147354364395,48.5));
#83401=CARTESIAN_POINT('Ctrl Pts',(78.9615279138088,2.44147354364395,48.35));
#83402=CARTESIAN_POINT('',(79.1521145105362,2.47148716449738,48.5));
#83403=CARTESIAN_POINT('Ctrl Pts',(79.1521145105362,2.47148716449738,48.5));
#83404=CARTESIAN_POINT('Ctrl Pts',(79.0755797624588,2.47148716449738,48.5));
#83405=CARTESIAN_POINT('Ctrl Pts',(78.9615279138088,2.44147354364395,48.5));
#83406=CARTESIAN_POINT('',(79.1521145105362,2.47148716449738,48.35));
#83407=CARTESIAN_POINT('',(79.1521145105362,2.47148716449738,48.5));
#83408=CARTESIAN_POINT('Ctrl Pts',(79.1521145105362,2.47148716449738,48.35));
#83409=CARTESIAN_POINT('Ctrl Pts',(79.0755797624588,2.47148716449738,48.35));
#83410=CARTESIAN_POINT('Ctrl Pts',(78.9615279138088,2.44147354364395,48.35));
#83411=CARTESIAN_POINT('Ctrl Pts',(79.4612548947334,2.35068225860596,48.5));
#83412=CARTESIAN_POINT('Ctrl Pts',(79.4612548947334,2.35068225860596,48.35));
#83413=CARTESIAN_POINT('Ctrl Pts',(79.3396998643875,2.47148716449738,48.5));
#83414=CARTESIAN_POINT('Ctrl Pts',(79.3396998643875,2.47148716449738,48.35));
#83415=CARTESIAN_POINT('Ctrl Pts',(79.1521145105362,2.47148716449738,48.5));
#83416=CARTESIAN_POINT('Ctrl Pts',(79.1521145105362,2.47148716449738,48.35));
#83417=CARTESIAN_POINT('',(79.4612548947334,2.35068225860596,48.5));
#83418=CARTESIAN_POINT('Ctrl Pts',(79.4612548947334,2.35068225860596,48.5));
#83419=CARTESIAN_POINT('Ctrl Pts',(79.3396998643875,2.47148716449738,48.5));
#83420=CARTESIAN_POINT('Ctrl Pts',(79.1521145105362,2.47148716449738,48.5));
#83421=CARTESIAN_POINT('',(79.4612548947334,2.35068225860596,48.35));
#83422=CARTESIAN_POINT('',(79.4612548947334,2.35068225860596,48.5));
#83423=CARTESIAN_POINT('Ctrl Pts',(79.4612548947334,2.35068225860596,48.35));
#83424=CARTESIAN_POINT('Ctrl Pts',(79.3396998643875,2.47148716449738,48.35));
#83425=CARTESIAN_POINT('Ctrl Pts',(79.1521145105362,2.47148716449738,48.35));
#83426=CARTESIAN_POINT('Ctrl Pts',(79.5828102231026,2.04379284381866,48.5));
#83427=CARTESIAN_POINT('Ctrl Pts',(79.5828102231026,2.04379284381866,48.35));
#83428=CARTESIAN_POINT('Ctrl Pts',(79.5828102231026,2.22987735271454,48.5));
#83429=CARTESIAN_POINT('Ctrl Pts',(79.5828102231026,2.22987735271454,48.35));
#83430=CARTESIAN_POINT('Ctrl Pts',(79.4612548947334,2.35068225860596,48.5));
#83431=CARTESIAN_POINT('Ctrl Pts',(79.4612548947334,2.35068225860596,48.35));
#83432=CARTESIAN_POINT('',(79.5828102231026,2.04379284381866,48.5));
#83433=CARTESIAN_POINT('Ctrl Pts',(79.5828102231026,2.04379284381866,48.5));
#83434=CARTESIAN_POINT('Ctrl Pts',(79.5828102231026,2.22987735271454,48.5));
#83435=CARTESIAN_POINT('Ctrl Pts',(79.4612548947334,2.35068225860596,48.5));
#83436=CARTESIAN_POINT('',(79.5828102231026,2.04379284381866,48.35));
#83437=CARTESIAN_POINT('',(79.5828102231026,2.04379284381866,48.5));
#83438=CARTESIAN_POINT('Ctrl Pts',(79.5828102231026,2.04379284381866,48.35));
#83439=CARTESIAN_POINT('Ctrl Pts',(79.5828102231026,2.22987735271454,48.35));
#83440=CARTESIAN_POINT('Ctrl Pts',(79.4612548947334,2.35068225860596,48.35));
#83441=CARTESIAN_POINT('Ctrl Pts',(79.4515005946159,1.71664410829544,48.5));
#83442=CARTESIAN_POINT('Ctrl Pts',(79.4515005946159,1.71664410829544,48.35));
#83443=CARTESIAN_POINT('Ctrl Pts',(79.5828102231026,1.8487041592598,48.5));
#83444=CARTESIAN_POINT('Ctrl Pts',(79.5828102231026,1.8487041592598,48.35));
#83445=CARTESIAN_POINT('Ctrl Pts',(79.5828102231026,2.04379284381866,48.5));
#83446=CARTESIAN_POINT('Ctrl Pts',(79.5828102231026,2.04379284381866,48.35));
#83447=CARTESIAN_POINT('',(79.4515005946159,1.71664410829544,48.5));
#83448=CARTESIAN_POINT('Ctrl Pts',(79.4515005946159,1.71664410829544,48.5));
#83449=CARTESIAN_POINT('Ctrl Pts',(79.5828102231026,1.8487041592598,48.5));
#83450=CARTESIAN_POINT('Ctrl Pts',(79.5828102231026,2.04379284381866,48.5));
#83451=CARTESIAN_POINT('',(79.4515005946159,1.71664410829544,48.35));
#83452=CARTESIAN_POINT('',(79.4515005946159,1.71664410829544,48.5));
#83453=CARTESIAN_POINT('Ctrl Pts',(79.4515005946159,1.71664410829544,48.35));
#83454=CARTESIAN_POINT('Ctrl Pts',(79.5828102231026,1.8487041592598,48.35));
#83455=CARTESIAN_POINT('Ctrl Pts',(79.5828102231026,2.04379284381866,48.35));
#83456=CARTESIAN_POINT('Ctrl Pts',(79.1296042203903,1.58458405733109,48.5));
#83457=CARTESIAN_POINT('Ctrl Pts',(79.1296042203903,1.58458405733109,48.35));
#83458=CARTESIAN_POINT('Ctrl Pts',(79.3201909661293,1.58458405733109,48.5));
#83459=CARTESIAN_POINT('Ctrl Pts',(79.3201909661293,1.58458405733109,48.35));
#83460=CARTESIAN_POINT('Ctrl Pts',(79.4515005946159,1.71664410829544,48.5));
#83461=CARTESIAN_POINT('Ctrl Pts',(79.4515005946159,1.71664410829544,48.35));
#83462=CARTESIAN_POINT('',(79.1296042203903,1.58458405733109,48.5));
#83463=CARTESIAN_POINT('Ctrl Pts',(79.1296042203903,1.58458405733109,48.5));
#83464=CARTESIAN_POINT('Ctrl Pts',(79.3201909661293,1.58458405733109,48.5));
#83465=CARTESIAN_POINT('Ctrl Pts',(79.4515005946159,1.71664410829544,48.5));
#83466=CARTESIAN_POINT('',(79.1296042203903,1.58458405733109,48.35));
#83467=CARTESIAN_POINT('',(79.1296042203903,1.58458405733109,48.5));
#83468=CARTESIAN_POINT('Ctrl Pts',(79.1296042203903,1.58458405733109,48.35));
#83469=CARTESIAN_POINT('Ctrl Pts',(79.3201909661293,1.58458405733109,48.35));
#83470=CARTESIAN_POINT('Ctrl Pts',(79.4515005946159,1.71664410829544,48.35));
#83471=CARTESIAN_POINT('Ctrl Pts',(78.8572305142879,1.68588006496429,48.5));
#83472=CARTESIAN_POINT('Ctrl Pts',(78.8572305142879,1.68588006496429,48.35));
#83473=CARTESIAN_POINT('Ctrl Pts',(78.969031393528,1.58458405733109,48.5));
#83474=CARTESIAN_POINT('Ctrl Pts',(78.969031393528,1.58458405733109,48.35));
#83475=CARTESIAN_POINT('Ctrl Pts',(79.1296042203903,1.58458405733109,48.5));
#83476=CARTESIAN_POINT('Ctrl Pts',(79.1296042203903,1.58458405733109,48.35));
#83477=CARTESIAN_POINT('',(78.8572305142879,1.68588006496429,48.5));
#83478=CARTESIAN_POINT('Ctrl Pts',(78.8572305142879,1.68588006496429,48.5));
#83479=CARTESIAN_POINT('Ctrl Pts',(78.969031393528,1.58458405733109,48.5));
#83480=CARTESIAN_POINT('Ctrl Pts',(79.1296042203903,1.58458405733109,48.5));
#83481=CARTESIAN_POINT('',(78.8572305142879,1.68588006496429,48.35));
#83482=CARTESIAN_POINT('',(78.8572305142879,1.68588006496429,48.5));
#83483=CARTESIAN_POINT('Ctrl Pts',(78.8572305142879,1.68588006496429,48.35));
#83484=CARTESIAN_POINT('Ctrl Pts',(78.969031393528,1.58458405733109,48.35));
#83485=CARTESIAN_POINT('Ctrl Pts',(79.1296042203903,1.58458405733109,48.35));
#83486=CARTESIAN_POINT('Ctrl Pts',(78.6989085078239,2.01678061485291,48.5));
#83487=CARTESIAN_POINT('Ctrl Pts',(78.6989085078239,2.01678061485291,48.35));
#83488=CARTESIAN_POINT('Ctrl Pts',(78.7454296350479,1.7871760725975,48.5));
#83489=CARTESIAN_POINT('Ctrl Pts',(78.7454296350479,1.7871760725975,48.35));
#83490=CARTESIAN_POINT('Ctrl Pts',(78.8572305142879,1.68588006496429,48.5));
#83491=CARTESIAN_POINT('Ctrl Pts',(78.8572305142879,1.68588006496429,48.35));
#83492=CARTESIAN_POINT('',(78.6989085078239,2.01678061485291,48.5));
#83493=CARTESIAN_POINT('Ctrl Pts',(78.6989085078239,2.01678061485291,48.5));
#83494=CARTESIAN_POINT('Ctrl Pts',(78.7454296350479,1.7871760725975,48.5));
#83495=CARTESIAN_POINT('Ctrl Pts',(78.8572305142879,1.68588006496429,48.5));
#83496=CARTESIAN_POINT('',(78.6989085078239,2.01678061485291,48.35));
#83497=CARTESIAN_POINT('',(78.6989085078239,2.01678061485291,48.5));
#83498=CARTESIAN_POINT('Ctrl Pts',(78.6989085078239,2.01678061485291,48.35));
#83499=CARTESIAN_POINT('Ctrl Pts',(78.7454296350479,1.7871760725975,48.35));
#83500=CARTESIAN_POINT('Ctrl Pts',(78.8572305142879,1.68588006496429,48.35));
#83501=CARTESIAN_POINT('Origin',(78.4287857711315,1.98076421022415,48.5));
#83502=CARTESIAN_POINT('',(78.4287857711315,1.98076421022415,48.5));
#83503=CARTESIAN_POINT('',(40.2936354383861,-3.10392811068335,48.5));
#83504=CARTESIAN_POINT('',(78.4287857711315,1.98076421022415,48.35));
#83505=CARTESIAN_POINT('',(78.4287857711315,1.98076421022415,48.5));
#83506=CARTESIAN_POINT('',(78.4287857711315,1.98076421022415,48.35));
#83507=CARTESIAN_POINT('Ctrl Pts',(78.6471350193024,1.53356069326401,48.5));
#83508=CARTESIAN_POINT('Ctrl Pts',(78.6471350193024,1.53356069326401,48.35));
#83509=CARTESIAN_POINT('Ctrl Pts',(78.4557980000973,1.70613938570023,48.5));
#83510=CARTESIAN_POINT('Ctrl Pts',(78.4557980000973,1.70613938570023,48.35));
#83511=CARTESIAN_POINT('Ctrl Pts',(78.4287857711315,1.98076421022415,48.5));
#83512=CARTESIAN_POINT('Ctrl Pts',(78.4287857711315,1.98076421022415,48.35));
#83513=CARTESIAN_POINT('Ctrl Pts',(78.6471350193024,1.53356069326401,48.5));
#83514=CARTESIAN_POINT('Ctrl Pts',(78.4557980000973,1.70613938570023,48.5));
#83515=CARTESIAN_POINT('Ctrl Pts',(78.4287857711315,1.98076421022415,48.5));
#83516=CARTESIAN_POINT('Ctrl Pts',(78.6471350193024,1.53356069326401,48.35));
#83517=CARTESIAN_POINT('Ctrl Pts',(78.4557980000973,1.70613938570023,48.35));
#83518=CARTESIAN_POINT('Ctrl Pts',(78.4287857711315,1.98076421022415,48.35));
#83519=CARTESIAN_POINT('Origin',(79.9999998956919,2.48499320447445,48.35));
#83520=CARTESIAN_POINT('Origin',(0.,8.,48.5));
#83521=CARTESIAN_POINT('Ctrl Pts',(70.8959074625745,3.38540250062943,48.5));
#83522=CARTESIAN_POINT('Ctrl Pts',(70.8959074625745,3.38540250062943,48.35));
#83523=CARTESIAN_POINT('Ctrl Pts',(70.7098226556554,3.38540250062943,48.5));
#83524=CARTESIAN_POINT('Ctrl Pts',(70.7098226556554,3.38540250062943,48.35));
#83525=CARTESIAN_POINT('Ctrl Pts',(70.5987723479047,3.22783091664314,48.5));
#83526=CARTESIAN_POINT('Ctrl Pts',(70.5987723479047,3.22783091664314,48.35));
#83527=CARTESIAN_POINT('',(70.8959074625745,3.38540250062943,48.5));
#83528=CARTESIAN_POINT('',(70.5987723479047,3.22783091664314,48.5));
#83529=CARTESIAN_POINT('Ctrl Pts',(70.8959074625745,3.38540250062943,48.5));
#83530=CARTESIAN_POINT('Ctrl Pts',(70.7098226556554,3.38540250062943,48.5));
#83531=CARTESIAN_POINT('Ctrl Pts',(70.5987723479047,3.22783091664314,48.5));
#83532=CARTESIAN_POINT('',(70.8959074625745,3.38540250062943,48.35));
#83533=CARTESIAN_POINT('',(70.8959074625745,3.38540250062943,48.5));
#83534=CARTESIAN_POINT('',(70.5987723479047,3.22783091664314,48.35));
#83535=CARTESIAN_POINT('Ctrl Pts',(70.8959074625745,3.38540250062943,48.35));
#83536=CARTESIAN_POINT('Ctrl Pts',(70.7098226556554,3.38540250062943,48.35));
#83537=CARTESIAN_POINT('Ctrl Pts',(70.5987723479047,3.22783091664314,48.35));
#83538=CARTESIAN_POINT('',(70.5987723479047,3.22783091664314,48.5));
#83539=CARTESIAN_POINT('Ctrl Pts',(71.2118007550016,3.2068213224411,48.5));
#83540=CARTESIAN_POINT('Ctrl Pts',(71.2118007550016,3.2068213224411,48.35));
#83541=CARTESIAN_POINT('Ctrl Pts',(71.0849930653349,3.38540250062943,48.5));
#83542=CARTESIAN_POINT('Ctrl Pts',(71.0849930653349,3.38540250062943,48.35));
#83543=CARTESIAN_POINT('Ctrl Pts',(70.8959074625745,3.38540250062943,48.5));
#83544=CARTESIAN_POINT('Ctrl Pts',(70.8959074625745,3.38540250062943,48.35));
#83545=CARTESIAN_POINT('',(71.2118007550016,3.2068213224411,48.5));
#83546=CARTESIAN_POINT('Ctrl Pts',(71.2118007550016,3.2068213224411,48.5));
#83547=CARTESIAN_POINT('Ctrl Pts',(71.0849930653349,3.38540250062943,48.5));
#83548=CARTESIAN_POINT('Ctrl Pts',(70.8959074625745,3.38540250062943,48.5));
#83549=CARTESIAN_POINT('',(71.2118007550016,3.2068213224411,48.35));
#83550=CARTESIAN_POINT('',(71.2118007550016,3.2068213224411,48.5));
#83551=CARTESIAN_POINT('Ctrl Pts',(71.2118007550016,3.2068213224411,48.35));
#83552=CARTESIAN_POINT('Ctrl Pts',(71.0849930653349,3.38540250062943,48.35));
#83553=CARTESIAN_POINT('Ctrl Pts',(70.8959074625745,3.38540250062943,48.35));
#83554=CARTESIAN_POINT('Ctrl Pts',(71.3386084446684,2.48499327898026,48.5));
#83555=CARTESIAN_POINT('Ctrl Pts',(71.3386084446684,2.48499327898026,48.35));
#83556=CARTESIAN_POINT('Ctrl Pts',(71.3386084446684,3.02824014425278,48.5));
#83557=CARTESIAN_POINT('Ctrl Pts',(71.3386084446684,3.02824014425278,48.35));
#83558=CARTESIAN_POINT('Ctrl Pts',(71.2118007550016,3.2068213224411,48.5));
#83559=CARTESIAN_POINT('Ctrl Pts',(71.2118007550016,3.2068213224411,48.35));
#83560=CARTESIAN_POINT('',(71.3386084446684,2.48499327898026,48.5));
#83561=CARTESIAN_POINT('Ctrl Pts',(71.3386084446684,2.48499327898026,48.5));
#83562=CARTESIAN_POINT('Ctrl Pts',(71.3386084446684,3.02824014425278,48.5));
#83563=CARTESIAN_POINT('Ctrl Pts',(71.2118007550016,3.2068213224411,48.5));
#83564=CARTESIAN_POINT('',(71.3386084446684,2.48499327898026,48.35));
#83565=CARTESIAN_POINT('',(71.3386084446684,2.48499327898026,48.5));
#83566=CARTESIAN_POINT('Ctrl Pts',(71.3386084446684,2.48499327898026,48.35));
#83567=CARTESIAN_POINT('Ctrl Pts',(71.3386084446684,3.02824014425278,48.35));
#83568=CARTESIAN_POINT('Ctrl Pts',(71.2118007550016,3.2068213224411,48.35));
#83569=CARTESIAN_POINT('Ctrl Pts',(71.2118007550016,1.76466578245163,48.5));
#83570=CARTESIAN_POINT('Ctrl Pts',(71.2118007550016,1.76466578245163,48.35));
#83571=CARTESIAN_POINT('Ctrl Pts',(71.3386084446684,1.9447478055954,48.5));
#83572=CARTESIAN_POINT('Ctrl Pts',(71.3386084446684,1.9447478055954,48.35));
#83573=CARTESIAN_POINT('Ctrl Pts',(71.3386084446684,2.48499327898026,48.5));
#83574=CARTESIAN_POINT('Ctrl Pts',(71.3386084446684,2.48499327898026,48.35));
#83575=CARTESIAN_POINT('',(71.2118007550016,1.76466578245163,48.5));
#83576=CARTESIAN_POINT('Ctrl Pts',(71.2118007550016,1.76466578245163,48.5));
#83577=CARTESIAN_POINT('Ctrl Pts',(71.3386084446684,1.9447478055954,48.5));
#83578=CARTESIAN_POINT('Ctrl Pts',(71.3386084446684,2.48499327898026,48.5));
#83579=CARTESIAN_POINT('',(71.2118007550016,1.76466578245163,48.35));
#83580=CARTESIAN_POINT('',(71.2118007550016,1.76466578245163,48.5));
#83581=CARTESIAN_POINT('Ctrl Pts',(71.2118007550016,1.76466578245163,48.35));
#83582=CARTESIAN_POINT('Ctrl Pts',(71.3386084446684,1.9447478055954,48.35));
#83583=CARTESIAN_POINT('Ctrl Pts',(71.3386084446684,2.48499327898026,48.35));
#83584=CARTESIAN_POINT('Ctrl Pts',(70.898908556439,1.58458405733109,48.5));
#83585=CARTESIAN_POINT('Ctrl Pts',(70.898908556439,1.58458405733109,48.35));
#83586=CARTESIAN_POINT('Ctrl Pts',(71.0849930653349,1.58458405733109,48.5));
#83587=CARTESIAN_POINT('Ctrl Pts',(71.0849930653349,1.58458405733109,48.35));
#83588=CARTESIAN_POINT('Ctrl Pts',(71.2118007550016,1.76466578245163,48.5));
#83589=CARTESIAN_POINT('Ctrl Pts',(71.2118007550016,1.76466578245163,48.35));
#83590=CARTESIAN_POINT('',(70.898908556439,1.58458405733109,48.5));
#83591=CARTESIAN_POINT('Ctrl Pts',(70.898908556439,1.58458405733109,48.5));
#83592=CARTESIAN_POINT('Ctrl Pts',(71.0849930653349,1.58458405733109,48.5));
#83593=CARTESIAN_POINT('Ctrl Pts',(71.2118007550016,1.76466578245163,48.5));
#83594=CARTESIAN_POINT('',(70.898908556439,1.58458405733109,48.35));
#83595=CARTESIAN_POINT('',(70.898908556439,1.58458405733109,48.5));
#83596=CARTESIAN_POINT('Ctrl Pts',(70.898908556439,1.58458405733109,48.35));
#83597=CARTESIAN_POINT('Ctrl Pts',(71.0849930653349,1.58458405733109,48.35));
#83598=CARTESIAN_POINT('Ctrl Pts',(71.2118007550016,1.76466578245163,48.35));
#83599=CARTESIAN_POINT('Ctrl Pts',(70.5860163578764,1.76391565799713,48.5));
#83600=CARTESIAN_POINT('Ctrl Pts',(70.5860163578764,1.76391565799713,48.35));
#83601=CARTESIAN_POINT('Ctrl Pts',(70.7128240475431,1.58458405733109,48.5));
#83602=CARTESIAN_POINT('Ctrl Pts',(70.7128240475431,1.58458405733109,48.35));
#83603=CARTESIAN_POINT('Ctrl Pts',(70.898908556439,1.58458405733109,48.5));
#83604=CARTESIAN_POINT('Ctrl Pts',(70.898908556439,1.58458405733109,48.35));
#83605=CARTESIAN_POINT('',(70.5860163578764,1.76391565799713,48.5));
#83606=CARTESIAN_POINT('Ctrl Pts',(70.5860163578764,1.76391565799713,48.5));
#83607=CARTESIAN_POINT('Ctrl Pts',(70.7128240475431,1.58458405733109,48.5));
#83608=CARTESIAN_POINT('Ctrl Pts',(70.898908556439,1.58458405733109,48.5));
#83609=CARTESIAN_POINT('',(70.5860163578764,1.76391565799713,48.35));
#83610=CARTESIAN_POINT('',(70.5860163578764,1.76391565799713,48.5));
#83611=CARTESIAN_POINT('Ctrl Pts',(70.5860163578764,1.76391565799713,48.35));
#83612=CARTESIAN_POINT('Ctrl Pts',(70.7128240475431,1.58458405733109,48.35));
#83613=CARTESIAN_POINT('Ctrl Pts',(70.898908556439,1.58458405733109,48.35));
#83614=CARTESIAN_POINT('Ctrl Pts',(70.4592086682096,2.48499327898026,48.5));
#83615=CARTESIAN_POINT('Ctrl Pts',(70.4592086682096,2.48499327898026,48.35));
#83616=CARTESIAN_POINT('Ctrl Pts',(70.4592086682096,1.94324696063995,48.5));
#83617=CARTESIAN_POINT('Ctrl Pts',(70.4592086682096,1.94324696063995,48.35));
#83618=CARTESIAN_POINT('Ctrl Pts',(70.5860163578764,1.76391565799713,48.5));
#83619=CARTESIAN_POINT('Ctrl Pts',(70.5860163578764,1.76391565799713,48.35));
#83620=CARTESIAN_POINT('',(70.4592086682096,2.48499327898026,48.5));
#83621=CARTESIAN_POINT('Ctrl Pts',(70.4592086682096,2.48499327898026,48.5));
#83622=CARTESIAN_POINT('Ctrl Pts',(70.4592086682096,1.94324696063995,48.5));
#83623=CARTESIAN_POINT('Ctrl Pts',(70.5860163578764,1.76391565799713,48.5));
#83624=CARTESIAN_POINT('',(70.4592086682096,2.48499327898026,48.35));
#83625=CARTESIAN_POINT('',(70.4592086682096,2.48499327898026,48.5));
#83626=CARTESIAN_POINT('Ctrl Pts',(70.4592086682096,2.48499327898026,48.35));
#83627=CARTESIAN_POINT('Ctrl Pts',(70.4592086682096,1.94324696063995,48.35));
#83628=CARTESIAN_POINT('Ctrl Pts',(70.5860163578764,1.76391565799713,48.35));
#83629=CARTESIAN_POINT('Ctrl Pts',(70.5987723479047,3.22783091664314,48.5));
#83630=CARTESIAN_POINT('Ctrl Pts',(70.5987723479047,3.22783091664314,48.35));
#83631=CARTESIAN_POINT('Ctrl Pts',(70.4592086682096,3.02673944830894,48.5));
#83632=CARTESIAN_POINT('Ctrl Pts',(70.4592086682096,3.02673944830894,48.35));
#83633=CARTESIAN_POINT('Ctrl Pts',(70.4592086682096,2.48499327898026,48.5));
#83634=CARTESIAN_POINT('Ctrl Pts',(70.4592086682096,2.48499327898026,48.35));
#83635=CARTESIAN_POINT('Ctrl Pts',(70.5987723479047,3.22783091664314,48.5));
#83636=CARTESIAN_POINT('Ctrl Pts',(70.4592086682096,3.02673944830894,48.5));
#83637=CARTESIAN_POINT('Ctrl Pts',(70.4592086682096,2.48499327898026,48.5));
#83638=CARTESIAN_POINT('Ctrl Pts',(70.5987723479047,3.22783091664314,48.35));
#83639=CARTESIAN_POINT('Ctrl Pts',(70.4592086682096,3.02673944830894,48.35));
#83640=CARTESIAN_POINT('Ctrl Pts',(70.4592086682096,2.48499327898026,48.35));
#83641=CARTESIAN_POINT('Ctrl Pts',(70.898908556439,1.36248314380646,48.5));
#83642=CARTESIAN_POINT('Ctrl Pts',(70.898908556439,1.36248314380646,48.35));
#83643=CARTESIAN_POINT('Ctrl Pts',(70.5807639965788,1.36248314380646,48.5));
#83644=CARTESIAN_POINT('Ctrl Pts',(70.5807639965788,1.36248314380646,48.35));
#83645=CARTESIAN_POINT('Ctrl Pts',(70.3991814265028,1.59058684110642,48.5));
#83646=CARTESIAN_POINT('Ctrl Pts',(70.3991814265028,1.59058684110642,48.35));
#83647=CARTESIAN_POINT('',(70.898908556439,1.36248314380646,48.5));
#83648=CARTESIAN_POINT('',(70.3991814265028,1.59058684110642,48.5));
#83649=CARTESIAN_POINT('Ctrl Pts',(70.898908556439,1.36248314380646,48.5));
#83650=CARTESIAN_POINT('Ctrl Pts',(70.5807639965788,1.36248314380646,48.5));
#83651=CARTESIAN_POINT('Ctrl Pts',(70.3991814265028,1.59058684110642,48.5));
#83652=CARTESIAN_POINT('',(70.898908556439,1.36248314380646,48.35));
#83653=CARTESIAN_POINT('',(70.898908556439,1.36248314380646,48.5));
#83654=CARTESIAN_POINT('',(70.3991814265028,1.59058684110642,48.35));
#83655=CARTESIAN_POINT('Ctrl Pts',(70.898908556439,1.36248314380646,48.35));
#83656=CARTESIAN_POINT('Ctrl Pts',(70.5807639965788,1.36248314380646,48.35));
#83657=CARTESIAN_POINT('Ctrl Pts',(70.3991814265028,1.59058684110642,48.35));
#83658=CARTESIAN_POINT('',(70.3991814265028,1.59058684110642,48.5));
#83659=CARTESIAN_POINT('Ctrl Pts',(71.2988402256742,1.49229192733765,48.5));
#83660=CARTESIAN_POINT('Ctrl Pts',(71.2988402256742,1.49229192733765,48.35));
#83661=CARTESIAN_POINT('Ctrl Pts',(71.1405183682218,1.36248314380646,48.5));
#83662=CARTESIAN_POINT('Ctrl Pts',(71.1405183682218,1.36248314380646,48.35));
#83663=CARTESIAN_POINT('Ctrl Pts',(70.898908556439,1.36248314380646,48.5));
#83664=CARTESIAN_POINT('Ctrl Pts',(70.898908556439,1.36248314380646,48.35));
#83665=CARTESIAN_POINT('',(71.2988402256742,1.49229192733765,48.5));
#83666=CARTESIAN_POINT('Ctrl Pts',(71.2988402256742,1.49229192733765,48.5));
#83667=CARTESIAN_POINT('Ctrl Pts',(71.1405183682218,1.36248314380646,48.5));
#83668=CARTESIAN_POINT('Ctrl Pts',(70.898908556439,1.36248314380646,48.5));
#83669=CARTESIAN_POINT('',(71.2988402256742,1.49229192733765,48.35));
#83670=CARTESIAN_POINT('',(71.2988402256742,1.49229192733765,48.5));
#83671=CARTESIAN_POINT('Ctrl Pts',(71.2988402256742,1.49229192733765,48.35));
#83672=CARTESIAN_POINT('Ctrl Pts',(71.1405183682218,1.36248314380646,48.35));
#83673=CARTESIAN_POINT('Ctrl Pts',(70.898908556439,1.36248314380646,48.35));
#83674=CARTESIAN_POINT('Ctrl Pts',(71.5366985211149,1.85995900630951,48.5));
#83675=CARTESIAN_POINT('Ctrl Pts',(71.5366985211149,1.85995900630951,48.35));
#83676=CARTESIAN_POINT('Ctrl Pts',(71.4571620831266,1.62210100889206,48.5));
#83677=CARTESIAN_POINT('Ctrl Pts',(71.4571620831266,1.62210100889206,48.35));
#83678=CARTESIAN_POINT('Ctrl Pts',(71.2988402256742,1.49229192733765,48.5));
#83679=CARTESIAN_POINT('Ctrl Pts',(71.2988402256742,1.49229192733765,48.35));
#83680=CARTESIAN_POINT('',(71.5366985211149,1.85995900630951,48.5));
#83681=CARTESIAN_POINT('Ctrl Pts',(71.5366985211149,1.85995900630951,48.5));
#83682=CARTESIAN_POINT('Ctrl Pts',(71.4571620831266,1.62210100889206,48.5));
#83683=CARTESIAN_POINT('Ctrl Pts',(71.2988402256742,1.49229192733765,48.5));
#83684=CARTESIAN_POINT('',(71.5366985211149,1.85995900630951,48.35));
#83685=CARTESIAN_POINT('',(71.5366985211149,1.85995900630951,48.5));
#83686=CARTESIAN_POINT('Ctrl Pts',(71.5366985211149,1.85995900630951,48.35));
#83687=CARTESIAN_POINT('Ctrl Pts',(71.4571620831266,1.62210100889206,48.35));
#83688=CARTESIAN_POINT('Ctrl Pts',(71.2988402256742,1.49229192733765,48.35));
#83689=CARTESIAN_POINT('Ctrl Pts',(71.6162343630567,2.48499327898026,48.5));
#83690=CARTESIAN_POINT('Ctrl Pts',(71.6162343630567,2.48499327898026,48.35));
#83691=CARTESIAN_POINT('Ctrl Pts',(71.6162343630567,2.09781730175018,48.5));
#83692=CARTESIAN_POINT('Ctrl Pts',(71.6162343630567,2.09781730175018,48.35));
#83693=CARTESIAN_POINT('Ctrl Pts',(71.5366985211149,1.85995900630951,48.5));
#83694=CARTESIAN_POINT('Ctrl Pts',(71.5366985211149,1.85995900630951,48.35));
#83695=CARTESIAN_POINT('',(71.6162343630567,2.48499327898026,48.5));
#83696=CARTESIAN_POINT('Ctrl Pts',(71.6162343630567,2.48499327898026,48.5));
#83697=CARTESIAN_POINT('Ctrl Pts',(71.6162343630567,2.09781730175018,48.5));
#83698=CARTESIAN_POINT('Ctrl Pts',(71.5366985211149,1.85995900630951,48.5));
#83699=CARTESIAN_POINT('',(71.6162343630567,2.48499327898026,48.35));
#83700=CARTESIAN_POINT('',(71.6162343630567,2.48499327898026,48.5));
#83701=CARTESIAN_POINT('Ctrl Pts',(71.6162343630567,2.48499327898026,48.35));
#83702=CARTESIAN_POINT('Ctrl Pts',(71.6162343630567,2.09781730175018,48.35));
#83703=CARTESIAN_POINT('Ctrl Pts',(71.5366985211149,1.85995900630951,48.35));
#83704=CARTESIAN_POINT('Ctrl Pts',(71.5667118439451,3.00497958064079,48.5));
#83705=CARTESIAN_POINT('Ctrl Pts',(71.5667118439451,3.00497958064079,48.35));
#83706=CARTESIAN_POINT('Ctrl Pts',(71.6162343630567,2.81214186549187,48.5));
#83707=CARTESIAN_POINT('Ctrl Pts',(71.6162343630567,2.81214186549187,48.35));
#83708=CARTESIAN_POINT('Ctrl Pts',(71.6162343630567,2.48499327898026,48.5));
#83709=CARTESIAN_POINT('Ctrl Pts',(71.6162343630567,2.48499327898026,48.35));
#83710=CARTESIAN_POINT('',(71.5667118439451,3.00497958064079,48.5));
#83711=CARTESIAN_POINT('Ctrl Pts',(71.5667118439451,3.00497958064079,48.5));
#83712=CARTESIAN_POINT('Ctrl Pts',(71.6162343630567,2.81214186549187,48.5));
#83713=CARTESIAN_POINT('Ctrl Pts',(71.6162343630567,2.48499327898026,48.5));
#83714=CARTESIAN_POINT('',(71.5667118439451,3.00497958064079,48.35));
#83715=CARTESIAN_POINT('',(71.5667118439451,3.00497958064079,48.5));
#83716=CARTESIAN_POINT('Ctrl Pts',(71.5667118439451,3.00497958064079,48.35));
#83717=CARTESIAN_POINT('Ctrl Pts',(71.6162343630567,2.81214186549187,48.35));
#83718=CARTESIAN_POINT('Ctrl Pts',(71.6162343630567,2.48499327898026,48.35));
#83719=CARTESIAN_POINT('Ctrl Pts',(71.4301498541608,3.33212831616402,48.5));
#83720=CARTESIAN_POINT('Ctrl Pts',(71.4301498541608,3.33212831616402,48.35));
#83721=CARTESIAN_POINT('Ctrl Pts',(71.5171893248335,3.19781729578972,48.5));
#83722=CARTESIAN_POINT('Ctrl Pts',(71.5171893248335,3.19781729578972,48.35));
#83723=CARTESIAN_POINT('Ctrl Pts',(71.5667118439451,3.00497958064079,48.5));
#83724=CARTESIAN_POINT('Ctrl Pts',(71.5667118439451,3.00497958064079,48.35));
#83725=CARTESIAN_POINT('',(71.4301498541608,3.33212831616402,48.5));
#83726=CARTESIAN_POINT('Ctrl Pts',(71.4301498541608,3.33212831616402,48.5));
#83727=CARTESIAN_POINT('Ctrl Pts',(71.5171893248335,3.19781729578972,48.5));
#83728=CARTESIAN_POINT('Ctrl Pts',(71.5667118439451,3.00497958064079,48.5));
#83729=CARTESIAN_POINT('',(71.4301498541608,3.33212831616402,48.35));
#83730=CARTESIAN_POINT('',(71.4301498541608,3.33212831616402,48.5));
#83731=CARTESIAN_POINT('Ctrl Pts',(71.4301498541608,3.33212831616402,48.35));
#83732=CARTESIAN_POINT('Ctrl Pts',(71.5171893248335,3.19781729578972,48.35));
#83733=CARTESIAN_POINT('Ctrl Pts',(71.5667118439451,3.00497958064079,48.35));
#83734=CARTESIAN_POINT('Ctrl Pts',(71.2095500836149,3.5377217233181,48.5));
#83735=CARTESIAN_POINT('Ctrl Pts',(71.2095500836149,3.5377217233181,48.35));
#83736=CARTESIAN_POINT('Ctrl Pts',(71.3431103834882,3.46643933653831,48.5));
#83737=CARTESIAN_POINT('Ctrl Pts',(71.3431103834882,3.46643933653831,48.35));
#83738=CARTESIAN_POINT('Ctrl Pts',(71.4301498541608,3.33212831616402,48.5));
#83739=CARTESIAN_POINT('Ctrl Pts',(71.4301498541608,3.33212831616402,48.35));
#83740=CARTESIAN_POINT('',(71.2095500836149,3.5377217233181,48.5));
#83741=CARTESIAN_POINT('Ctrl Pts',(71.2095500836149,3.5377217233181,48.5));
#83742=CARTESIAN_POINT('Ctrl Pts',(71.3431103834882,3.46643933653831,48.5));
#83743=CARTESIAN_POINT('Ctrl Pts',(71.4301498541608,3.33212831616402,48.5));
#83744=CARTESIAN_POINT('',(71.2095500836149,3.5377217233181,48.35));
#83745=CARTESIAN_POINT('',(71.2095500836149,3.5377217233181,48.5));
#83746=CARTESIAN_POINT('Ctrl Pts',(71.2095500836149,3.5377217233181,48.35));
#83747=CARTESIAN_POINT('Ctrl Pts',(71.3431103834882,3.46643933653831,48.35));
#83748=CARTESIAN_POINT('Ctrl Pts',(71.4301498541608,3.33212831616402,48.35));
#83749=CARTESIAN_POINT('Ctrl Pts',(70.898908556439,3.60900411009789,48.5));
#83750=CARTESIAN_POINT('Ctrl Pts',(70.898908556439,3.60900411009789,48.35));
#83751=CARTESIAN_POINT('Ctrl Pts',(71.0759891876951,3.60900411009789,48.5));
#83752=CARTESIAN_POINT('Ctrl Pts',(71.0759891876951,3.60900411009789,48.35));
#83753=CARTESIAN_POINT('Ctrl Pts',(71.2095500836149,3.5377217233181,48.5));
#83754=CARTESIAN_POINT('Ctrl Pts',(71.2095500836149,3.5377217233181,48.35));
#83755=CARTESIAN_POINT('',(70.898908556439,3.60900411009789,48.5));
#83756=CARTESIAN_POINT('Ctrl Pts',(70.898908556439,3.60900411009789,48.5));
#83757=CARTESIAN_POINT('Ctrl Pts',(71.0759891876951,3.60900411009789,48.5));
#83758=CARTESIAN_POINT('Ctrl Pts',(71.2095500836149,3.5377217233181,48.5));
#83759=CARTESIAN_POINT('',(70.898908556439,3.60900411009789,48.35));
#83760=CARTESIAN_POINT('',(70.898908556439,3.60900411009789,48.5));
#83761=CARTESIAN_POINT('Ctrl Pts',(70.898908556439,3.60900411009789,48.35));
#83762=CARTESIAN_POINT('Ctrl Pts',(71.0759891876951,3.60900411009789,48.35));
#83763=CARTESIAN_POINT('Ctrl Pts',(71.2095500836149,3.5377217233181,48.35));
#83764=CARTESIAN_POINT('Ctrl Pts',(70.5004777321592,3.47994545102119,48.5));
#83765=CARTESIAN_POINT('Ctrl Pts',(70.5004777321592,3.47994545102119,48.35));
#83766=CARTESIAN_POINT('Ctrl Pts',(70.6587995896116,3.60900411009789,48.5));
#83767=CARTESIAN_POINT('Ctrl Pts',(70.6587995896116,3.60900411009789,48.35));
#83768=CARTESIAN_POINT('Ctrl Pts',(70.898908556439,3.60900411009789,48.5));
#83769=CARTESIAN_POINT('Ctrl Pts',(70.898908556439,3.60900411009789,48.35));
#83770=CARTESIAN_POINT('',(70.5004777321592,3.47994545102119,48.5));
#83771=CARTESIAN_POINT('Ctrl Pts',(70.5004777321592,3.47994545102119,48.5));
#83772=CARTESIAN_POINT('Ctrl Pts',(70.6587995896116,3.60900411009789,48.5));
#83773=CARTESIAN_POINT('Ctrl Pts',(70.898908556439,3.60900411009789,48.5));
#83774=CARTESIAN_POINT('',(70.5004777321592,3.47994545102119,48.35));
#83775=CARTESIAN_POINT('',(70.5004777321592,3.47994545102119,48.5));
#83776=CARTESIAN_POINT('Ctrl Pts',(70.5004777321592,3.47994545102119,48.35));
#83777=CARTESIAN_POINT('Ctrl Pts',(70.6587995896116,3.60900411009789,48.35));
#83778=CARTESIAN_POINT('Ctrl Pts',(70.898908556439,3.60900411009789,48.35));
#83779=CARTESIAN_POINT('Ctrl Pts',(70.2618690142408,3.11302864551544,48.5));
#83780=CARTESIAN_POINT('Ctrl Pts',(70.2618690142408,3.11302864551544,48.35));
#83781=CARTESIAN_POINT('Ctrl Pts',(70.3421555766836,3.3508867919445,48.5));
#83782=CARTESIAN_POINT('Ctrl Pts',(70.3421555766836,3.3508867919445,48.35));
#83783=CARTESIAN_POINT('Ctrl Pts',(70.5004777321592,3.47994545102119,48.5));
#83784=CARTESIAN_POINT('Ctrl Pts',(70.5004777321592,3.47994545102119,48.35));
#83785=CARTESIAN_POINT('',(70.2618690142408,3.11302864551544,48.5));
#83786=CARTESIAN_POINT('Ctrl Pts',(70.2618690142408,3.11302864551544,48.5));
#83787=CARTESIAN_POINT('Ctrl Pts',(70.3421555766836,3.3508867919445,48.5));
#83788=CARTESIAN_POINT('Ctrl Pts',(70.5004777321592,3.47994545102119,48.5));
#83789=CARTESIAN_POINT('',(70.2618690142408,3.11302864551544,48.35));
#83790=CARTESIAN_POINT('',(70.2618690142408,3.11302864551544,48.5));
#83791=CARTESIAN_POINT('Ctrl Pts',(70.2618690142408,3.11302864551544,48.35));
#83792=CARTESIAN_POINT('Ctrl Pts',(70.3421555766836,3.3508867919445,48.35));
#83793=CARTESIAN_POINT('Ctrl Pts',(70.5004777321592,3.47994545102119,48.35));
#83794=CARTESIAN_POINT('Ctrl Pts',(70.1815827498212,2.48499327898026,48.5));
#83795=CARTESIAN_POINT('Ctrl Pts',(70.1815827498212,2.48499327898026,48.35));
#83796=CARTESIAN_POINT('Ctrl Pts',(70.1815827498212,2.87517049908638,48.5));
#83797=CARTESIAN_POINT('Ctrl Pts',(70.1815827498212,2.87517049908638,48.35));
#83798=CARTESIAN_POINT('Ctrl Pts',(70.2618690142408,3.11302864551544,48.5));
#83799=CARTESIAN_POINT('Ctrl Pts',(70.2618690142408,3.11302864551544,48.35));
#83800=CARTESIAN_POINT('',(70.1815827498212,2.48499327898026,48.5));
#83801=CARTESIAN_POINT('Ctrl Pts',(70.1815827498212,2.48499327898026,48.5));
#83802=CARTESIAN_POINT('Ctrl Pts',(70.1815827498212,2.87517049908638,48.5));
#83803=CARTESIAN_POINT('Ctrl Pts',(70.2618690142408,3.11302864551544,48.5));
#83804=CARTESIAN_POINT('',(70.1815827498212,2.48499327898026,48.35));
#83805=CARTESIAN_POINT('',(70.1815827498212,2.48499327898026,48.5));
#83806=CARTESIAN_POINT('Ctrl Pts',(70.1815827498212,2.48499327898026,48.35));
#83807=CARTESIAN_POINT('Ctrl Pts',(70.1815827498212,2.87517049908638,48.35));
#83808=CARTESIAN_POINT('Ctrl Pts',(70.2618690142408,3.11302864551544,48.35));
#83809=CARTESIAN_POINT('Ctrl Pts',(70.3991814265028,1.59058684110642,48.5));
#83810=CARTESIAN_POINT('Ctrl Pts',(70.3991814265028,1.59058684110642,48.35));
#83811=CARTESIAN_POINT('Ctrl Pts',(70.1815827498212,1.86521166563034,48.5));
#83812=CARTESIAN_POINT('Ctrl Pts',(70.1815827498212,1.86521166563034,48.35));
#83813=CARTESIAN_POINT('Ctrl Pts',(70.1815827498212,2.48499327898026,48.5));
#83814=CARTESIAN_POINT('Ctrl Pts',(70.1815827498212,2.48499327898026,48.35));
#83815=CARTESIAN_POINT('Ctrl Pts',(70.3991814265028,1.59058684110642,48.5));
#83816=CARTESIAN_POINT('Ctrl Pts',(70.1815827498212,1.86521166563034,48.5));
#83817=CARTESIAN_POINT('Ctrl Pts',(70.1815827498212,2.48499327898026,48.5));
#83818=CARTESIAN_POINT('Ctrl Pts',(70.3991814265028,1.59058684110642,48.35));
#83819=CARTESIAN_POINT('Ctrl Pts',(70.1815827498212,1.86521166563034,48.35));
#83820=CARTESIAN_POINT('Ctrl Pts',(70.1815827498212,2.48499327898026,48.35));
#83821=CARTESIAN_POINT('Origin',(69.9999999562278,2.48574362695217,48.35));
#83822=CARTESIAN_POINT('Origin',(69.3381993779913,3.16630297899246,48.5));
#83823=CARTESIAN_POINT('',(69.3381993779913,3.16630297899246,48.5));
#83824=CARTESIAN_POINT('',(68.6493861982599,2.17435204982758,48.5));
#83825=CARTESIAN_POINT('',(59.1917638899362,-11.4454472114045,48.5));
#83826=CARTESIAN_POINT('',(69.3381993779913,3.16630297899246,48.35));
#83827=CARTESIAN_POINT('',(69.3381993779913,3.16630297899246,48.5));
#83828=CARTESIAN_POINT('',(68.6493861982599,2.17435204982758,48.35));
#83829=CARTESIAN_POINT('',(69.3381993779913,3.16630297899246,48.35));
#83830=CARTESIAN_POINT('',(68.6493861982599,2.17435204982758,48.5));
#83831=CARTESIAN_POINT('Origin',(69.3381993779913,2.17435204982758,48.5));
#83832=CARTESIAN_POINT('',(69.3381993779913,2.17435204982758,48.5));
#83833=CARTESIAN_POINT('',(69.3381993779913,5.08717602491379,48.5));
#83834=CARTESIAN_POINT('',(69.3381993779913,2.17435204982758,48.35));
#83835=CARTESIAN_POINT('',(69.3381993779913,2.17435204982758,48.5));
#83836=CARTESIAN_POINT('',(69.3381993779913,2.17435204982758,48.35));
#83837=CARTESIAN_POINT('Origin',(68.6493861982599,2.17435204982758,48.5));
#83838=CARTESIAN_POINT('',(34.3246930991299,2.17435204982758,48.5));
#83839=CARTESIAN_POINT('',(68.6493861982599,2.17435204982758,48.35));
#83840=CARTESIAN_POINT('Origin',(69.6083219656721,1.92673945426941,48.5));
#83841=CARTESIAN_POINT('',(69.6083219656721,1.92673945426941,48.5));
#83842=CARTESIAN_POINT('',(69.6083219656721,1.40000009536743,48.5));
#83843=CARTESIAN_POINT('',(69.6083219656721,4.9633697271347,48.5));
#83844=CARTESIAN_POINT('',(69.6083219656721,1.92673945426941,48.35));
#83845=CARTESIAN_POINT('',(69.6083219656721,1.92673945426941,48.5));
#83846=CARTESIAN_POINT('',(69.6083219656721,1.40000009536743,48.35));
#83847=CARTESIAN_POINT('',(69.6083219656721,1.92673945426941,48.35));
#83848=CARTESIAN_POINT('',(69.6083219656721,1.40000009536743,48.5));
#83849=CARTESIAN_POINT('Origin',(69.9054570803419,1.92673945426941,48.5));
#83850=CARTESIAN_POINT('',(69.9054570803419,1.92673945426941,48.5));
#83851=CARTESIAN_POINT('',(34.9527285401709,1.92673945426941,48.5));
#83852=CARTESIAN_POINT('',(69.9054570803419,1.92673945426941,48.35));
#83853=CARTESIAN_POINT('',(69.9054570803419,1.92673945426941,48.5));
#83854=CARTESIAN_POINT('',(69.9054570803419,1.92673945426941,48.35));
#83855=CARTESIAN_POINT('Origin',(69.9054570803419,2.17435204982758,48.5));
#83856=CARTESIAN_POINT('',(69.9054570803419,2.17435204982758,48.5));
#83857=CARTESIAN_POINT('',(69.9054570803419,5.08717602491379,48.5));
#83858=CARTESIAN_POINT('',(69.9054570803419,2.17435204982758,48.35));
#83859=CARTESIAN_POINT('',(69.9054570803419,2.17435204982758,48.5));
#83860=CARTESIAN_POINT('',(69.9054570803419,2.17435204982758,48.35));
#83861=CARTESIAN_POINT('Origin',(69.6083219656721,2.17435204982758,48.5));
#83862=CARTESIAN_POINT('',(69.6083219656721,2.17435204982758,48.5));
#83863=CARTESIAN_POINT('',(34.804160982836,2.17435204982758,48.5));
#83864=CARTESIAN_POINT('',(69.6083219656721,2.17435204982758,48.35));
#83865=CARTESIAN_POINT('',(69.6083219656721,2.17435204982758,48.5));
#83866=CARTESIAN_POINT('',(69.6083219656721,2.17435204982758,48.35));
#83867=CARTESIAN_POINT('Origin',(69.6083219656721,3.6000000834465,48.5));
#83868=CARTESIAN_POINT('',(69.6083219656721,3.6000000834465,48.5));
#83869=CARTESIAN_POINT('',(69.6083219656721,5.80000004172325,48.5));
#83870=CARTESIAN_POINT('',(69.6083219656721,3.6000000834465,48.35));
#83871=CARTESIAN_POINT('',(69.6083219656721,3.6000000834465,48.5));
#83872=CARTESIAN_POINT('',(69.6083219656721,3.6000000834465,48.35));
#83873=CARTESIAN_POINT('Origin',(69.3877218971029,3.6000000834465,48.5));
#83874=CARTESIAN_POINT('',(69.3877218971029,3.6000000834465,48.5));
#83875=CARTESIAN_POINT('',(34.6938609485514,3.6000000834465,48.5));
#83876=CARTESIAN_POINT('',(69.3877218971029,3.6000000834465,48.35));
#83877=CARTESIAN_POINT('',(69.3877218971029,3.6000000834465,48.5));
#83878=CARTESIAN_POINT('',(69.3877218971029,3.6000000834465,48.35));
#83879=CARTESIAN_POINT('Origin',(68.383765549399,2.17435204982758,48.5));
#83880=CARTESIAN_POINT('',(68.383765549399,2.17435204982758,48.5));
#83881=CARTESIAN_POINT('',(58.4199877035187,-11.9745104240059,48.5));
#83882=CARTESIAN_POINT('',(68.383765549399,2.17435204982758,48.35));
#83883=CARTESIAN_POINT('',(68.383765549399,2.17435204982758,48.5));
#83884=CARTESIAN_POINT('',(68.383765549399,2.17435204982758,48.35));
#83885=CARTESIAN_POINT('Origin',(68.383765549399,1.92673945426941,48.5));
#83886=CARTESIAN_POINT('',(68.383765549399,1.92673945426941,48.5));
#83887=CARTESIAN_POINT('',(68.383765549399,4.9633697271347,48.5));
#83888=CARTESIAN_POINT('',(68.383765549399,1.92673945426941,48.35));
#83889=CARTESIAN_POINT('',(68.383765549399,1.92673945426941,48.5));
#83890=CARTESIAN_POINT('',(68.383765549399,1.92673945426941,48.35));
#83891=CARTESIAN_POINT('Origin',(69.3381993779913,1.92673945426941,48.5));
#83892=CARTESIAN_POINT('',(69.3381993779913,1.92673945426941,48.5));
#83893=CARTESIAN_POINT('',(34.6690996889956,1.92673945426941,48.5));
#83894=CARTESIAN_POINT('',(69.3381993779913,1.92673945426941,48.35));
#83895=CARTESIAN_POINT('',(69.3381993779913,1.92673945426941,48.5));
#83896=CARTESIAN_POINT('',(69.3381993779913,1.92673945426941,48.35));
#83897=CARTESIAN_POINT('Origin',(69.3381993779913,1.40000009536743,48.5));
#83898=CARTESIAN_POINT('',(69.3381993779913,1.40000009536743,48.5));
#83899=CARTESIAN_POINT('',(69.3381993779913,4.70000004768372,48.5));
#83900=CARTESIAN_POINT('',(69.3381993779913,1.40000009536743,48.35));
#83901=CARTESIAN_POINT('',(69.3381993779913,1.40000009536743,48.5));
#83902=CARTESIAN_POINT('',(69.3381993779913,1.40000009536743,48.35));
#83903=CARTESIAN_POINT('Origin',(69.6083219656721,1.40000009536743,48.5));
#83904=CARTESIAN_POINT('',(34.804160982836,1.40000009536743,48.5));
#83905=CARTESIAN_POINT('',(69.6083219656721,1.40000009536743,48.35));
#83906=CARTESIAN_POINT('Origin',(69.9999999562278,2.48574362695217,48.35));
#83907=CARTESIAN_POINT('Origin',(0.,8.,48.5));
#83908=CARTESIAN_POINT('Origin',(0.,8.,48.5));
#83909=CARTESIAN_POINT('Ctrl Pts',(60.8516373746097,3.38540250062943,48.5));
#83910=CARTESIAN_POINT('Ctrl Pts',(60.8516373746097,3.38540250062943,48.35));
#83911=CARTESIAN_POINT('Ctrl Pts',(60.6655525676906,3.38540250062943,48.5));
#83912=CARTESIAN_POINT('Ctrl Pts',(60.6655525676906,3.38540250062943,48.35));
#83913=CARTESIAN_POINT('Ctrl Pts',(60.5545022599399,3.22783091664314,48.5));
#83914=CARTESIAN_POINT('Ctrl Pts',(60.5545022599399,3.22783091664314,48.35));
#83915=CARTESIAN_POINT('',(60.8516373746097,3.38540250062943,48.5));
#83916=CARTESIAN_POINT('',(60.5545022599399,3.22783091664314,48.5));
#83917=CARTESIAN_POINT('Ctrl Pts',(60.8516373746097,3.38540250062943,48.5));
#83918=CARTESIAN_POINT('Ctrl Pts',(60.6655525676906,3.38540250062943,48.5));
#83919=CARTESIAN_POINT('Ctrl Pts',(60.5545022599399,3.22783091664314,48.5));
#83920=CARTESIAN_POINT('',(60.8516373746097,3.38540250062943,48.35));
#83921=CARTESIAN_POINT('',(60.8516373746097,3.38540250062943,48.5));
#83922=CARTESIAN_POINT('',(60.5545022599399,3.22783091664314,48.35));
#83923=CARTESIAN_POINT('Ctrl Pts',(60.8516373746097,3.38540250062943,48.35));
#83924=CARTESIAN_POINT('Ctrl Pts',(60.6655525676906,3.38540250062943,48.35));
#83925=CARTESIAN_POINT('Ctrl Pts',(60.5545022599399,3.22783091664314,48.35));
#83926=CARTESIAN_POINT('',(60.5545022599399,3.22783091664314,48.5));
#83927=CARTESIAN_POINT('Ctrl Pts',(61.1675306670368,3.2068213224411,48.5));
#83928=CARTESIAN_POINT('Ctrl Pts',(61.1675306670368,3.2068213224411,48.35));
#83929=CARTESIAN_POINT('Ctrl Pts',(61.04072297737,3.38540250062943,48.5));
#83930=CARTESIAN_POINT('Ctrl Pts',(61.04072297737,3.38540250062943,48.35));
#83931=CARTESIAN_POINT('Ctrl Pts',(60.8516373746097,3.38540250062943,48.5));
#83932=CARTESIAN_POINT('Ctrl Pts',(60.8516373746097,3.38540250062943,48.35));
#83933=CARTESIAN_POINT('',(61.1675306670368,3.2068213224411,48.5));
#83934=CARTESIAN_POINT('Ctrl Pts',(61.1675306670368,3.2068213224411,48.5));
#83935=CARTESIAN_POINT('Ctrl Pts',(61.04072297737,3.38540250062943,48.5));
#83936=CARTESIAN_POINT('Ctrl Pts',(60.8516373746097,3.38540250062943,48.5));
#83937=CARTESIAN_POINT('',(61.1675306670368,3.2068213224411,48.35));
#83938=CARTESIAN_POINT('',(61.1675306670368,3.2068213224411,48.5));
#83939=CARTESIAN_POINT('Ctrl Pts',(61.1675306670368,3.2068213224411,48.35));
#83940=CARTESIAN_POINT('Ctrl Pts',(61.04072297737,3.38540250062943,48.35));
#83941=CARTESIAN_POINT('Ctrl Pts',(60.8516373746097,3.38540250062943,48.35));
#83942=CARTESIAN_POINT('Ctrl Pts',(61.2943383567035,2.48499327898026,48.5));
#83943=CARTESIAN_POINT('Ctrl Pts',(61.2943383567035,2.48499327898026,48.35));
#83944=CARTESIAN_POINT('Ctrl Pts',(61.2943383567035,3.02824014425278,48.5));
#83945=CARTESIAN_POINT('Ctrl Pts',(61.2943383567035,3.02824014425278,48.35));
#83946=CARTESIAN_POINT('Ctrl Pts',(61.1675306670368,3.2068213224411,48.5));
#83947=CARTESIAN_POINT('Ctrl Pts',(61.1675306670368,3.2068213224411,48.35));
#83948=CARTESIAN_POINT('',(61.2943383567035,2.48499327898026,48.5));
#83949=CARTESIAN_POINT('Ctrl Pts',(61.2943383567035,2.48499327898026,48.5));
#83950=CARTESIAN_POINT('Ctrl Pts',(61.2943383567035,3.02824014425278,48.5));
#83951=CARTESIAN_POINT('Ctrl Pts',(61.1675306670368,3.2068213224411,48.5));
#83952=CARTESIAN_POINT('',(61.2943383567035,2.48499327898026,48.35));
#83953=CARTESIAN_POINT('',(61.2943383567035,2.48499327898026,48.5));
#83954=CARTESIAN_POINT('Ctrl Pts',(61.2943383567035,2.48499327898026,48.35));
#83955=CARTESIAN_POINT('Ctrl Pts',(61.2943383567035,3.02824014425278,48.35));
#83956=CARTESIAN_POINT('Ctrl Pts',(61.1675306670368,3.2068213224411,48.35));
#83957=CARTESIAN_POINT('Ctrl Pts',(61.1675306670368,1.76466578245163,48.5));
#83958=CARTESIAN_POINT('Ctrl Pts',(61.1675306670368,1.76466578245163,48.35));
#83959=CARTESIAN_POINT('Ctrl Pts',(61.2943383567035,1.9447478055954,48.5));
#83960=CARTESIAN_POINT('Ctrl Pts',(61.2943383567035,1.9447478055954,48.35));
#83961=CARTESIAN_POINT('Ctrl Pts',(61.2943383567035,2.48499327898026,48.5));
#83962=CARTESIAN_POINT('Ctrl Pts',(61.2943383567035,2.48499327898026,48.35));
#83963=CARTESIAN_POINT('',(61.1675306670368,1.76466578245163,48.5));
#83964=CARTESIAN_POINT('Ctrl Pts',(61.1675306670368,1.76466578245163,48.5));
#83965=CARTESIAN_POINT('Ctrl Pts',(61.2943383567035,1.9447478055954,48.5));
#83966=CARTESIAN_POINT('Ctrl Pts',(61.2943383567035,2.48499327898026,48.5));
#83967=CARTESIAN_POINT('',(61.1675306670368,1.76466578245163,48.35));
#83968=CARTESIAN_POINT('',(61.1675306670368,1.76466578245163,48.5));
#83969=CARTESIAN_POINT('Ctrl Pts',(61.1675306670368,1.76466578245163,48.35));
#83970=CARTESIAN_POINT('Ctrl Pts',(61.2943383567035,1.9447478055954,48.35));
#83971=CARTESIAN_POINT('Ctrl Pts',(61.2943383567035,2.48499327898026,48.35));
#83972=CARTESIAN_POINT('Ctrl Pts',(60.8546384684741,1.58458405733109,48.5));
#83973=CARTESIAN_POINT('Ctrl Pts',(60.8546384684741,1.58458405733109,48.35));
#83974=CARTESIAN_POINT('Ctrl Pts',(61.04072297737,1.58458405733109,48.5));
#83975=CARTESIAN_POINT('Ctrl Pts',(61.04072297737,1.58458405733109,48.35));
#83976=CARTESIAN_POINT('Ctrl Pts',(61.1675306670368,1.76466578245163,48.5));
#83977=CARTESIAN_POINT('Ctrl Pts',(61.1675306670368,1.76466578245163,48.35));
#83978=CARTESIAN_POINT('',(60.8546384684741,1.58458405733109,48.5));
#83979=CARTESIAN_POINT('Ctrl Pts',(60.8546384684741,1.58458405733109,48.5));
#83980=CARTESIAN_POINT('Ctrl Pts',(61.04072297737,1.58458405733109,48.5));
#83981=CARTESIAN_POINT('Ctrl Pts',(61.1675306670368,1.76466578245163,48.5));
#83982=CARTESIAN_POINT('',(60.8546384684741,1.58458405733109,48.35));
#83983=CARTESIAN_POINT('',(60.8546384684741,1.58458405733109,48.5));
#83984=CARTESIAN_POINT('Ctrl Pts',(60.8546384684741,1.58458405733109,48.35));
#83985=CARTESIAN_POINT('Ctrl Pts',(61.04072297737,1.58458405733109,48.35));
#83986=CARTESIAN_POINT('Ctrl Pts',(61.1675306670368,1.76466578245163,48.35));
#83987=CARTESIAN_POINT('Ctrl Pts',(60.5417462699115,1.76391565799713,48.5));
#83988=CARTESIAN_POINT('Ctrl Pts',(60.5417462699115,1.76391565799713,48.35));
#83989=CARTESIAN_POINT('Ctrl Pts',(60.6685539595783,1.58458405733109,48.5));
#83990=CARTESIAN_POINT('Ctrl Pts',(60.6685539595783,1.58458405733109,48.35));
#83991=CARTESIAN_POINT('Ctrl Pts',(60.8546384684741,1.58458405733109,48.5));
#83992=CARTESIAN_POINT('Ctrl Pts',(60.8546384684741,1.58458405733109,48.35));
#83993=CARTESIAN_POINT('',(60.5417462699115,1.76391565799713,48.5));
#83994=CARTESIAN_POINT('Ctrl Pts',(60.5417462699115,1.76391565799713,48.5));
#83995=CARTESIAN_POINT('Ctrl Pts',(60.6685539595783,1.58458405733109,48.5));
#83996=CARTESIAN_POINT('Ctrl Pts',(60.8546384684741,1.58458405733109,48.5));
#83997=CARTESIAN_POINT('',(60.5417462699115,1.76391565799713,48.35));
#83998=CARTESIAN_POINT('',(60.5417462699115,1.76391565799713,48.5));
#83999=CARTESIAN_POINT('Ctrl Pts',(60.5417462699115,1.76391565799713,48.35));
#84000=CARTESIAN_POINT('Ctrl Pts',(60.6685539595783,1.58458405733109,48.35));
#84001=CARTESIAN_POINT('Ctrl Pts',(60.8546384684741,1.58458405733109,48.35));
#84002=CARTESIAN_POINT('Ctrl Pts',(60.4149385802448,2.48499327898026,48.5));
#84003=CARTESIAN_POINT('Ctrl Pts',(60.4149385802448,2.48499327898026,48.35));
#84004=CARTESIAN_POINT('Ctrl Pts',(60.4149385802448,1.94324696063995,48.5));
#84005=CARTESIAN_POINT('Ctrl Pts',(60.4149385802448,1.94324696063995,48.35));
#84006=CARTESIAN_POINT('Ctrl Pts',(60.5417462699115,1.76391565799713,48.5));
#84007=CARTESIAN_POINT('Ctrl Pts',(60.5417462699115,1.76391565799713,48.35));
#84008=CARTESIAN_POINT('',(60.4149385802448,2.48499327898026,48.5));
#84009=CARTESIAN_POINT('Ctrl Pts',(60.4149385802448,2.48499327898026,48.5));
#84010=CARTESIAN_POINT('Ctrl Pts',(60.4149385802448,1.94324696063995,48.5));
#84011=CARTESIAN_POINT('Ctrl Pts',(60.5417462699115,1.76391565799713,48.5));
#84012=CARTESIAN_POINT('',(60.4149385802448,2.48499327898026,48.35));
#84013=CARTESIAN_POINT('',(60.4149385802448,2.48499327898026,48.5));
#84014=CARTESIAN_POINT('Ctrl Pts',(60.4149385802448,2.48499327898026,48.35));
#84015=CARTESIAN_POINT('Ctrl Pts',(60.4149385802448,1.94324696063995,48.35));
#84016=CARTESIAN_POINT('Ctrl Pts',(60.5417462699115,1.76391565799713,48.35));
#84017=CARTESIAN_POINT('Ctrl Pts',(60.5545022599399,3.22783091664314,48.5));
#84018=CARTESIAN_POINT('Ctrl Pts',(60.5545022599399,3.22783091664314,48.35));
#84019=CARTESIAN_POINT('Ctrl Pts',(60.4149385802448,3.02673944830894,48.5));
#84020=CARTESIAN_POINT('Ctrl Pts',(60.4149385802448,3.02673944830894,48.35));
#84021=CARTESIAN_POINT('Ctrl Pts',(60.4149385802448,2.48499327898026,48.5));
#84022=CARTESIAN_POINT('Ctrl Pts',(60.4149385802448,2.48499327898026,48.35));
#84023=CARTESIAN_POINT('Ctrl Pts',(60.5545022599399,3.22783091664314,48.5));
#84024=CARTESIAN_POINT('Ctrl Pts',(60.4149385802448,3.02673944830894,48.5));
#84025=CARTESIAN_POINT('Ctrl Pts',(60.4149385802448,2.48499327898026,48.5));
#84026=CARTESIAN_POINT('Ctrl Pts',(60.5545022599399,3.22783091664314,48.35));
#84027=CARTESIAN_POINT('Ctrl Pts',(60.4149385802448,3.02673944830894,48.35));
#84028=CARTESIAN_POINT('Ctrl Pts',(60.4149385802448,2.48499327898026,48.35));
#84029=CARTESIAN_POINT('Ctrl Pts',(60.8546384684741,1.36248314380646,48.5));
#84030=CARTESIAN_POINT('Ctrl Pts',(60.8546384684741,1.36248314380646,48.35));
#84031=CARTESIAN_POINT('Ctrl Pts',(60.5364939086139,1.36248314380646,48.5));
#84032=CARTESIAN_POINT('Ctrl Pts',(60.5364939086139,1.36248314380646,48.35));
#84033=CARTESIAN_POINT('Ctrl Pts',(60.3549113385379,1.59058684110642,48.5));
#84034=CARTESIAN_POINT('Ctrl Pts',(60.3549113385379,1.59058684110642,48.35));
#84035=CARTESIAN_POINT('',(60.8546384684741,1.36248314380646,48.5));
#84036=CARTESIAN_POINT('',(60.3549113385379,1.59058684110642,48.5));
#84037=CARTESIAN_POINT('Ctrl Pts',(60.8546384684741,1.36248314380646,48.5));
#84038=CARTESIAN_POINT('Ctrl Pts',(60.5364939086139,1.36248314380646,48.5));
#84039=CARTESIAN_POINT('Ctrl Pts',(60.3549113385379,1.59058684110642,48.5));
#84040=CARTESIAN_POINT('',(60.8546384684741,1.36248314380646,48.35));
#84041=CARTESIAN_POINT('',(60.8546384684741,1.36248314380646,48.5));
#84042=CARTESIAN_POINT('',(60.3549113385379,1.59058684110642,48.35));
#84043=CARTESIAN_POINT('Ctrl Pts',(60.8546384684741,1.36248314380646,48.35));
#84044=CARTESIAN_POINT('Ctrl Pts',(60.5364939086139,1.36248314380646,48.35));
#84045=CARTESIAN_POINT('Ctrl Pts',(60.3549113385379,1.59058684110642,48.35));
#84046=CARTESIAN_POINT('',(60.3549113385379,1.59058684110642,48.5));
#84047=CARTESIAN_POINT('Ctrl Pts',(61.2545701377094,1.49229192733765,48.5));
#84048=CARTESIAN_POINT('Ctrl Pts',(61.2545701377094,1.49229192733765,48.35));
#84049=CARTESIAN_POINT('Ctrl Pts',(61.096248280257,1.36248314380646,48.5));
#84050=CARTESIAN_POINT('Ctrl Pts',(61.096248280257,1.36248314380646,48.35));
#84051=CARTESIAN_POINT('Ctrl Pts',(60.8546384684741,1.36248314380646,48.5));
#84052=CARTESIAN_POINT('Ctrl Pts',(60.8546384684741,1.36248314380646,48.35));
#84053=CARTESIAN_POINT('',(61.2545701377094,1.49229192733765,48.5));
#84054=CARTESIAN_POINT('Ctrl Pts',(61.2545701377094,1.49229192733765,48.5));
#84055=CARTESIAN_POINT('Ctrl Pts',(61.096248280257,1.36248314380646,48.5));
#84056=CARTESIAN_POINT('Ctrl Pts',(60.8546384684741,1.36248314380646,48.5));
#84057=CARTESIAN_POINT('',(61.2545701377094,1.49229192733765,48.35));
#84058=CARTESIAN_POINT('',(61.2545701377094,1.49229192733765,48.5));
#84059=CARTESIAN_POINT('Ctrl Pts',(61.2545701377094,1.49229192733765,48.35));
#84060=CARTESIAN_POINT('Ctrl Pts',(61.096248280257,1.36248314380646,48.35));
#84061=CARTESIAN_POINT('Ctrl Pts',(60.8546384684741,1.36248314380646,48.35));
#84062=CARTESIAN_POINT('Ctrl Pts',(61.4924284331501,1.85995900630951,48.5));
#84063=CARTESIAN_POINT('Ctrl Pts',(61.4924284331501,1.85995900630951,48.35));
#84064=CARTESIAN_POINT('Ctrl Pts',(61.4128919951618,1.62210100889206,48.5));
#84065=CARTESIAN_POINT('Ctrl Pts',(61.4128919951618,1.62210100889206,48.35));
#84066=CARTESIAN_POINT('Ctrl Pts',(61.2545701377094,1.49229192733765,48.5));
#84067=CARTESIAN_POINT('Ctrl Pts',(61.2545701377094,1.49229192733765,48.35));
#84068=CARTESIAN_POINT('',(61.4924284331501,1.85995900630951,48.5));
#84069=CARTESIAN_POINT('Ctrl Pts',(61.4924284331501,1.85995900630951,48.5));
#84070=CARTESIAN_POINT('Ctrl Pts',(61.4128919951618,1.62210100889206,48.5));
#84071=CARTESIAN_POINT('Ctrl Pts',(61.2545701377094,1.49229192733765,48.5));
#84072=CARTESIAN_POINT('',(61.4924284331501,1.85995900630951,48.35));
#84073=CARTESIAN_POINT('',(61.4924284331501,1.85995900630951,48.5));
#84074=CARTESIAN_POINT('Ctrl Pts',(61.4924284331501,1.85995900630951,48.35));
#84075=CARTESIAN_POINT('Ctrl Pts',(61.4128919951618,1.62210100889206,48.35));
#84076=CARTESIAN_POINT('Ctrl Pts',(61.2545701377094,1.49229192733765,48.35));
#84077=CARTESIAN_POINT('Ctrl Pts',(61.5719642750919,2.48499327898026,48.5));
#84078=CARTESIAN_POINT('Ctrl Pts',(61.5719642750919,2.48499327898026,48.35));
#84079=CARTESIAN_POINT('Ctrl Pts',(61.5719642750919,2.09781730175018,48.5));
#84080=CARTESIAN_POINT('Ctrl Pts',(61.5719642750919,2.09781730175018,48.35));
#84081=CARTESIAN_POINT('Ctrl Pts',(61.4924284331501,1.85995900630951,48.5));
#84082=CARTESIAN_POINT('Ctrl Pts',(61.4924284331501,1.85995900630951,48.35));
#84083=CARTESIAN_POINT('',(61.5719642750919,2.48499327898026,48.5));
#84084=CARTESIAN_POINT('Ctrl Pts',(61.5719642750919,2.48499327898026,48.5));
#84085=CARTESIAN_POINT('Ctrl Pts',(61.5719642750919,2.09781730175018,48.5));
#84086=CARTESIAN_POINT('Ctrl Pts',(61.4924284331501,1.85995900630951,48.5));
#84087=CARTESIAN_POINT('',(61.5719642750919,2.48499327898026,48.35));
#84088=CARTESIAN_POINT('',(61.5719642750919,2.48499327898026,48.5));
#84089=CARTESIAN_POINT('Ctrl Pts',(61.5719642750919,2.48499327898026,48.35));
#84090=CARTESIAN_POINT('Ctrl Pts',(61.5719642750919,2.09781730175018,48.35));
#84091=CARTESIAN_POINT('Ctrl Pts',(61.4924284331501,1.85995900630951,48.35));
#84092=CARTESIAN_POINT('Ctrl Pts',(61.5224417559803,3.00497958064079,48.5));
#84093=CARTESIAN_POINT('Ctrl Pts',(61.5224417559803,3.00497958064079,48.35));
#84094=CARTESIAN_POINT('Ctrl Pts',(61.5719642750919,2.81214186549187,48.5));
#84095=CARTESIAN_POINT('Ctrl Pts',(61.5719642750919,2.81214186549187,48.35));
#84096=CARTESIAN_POINT('Ctrl Pts',(61.5719642750919,2.48499327898026,48.5));
#84097=CARTESIAN_POINT('Ctrl Pts',(61.5719642750919,2.48499327898026,48.35));
#84098=CARTESIAN_POINT('',(61.5224417559803,3.00497958064079,48.5));
#84099=CARTESIAN_POINT('Ctrl Pts',(61.5224417559803,3.00497958064079,48.5));
#84100=CARTESIAN_POINT('Ctrl Pts',(61.5719642750919,2.81214186549187,48.5));
#84101=CARTESIAN_POINT('Ctrl Pts',(61.5719642750919,2.48499327898026,48.5));
#84102=CARTESIAN_POINT('',(61.5224417559803,3.00497958064079,48.35));
#84103=CARTESIAN_POINT('',(61.5224417559803,3.00497958064079,48.5));
#84104=CARTESIAN_POINT('Ctrl Pts',(61.5224417559803,3.00497958064079,48.35));
#84105=CARTESIAN_POINT('Ctrl Pts',(61.5719642750919,2.81214186549187,48.35));
#84106=CARTESIAN_POINT('Ctrl Pts',(61.5719642750919,2.48499327898026,48.35));
#84107=CARTESIAN_POINT('Ctrl Pts',(61.385879766196,3.33212831616402,48.5));
#84108=CARTESIAN_POINT('Ctrl Pts',(61.385879766196,3.33212831616402,48.35));
#84109=CARTESIAN_POINT('Ctrl Pts',(61.4729192368686,3.19781729578972,48.5));
#84110=CARTESIAN_POINT('Ctrl Pts',(61.4729192368686,3.19781729578972,48.35));
#84111=CARTESIAN_POINT('Ctrl Pts',(61.5224417559803,3.00497958064079,48.5));
#84112=CARTESIAN_POINT('Ctrl Pts',(61.5224417559803,3.00497958064079,48.35));
#84113=CARTESIAN_POINT('',(61.385879766196,3.33212831616402,48.5));
#84114=CARTESIAN_POINT('Ctrl Pts',(61.385879766196,3.33212831616402,48.5));
#84115=CARTESIAN_POINT('Ctrl Pts',(61.4729192368686,3.19781729578972,48.5));
#84116=CARTESIAN_POINT('Ctrl Pts',(61.5224417559803,3.00497958064079,48.5));
#84117=CARTESIAN_POINT('',(61.385879766196,3.33212831616402,48.35));
#84118=CARTESIAN_POINT('',(61.385879766196,3.33212831616402,48.5));
#84119=CARTESIAN_POINT('Ctrl Pts',(61.385879766196,3.33212831616402,48.35));
#84120=CARTESIAN_POINT('Ctrl Pts',(61.4729192368686,3.19781729578972,48.35));
#84121=CARTESIAN_POINT('Ctrl Pts',(61.5224417559803,3.00497958064079,48.35));
#84122=CARTESIAN_POINT('Ctrl Pts',(61.1652799956501,3.5377217233181,48.5));
#84123=CARTESIAN_POINT('Ctrl Pts',(61.1652799956501,3.5377217233181,48.35));
#84124=CARTESIAN_POINT('Ctrl Pts',(61.2988402955234,3.46643933653831,48.5));
#84125=CARTESIAN_POINT('Ctrl Pts',(61.2988402955234,3.46643933653831,48.35));
#84126=CARTESIAN_POINT('Ctrl Pts',(61.385879766196,3.33212831616402,48.5));
#84127=CARTESIAN_POINT('Ctrl Pts',(61.385879766196,3.33212831616402,48.35));
#84128=CARTESIAN_POINT('',(61.1652799956501,3.5377217233181,48.5));
#84129=CARTESIAN_POINT('Ctrl Pts',(61.1652799956501,3.5377217233181,48.5));
#84130=CARTESIAN_POINT('Ctrl Pts',(61.2988402955234,3.46643933653831,48.5));
#84131=CARTESIAN_POINT('Ctrl Pts',(61.385879766196,3.33212831616402,48.5));
#84132=CARTESIAN_POINT('',(61.1652799956501,3.5377217233181,48.35));
#84133=CARTESIAN_POINT('',(61.1652799956501,3.5377217233181,48.5));
#84134=CARTESIAN_POINT('Ctrl Pts',(61.1652799956501,3.5377217233181,48.35));
#84135=CARTESIAN_POINT('Ctrl Pts',(61.2988402955234,3.46643933653831,48.35));
#84136=CARTESIAN_POINT('Ctrl Pts',(61.385879766196,3.33212831616402,48.35));
#84137=CARTESIAN_POINT('Ctrl Pts',(60.8546384684741,3.60900411009789,48.5));
#84138=CARTESIAN_POINT('Ctrl Pts',(60.8546384684741,3.60900411009789,48.35));
#84139=CARTESIAN_POINT('Ctrl Pts',(61.0317190997303,3.60900411009789,48.5));
#84140=CARTESIAN_POINT('Ctrl Pts',(61.0317190997303,3.60900411009789,48.35));
#84141=CARTESIAN_POINT('Ctrl Pts',(61.1652799956501,3.5377217233181,48.5));
#84142=CARTESIAN_POINT('Ctrl Pts',(61.1652799956501,3.5377217233181,48.35));
#84143=CARTESIAN_POINT('',(60.8546384684741,3.60900411009789,48.5));
#84144=CARTESIAN_POINT('Ctrl Pts',(60.8546384684741,3.60900411009789,48.5));
#84145=CARTESIAN_POINT('Ctrl Pts',(61.0317190997303,3.60900411009789,48.5));
#84146=CARTESIAN_POINT('Ctrl Pts',(61.1652799956501,3.5377217233181,48.5));
#84147=CARTESIAN_POINT('',(60.8546384684741,3.60900411009789,48.35));
#84148=CARTESIAN_POINT('',(60.8546384684741,3.60900411009789,48.5));
#84149=CARTESIAN_POINT('Ctrl Pts',(60.8546384684741,3.60900411009789,48.35));
#84150=CARTESIAN_POINT('Ctrl Pts',(61.0317190997303,3.60900411009789,48.35));
#84151=CARTESIAN_POINT('Ctrl Pts',(61.1652799956501,3.5377217233181,48.35));
#84152=CARTESIAN_POINT('Ctrl Pts',(60.4562076441944,3.47994545102119,48.5));
#84153=CARTESIAN_POINT('Ctrl Pts',(60.4562076441944,3.47994545102119,48.35));
#84154=CARTESIAN_POINT('Ctrl Pts',(60.6145295016468,3.60900411009789,48.5));
#84155=CARTESIAN_POINT('Ctrl Pts',(60.6145295016468,3.60900411009789,48.35));
#84156=CARTESIAN_POINT('Ctrl Pts',(60.8546384684741,3.60900411009789,48.5));
#84157=CARTESIAN_POINT('Ctrl Pts',(60.8546384684741,3.60900411009789,48.35));
#84158=CARTESIAN_POINT('',(60.4562076441944,3.47994545102119,48.5));
#84159=CARTESIAN_POINT('Ctrl Pts',(60.4562076441944,3.47994545102119,48.5));
#84160=CARTESIAN_POINT('Ctrl Pts',(60.6145295016468,3.60900411009789,48.5));
#84161=CARTESIAN_POINT('Ctrl Pts',(60.8546384684741,3.60900411009789,48.5));
#84162=CARTESIAN_POINT('',(60.4562076441944,3.47994545102119,48.35));
#84163=CARTESIAN_POINT('',(60.4562076441944,3.47994545102119,48.5));
#84164=CARTESIAN_POINT('Ctrl Pts',(60.4562076441944,3.47994545102119,48.35));
#84165=CARTESIAN_POINT('Ctrl Pts',(60.6145295016468,3.60900411009789,48.35));
#84166=CARTESIAN_POINT('Ctrl Pts',(60.8546384684741,3.60900411009789,48.35));
#84167=CARTESIAN_POINT('Ctrl Pts',(60.217598926276,3.11302864551544,48.5));
#84168=CARTESIAN_POINT('Ctrl Pts',(60.217598926276,3.11302864551544,48.35));
#84169=CARTESIAN_POINT('Ctrl Pts',(60.2978854887187,3.3508867919445,48.5));
#84170=CARTESIAN_POINT('Ctrl Pts',(60.2978854887187,3.3508867919445,48.35));
#84171=CARTESIAN_POINT('Ctrl Pts',(60.4562076441944,3.47994545102119,48.5));
#84172=CARTESIAN_POINT('Ctrl Pts',(60.4562076441944,3.47994545102119,48.35));
#84173=CARTESIAN_POINT('',(60.217598926276,3.11302864551544,48.5));
#84174=CARTESIAN_POINT('Ctrl Pts',(60.217598926276,3.11302864551544,48.5));
#84175=CARTESIAN_POINT('Ctrl Pts',(60.2978854887187,3.3508867919445,48.5));
#84176=CARTESIAN_POINT('Ctrl Pts',(60.4562076441944,3.47994545102119,48.5));
#84177=CARTESIAN_POINT('',(60.217598926276,3.11302864551544,48.35));
#84178=CARTESIAN_POINT('',(60.217598926276,3.11302864551544,48.5));
#84179=CARTESIAN_POINT('Ctrl Pts',(60.217598926276,3.11302864551544,48.35));
#84180=CARTESIAN_POINT('Ctrl Pts',(60.2978854887187,3.3508867919445,48.35));
#84181=CARTESIAN_POINT('Ctrl Pts',(60.4562076441944,3.47994545102119,48.35));
#84182=CARTESIAN_POINT('Ctrl Pts',(60.1373126618564,2.48499327898026,48.5));
#84183=CARTESIAN_POINT('Ctrl Pts',(60.1373126618564,2.48499327898026,48.35));
#84184=CARTESIAN_POINT('Ctrl Pts',(60.1373126618564,2.87517049908638,48.5));
#84185=CARTESIAN_POINT('Ctrl Pts',(60.1373126618564,2.87517049908638,48.35));
#84186=CARTESIAN_POINT('Ctrl Pts',(60.217598926276,3.11302864551544,48.5));
#84187=CARTESIAN_POINT('Ctrl Pts',(60.217598926276,3.11302864551544,48.35));
#84188=CARTESIAN_POINT('',(60.1373126618564,2.48499327898026,48.5));
#84189=CARTESIAN_POINT('Ctrl Pts',(60.1373126618564,2.48499327898026,48.5));
#84190=CARTESIAN_POINT('Ctrl Pts',(60.1373126618564,2.87517049908638,48.5));
#84191=CARTESIAN_POINT('Ctrl Pts',(60.217598926276,3.11302864551544,48.5));
#84192=CARTESIAN_POINT('',(60.1373126618564,2.48499327898026,48.35));
#84193=CARTESIAN_POINT('',(60.1373126618564,2.48499327898026,48.5));
#84194=CARTESIAN_POINT('Ctrl Pts',(60.1373126618564,2.48499327898026,48.35));
#84195=CARTESIAN_POINT('Ctrl Pts',(60.1373126618564,2.87517049908638,48.35));
#84196=CARTESIAN_POINT('Ctrl Pts',(60.217598926276,3.11302864551544,48.35));
#84197=CARTESIAN_POINT('Ctrl Pts',(60.3549113385379,1.59058684110642,48.5));
#84198=CARTESIAN_POINT('Ctrl Pts',(60.3549113385379,1.59058684110642,48.35));
#84199=CARTESIAN_POINT('Ctrl Pts',(60.1373126618564,1.86521166563034,48.5));
#84200=CARTESIAN_POINT('Ctrl Pts',(60.1373126618564,1.86521166563034,48.35));
#84201=CARTESIAN_POINT('Ctrl Pts',(60.1373126618564,2.48499327898026,48.5));
#84202=CARTESIAN_POINT('Ctrl Pts',(60.1373126618564,2.48499327898026,48.35));
#84203=CARTESIAN_POINT('Ctrl Pts',(60.3549113385379,1.59058684110642,48.5));
#84204=CARTESIAN_POINT('Ctrl Pts',(60.1373126618564,1.86521166563034,48.5));
#84205=CARTESIAN_POINT('Ctrl Pts',(60.1373126618564,2.48499327898026,48.5));
#84206=CARTESIAN_POINT('Ctrl Pts',(60.3549113385379,1.59058684110642,48.35));
#84207=CARTESIAN_POINT('Ctrl Pts',(60.1373126618564,1.86521166563034,48.35));
#84208=CARTESIAN_POINT('Ctrl Pts',(60.1373126618564,2.48499327898026,48.35));
#84209=CARTESIAN_POINT('Origin',(59.9999999515712,2.48574362695217,48.35));
#84210=CARTESIAN_POINT('Ctrl Pts',(59.1348570100963,1.36248314380646,48.5));
#84211=CARTESIAN_POINT('Ctrl Pts',(59.1348570100963,1.36248314380646,48.35));
#84212=CARTESIAN_POINT('Ctrl Pts',(58.8347205035388,1.36248314380646,48.5));
#84213=CARTESIAN_POINT('Ctrl Pts',(58.8347205035388,1.36248314380646,48.35));
#84214=CARTESIAN_POINT('Ctrl Pts',(58.6448841802776,1.53055930137634,48.5));
#84215=CARTESIAN_POINT('Ctrl Pts',(58.6448841802776,1.53055930137634,48.35));
#84216=CARTESIAN_POINT('',(59.1348570100963,1.36248314380646,48.5));
#84217=CARTESIAN_POINT('',(58.6448841802776,1.53055930137634,48.5));
#84218=CARTESIAN_POINT('Ctrl Pts',(59.1348570100963,1.36248314380646,48.5));
#84219=CARTESIAN_POINT('Ctrl Pts',(58.8347205035388,1.36248314380646,48.5));
#84220=CARTESIAN_POINT('Ctrl Pts',(58.6448841802776,1.53055930137634,48.5));
#84221=CARTESIAN_POINT('',(59.1348570100963,1.36248314380646,48.35));
#84222=CARTESIAN_POINT('',(59.1348570100963,1.36248314380646,48.5));
#84223=CARTESIAN_POINT('',(58.6448841802776,1.53055930137634,48.35));
#84224=CARTESIAN_POINT('Ctrl Pts',(59.1348570100963,1.36248314380646,48.35));
#84225=CARTESIAN_POINT('Ctrl Pts',(58.8347205035388,1.36248314380646,48.35));
#84226=CARTESIAN_POINT('Ctrl Pts',(58.6448841802776,1.53055930137634,48.35));
#84227=CARTESIAN_POINT('',(58.6448841802776,1.53055930137634,48.5));
#84228=CARTESIAN_POINT('Ctrl Pts',(59.7126194350421,1.62960433959961,48.5));
#84229=CARTESIAN_POINT('Ctrl Pts',(59.7126194350421,1.62960433959961,48.35));
#84230=CARTESIAN_POINT('Ctrl Pts',(59.5010232441127,1.36248314380646,48.5));
#84231=CARTESIAN_POINT('Ctrl Pts',(59.5010232441127,1.36248314380646,48.35));
#84232=CARTESIAN_POINT('Ctrl Pts',(59.1348570100963,1.36248314380646,48.5));
#84233=CARTESIAN_POINT('Ctrl Pts',(59.1348570100963,1.36248314380646,48.35));
#84234=CARTESIAN_POINT('',(59.7126194350421,1.62960433959961,48.5));
#84235=CARTESIAN_POINT('Ctrl Pts',(59.7126194350421,1.62960433959961,48.5));
#84236=CARTESIAN_POINT('Ctrl Pts',(59.5010232441127,1.36248314380646,48.5));
#84237=CARTESIAN_POINT('Ctrl Pts',(59.1348570100963,1.36248314380646,48.5));
#84238=CARTESIAN_POINT('',(59.7126194350421,1.62960433959961,48.35));
#84239=CARTESIAN_POINT('',(59.7126194350421,1.62960433959961,48.5));
#84240=CARTESIAN_POINT('Ctrl Pts',(59.7126194350421,1.62960433959961,48.35));
#84241=CARTESIAN_POINT('Ctrl Pts',(59.5010232441127,1.36248314380646,48.35));
#84242=CARTESIAN_POINT('Ctrl Pts',(59.1348570100963,1.36248314380646,48.35));
#84243=CARTESIAN_POINT('Ctrl Pts',(59.8866986744106,2.14583912491798,48.5));
#84244=CARTESIAN_POINT('Ctrl Pts',(59.8866986744106,2.14583912491798,48.35));
#84245=CARTESIAN_POINT('Ctrl Pts',(59.8866986744106,1.84720331430435,48.5));
#84246=CARTESIAN_POINT('Ctrl Pts',(59.8866986744106,1.84720331430435,48.35));
#84247=CARTESIAN_POINT('Ctrl Pts',(59.7126194350421,1.62960433959961,48.5));
#84248=CARTESIAN_POINT('Ctrl Pts',(59.7126194350421,1.62960433959961,48.35));
#84249=CARTESIAN_POINT('',(59.8866986744106,2.14583912491798,48.5));
#84250=CARTESIAN_POINT('Ctrl Pts',(59.8866986744106,2.14583912491798,48.5));
#84251=CARTESIAN_POINT('Ctrl Pts',(59.8866986744106,1.84720331430435,48.5));
#84252=CARTESIAN_POINT('Ctrl Pts',(59.7126194350421,1.62960433959961,48.5));
#84253=CARTESIAN_POINT('',(59.8866986744106,2.14583912491798,48.35));
#84254=CARTESIAN_POINT('',(59.8866986744106,2.14583912491798,48.5));
#84255=CARTESIAN_POINT('Ctrl Pts',(59.8866986744106,2.14583912491798,48.35));
#84256=CARTESIAN_POINT('Ctrl Pts',(59.8866986744106,1.84720331430435,48.35));
#84257=CARTESIAN_POINT('Ctrl Pts',(59.7126194350421,1.62960433959961,48.35));
#84258=CARTESIAN_POINT('Ctrl Pts',(59.688608597964,2.65907236933708,48.5));
#84259=CARTESIAN_POINT('Ctrl Pts',(59.688608597964,2.65907236933708,48.35));
#84260=CARTESIAN_POINT('Ctrl Pts',(59.8866986744106,2.45948159694672,48.5));
#84261=CARTESIAN_POINT('Ctrl Pts',(59.8866986744106,2.45948159694672,48.35));
#84262=CARTESIAN_POINT('Ctrl Pts',(59.8866986744106,2.14583912491798,48.5));
#84263=CARTESIAN_POINT('Ctrl Pts',(59.8866986744106,2.14583912491798,48.35));
#84264=CARTESIAN_POINT('',(59.688608597964,2.65907236933708,48.5));
#84265=CARTESIAN_POINT('Ctrl Pts',(59.688608597964,2.65907236933708,48.5));
#84266=CARTESIAN_POINT('Ctrl Pts',(59.8866986744106,2.45948159694672,48.5));
#84267=CARTESIAN_POINT('Ctrl Pts',(59.8866986744106,2.14583912491798,48.5));
#84268=CARTESIAN_POINT('',(59.688608597964,2.65907236933708,48.35));
#84269=CARTESIAN_POINT('',(59.688608597964,2.65907236933708,48.5));
#84270=CARTESIAN_POINT('Ctrl Pts',(59.688608597964,2.65907236933708,48.35));
#84271=CARTESIAN_POINT('Ctrl Pts',(59.8866986744106,2.45948159694672,48.35));
#84272=CARTESIAN_POINT('Ctrl Pts',(59.8866986744106,2.14583912491798,48.35));
#84273=CARTESIAN_POINT('Ctrl Pts',(59.2023875825107,2.85866314172745,48.5));
#84274=CARTESIAN_POINT('Ctrl Pts',(59.2023875825107,2.85866314172745,48.35));
#84275=CARTESIAN_POINT('Ctrl Pts',(59.4905185215175,2.85866314172745,48.5));
#84276=CARTESIAN_POINT('Ctrl Pts',(59.4905185215175,2.85866314172745,48.35));
#84277=CARTESIAN_POINT('Ctrl Pts',(59.688608597964,2.65907236933708,48.5));
#84278=CARTESIAN_POINT('Ctrl Pts',(59.688608597964,2.65907236933708,48.35));
#84279=CARTESIAN_POINT('',(59.2023875825107,2.85866314172745,48.5));
#84280=CARTESIAN_POINT('Ctrl Pts',(59.2023875825107,2.85866314172745,48.5));
#84281=CARTESIAN_POINT('Ctrl Pts',(59.4905185215175,2.85866314172745,48.5));
#84282=CARTESIAN_POINT('Ctrl Pts',(59.688608597964,2.65907236933708,48.5));
#84283=CARTESIAN_POINT('',(59.2023875825107,2.85866314172745,48.35));
#84284=CARTESIAN_POINT('',(59.2023875825107,2.85866314172745,48.5));
#84285=CARTESIAN_POINT('Ctrl Pts',(59.2023875825107,2.85866314172745,48.35));
#84286=CARTESIAN_POINT('Ctrl Pts',(59.4905185215175,2.85866314172745,48.35));
#84287=CARTESIAN_POINT('Ctrl Pts',(59.688608597964,2.65907236933708,48.35));
#84288=CARTESIAN_POINT('Ctrl Pts',(58.786698680371,2.72060030698776,48.5));
#84289=CARTESIAN_POINT('Ctrl Pts',(58.786698680371,2.72060030698776,48.35));
#84290=CARTESIAN_POINT('Ctrl Pts',(58.984788607806,2.85866314172745,48.5));
#84291=CARTESIAN_POINT('Ctrl Pts',(58.984788607806,2.85866314172745,48.35));
#84292=CARTESIAN_POINT('Ctrl Pts',(59.2023875825107,2.85866314172745,48.5));
#84293=CARTESIAN_POINT('Ctrl Pts',(59.2023875825107,2.85866314172745,48.35));
#84294=CARTESIAN_POINT('',(58.786698680371,2.72060030698776,48.5));
#84295=CARTESIAN_POINT('Ctrl Pts',(58.786698680371,2.72060030698776,48.5));
#84296=CARTESIAN_POINT('Ctrl Pts',(58.984788607806,2.85866314172745,48.5));
#84297=CARTESIAN_POINT('Ctrl Pts',(59.2023875825107,2.85866314172745,48.5));
#84298=CARTESIAN_POINT('',(58.786698680371,2.72060030698776,48.35));
#84299=CARTESIAN_POINT('',(58.786698680371,2.72060030698776,48.5));
#84300=CARTESIAN_POINT('Ctrl Pts',(58.786698680371,2.72060030698776,48.35));
#84301=CARTESIAN_POINT('Ctrl Pts',(58.984788607806,2.85866314172745,48.35));
#84302=CARTESIAN_POINT('Ctrl Pts',(59.2023875825107,2.85866314172745,48.35));
#84303=CARTESIAN_POINT('Origin',(58.9052524678409,3.31186899542809,48.5));
#84304=CARTESIAN_POINT('',(58.9052524678409,3.31186899542809,48.5));
#84305=CARTESIAN_POINT('',(58.2187630699928,-0.111890755790727,48.5));
#84306=CARTESIAN_POINT('',(58.9052524678409,3.31186899542809,48.35));
#84307=CARTESIAN_POINT('',(58.9052524678409,3.31186899542809,48.5));
#84308=CARTESIAN_POINT('',(58.9052524678409,3.31186899542809,48.35));
#84309=CARTESIAN_POINT('Origin',(59.7831513993442,3.31186899542809,48.5));
#84310=CARTESIAN_POINT('',(59.7831513993442,3.31186899542809,48.5));
#84311=CARTESIAN_POINT('',(29.8915756996721,3.31186899542809,48.5));
#84312=CARTESIAN_POINT('',(59.7831513993442,3.31186899542809,48.35));
#84313=CARTESIAN_POINT('',(59.7831513993442,3.31186899542809,48.5));
#84314=CARTESIAN_POINT('',(59.7831513993442,3.31186899542809,48.35));
#84315=CARTESIAN_POINT('Origin',(59.7831513993442,3.56998646259308,48.5));
#84316=CARTESIAN_POINT('',(59.7831513993442,3.56998646259308,48.5));
#84317=CARTESIAN_POINT('',(59.7831513993442,5.78499323129654,48.5));
#84318=CARTESIAN_POINT('',(59.7831513993442,3.56998646259308,48.35));
#84319=CARTESIAN_POINT('',(59.7831513993442,3.56998646259308,48.5));
#84320=CARTESIAN_POINT('',(59.7831513993442,3.56998646259308,48.35));
#84321=CARTESIAN_POINT('Origin',(58.6891543380916,3.56998646259308,48.5));
#84322=CARTESIAN_POINT('',(58.6891543380916,3.56998646259308,48.5));
#84323=CARTESIAN_POINT('',(29.3445771690458,3.56998646259308,48.5));
#84324=CARTESIAN_POINT('',(58.6891543380916,3.56998646259308,48.35));
#84325=CARTESIAN_POINT('',(58.6891543380916,3.56998646259308,48.5));
#84326=CARTESIAN_POINT('',(58.6891543380916,3.56998646259308,48.35));
#84327=CARTESIAN_POINT('Origin',(58.4760574512184,2.43997284770012,48.5));
#84328=CARTESIAN_POINT('',(58.4760574512184,2.43997284770012,48.5));
#84329=CARTESIAN_POINT('',(57.9782484572375,-0.199816729090836,48.5));
#84330=CARTESIAN_POINT('',(58.4760574512184,2.43997284770012,48.35));
#84331=CARTESIAN_POINT('',(58.4760574512184,2.43997284770012,48.5));
#84332=CARTESIAN_POINT('',(58.4760574512184,2.43997284770012,48.35));
#84333=CARTESIAN_POINT('Origin',(58.7296726815403,2.40695783495903,48.5));
#84334=CARTESIAN_POINT('',(58.7296726815403,2.40695783495903,48.5));
#84335=CARTESIAN_POINT('',(29.4961884529084,6.21250158345456,48.5));
#84336=CARTESIAN_POINT('',(58.7296726815403,2.40695783495903,48.35));
#84337=CARTESIAN_POINT('',(58.7296726815403,2.40695783495903,48.5));
#84338=CARTESIAN_POINT('',(58.7296726815403,2.40695783495903,48.35));
#84339=CARTESIAN_POINT('Ctrl Pts',(58.8947477452457,2.56077775359154,48.5));
#84340=CARTESIAN_POINT('Ctrl Pts',(58.8947477452457,2.56077775359154,48.35));
#84341=CARTESIAN_POINT('Ctrl Pts',(58.7897000722587,2.5015007853508,48.5));
#84342=CARTESIAN_POINT('Ctrl Pts',(58.7897000722587,2.5015007853508,48.35));
#84343=CARTESIAN_POINT('Ctrl Pts',(58.7296726815403,2.40695783495903,48.5));
#84344=CARTESIAN_POINT('Ctrl Pts',(58.7296726815403,2.40695783495903,48.35));
#84345=CARTESIAN_POINT('',(58.8947477452457,2.56077775359154,48.5));
#84346=CARTESIAN_POINT('Ctrl Pts',(58.8947477452457,2.56077775359154,48.5));
#84347=CARTESIAN_POINT('Ctrl Pts',(58.7897000722587,2.5015007853508,48.5));
#84348=CARTESIAN_POINT('Ctrl Pts',(58.7296726815403,2.40695783495903,48.5));
#84349=CARTESIAN_POINT('',(58.8947477452457,2.56077775359154,48.35));
#84350=CARTESIAN_POINT('',(58.8947477452457,2.56077775359154,48.5));
#84351=CARTESIAN_POINT('Ctrl Pts',(58.8947477452457,2.56077775359154,48.35));
#84352=CARTESIAN_POINT('Ctrl Pts',(58.7897000722587,2.5015007853508,48.35));
#84353=CARTESIAN_POINT('Ctrl Pts',(58.7296726815403,2.40695783495903,48.35));
#84354=CARTESIAN_POINT('Ctrl Pts',(59.1303547732532,2.62005472183228,48.5));
#84355=CARTESIAN_POINT('Ctrl Pts',(59.1303547732532,2.62005472183228,48.35));
#84356=CARTESIAN_POINT('Ctrl Pts',(58.9997955672443,2.62005472183228,48.5));
#84357=CARTESIAN_POINT('Ctrl Pts',(58.9997955672443,2.62005472183228,48.35));
#84358=CARTESIAN_POINT('Ctrl Pts',(58.8947477452457,2.56077775359154,48.5));
#84359=CARTESIAN_POINT('Ctrl Pts',(58.8947477452457,2.56077775359154,48.35));
#84360=CARTESIAN_POINT('',(59.1303547732532,2.62005472183228,48.5));
#84361=CARTESIAN_POINT('Ctrl Pts',(59.1303547732532,2.62005472183228,48.5));
#84362=CARTESIAN_POINT('Ctrl Pts',(58.9997955672443,2.62005472183228,48.5));
#84363=CARTESIAN_POINT('Ctrl Pts',(58.8947477452457,2.56077775359154,48.5));
#84364=CARTESIAN_POINT('',(59.1303547732532,2.62005472183228,48.35));
#84365=CARTESIAN_POINT('',(59.1303547732532,2.62005472183228,48.5));
#84366=CARTESIAN_POINT('Ctrl Pts',(59.1303547732532,2.62005472183228,48.35));
#84367=CARTESIAN_POINT('Ctrl Pts',(58.9997955672443,2.62005472183228,48.35));
#84368=CARTESIAN_POINT('Ctrl Pts',(58.8947477452457,2.56077775359154,48.35));
#84369=CARTESIAN_POINT('Ctrl Pts',(59.4702592007816,2.48649397492409,48.5));
#84370=CARTESIAN_POINT('Ctrl Pts',(59.4702592007816,2.48649397492409,48.35));
#84371=CARTESIAN_POINT('Ctrl Pts',(59.3404504172504,2.62005472183228,48.5));
#84372=CARTESIAN_POINT('Ctrl Pts',(59.3404504172504,2.62005472183228,48.35));
#84373=CARTESIAN_POINT('Ctrl Pts',(59.1303547732532,2.62005472183228,48.5));
#84374=CARTESIAN_POINT('Ctrl Pts',(59.1303547732532,2.62005472183228,48.35));
#84375=CARTESIAN_POINT('',(59.4702592007816,2.48649397492409,48.5));
#84376=CARTESIAN_POINT('Ctrl Pts',(59.4702592007816,2.48649397492409,48.5));
#84377=CARTESIAN_POINT('Ctrl Pts',(59.3404504172504,2.62005472183228,48.5));
#84378=CARTESIAN_POINT('Ctrl Pts',(59.1303547732532,2.62005472183228,48.5));
#84379=CARTESIAN_POINT('',(59.4702592007816,2.48649397492409,48.35));
#84380=CARTESIAN_POINT('',(59.4702592007816,2.48649397492409,48.5));
#84381=CARTESIAN_POINT('Ctrl Pts',(59.4702592007816,2.48649397492409,48.35));
#84382=CARTESIAN_POINT('Ctrl Pts',(59.3404504172504,2.62005472183228,48.35));
#84383=CARTESIAN_POINT('Ctrl Pts',(59.1303547732532,2.62005472183228,48.35));
#84384=CARTESIAN_POINT('Ctrl Pts',(59.6000685803592,2.12182813882828,48.5));
#84385=CARTESIAN_POINT('Ctrl Pts',(59.6000685803592,2.12182813882828,48.35));
#84386=CARTESIAN_POINT('Ctrl Pts',(59.6000685803592,2.3529332280159,48.5));
#84387=CARTESIAN_POINT('Ctrl Pts',(59.6000685803592,2.3529332280159,48.35));
#84388=CARTESIAN_POINT('Ctrl Pts',(59.4702592007816,2.48649397492409,48.5));
#84389=CARTESIAN_POINT('Ctrl Pts',(59.4702592007816,2.48649397492409,48.35));
#84390=CARTESIAN_POINT('',(59.6000685803592,2.12182813882828,48.5));
#84391=CARTESIAN_POINT('Ctrl Pts',(59.6000685803592,2.12182813882828,48.5));
#84392=CARTESIAN_POINT('Ctrl Pts',(59.6000685803592,2.3529332280159,48.5));
#84393=CARTESIAN_POINT('Ctrl Pts',(59.4702592007816,2.48649397492409,48.5));
#84394=CARTESIAN_POINT('',(59.6000685803592,2.12182813882828,48.35));
#84395=CARTESIAN_POINT('',(59.6000685803592,2.12182813882828,48.5));
#84396=CARTESIAN_POINT('Ctrl Pts',(59.6000685803592,2.12182813882828,48.35));
#84397=CARTESIAN_POINT('Ctrl Pts',(59.6000685803592,2.3529332280159,48.35));
#84398=CARTESIAN_POINT('Ctrl Pts',(59.4702592007816,2.48649397492409,48.35));
#84399=CARTESIAN_POINT('Ctrl Pts',(59.465006839484,1.73165076971054,48.5));
#84400=CARTESIAN_POINT('Ctrl Pts',(59.465006839484,1.73165076971054,48.35));
#84401=CARTESIAN_POINT('Ctrl Pts',(59.6000685803592,1.87871778011322,48.5));
#84402=CARTESIAN_POINT('Ctrl Pts',(59.6000685803592,1.87871778011322,48.35));
#84403=CARTESIAN_POINT('Ctrl Pts',(59.6000685803592,2.12182813882828,48.5));
#84404=CARTESIAN_POINT('Ctrl Pts',(59.6000685803592,2.12182813882828,48.35));
#84405=CARTESIAN_POINT('',(59.465006839484,1.73165076971054,48.5));
#84406=CARTESIAN_POINT('Ctrl Pts',(59.465006839484,1.73165076971054,48.5));
#84407=CARTESIAN_POINT('Ctrl Pts',(59.6000685803592,1.87871778011322,48.5));
#84408=CARTESIAN_POINT('Ctrl Pts',(59.6000685803592,2.12182813882828,48.5));
#84409=CARTESIAN_POINT('',(59.465006839484,1.73165076971054,48.35));
#84410=CARTESIAN_POINT('',(59.465006839484,1.73165076971054,48.5));
#84411=CARTESIAN_POINT('Ctrl Pts',(59.465006839484,1.73165076971054,48.35));
#84412=CARTESIAN_POINT('Ctrl Pts',(59.6000685803592,1.87871778011322,48.35));
#84413=CARTESIAN_POINT('Ctrl Pts',(59.6000685803592,2.12182813882828,48.35));
#84414=CARTESIAN_POINT('Ctrl Pts',(59.1348570100963,1.58458405733109,48.5));
#84415=CARTESIAN_POINT('Ctrl Pts',(59.1348570100963,1.58458405733109,48.35));
#84416=CARTESIAN_POINT('Ctrl Pts',(59.3299455456436,1.58458405733109,48.5));
#84417=CARTESIAN_POINT('Ctrl Pts',(59.3299455456436,1.58458405733109,48.35));
#84418=CARTESIAN_POINT('Ctrl Pts',(59.465006839484,1.73165076971054,48.5));
#84419=CARTESIAN_POINT('Ctrl Pts',(59.465006839484,1.73165076971054,48.35));
#84420=CARTESIAN_POINT('',(59.1348570100963,1.58458405733109,48.5));
#84421=CARTESIAN_POINT('Ctrl Pts',(59.1348570100963,1.58458405733109,48.5));
#84422=CARTESIAN_POINT('Ctrl Pts',(59.3299455456436,1.58458405733109,48.5));
#84423=CARTESIAN_POINT('Ctrl Pts',(59.465006839484,1.73165076971054,48.5));
#84424=CARTESIAN_POINT('',(59.1348570100963,1.58458405733109,48.35));
#84425=CARTESIAN_POINT('',(59.1348570100963,1.58458405733109,48.5));
#84426=CARTESIAN_POINT('Ctrl Pts',(59.1348570100963,1.58458405733109,48.35));
#84427=CARTESIAN_POINT('Ctrl Pts',(59.3299455456436,1.58458405733109,48.35));
#84428=CARTESIAN_POINT('Ctrl Pts',(59.465006839484,1.73165076971054,48.35));
#84429=CARTESIAN_POINT('Ctrl Pts',(58.8579810671508,1.68888145685196,48.5));
#84430=CARTESIAN_POINT('Ctrl Pts',(58.8579810671508,1.68888145685196,48.35));
#84431=CARTESIAN_POINT('Ctrl Pts',(58.9727833382785,1.58458405733109,48.5));
#84432=CARTESIAN_POINT('Ctrl Pts',(58.9727833382785,1.58458405733109,48.35));
#84433=CARTESIAN_POINT('Ctrl Pts',(59.1348570100963,1.58458405733109,48.5));
#84434=CARTESIAN_POINT('Ctrl Pts',(59.1348570100963,1.58458405733109,48.35));
#84435=CARTESIAN_POINT('',(58.8579810671508,1.68888145685196,48.5));
#84436=CARTESIAN_POINT('Ctrl Pts',(58.8579810671508,1.68888145685196,48.5));
#84437=CARTESIAN_POINT('Ctrl Pts',(58.9727833382785,1.58458405733109,48.5));
#84438=CARTESIAN_POINT('Ctrl Pts',(59.1348570100963,1.58458405733109,48.5));
#84439=CARTESIAN_POINT('',(58.8579810671508,1.68888145685196,48.35));
#84440=CARTESIAN_POINT('',(58.8579810671508,1.68888145685196,48.5));
#84441=CARTESIAN_POINT('Ctrl Pts',(58.8579810671508,1.68888145685196,48.35));
#84442=CARTESIAN_POINT('Ctrl Pts',(58.9727833382785,1.58458405733109,48.35));
#84443=CARTESIAN_POINT('Ctrl Pts',(59.1348570100963,1.58458405733109,48.35));
#84444=CARTESIAN_POINT('Ctrl Pts',(58.7116646282375,2.00027281045914,48.5));
#84445=CARTESIAN_POINT('Ctrl Pts',(58.7116646282375,2.00027281045914,48.35));
#84446=CARTESIAN_POINT('Ctrl Pts',(58.7431787960231,1.79317885637283,48.5));
#84447=CARTESIAN_POINT('Ctrl Pts',(58.7431787960231,1.79317885637283,48.35));
#84448=CARTESIAN_POINT('Ctrl Pts',(58.8579810671508,1.68888145685196,48.5));
#84449=CARTESIAN_POINT('Ctrl Pts',(58.8579810671508,1.68888145685196,48.35));
#84450=CARTESIAN_POINT('',(58.7116646282375,2.00027281045914,48.5));
#84451=CARTESIAN_POINT('Ctrl Pts',(58.7116646282375,2.00027281045914,48.5));
#84452=CARTESIAN_POINT('Ctrl Pts',(58.7431787960231,1.79317885637283,48.5));
#84453=CARTESIAN_POINT('Ctrl Pts',(58.8579810671508,1.68888145685196,48.5));
#84454=CARTESIAN_POINT('',(58.7116646282375,2.00027281045914,48.35));
#84455=CARTESIAN_POINT('',(58.7116646282375,2.00027281045914,48.5));
#84456=CARTESIAN_POINT('Ctrl Pts',(58.7116646282375,2.00027281045914,48.35));
#84457=CARTESIAN_POINT('Ctrl Pts',(58.7431787960231,1.79317885637283,48.35));
#84458=CARTESIAN_POINT('Ctrl Pts',(58.8579810671508,1.68888145685196,48.35));
#84459=CARTESIAN_POINT('Origin',(58.4280356280506,1.97626197338104,48.5));
#84460=CARTESIAN_POINT('',(58.4280356280506,1.97626197338104,48.5));
#84461=CARTESIAN_POINT('',(29.6750511830058,-0.457844639708494,48.5));
#84462=CARTESIAN_POINT('',(58.4280356280506,1.97626197338104,48.35));
#84463=CARTESIAN_POINT('',(58.4280356280506,1.97626197338104,48.5));
#84464=CARTESIAN_POINT('',(58.4280356280506,1.97626197338104,48.35));
#84465=CARTESIAN_POINT('Ctrl Pts',(58.6448841802776,1.53055930137634,48.5));
#84466=CARTESIAN_POINT('Ctrl Pts',(58.6448841802776,1.53055930137634,48.35));
#84467=CARTESIAN_POINT('Ctrl Pts',(58.4550478570163,1.69863575696945,48.5));
#84468=CARTESIAN_POINT('Ctrl Pts',(58.4550478570163,1.69863575696945,48.35));
#84469=CARTESIAN_POINT('Ctrl Pts',(58.4280356280506,1.97626197338104,48.5));
#84470=CARTESIAN_POINT('Ctrl Pts',(58.4280356280506,1.97626197338104,48.35));
#84471=CARTESIAN_POINT('Ctrl Pts',(58.6448841802776,1.53055930137634,48.5));
#84472=CARTESIAN_POINT('Ctrl Pts',(58.4550478570163,1.69863575696945,48.5));
#84473=CARTESIAN_POINT('Ctrl Pts',(58.4280356280506,1.97626197338104,48.5));
#84474=CARTESIAN_POINT('Ctrl Pts',(58.6448841802776,1.53055930137634,48.35));
#84475=CARTESIAN_POINT('Ctrl Pts',(58.4550478570163,1.69863575696945,48.35));
#84476=CARTESIAN_POINT('Ctrl Pts',(58.4280356280506,1.97626197338104,48.35));
#84477=CARTESIAN_POINT('Origin',(59.9999999515712,2.48574362695217,48.35));
#84478=CARTESIAN_POINT('Origin',(0.,8.,48.5));
#84479=CARTESIAN_POINT('Ctrl Pts',(50.8576400466263,3.38540250062943,48.5));
#84480=CARTESIAN_POINT('Ctrl Pts',(50.8576400466263,3.38540250062943,48.35));
#84481=CARTESIAN_POINT('Ctrl Pts',(50.6715552397072,3.38540250062943,48.5));
#84482=CARTESIAN_POINT('Ctrl Pts',(50.6715552397072,3.38540250062943,48.35));
#84483=CARTESIAN_POINT('Ctrl Pts',(50.5605049319565,3.22783091664314,48.5));
#84484=CARTESIAN_POINT('Ctrl Pts',(50.5605049319565,3.22783091664314,48.35));
#84485=CARTESIAN_POINT('',(50.8576400466263,3.38540250062943,48.5));
#84486=CARTESIAN_POINT('',(50.5605049319565,3.22783091664314,48.5));
#84487=CARTESIAN_POINT('Ctrl Pts',(50.8576400466263,3.38540250062943,48.5));
#84488=CARTESIAN_POINT('Ctrl Pts',(50.6715552397072,3.38540250062943,48.5));
#84489=CARTESIAN_POINT('Ctrl Pts',(50.5605049319565,3.22783091664314,48.5));
#84490=CARTESIAN_POINT('',(50.8576400466263,3.38540250062943,48.35));
#84491=CARTESIAN_POINT('',(50.8576400466263,3.38540250062943,48.5));
#84492=CARTESIAN_POINT('',(50.5605049319565,3.22783091664314,48.35));
#84493=CARTESIAN_POINT('Ctrl Pts',(50.8576400466263,3.38540250062943,48.35));
#84494=CARTESIAN_POINT('Ctrl Pts',(50.6715552397072,3.38540250062943,48.35));
#84495=CARTESIAN_POINT('Ctrl Pts',(50.5605049319565,3.22783091664314,48.35));
#84496=CARTESIAN_POINT('',(50.5605049319565,3.22783091664314,48.5));
#84497=CARTESIAN_POINT('Ctrl Pts',(51.1735333390534,3.2068213224411,48.5));
#84498=CARTESIAN_POINT('Ctrl Pts',(51.1735333390534,3.2068213224411,48.35));
#84499=CARTESIAN_POINT('Ctrl Pts',(51.0467256493866,3.38540250062943,48.5));
#84500=CARTESIAN_POINT('Ctrl Pts',(51.0467256493866,3.38540250062943,48.35));
#84501=CARTESIAN_POINT('Ctrl Pts',(50.8576400466263,3.38540250062943,48.5));
#84502=CARTESIAN_POINT('Ctrl Pts',(50.8576400466263,3.38540250062943,48.35));
#84503=CARTESIAN_POINT('',(51.1735333390534,3.2068213224411,48.5));
#84504=CARTESIAN_POINT('Ctrl Pts',(51.1735333390534,3.2068213224411,48.5));
#84505=CARTESIAN_POINT('Ctrl Pts',(51.0467256493866,3.38540250062943,48.5));
#84506=CARTESIAN_POINT('Ctrl Pts',(50.8576400466263,3.38540250062943,48.5));
#84507=CARTESIAN_POINT('',(51.1735333390534,3.2068213224411,48.35));
#84508=CARTESIAN_POINT('',(51.1735333390534,3.2068213224411,48.5));
#84509=CARTESIAN_POINT('Ctrl Pts',(51.1735333390534,3.2068213224411,48.35));
#84510=CARTESIAN_POINT('Ctrl Pts',(51.0467256493866,3.38540250062943,48.35));
#84511=CARTESIAN_POINT('Ctrl Pts',(50.8576400466263,3.38540250062943,48.35));
#84512=CARTESIAN_POINT('Ctrl Pts',(51.3003410287201,2.48499327898026,48.5));
#84513=CARTESIAN_POINT('Ctrl Pts',(51.3003410287201,2.48499327898026,48.35));
#84514=CARTESIAN_POINT('Ctrl Pts',(51.3003410287201,3.02824014425278,48.5));
#84515=CARTESIAN_POINT('Ctrl Pts',(51.3003410287201,3.02824014425278,48.35));
#84516=CARTESIAN_POINT('Ctrl Pts',(51.1735333390534,3.2068213224411,48.5));
#84517=CARTESIAN_POINT('Ctrl Pts',(51.1735333390534,3.2068213224411,48.35));
#84518=CARTESIAN_POINT('',(51.3003410287201,2.48499327898026,48.5));
#84519=CARTESIAN_POINT('Ctrl Pts',(51.3003410287201,2.48499327898026,48.5));
#84520=CARTESIAN_POINT('Ctrl Pts',(51.3003410287201,3.02824014425278,48.5));
#84521=CARTESIAN_POINT('Ctrl Pts',(51.1735333390534,3.2068213224411,48.5));
#84522=CARTESIAN_POINT('',(51.3003410287201,2.48499327898026,48.35));
#84523=CARTESIAN_POINT('',(51.3003410287201,2.48499327898026,48.5));
#84524=CARTESIAN_POINT('Ctrl Pts',(51.3003410287201,2.48499327898026,48.35));
#84525=CARTESIAN_POINT('Ctrl Pts',(51.3003410287201,3.02824014425278,48.35));
#84526=CARTESIAN_POINT('Ctrl Pts',(51.1735333390534,3.2068213224411,48.35));
#84527=CARTESIAN_POINT('Ctrl Pts',(51.1735333390534,1.76466578245163,48.5));
#84528=CARTESIAN_POINT('Ctrl Pts',(51.1735333390534,1.76466578245163,48.35));
#84529=CARTESIAN_POINT('Ctrl Pts',(51.3003410287201,1.9447478055954,48.5));
#84530=CARTESIAN_POINT('Ctrl Pts',(51.3003410287201,1.9447478055954,48.35));
#84531=CARTESIAN_POINT('Ctrl Pts',(51.3003410287201,2.48499327898026,48.5));
#84532=CARTESIAN_POINT('Ctrl Pts',(51.3003410287201,2.48499327898026,48.35));
#84533=CARTESIAN_POINT('',(51.1735333390534,1.76466578245163,48.5));
#84534=CARTESIAN_POINT('Ctrl Pts',(51.1735333390534,1.76466578245163,48.5));
#84535=CARTESIAN_POINT('Ctrl Pts',(51.3003410287201,1.9447478055954,48.5));
#84536=CARTESIAN_POINT('Ctrl Pts',(51.3003410287201,2.48499327898026,48.5));
#84537=CARTESIAN_POINT('',(51.1735333390534,1.76466578245163,48.35));
#84538=CARTESIAN_POINT('',(51.1735333390534,1.76466578245163,48.5));
#84539=CARTESIAN_POINT('Ctrl Pts',(51.1735333390534,1.76466578245163,48.35));
#84540=CARTESIAN_POINT('Ctrl Pts',(51.3003410287201,1.9447478055954,48.35));
#84541=CARTESIAN_POINT('Ctrl Pts',(51.3003410287201,2.48499327898026,48.35));
#84542=CARTESIAN_POINT('Ctrl Pts',(50.8606411404908,1.58458405733109,48.5));
#84543=CARTESIAN_POINT('Ctrl Pts',(50.8606411404908,1.58458405733109,48.35));
#84544=CARTESIAN_POINT('Ctrl Pts',(51.0467256493866,1.58458405733109,48.5));
#84545=CARTESIAN_POINT('Ctrl Pts',(51.0467256493866,1.58458405733109,48.35));
#84546=CARTESIAN_POINT('Ctrl Pts',(51.1735333390534,1.76466578245163,48.5));
#84547=CARTESIAN_POINT('Ctrl Pts',(51.1735333390534,1.76466578245163,48.35));
#84548=CARTESIAN_POINT('',(50.8606411404908,1.58458405733109,48.5));
#84549=CARTESIAN_POINT('Ctrl Pts',(50.8606411404908,1.58458405733109,48.5));
#84550=CARTESIAN_POINT('Ctrl Pts',(51.0467256493866,1.58458405733109,48.5));
#84551=CARTESIAN_POINT('Ctrl Pts',(51.1735333390534,1.76466578245163,48.5));
#84552=CARTESIAN_POINT('',(50.8606411404908,1.58458405733109,48.35));
#84553=CARTESIAN_POINT('',(50.8606411404908,1.58458405733109,48.5));
#84554=CARTESIAN_POINT('Ctrl Pts',(50.8606411404908,1.58458405733109,48.35));
#84555=CARTESIAN_POINT('Ctrl Pts',(51.0467256493866,1.58458405733109,48.35));
#84556=CARTESIAN_POINT('Ctrl Pts',(51.1735333390534,1.76466578245163,48.35));
#84557=CARTESIAN_POINT('Ctrl Pts',(50.5477489419281,1.76391565799713,48.5));
#84558=CARTESIAN_POINT('Ctrl Pts',(50.5477489419281,1.76391565799713,48.35));
#84559=CARTESIAN_POINT('Ctrl Pts',(50.6745566315949,1.58458405733109,48.5));
#84560=CARTESIAN_POINT('Ctrl Pts',(50.6745566315949,1.58458405733109,48.35));
#84561=CARTESIAN_POINT('Ctrl Pts',(50.8606411404908,1.58458405733109,48.5));
#84562=CARTESIAN_POINT('Ctrl Pts',(50.8606411404908,1.58458405733109,48.35));
#84563=CARTESIAN_POINT('',(50.5477489419281,1.76391565799713,48.5));
#84564=CARTESIAN_POINT('Ctrl Pts',(50.5477489419281,1.76391565799713,48.5));
#84565=CARTESIAN_POINT('Ctrl Pts',(50.6745566315949,1.58458405733109,48.5));
#84566=CARTESIAN_POINT('Ctrl Pts',(50.8606411404908,1.58458405733109,48.5));
#84567=CARTESIAN_POINT('',(50.5477489419281,1.76391565799713,48.35));
#84568=CARTESIAN_POINT('',(50.5477489419281,1.76391565799713,48.5));
#84569=CARTESIAN_POINT('Ctrl Pts',(50.5477489419281,1.76391565799713,48.35));
#84570=CARTESIAN_POINT('Ctrl Pts',(50.6745566315949,1.58458405733109,48.35));
#84571=CARTESIAN_POINT('Ctrl Pts',(50.8606411404908,1.58458405733109,48.35));
#84572=CARTESIAN_POINT('Ctrl Pts',(50.4209412522614,2.48499327898026,48.5));
#84573=CARTESIAN_POINT('Ctrl Pts',(50.4209412522614,2.48499327898026,48.35));
#84574=CARTESIAN_POINT('Ctrl Pts',(50.4209412522614,1.94324696063995,48.5));
#84575=CARTESIAN_POINT('Ctrl Pts',(50.4209412522614,1.94324696063995,48.35));
#84576=CARTESIAN_POINT('Ctrl Pts',(50.5477489419281,1.76391565799713,48.5));
#84577=CARTESIAN_POINT('Ctrl Pts',(50.5477489419281,1.76391565799713,48.35));
#84578=CARTESIAN_POINT('',(50.4209412522614,2.48499327898026,48.5));
#84579=CARTESIAN_POINT('Ctrl Pts',(50.4209412522614,2.48499327898026,48.5));
#84580=CARTESIAN_POINT('Ctrl Pts',(50.4209412522614,1.94324696063995,48.5));
#84581=CARTESIAN_POINT('Ctrl Pts',(50.5477489419281,1.76391565799713,48.5));
#84582=CARTESIAN_POINT('',(50.4209412522614,2.48499327898026,48.35));
#84583=CARTESIAN_POINT('',(50.4209412522614,2.48499327898026,48.5));
#84584=CARTESIAN_POINT('Ctrl Pts',(50.4209412522614,2.48499327898026,48.35));
#84585=CARTESIAN_POINT('Ctrl Pts',(50.4209412522614,1.94324696063995,48.35));
#84586=CARTESIAN_POINT('Ctrl Pts',(50.5477489419281,1.76391565799713,48.35));
#84587=CARTESIAN_POINT('Ctrl Pts',(50.5605049319565,3.22783091664314,48.5));
#84588=CARTESIAN_POINT('Ctrl Pts',(50.5605049319565,3.22783091664314,48.35));
#84589=CARTESIAN_POINT('Ctrl Pts',(50.4209412522614,3.02673944830894,48.5));
#84590=CARTESIAN_POINT('Ctrl Pts',(50.4209412522614,3.02673944830894,48.35));
#84591=CARTESIAN_POINT('Ctrl Pts',(50.4209412522614,2.48499327898026,48.5));
#84592=CARTESIAN_POINT('Ctrl Pts',(50.4209412522614,2.48499327898026,48.35));
#84593=CARTESIAN_POINT('Ctrl Pts',(50.5605049319565,3.22783091664314,48.5));
#84594=CARTESIAN_POINT('Ctrl Pts',(50.4209412522614,3.02673944830894,48.5));
#84595=CARTESIAN_POINT('Ctrl Pts',(50.4209412522614,2.48499327898026,48.5));
#84596=CARTESIAN_POINT('Ctrl Pts',(50.5605049319565,3.22783091664314,48.35));
#84597=CARTESIAN_POINT('Ctrl Pts',(50.4209412522614,3.02673944830894,48.35));
#84598=CARTESIAN_POINT('Ctrl Pts',(50.4209412522614,2.48499327898026,48.35));
#84599=CARTESIAN_POINT('Ctrl Pts',(50.8606411404908,1.36248314380646,48.5));
#84600=CARTESIAN_POINT('Ctrl Pts',(50.8606411404908,1.36248314380646,48.35));
#84601=CARTESIAN_POINT('Ctrl Pts',(50.5424965806305,1.36248314380646,48.5));
#84602=CARTESIAN_POINT('Ctrl Pts',(50.5424965806305,1.36248314380646,48.35));
#84603=CARTESIAN_POINT('Ctrl Pts',(50.3609140105546,1.59058684110642,48.5));
#84604=CARTESIAN_POINT('Ctrl Pts',(50.3609140105546,1.59058684110642,48.35));
#84605=CARTESIAN_POINT('',(50.8606411404908,1.36248314380646,48.5));
#84606=CARTESIAN_POINT('',(50.3609140105546,1.59058684110642,48.5));
#84607=CARTESIAN_POINT('Ctrl Pts',(50.8606411404908,1.36248314380646,48.5));
#84608=CARTESIAN_POINT('Ctrl Pts',(50.5424965806305,1.36248314380646,48.5));
#84609=CARTESIAN_POINT('Ctrl Pts',(50.3609140105546,1.59058684110642,48.5));
#84610=CARTESIAN_POINT('',(50.8606411404908,1.36248314380646,48.35));
#84611=CARTESIAN_POINT('',(50.8606411404908,1.36248314380646,48.5));
#84612=CARTESIAN_POINT('',(50.3609140105546,1.59058684110642,48.35));
#84613=CARTESIAN_POINT('Ctrl Pts',(50.8606411404908,1.36248314380646,48.35));
#84614=CARTESIAN_POINT('Ctrl Pts',(50.5424965806305,1.36248314380646,48.35));
#84615=CARTESIAN_POINT('Ctrl Pts',(50.3609140105546,1.59058684110642,48.35));
#84616=CARTESIAN_POINT('',(50.3609140105546,1.59058684110642,48.5));
#84617=CARTESIAN_POINT('Ctrl Pts',(51.260572809726,1.49229192733765,48.5));
#84618=CARTESIAN_POINT('Ctrl Pts',(51.260572809726,1.49229192733765,48.35));
#84619=CARTESIAN_POINT('Ctrl Pts',(51.1022509522736,1.36248314380646,48.5));
#84620=CARTESIAN_POINT('Ctrl Pts',(51.1022509522736,1.36248314380646,48.35));
#84621=CARTESIAN_POINT('Ctrl Pts',(50.8606411404908,1.36248314380646,48.5));
#84622=CARTESIAN_POINT('Ctrl Pts',(50.8606411404908,1.36248314380646,48.35));
#84623=CARTESIAN_POINT('',(51.260572809726,1.49229192733765,48.5));
#84624=CARTESIAN_POINT('Ctrl Pts',(51.260572809726,1.49229192733765,48.5));
#84625=CARTESIAN_POINT('Ctrl Pts',(51.1022509522736,1.36248314380646,48.5));
#84626=CARTESIAN_POINT('Ctrl Pts',(50.8606411404908,1.36248314380646,48.5));
#84627=CARTESIAN_POINT('',(51.260572809726,1.49229192733765,48.35));
#84628=CARTESIAN_POINT('',(51.260572809726,1.49229192733765,48.5));
#84629=CARTESIAN_POINT('Ctrl Pts',(51.260572809726,1.49229192733765,48.35));
#84630=CARTESIAN_POINT('Ctrl Pts',(51.1022509522736,1.36248314380646,48.35));
#84631=CARTESIAN_POINT('Ctrl Pts',(50.8606411404908,1.36248314380646,48.35));
#84632=CARTESIAN_POINT('Ctrl Pts',(51.4984311051667,1.85995900630951,48.5));
#84633=CARTESIAN_POINT('Ctrl Pts',(51.4984311051667,1.85995900630951,48.35));
#84634=CARTESIAN_POINT('Ctrl Pts',(51.4188946671784,1.62210100889206,48.5));
#84635=CARTESIAN_POINT('Ctrl Pts',(51.4188946671784,1.62210100889206,48.35));
#84636=CARTESIAN_POINT('Ctrl Pts',(51.260572809726,1.49229192733765,48.5));
#84637=CARTESIAN_POINT('Ctrl Pts',(51.260572809726,1.49229192733765,48.35));
#84638=CARTESIAN_POINT('',(51.4984311051667,1.85995900630951,48.5));
#84639=CARTESIAN_POINT('Ctrl Pts',(51.4984311051667,1.85995900630951,48.5));
#84640=CARTESIAN_POINT('Ctrl Pts',(51.4188946671784,1.62210100889206,48.5));
#84641=CARTESIAN_POINT('Ctrl Pts',(51.260572809726,1.49229192733765,48.5));
#84642=CARTESIAN_POINT('',(51.4984311051667,1.85995900630951,48.35));
#84643=CARTESIAN_POINT('',(51.4984311051667,1.85995900630951,48.5));
#84644=CARTESIAN_POINT('Ctrl Pts',(51.4984311051667,1.85995900630951,48.35));
#84645=CARTESIAN_POINT('Ctrl Pts',(51.4188946671784,1.62210100889206,48.35));
#84646=CARTESIAN_POINT('Ctrl Pts',(51.260572809726,1.49229192733765,48.35));
#84647=CARTESIAN_POINT('Ctrl Pts',(51.5779669471085,2.48499327898026,48.5));
#84648=CARTESIAN_POINT('Ctrl Pts',(51.5779669471085,2.48499327898026,48.35));
#84649=CARTESIAN_POINT('Ctrl Pts',(51.5779669471085,2.09781730175018,48.5));
#84650=CARTESIAN_POINT('Ctrl Pts',(51.5779669471085,2.09781730175018,48.35));
#84651=CARTESIAN_POINT('Ctrl Pts',(51.4984311051667,1.85995900630951,48.5));
#84652=CARTESIAN_POINT('Ctrl Pts',(51.4984311051667,1.85995900630951,48.35));
#84653=CARTESIAN_POINT('',(51.5779669471085,2.48499327898026,48.5));
#84654=CARTESIAN_POINT('Ctrl Pts',(51.5779669471085,2.48499327898026,48.5));
#84655=CARTESIAN_POINT('Ctrl Pts',(51.5779669471085,2.09781730175018,48.5));
#84656=CARTESIAN_POINT('Ctrl Pts',(51.4984311051667,1.85995900630951,48.5));
#84657=CARTESIAN_POINT('',(51.5779669471085,2.48499327898026,48.35));
#84658=CARTESIAN_POINT('',(51.5779669471085,2.48499327898026,48.5));
#84659=CARTESIAN_POINT('Ctrl Pts',(51.5779669471085,2.48499327898026,48.35));
#84660=CARTESIAN_POINT('Ctrl Pts',(51.5779669471085,2.09781730175018,48.35));
#84661=CARTESIAN_POINT('Ctrl Pts',(51.4984311051667,1.85995900630951,48.35));
#84662=CARTESIAN_POINT('Ctrl Pts',(51.5284444279969,3.00497958064079,48.5));
#84663=CARTESIAN_POINT('Ctrl Pts',(51.5284444279969,3.00497958064079,48.35));
#84664=CARTESIAN_POINT('Ctrl Pts',(51.5779669471085,2.81214186549187,48.5));
#84665=CARTESIAN_POINT('Ctrl Pts',(51.5779669471085,2.81214186549187,48.35));
#84666=CARTESIAN_POINT('Ctrl Pts',(51.5779669471085,2.48499327898026,48.5));
#84667=CARTESIAN_POINT('Ctrl Pts',(51.5779669471085,2.48499327898026,48.35));
#84668=CARTESIAN_POINT('',(51.5284444279969,3.00497958064079,48.5));
#84669=CARTESIAN_POINT('Ctrl Pts',(51.5284444279969,3.00497958064079,48.5));
#84670=CARTESIAN_POINT('Ctrl Pts',(51.5779669471085,2.81214186549187,48.5));
#84671=CARTESIAN_POINT('Ctrl Pts',(51.5779669471085,2.48499327898026,48.5));
#84672=CARTESIAN_POINT('',(51.5284444279969,3.00497958064079,48.35));
#84673=CARTESIAN_POINT('',(51.5284444279969,3.00497958064079,48.5));
#84674=CARTESIAN_POINT('Ctrl Pts',(51.5284444279969,3.00497958064079,48.35));
#84675=CARTESIAN_POINT('Ctrl Pts',(51.5779669471085,2.81214186549187,48.35));
#84676=CARTESIAN_POINT('Ctrl Pts',(51.5779669471085,2.48499327898026,48.35));
#84677=CARTESIAN_POINT('Ctrl Pts',(51.3918824382126,3.33212831616402,48.5));
#84678=CARTESIAN_POINT('Ctrl Pts',(51.3918824382126,3.33212831616402,48.35));
#84679=CARTESIAN_POINT('Ctrl Pts',(51.4789219088852,3.19781729578972,48.5));
#84680=CARTESIAN_POINT('Ctrl Pts',(51.4789219088852,3.19781729578972,48.35));
#84681=CARTESIAN_POINT('Ctrl Pts',(51.5284444279969,3.00497958064079,48.5));
#84682=CARTESIAN_POINT('Ctrl Pts',(51.5284444279969,3.00497958064079,48.35));
#84683=CARTESIAN_POINT('',(51.3918824382126,3.33212831616402,48.5));
#84684=CARTESIAN_POINT('Ctrl Pts',(51.3918824382126,3.33212831616402,48.5));
#84685=CARTESIAN_POINT('Ctrl Pts',(51.4789219088852,3.19781729578972,48.5));
#84686=CARTESIAN_POINT('Ctrl Pts',(51.5284444279969,3.00497958064079,48.5));
#84687=CARTESIAN_POINT('',(51.3918824382126,3.33212831616402,48.35));
#84688=CARTESIAN_POINT('',(51.3918824382126,3.33212831616402,48.5));
#84689=CARTESIAN_POINT('Ctrl Pts',(51.3918824382126,3.33212831616402,48.35));
#84690=CARTESIAN_POINT('Ctrl Pts',(51.4789219088852,3.19781729578972,48.35));
#84691=CARTESIAN_POINT('Ctrl Pts',(51.5284444279969,3.00497958064079,48.35));
#84692=CARTESIAN_POINT('Ctrl Pts',(51.1712826676667,3.5377217233181,48.5));
#84693=CARTESIAN_POINT('Ctrl Pts',(51.1712826676667,3.5377217233181,48.35));
#84694=CARTESIAN_POINT('Ctrl Pts',(51.30484296754,3.46643933653831,48.5));
#84695=CARTESIAN_POINT('Ctrl Pts',(51.30484296754,3.46643933653831,48.35));
#84696=CARTESIAN_POINT('Ctrl Pts',(51.3918824382126,3.33212831616402,48.5));
#84697=CARTESIAN_POINT('Ctrl Pts',(51.3918824382126,3.33212831616402,48.35));
#84698=CARTESIAN_POINT('',(51.1712826676667,3.5377217233181,48.5));
#84699=CARTESIAN_POINT('Ctrl Pts',(51.1712826676667,3.5377217233181,48.5));
#84700=CARTESIAN_POINT('Ctrl Pts',(51.30484296754,3.46643933653831,48.5));
#84701=CARTESIAN_POINT('Ctrl Pts',(51.3918824382126,3.33212831616402,48.5));
#84702=CARTESIAN_POINT('',(51.1712826676667,3.5377217233181,48.35));
#84703=CARTESIAN_POINT('',(51.1712826676667,3.5377217233181,48.5));
#84704=CARTESIAN_POINT('Ctrl Pts',(51.1712826676667,3.5377217233181,48.35));
#84705=CARTESIAN_POINT('Ctrl Pts',(51.30484296754,3.46643933653831,48.35));
#84706=CARTESIAN_POINT('Ctrl Pts',(51.3918824382126,3.33212831616402,48.35));
#84707=CARTESIAN_POINT('Ctrl Pts',(50.8606411404908,3.60900411009789,48.5));
#84708=CARTESIAN_POINT('Ctrl Pts',(50.8606411404908,3.60900411009789,48.35));
#84709=CARTESIAN_POINT('Ctrl Pts',(51.0377217717469,3.60900411009789,48.5));
#84710=CARTESIAN_POINT('Ctrl Pts',(51.0377217717469,3.60900411009789,48.35));
#84711=CARTESIAN_POINT('Ctrl Pts',(51.1712826676667,3.5377217233181,48.5));
#84712=CARTESIAN_POINT('Ctrl Pts',(51.1712826676667,3.5377217233181,48.35));
#84713=CARTESIAN_POINT('',(50.8606411404908,3.60900411009789,48.5));
#84714=CARTESIAN_POINT('Ctrl Pts',(50.8606411404908,3.60900411009789,48.5));
#84715=CARTESIAN_POINT('Ctrl Pts',(51.0377217717469,3.60900411009789,48.5));
#84716=CARTESIAN_POINT('Ctrl Pts',(51.1712826676667,3.5377217233181,48.5));
#84717=CARTESIAN_POINT('',(50.8606411404908,3.60900411009789,48.35));
#84718=CARTESIAN_POINT('',(50.8606411404908,3.60900411009789,48.5));
#84719=CARTESIAN_POINT('Ctrl Pts',(50.8606411404908,3.60900411009789,48.35));
#84720=CARTESIAN_POINT('Ctrl Pts',(51.0377217717469,3.60900411009789,48.35));
#84721=CARTESIAN_POINT('Ctrl Pts',(51.1712826676667,3.5377217233181,48.35));
#84722=CARTESIAN_POINT('Ctrl Pts',(50.462210316211,3.47994545102119,48.5));
#84723=CARTESIAN_POINT('Ctrl Pts',(50.462210316211,3.47994545102119,48.35));
#84724=CARTESIAN_POINT('Ctrl Pts',(50.6205321736634,3.60900411009789,48.5));
#84725=CARTESIAN_POINT('Ctrl Pts',(50.6205321736634,3.60900411009789,48.35));
#84726=CARTESIAN_POINT('Ctrl Pts',(50.8606411404908,3.60900411009789,48.5));
#84727=CARTESIAN_POINT('Ctrl Pts',(50.8606411404908,3.60900411009789,48.35));
#84728=CARTESIAN_POINT('',(50.462210316211,3.47994545102119,48.5));
#84729=CARTESIAN_POINT('Ctrl Pts',(50.462210316211,3.47994545102119,48.5));
#84730=CARTESIAN_POINT('Ctrl Pts',(50.6205321736634,3.60900411009789,48.5));
#84731=CARTESIAN_POINT('Ctrl Pts',(50.8606411404908,3.60900411009789,48.5));
#84732=CARTESIAN_POINT('',(50.462210316211,3.47994545102119,48.35));
#84733=CARTESIAN_POINT('',(50.462210316211,3.47994545102119,48.5));
#84734=CARTESIAN_POINT('Ctrl Pts',(50.462210316211,3.47994545102119,48.35));
#84735=CARTESIAN_POINT('Ctrl Pts',(50.6205321736634,3.60900411009789,48.35));
#84736=CARTESIAN_POINT('Ctrl Pts',(50.8606411404908,3.60900411009789,48.35));
#84737=CARTESIAN_POINT('Ctrl Pts',(50.2236015982926,3.11302864551544,48.5));
#84738=CARTESIAN_POINT('Ctrl Pts',(50.2236015982926,3.11302864551544,48.35));
#84739=CARTESIAN_POINT('Ctrl Pts',(50.3038881607354,3.3508867919445,48.5));
#84740=CARTESIAN_POINT('Ctrl Pts',(50.3038881607354,3.3508867919445,48.35));
#84741=CARTESIAN_POINT('Ctrl Pts',(50.462210316211,3.47994545102119,48.5));
#84742=CARTESIAN_POINT('Ctrl Pts',(50.462210316211,3.47994545102119,48.35));
#84743=CARTESIAN_POINT('',(50.2236015982926,3.11302864551544,48.5));
#84744=CARTESIAN_POINT('Ctrl Pts',(50.2236015982926,3.11302864551544,48.5));
#84745=CARTESIAN_POINT('Ctrl Pts',(50.3038881607354,3.3508867919445,48.5));
#84746=CARTESIAN_POINT('Ctrl Pts',(50.462210316211,3.47994545102119,48.5));
#84747=CARTESIAN_POINT('',(50.2236015982926,3.11302864551544,48.35));
#84748=CARTESIAN_POINT('',(50.2236015982926,3.11302864551544,48.5));
#84749=CARTESIAN_POINT('Ctrl Pts',(50.2236015982926,3.11302864551544,48.35));
#84750=CARTESIAN_POINT('Ctrl Pts',(50.3038881607354,3.3508867919445,48.35));
#84751=CARTESIAN_POINT('Ctrl Pts',(50.462210316211,3.47994545102119,48.35));
#84752=CARTESIAN_POINT('Ctrl Pts',(50.143315333873,2.48499327898026,48.5));
#84753=CARTESIAN_POINT('Ctrl Pts',(50.143315333873,2.48499327898026,48.35));
#84754=CARTESIAN_POINT('Ctrl Pts',(50.143315333873,2.87517049908638,48.5));
#84755=CARTESIAN_POINT('Ctrl Pts',(50.143315333873,2.87517049908638,48.35));
#84756=CARTESIAN_POINT('Ctrl Pts',(50.2236015982926,3.11302864551544,48.5));
#84757=CARTESIAN_POINT('Ctrl Pts',(50.2236015982926,3.11302864551544,48.35));
#84758=CARTESIAN_POINT('',(50.143315333873,2.48499327898026,48.5));
#84759=CARTESIAN_POINT('Ctrl Pts',(50.143315333873,2.48499327898026,48.5));
#84760=CARTESIAN_POINT('Ctrl Pts',(50.143315333873,2.87517049908638,48.5));
#84761=CARTESIAN_POINT('Ctrl Pts',(50.2236015982926,3.11302864551544,48.5));
#84762=CARTESIAN_POINT('',(50.143315333873,2.48499327898026,48.35));
#84763=CARTESIAN_POINT('',(50.143315333873,2.48499327898026,48.5));
#84764=CARTESIAN_POINT('Ctrl Pts',(50.143315333873,2.48499327898026,48.35));
#84765=CARTESIAN_POINT('Ctrl Pts',(50.143315333873,2.87517049908638,48.35));
#84766=CARTESIAN_POINT('Ctrl Pts',(50.2236015982926,3.11302864551544,48.35));
#84767=CARTESIAN_POINT('Ctrl Pts',(50.3609140105546,1.59058684110642,48.5));
#84768=CARTESIAN_POINT('Ctrl Pts',(50.3609140105546,1.59058684110642,48.35));
#84769=CARTESIAN_POINT('Ctrl Pts',(50.143315333873,1.86521166563034,48.5));
#84770=CARTESIAN_POINT('Ctrl Pts',(50.143315333873,1.86521166563034,48.35));
#84771=CARTESIAN_POINT('Ctrl Pts',(50.143315333873,2.48499327898026,48.5));
#84772=CARTESIAN_POINT('Ctrl Pts',(50.143315333873,2.48499327898026,48.35));
#84773=CARTESIAN_POINT('Ctrl Pts',(50.3609140105546,1.59058684110642,48.5));
#84774=CARTESIAN_POINT('Ctrl Pts',(50.143315333873,1.86521166563034,48.5));
#84775=CARTESIAN_POINT('Ctrl Pts',(50.143315333873,2.48499327898026,48.5));
#84776=CARTESIAN_POINT('Ctrl Pts',(50.3609140105546,1.59058684110642,48.35));
#84777=CARTESIAN_POINT('Ctrl Pts',(50.143315333873,1.86521166563034,48.35));
#84778=CARTESIAN_POINT('Ctrl Pts',(50.143315333873,2.48499327898026,48.35));
#84779=CARTESIAN_POINT('Origin',(49.9999999143183,2.48574362695217,48.35));
#84780=CARTESIAN_POINT('Ctrl Pts',(49.1708733029664,2.58854025602341,48.5));
#84781=CARTESIAN_POINT('Ctrl Pts',(49.1708733029664,2.58854025602341,48.35));
#84782=CARTESIAN_POINT('Ctrl Pts',(48.9877900369465,2.58854025602341,48.5));
#84783=CARTESIAN_POINT('Ctrl Pts',(48.9877900369465,2.58854025602341,48.35));
#84784=CARTESIAN_POINT('Ctrl Pts',(48.8602320738137,2.45723062753677,48.5));
#84785=CARTESIAN_POINT('Ctrl Pts',(48.8602320738137,2.45723062753677,48.35));
#84786=CARTESIAN_POINT('',(49.1708733029664,2.58854025602341,48.5));
#84787=CARTESIAN_POINT('',(48.8602320738137,2.45723062753677,48.5));
#84788=CARTESIAN_POINT('Ctrl Pts',(49.1708733029664,2.58854025602341,48.5));
#84789=CARTESIAN_POINT('Ctrl Pts',(48.9877900369465,2.58854025602341,48.5));
#84790=CARTESIAN_POINT('Ctrl Pts',(48.8602320738137,2.45723062753677,48.5));
#84791=CARTESIAN_POINT('',(49.1708733029664,2.58854025602341,48.35));
#84792=CARTESIAN_POINT('',(49.1708733029664,2.58854025602341,48.5));
#84793=CARTESIAN_POINT('',(48.8602320738137,2.45723062753677,48.35));
#84794=CARTESIAN_POINT('Ctrl Pts',(49.1708733029664,2.58854025602341,48.35));
#84795=CARTESIAN_POINT('Ctrl Pts',(48.9877900369465,2.58854025602341,48.35));
#84796=CARTESIAN_POINT('Ctrl Pts',(48.8602320738137,2.45723062753677,48.35));
#84797=CARTESIAN_POINT('',(48.8602320738137,2.45723062753677,48.5));
#84798=CARTESIAN_POINT('Ctrl Pts',(49.4770122952759,2.45723062753677,48.5));
#84799=CARTESIAN_POINT('Ctrl Pts',(49.4770122952759,2.45723062753677,48.35));
#84800=CARTESIAN_POINT('Ctrl Pts',(49.35545726493,2.58854025602341,48.5));
#84801=CARTESIAN_POINT('Ctrl Pts',(49.35545726493,2.58854025602341,48.35));
#84802=CARTESIAN_POINT('Ctrl Pts',(49.1708733029664,2.58854025602341,48.5));
#84803=CARTESIAN_POINT('Ctrl Pts',(49.1708733029664,2.58854025602341,48.35));
#84804=CARTESIAN_POINT('',(49.4770122952759,2.45723062753677,48.5));
#84805=CARTESIAN_POINT('Ctrl Pts',(49.4770122952759,2.45723062753677,48.5));
#84806=CARTESIAN_POINT('Ctrl Pts',(49.35545726493,2.58854025602341,48.5));
#84807=CARTESIAN_POINT('Ctrl Pts',(49.1708733029664,2.58854025602341,48.5));
#84808=CARTESIAN_POINT('',(49.4770122952759,2.45723062753677,48.35));
#84809=CARTESIAN_POINT('',(49.4770122952759,2.45723062753677,48.5));
#84810=CARTESIAN_POINT('Ctrl Pts',(49.4770122952759,2.45723062753677,48.35));
#84811=CARTESIAN_POINT('Ctrl Pts',(49.35545726493,2.58854025602341,48.35));
#84812=CARTESIAN_POINT('Ctrl Pts',(49.1708733029664,2.58854025602341,48.35));
#84813=CARTESIAN_POINT('Ctrl Pts',(49.5985676236451,2.09781730175018,48.5));
#84814=CARTESIAN_POINT('Ctrl Pts',(49.5985676236451,2.09781730175018,48.35));
#84815=CARTESIAN_POINT('Ctrl Pts',(49.5985676236451,2.32592099905014,48.5));
#84816=CARTESIAN_POINT('Ctrl Pts',(49.5985676236451,2.32592099905014,48.35));
#84817=CARTESIAN_POINT('Ctrl Pts',(49.4770122952759,2.45723062753677,48.5));
#84818=CARTESIAN_POINT('Ctrl Pts',(49.4770122952759,2.45723062753677,48.35));
#84819=CARTESIAN_POINT('',(49.5985676236451,2.09781730175018,48.5));
#84820=CARTESIAN_POINT('Ctrl Pts',(49.5985676236451,2.09781730175018,48.5));
#84821=CARTESIAN_POINT('Ctrl Pts',(49.5985676236451,2.32592099905014,48.5));
#84822=CARTESIAN_POINT('Ctrl Pts',(49.4770122952759,2.45723062753677,48.5));
#84823=CARTESIAN_POINT('',(49.5985676236451,2.09781730175018,48.35));
#84824=CARTESIAN_POINT('',(49.5985676236451,2.09781730175018,48.5));
#84825=CARTESIAN_POINT('Ctrl Pts',(49.5985676236451,2.09781730175018,48.35));
#84826=CARTESIAN_POINT('Ctrl Pts',(49.5985676236451,2.32592099905014,48.35));
#84827=CARTESIAN_POINT('Ctrl Pts',(49.4770122952759,2.45723062753677,48.35));
#84828=CARTESIAN_POINT('Ctrl Pts',(49.4755117483437,1.72264659404755,48.5));
#84829=CARTESIAN_POINT('Ctrl Pts',(49.4755117483437,1.72264659404755,48.35));
#84830=CARTESIAN_POINT('Ctrl Pts',(49.5985676236451,1.86070942878723,48.5));
#84831=CARTESIAN_POINT('Ctrl Pts',(49.5985676236451,1.86070942878723,48.35));
#84832=CARTESIAN_POINT('Ctrl Pts',(49.5985676236451,2.09781730175018,48.5));
#84833=CARTESIAN_POINT('Ctrl Pts',(49.5985676236451,2.09781730175018,48.35));
#84834=CARTESIAN_POINT('',(49.4755117483437,1.72264659404755,48.5));
#84835=CARTESIAN_POINT('Ctrl Pts',(49.4755117483437,1.72264659404755,48.5));
#84836=CARTESIAN_POINT('Ctrl Pts',(49.5985676236451,1.86070942878723,48.5));
#84837=CARTESIAN_POINT('Ctrl Pts',(49.5985676236451,2.09781730175018,48.5));
#84838=CARTESIAN_POINT('',(49.4755117483437,1.72264659404755,48.35));
#84839=CARTESIAN_POINT('',(49.4755117483437,1.72264659404755,48.5));
#84840=CARTESIAN_POINT('Ctrl Pts',(49.4755117483437,1.72264659404755,48.35));
#84841=CARTESIAN_POINT('Ctrl Pts',(49.5985676236451,1.86070942878723,48.35));
#84842=CARTESIAN_POINT('Ctrl Pts',(49.5985676236451,2.09781730175018,48.35));
#84843=CARTESIAN_POINT('Ctrl Pts',(49.1813780255616,1.58458405733109,48.5));
#84844=CARTESIAN_POINT('Ctrl Pts',(49.1813780255616,1.58458405733109,48.35));
#84845=CARTESIAN_POINT('Ctrl Pts',(49.3524558730423,1.58458405733109,48.5));
#84846=CARTESIAN_POINT('Ctrl Pts',(49.3524558730423,1.58458405733109,48.35));
#84847=CARTESIAN_POINT('Ctrl Pts',(49.4755117483437,1.72264659404755,48.5));
#84848=CARTESIAN_POINT('Ctrl Pts',(49.4755117483437,1.72264659404755,48.35));
#84849=CARTESIAN_POINT('',(49.1813780255616,1.58458405733109,48.5));
#84850=CARTESIAN_POINT('Ctrl Pts',(49.1813780255616,1.58458405733109,48.5));
#84851=CARTESIAN_POINT('Ctrl Pts',(49.3524558730423,1.58458405733109,48.5));
#84852=CARTESIAN_POINT('Ctrl Pts',(49.4755117483437,1.72264659404755,48.5));
#84853=CARTESIAN_POINT('',(49.1813780255616,1.58458405733109,48.35));
#84854=CARTESIAN_POINT('',(49.1813780255616,1.58458405733109,48.5));
#84855=CARTESIAN_POINT('Ctrl Pts',(49.1813780255616,1.58458405733109,48.35));
#84856=CARTESIAN_POINT('Ctrl Pts',(49.3524558730423,1.58458405733109,48.35));
#84857=CARTESIAN_POINT('Ctrl Pts',(49.4755117483437,1.72264659404755,48.35));
#84858=CARTESIAN_POINT('Ctrl Pts',(48.9577764160931,1.65136420726776,48.5));
#84859=CARTESIAN_POINT('Ctrl Pts',(48.9577764160931,1.65136420726776,48.35));
#84860=CARTESIAN_POINT('Ctrl Pts',(49.0643249340355,1.58458405733109,48.5));
#84861=CARTESIAN_POINT('Ctrl Pts',(49.0643249340355,1.58458405733109,48.35));
#84862=CARTESIAN_POINT('Ctrl Pts',(49.1813780255616,1.58458405733109,48.5));
#84863=CARTESIAN_POINT('Ctrl Pts',(49.1813780255616,1.58458405733109,48.35));
#84864=CARTESIAN_POINT('',(48.9577764160931,1.65136420726776,48.5));
#84865=CARTESIAN_POINT('Ctrl Pts',(48.9577764160931,1.65136420726776,48.5));
#84866=CARTESIAN_POINT('Ctrl Pts',(49.0643249340355,1.58458405733109,48.5));
#84867=CARTESIAN_POINT('Ctrl Pts',(49.1813780255616,1.58458405733109,48.5));
#84868=CARTESIAN_POINT('',(48.9577764160931,1.65136420726776,48.35));
#84869=CARTESIAN_POINT('',(48.9577764160931,1.65136420726776,48.5));
#84870=CARTESIAN_POINT('Ctrl Pts',(48.9577764160931,1.65136420726776,48.35));
#84871=CARTESIAN_POINT('Ctrl Pts',(49.0643249340355,1.58458405733109,48.35));
#84872=CARTESIAN_POINT('Ctrl Pts',(49.1813780255616,1.58458405733109,48.35));
#84873=CARTESIAN_POINT('Ctrl Pts',(48.7919510789216,1.84570276737213,48.5));
#84874=CARTESIAN_POINT('Ctrl Pts',(48.7919510789216,1.84570276737213,48.35));
#84875=CARTESIAN_POINT('Ctrl Pts',(48.8512278981507,1.71814465522766,48.5));
#84876=CARTESIAN_POINT('Ctrl Pts',(48.8512278981507,1.71814465522766,48.35));
#84877=CARTESIAN_POINT('Ctrl Pts',(48.9577764160931,1.65136420726776,48.5));
#84878=CARTESIAN_POINT('Ctrl Pts',(48.9577764160931,1.65136420726776,48.35));
#84879=CARTESIAN_POINT('',(48.7919510789216,1.84570276737213,48.5));
#84880=CARTESIAN_POINT('Ctrl Pts',(48.7919510789216,1.84570276737213,48.5));
#84881=CARTESIAN_POINT('Ctrl Pts',(48.8512278981507,1.71814465522766,48.5));
#84882=CARTESIAN_POINT('Ctrl Pts',(48.9577764160931,1.65136420726776,48.5));
#84883=CARTESIAN_POINT('',(48.7919510789216,1.84570276737213,48.35));
#84884=CARTESIAN_POINT('',(48.7919510789216,1.84570276737213,48.5));
#84885=CARTESIAN_POINT('Ctrl Pts',(48.7919510789216,1.84570276737213,48.35));
#84886=CARTESIAN_POINT('Ctrl Pts',(48.8512278981507,1.71814465522766,48.35));
#84887=CARTESIAN_POINT('Ctrl Pts',(48.9577764160931,1.65136420726776,48.35));
#84888=CARTESIAN_POINT('Ctrl Pts',(48.7326739616692,2.1128241121769,48.5));
#84889=CARTESIAN_POINT('Ctrl Pts',(48.7326739616692,2.1128241121769,48.35));
#84890=CARTESIAN_POINT('Ctrl Pts',(48.7326739616692,1.97326058149338,48.5));
#84891=CARTESIAN_POINT('Ctrl Pts',(48.7326739616692,1.97326058149338,48.35));
#84892=CARTESIAN_POINT('Ctrl Pts',(48.7919510789216,1.84570276737213,48.5));
#84893=CARTESIAN_POINT('Ctrl Pts',(48.7919510789216,1.84570276737213,48.35));
#84894=CARTESIAN_POINT('',(48.7326739616692,2.1128241121769,48.5));
#84895=CARTESIAN_POINT('Ctrl Pts',(48.7326739616692,2.1128241121769,48.5));
#84896=CARTESIAN_POINT('Ctrl Pts',(48.7326739616692,1.97326058149338,48.5));
#84897=CARTESIAN_POINT('Ctrl Pts',(48.7919510789216,1.84570276737213,48.5));
#84898=CARTESIAN_POINT('',(48.7326739616692,2.1128241121769,48.35));
#84899=CARTESIAN_POINT('',(48.7326739616692,2.1128241121769,48.5));
#84900=CARTESIAN_POINT('Ctrl Pts',(48.7326739616692,2.1128241121769,48.35));
#84901=CARTESIAN_POINT('Ctrl Pts',(48.7326739616692,1.97326058149338,48.35));
#84902=CARTESIAN_POINT('Ctrl Pts',(48.7919510789216,1.84570276737213,48.35));
#84903=CARTESIAN_POINT('Ctrl Pts',(48.8602320738137,2.45723062753677,48.5));
#84904=CARTESIAN_POINT('Ctrl Pts',(48.8602320738137,2.45723062753677,48.35));
#84905=CARTESIAN_POINT('Ctrl Pts',(48.7326739616692,2.32592099905014,48.5));
#84906=CARTESIAN_POINT('Ctrl Pts',(48.7326739616692,2.32592099905014,48.35));
#84907=CARTESIAN_POINT('Ctrl Pts',(48.7326739616692,2.1128241121769,48.5));
#84908=CARTESIAN_POINT('Ctrl Pts',(48.7326739616692,2.1128241121769,48.35));
#84909=CARTESIAN_POINT('Ctrl Pts',(48.8602320738137,2.45723062753677,48.5));
#84910=CARTESIAN_POINT('Ctrl Pts',(48.7326739616692,2.32592099905014,48.5));
#84911=CARTESIAN_POINT('Ctrl Pts',(48.7326739616692,2.1128241121769,48.5));
#84912=CARTESIAN_POINT('Ctrl Pts',(48.8602320738137,2.45723062753677,48.35));
#84913=CARTESIAN_POINT('Ctrl Pts',(48.7326739616692,2.32592099905014,48.35));
#84914=CARTESIAN_POINT('Ctrl Pts',(48.7326739616692,2.1128241121769,48.35));
#84915=CARTESIAN_POINT('Ctrl Pts',(49.211391646415,3.60900411009789,48.5));
#84916=CARTESIAN_POINT('Ctrl Pts',(49.211391646415,3.60900411009789,48.35));
#84917=CARTESIAN_POINT('Ctrl Pts',(49.4710095115006,3.60900411009789,48.5));
#84918=CARTESIAN_POINT('Ctrl Pts',(49.4710095115006,3.60900411009789,48.35));
#84919=CARTESIAN_POINT('Ctrl Pts',(49.6368349976838,3.46343794465065,48.5));
#84920=CARTESIAN_POINT('Ctrl Pts',(49.6368349976838,3.46343794465065,48.35));
#84921=CARTESIAN_POINT('',(49.211391646415,3.60900411009789,48.5));
#84922=CARTESIAN_POINT('',(49.6368349976838,3.46343794465065,48.5));
#84923=CARTESIAN_POINT('Ctrl Pts',(49.211391646415,3.60900411009789,48.5));
#84924=CARTESIAN_POINT('Ctrl Pts',(49.4710095115006,3.60900411009789,48.5));
#84925=CARTESIAN_POINT('Ctrl Pts',(49.6368349976838,3.46343794465065,48.5));
#84926=CARTESIAN_POINT('',(49.211391646415,3.60900411009789,48.35));
#84927=CARTESIAN_POINT('',(49.211391646415,3.60900411009789,48.5));
#84928=CARTESIAN_POINT('',(49.6368349976838,3.46343794465065,48.35));
#84929=CARTESIAN_POINT('Ctrl Pts',(49.211391646415,3.60900411009789,48.35));
#84930=CARTESIAN_POINT('Ctrl Pts',(49.4710095115006,3.60900411009789,48.35));
#84931=CARTESIAN_POINT('Ctrl Pts',(49.6368349976838,3.46343794465065,48.35));
#84932=CARTESIAN_POINT('',(49.6368349976838,3.46343794465065,48.5));
#84933=CARTESIAN_POINT('Ctrl Pts',(48.6576399095356,3.35688957571983,48.5));
#84934=CARTESIAN_POINT('Ctrl Pts',(48.6576399095356,3.35688957571983,48.35));
#84935=CARTESIAN_POINT('Ctrl Pts',(48.8632334657013,3.60900411009789,48.5));
#84936=CARTESIAN_POINT('Ctrl Pts',(48.8632334657013,3.60900411009789,48.35));
#84937=CARTESIAN_POINT('Ctrl Pts',(49.211391646415,3.60900411009789,48.5));
#84938=CARTESIAN_POINT('Ctrl Pts',(49.211391646415,3.60900411009789,48.35));
#84939=CARTESIAN_POINT('',(48.6576399095356,3.35688957571983,48.5));
#84940=CARTESIAN_POINT('Ctrl Pts',(48.6576399095356,3.35688957571983,48.5));
#84941=CARTESIAN_POINT('Ctrl Pts',(48.8632334657013,3.60900411009789,48.5));
#84942=CARTESIAN_POINT('Ctrl Pts',(49.211391646415,3.60900411009789,48.5));
#84943=CARTESIAN_POINT('',(48.6576399095356,3.35688957571983,48.35));
#84944=CARTESIAN_POINT('',(48.6576399095356,3.35688957571983,48.5));
#84945=CARTESIAN_POINT('Ctrl Pts',(48.6576399095356,3.35688957571983,48.35));
#84946=CARTESIAN_POINT('Ctrl Pts',(48.8632334657013,3.60900411009789,48.35));
#84947=CARTESIAN_POINT('Ctrl Pts',(49.211391646415,3.60900411009789,48.35));
#84948=CARTESIAN_POINT('Ctrl Pts',(48.4220328815281,2.42946797609329,48.5));
#84949=CARTESIAN_POINT('Ctrl Pts',(48.4220328815281,2.42946797609329,48.35));
#84950=CARTESIAN_POINT('Ctrl Pts',(48.4220328815281,3.0672579407692,48.5));
#84951=CARTESIAN_POINT('Ctrl Pts',(48.4220328815281,3.0672579407692,48.35));
#84952=CARTESIAN_POINT('Ctrl Pts',(48.6576399095356,3.35688957571983,48.5));
#84953=CARTESIAN_POINT('Ctrl Pts',(48.6576399095356,3.35688957571983,48.35));
#84954=CARTESIAN_POINT('',(48.4220328815281,2.42946797609329,48.5));
#84955=CARTESIAN_POINT('Ctrl Pts',(48.4220328815281,2.42946797609329,48.5));
#84956=CARTESIAN_POINT('Ctrl Pts',(48.4220328815281,3.0672579407692,48.5));
#84957=CARTESIAN_POINT('Ctrl Pts',(48.6576399095356,3.35688957571983,48.5));
#84958=CARTESIAN_POINT('',(48.4220328815281,2.42946797609329,48.35));
#84959=CARTESIAN_POINT('',(48.4220328815281,2.42946797609329,48.5));
#84960=CARTESIAN_POINT('Ctrl Pts',(48.4220328815281,2.42946797609329,48.35));
#84961=CARTESIAN_POINT('Ctrl Pts',(48.4220328815281,3.0672579407692,48.35));
#84962=CARTESIAN_POINT('Ctrl Pts',(48.6576399095356,3.35688957571983,48.35));
#84963=CARTESIAN_POINT('Ctrl Pts',(48.6351297684014,1.61084586381912,48.5));
#84964=CARTESIAN_POINT('Ctrl Pts',(48.6351297684014,1.61084586381912,48.35));
#84965=CARTESIAN_POINT('Ctrl Pts',(48.4220328815281,1.85920888185501,48.5));
#84966=CARTESIAN_POINT('Ctrl Pts',(48.4220328815281,1.85920888185501,48.35));
#84967=CARTESIAN_POINT('Ctrl Pts',(48.4220328815281,2.42946797609329,48.5));
#84968=CARTESIAN_POINT('Ctrl Pts',(48.4220328815281,2.42946797609329,48.35));
#84969=CARTESIAN_POINT('',(48.6351297684014,1.61084586381912,48.5));
#84970=CARTESIAN_POINT('Ctrl Pts',(48.6351297684014,1.61084586381912,48.5));
#84971=CARTESIAN_POINT('Ctrl Pts',(48.4220328815281,1.85920888185501,48.5));
#84972=CARTESIAN_POINT('Ctrl Pts',(48.4220328815281,2.42946797609329,48.5));
#84973=CARTESIAN_POINT('',(48.6351297684014,1.61084586381912,48.35));
#84974=CARTESIAN_POINT('',(48.6351297684014,1.61084586381912,48.5));
#84975=CARTESIAN_POINT('Ctrl Pts',(48.6351297684014,1.61084586381912,48.35));
#84976=CARTESIAN_POINT('Ctrl Pts',(48.4220328815281,1.85920888185501,48.35));
#84977=CARTESIAN_POINT('Ctrl Pts',(48.4220328815281,2.42946797609329,48.35));
#84978=CARTESIAN_POINT('Ctrl Pts',(49.1858801133931,1.36248314380646,48.5));
#84979=CARTESIAN_POINT('Ctrl Pts',(49.1858801133931,1.36248314380646,48.35));
#84980=CARTESIAN_POINT('Ctrl Pts',(48.848226506263,1.36248314380646,48.5));
#84981=CARTESIAN_POINT('Ctrl Pts',(48.848226506263,1.36248314380646,48.35));
#84982=CARTESIAN_POINT('Ctrl Pts',(48.6351297684014,1.61084586381912,48.5));
#84983=CARTESIAN_POINT('Ctrl Pts',(48.6351297684014,1.61084586381912,48.35));
#84984=CARTESIAN_POINT('',(49.1858801133931,1.36248314380646,48.5));
#84985=CARTESIAN_POINT('Ctrl Pts',(49.1858801133931,1.36248314380646,48.5));
#84986=CARTESIAN_POINT('Ctrl Pts',(48.848226506263,1.36248314380646,48.5));
#84987=CARTESIAN_POINT('Ctrl Pts',(48.6351297684014,1.61084586381912,48.5));
#84988=CARTESIAN_POINT('',(49.1858801133931,1.36248314380646,48.35));
#84989=CARTESIAN_POINT('',(49.1858801133931,1.36248314380646,48.5));
#84990=CARTESIAN_POINT('Ctrl Pts',(49.1858801133931,1.36248314380646,48.35));
#84991=CARTESIAN_POINT('Ctrl Pts',(48.848226506263,1.36248314380646,48.35));
#84992=CARTESIAN_POINT('Ctrl Pts',(48.6351297684014,1.61084586381912,48.35));
#84993=CARTESIAN_POINT('Ctrl Pts',(49.5400412268937,1.45702594518662,48.5));
#84994=CARTESIAN_POINT('Ctrl Pts',(49.5400412268937,1.45702594518662,48.35));
#84995=CARTESIAN_POINT('Ctrl Pts',(49.383970040828,1.36248314380646,48.5));
#84996=CARTESIAN_POINT('Ctrl Pts',(49.383970040828,1.36248314380646,48.35));
#84997=CARTESIAN_POINT('Ctrl Pts',(49.1858801133931,1.36248314380646,48.5));
#84998=CARTESIAN_POINT('Ctrl Pts',(49.1858801133931,1.36248314380646,48.35));
#84999=CARTESIAN_POINT('',(49.5400412268937,1.45702594518662,48.5));
#85000=CARTESIAN_POINT('Ctrl Pts',(49.5400412268937,1.45702594518662,48.5));
#85001=CARTESIAN_POINT('Ctrl Pts',(49.383970040828,1.36248314380646,48.5));
#85002=CARTESIAN_POINT('Ctrl Pts',(49.1858801133931,1.36248314380646,48.5));
#85003=CARTESIAN_POINT('',(49.5400412268937,1.45702594518662,48.35));
#85004=CARTESIAN_POINT('',(49.5400412268937,1.45702594518662,48.5));
#85005=CARTESIAN_POINT('Ctrl Pts',(49.5400412268937,1.45702594518662,48.35));
#85006=CARTESIAN_POINT('Ctrl Pts',(49.383970040828,1.36248314380646,48.35));
#85007=CARTESIAN_POINT('Ctrl Pts',(49.1858801133931,1.36248314380646,48.35));
#85008=CARTESIAN_POINT('Ctrl Pts',(49.7854025550187,1.7293998003006,48.5));
#85009=CARTESIAN_POINT('Ctrl Pts',(49.7854025550187,1.7293998003006,48.35));
#85010=CARTESIAN_POINT('Ctrl Pts',(49.6961118169129,1.55156904459,48.5));
#85011=CARTESIAN_POINT('Ctrl Pts',(49.6961118169129,1.55156904459,48.35));
#85012=CARTESIAN_POINT('Ctrl Pts',(49.5400412268937,1.45702594518662,48.5));
#85013=CARTESIAN_POINT('Ctrl Pts',(49.5400412268937,1.45702594518662,48.35));
#85014=CARTESIAN_POINT('',(49.7854025550187,1.7293998003006,48.5));
#85015=CARTESIAN_POINT('Ctrl Pts',(49.7854025550187,1.7293998003006,48.5));
#85016=CARTESIAN_POINT('Ctrl Pts',(49.6961118169129,1.55156904459,48.5));
#85017=CARTESIAN_POINT('Ctrl Pts',(49.5400412268937,1.45702594518662,48.5));
#85018=CARTESIAN_POINT('',(49.7854025550187,1.7293998003006,48.35));
#85019=CARTESIAN_POINT('',(49.7854025550187,1.7293998003006,48.5));
#85020=CARTESIAN_POINT('Ctrl Pts',(49.7854025550187,1.7293998003006,48.35));
#85021=CARTESIAN_POINT('Ctrl Pts',(49.6961118169129,1.55156904459,48.35));
#85022=CARTESIAN_POINT('Ctrl Pts',(49.5400412268937,1.45702594518662,48.35));
#85023=CARTESIAN_POINT('Ctrl Pts',(49.8746932931244,2.11432480812073,48.5));
#85024=CARTESIAN_POINT('Ctrl Pts',(49.8746932931244,2.11432480812073,48.35));
#85025=CARTESIAN_POINT('Ctrl Pts',(49.8746932931244,1.9072305560112,48.5));
#85026=CARTESIAN_POINT('Ctrl Pts',(49.8746932931244,1.9072305560112,48.35));
#85027=CARTESIAN_POINT('Ctrl Pts',(49.7854025550187,1.7293998003006,48.5));
#85028=CARTESIAN_POINT('Ctrl Pts',(49.7854025550187,1.7293998003006,48.35));
#85029=CARTESIAN_POINT('',(49.8746932931244,2.11432480812073,48.5));
#85030=CARTESIAN_POINT('Ctrl Pts',(49.8746932931244,2.11432480812073,48.5));
#85031=CARTESIAN_POINT('Ctrl Pts',(49.8746932931244,1.9072305560112,48.5));
#85032=CARTESIAN_POINT('Ctrl Pts',(49.7854025550187,1.7293998003006,48.5));
#85033=CARTESIAN_POINT('',(49.8746932931244,2.11432480812073,48.35));
#85034=CARTESIAN_POINT('',(49.8746932931244,2.11432480812073,48.5));
#85035=CARTESIAN_POINT('Ctrl Pts',(49.8746932931244,2.11432480812073,48.35));
#85036=CARTESIAN_POINT('Ctrl Pts',(49.8746932931244,1.9072305560112,48.35));
#85037=CARTESIAN_POINT('Ctrl Pts',(49.7854025550187,1.7293998003006,48.35));
#85038=CARTESIAN_POINT('Ctrl Pts',(49.68485667184,2.62830847501755,48.5));
#85039=CARTESIAN_POINT('Ctrl Pts',(49.68485667184,2.62830847501755,48.35));
#85040=CARTESIAN_POINT('Ctrl Pts',(49.8746932931244,2.42946797609329,48.5));
#85041=CARTESIAN_POINT('Ctrl Pts',(49.8746932931244,2.42946797609329,48.35));
#85042=CARTESIAN_POINT('Ctrl Pts',(49.8746932931244,2.11432480812073,48.5));
#85043=CARTESIAN_POINT('Ctrl Pts',(49.8746932931244,2.11432480812073,48.35));
#85044=CARTESIAN_POINT('',(49.68485667184,2.62830847501755,48.5));
#85045=CARTESIAN_POINT('Ctrl Pts',(49.68485667184,2.62830847501755,48.5));
#85046=CARTESIAN_POINT('Ctrl Pts',(49.8746932931244,2.42946797609329,48.5));
#85047=CARTESIAN_POINT('Ctrl Pts',(49.8746932931244,2.11432480812073,48.5));
#85048=CARTESIAN_POINT('',(49.68485667184,2.62830847501755,48.35));
#85049=CARTESIAN_POINT('',(49.68485667184,2.62830847501755,48.5));
#85050=CARTESIAN_POINT('Ctrl Pts',(49.68485667184,2.62830847501755,48.35));
#85051=CARTESIAN_POINT('Ctrl Pts',(49.8746932931244,2.42946797609329,48.35));
#85052=CARTESIAN_POINT('Ctrl Pts',(49.8746932931244,2.11432480812073,48.35));
#85053=CARTESIAN_POINT('Ctrl Pts',(49.2248977608979,2.82714867591858,48.5));
#85054=CARTESIAN_POINT('Ctrl Pts',(49.2248977608979,2.82714867591858,48.35));
#85055=CARTESIAN_POINT('Ctrl Pts',(49.4950206466019,2.82714867591858,48.5));
#85056=CARTESIAN_POINT('Ctrl Pts',(49.4950206466019,2.82714867591858,48.35));
#85057=CARTESIAN_POINT('Ctrl Pts',(49.68485667184,2.62830847501755,48.5));
#85058=CARTESIAN_POINT('Ctrl Pts',(49.68485667184,2.62830847501755,48.35));
#85059=CARTESIAN_POINT('',(49.2248977608979,2.82714867591858,48.5));
#85060=CARTESIAN_POINT('Ctrl Pts',(49.2248977608979,2.82714867591858,48.5));
#85061=CARTESIAN_POINT('Ctrl Pts',(49.4950206466019,2.82714867591858,48.5));
#85062=CARTESIAN_POINT('Ctrl Pts',(49.68485667184,2.62830847501755,48.5));
#85063=CARTESIAN_POINT('',(49.2248977608979,2.82714867591858,48.35));
#85064=CARTESIAN_POINT('',(49.2248977608979,2.82714867591858,48.5));
#85065=CARTESIAN_POINT('Ctrl Pts',(49.2248977608979,2.82714867591858,48.35));
#85066=CARTESIAN_POINT('Ctrl Pts',(49.4950206466019,2.82714867591858,48.35));
#85067=CARTESIAN_POINT('Ctrl Pts',(49.68485667184,2.62830847501755,48.35));
#85068=CARTESIAN_POINT('Ctrl Pts',(48.9292634911835,2.75511601567268,48.5));
#85069=CARTESIAN_POINT('Ctrl Pts',(48.9292634911835,2.75511601567268,48.35));
#85070=CARTESIAN_POINT('Ctrl Pts',(49.0703275687993,2.82714867591858,48.5));
#85071=CARTESIAN_POINT('Ctrl Pts',(49.0703275687993,2.82714867591858,48.35));
#85072=CARTESIAN_POINT('Ctrl Pts',(49.2248977608979,2.82714867591858,48.5));
#85073=CARTESIAN_POINT('Ctrl Pts',(49.2248977608979,2.82714867591858,48.35));
#85074=CARTESIAN_POINT('',(48.9292634911835,2.75511601567268,48.5));
#85075=CARTESIAN_POINT('Ctrl Pts',(48.9292634911835,2.75511601567268,48.5));
#85076=CARTESIAN_POINT('Ctrl Pts',(49.0703275687993,2.82714867591858,48.5));
#85077=CARTESIAN_POINT('Ctrl Pts',(49.2248977608979,2.82714867591858,48.5));
#85078=CARTESIAN_POINT('',(48.9292634911835,2.75511601567268,48.35));
#85079=CARTESIAN_POINT('',(48.9292634911835,2.75511601567268,48.5));
#85080=CARTESIAN_POINT('Ctrl Pts',(48.9292634911835,2.75511601567268,48.35));
#85081=CARTESIAN_POINT('Ctrl Pts',(49.0703275687993,2.82714867591858,48.35));
#85082=CARTESIAN_POINT('Ctrl Pts',(49.2248977608979,2.82714867591858,48.35));
#85083=CARTESIAN_POINT('Ctrl Pts',(48.6906549222767,2.53451579809189,48.5));
#85084=CARTESIAN_POINT('Ctrl Pts',(48.6906549222767,2.53451579809189,48.35));
#85085=CARTESIAN_POINT('Ctrl Pts',(48.7881992645562,2.68308320641518,48.5));
#85086=CARTESIAN_POINT('Ctrl Pts',(48.7881992645562,2.68308320641518,48.35));
#85087=CARTESIAN_POINT('Ctrl Pts',(48.9292634911835,2.75511601567268,48.5));
#85088=CARTESIAN_POINT('Ctrl Pts',(48.9292634911835,2.75511601567268,48.35));
#85089=CARTESIAN_POINT('',(48.6906549222767,2.53451579809189,48.5));
#85090=CARTESIAN_POINT('Ctrl Pts',(48.6906549222767,2.53451579809189,48.5));
#85091=CARTESIAN_POINT('Ctrl Pts',(48.7881992645562,2.68308320641518,48.5));
#85092=CARTESIAN_POINT('Ctrl Pts',(48.9292634911835,2.75511601567268,48.5));
#85093=CARTESIAN_POINT('',(48.6906549222767,2.53451579809189,48.35));
#85094=CARTESIAN_POINT('',(48.6906549222767,2.53451579809189,48.5));
#85095=CARTESIAN_POINT('Ctrl Pts',(48.6906549222767,2.53451579809189,48.35));
#85096=CARTESIAN_POINT('Ctrl Pts',(48.7881992645562,2.68308320641518,48.35));
#85097=CARTESIAN_POINT('Ctrl Pts',(48.9292634911835,2.75511601567268,48.35));
#85098=CARTESIAN_POINT('Ctrl Pts',(48.7671898193657,3.04324695467949,48.5));
#85099=CARTESIAN_POINT('Ctrl Pts',(48.7671898193657,3.04324695467949,48.35));
#85100=CARTESIAN_POINT('Ctrl Pts',(48.6936563141644,2.86466577649117,48.5));
#85101=CARTESIAN_POINT('Ctrl Pts',(48.6936563141644,2.86466577649117,48.35));
#85102=CARTESIAN_POINT('Ctrl Pts',(48.6906549222767,2.53451579809189,48.5));
#85103=CARTESIAN_POINT('Ctrl Pts',(48.6906549222767,2.53451579809189,48.35));
#85104=CARTESIAN_POINT('',(48.7671898193657,3.04324695467949,48.5));
#85105=CARTESIAN_POINT('Ctrl Pts',(48.7671898193657,3.04324695467949,48.5));
#85106=CARTESIAN_POINT('Ctrl Pts',(48.6936563141644,2.86466577649117,48.5));
#85107=CARTESIAN_POINT('Ctrl Pts',(48.6906549222767,2.53451579809189,48.5));
#85108=CARTESIAN_POINT('',(48.7671898193657,3.04324695467949,48.35));
#85109=CARTESIAN_POINT('',(48.7671898193657,3.04324695467949,48.5));
#85110=CARTESIAN_POINT('Ctrl Pts',(48.7671898193657,3.04324695467949,48.35));
#85111=CARTESIAN_POINT('Ctrl Pts',(48.6936563141644,2.86466577649117,48.35));
#85112=CARTESIAN_POINT('Ctrl Pts',(48.6906549222767,2.53451579809189,48.35));
#85113=CARTESIAN_POINT('Ctrl Pts',(48.9682811386883,3.31487038731575,48.5));
#85114=CARTESIAN_POINT('Ctrl Pts',(48.9682811386883,3.31487038731575,48.35));
#85115=CARTESIAN_POINT('Ctrl Pts',(48.8407231755555,3.22182813286781,48.5));
#85116=CARTESIAN_POINT('Ctrl Pts',(48.8407231755555,3.22182813286781,48.35));
#85117=CARTESIAN_POINT('Ctrl Pts',(48.7671898193657,3.04324695467949,48.5));
#85118=CARTESIAN_POINT('Ctrl Pts',(48.7671898193657,3.04324695467949,48.35));
#85119=CARTESIAN_POINT('',(48.9682811386883,3.31487038731575,48.5));
#85120=CARTESIAN_POINT('Ctrl Pts',(48.9682811386883,3.31487038731575,48.5));
#85121=CARTESIAN_POINT('Ctrl Pts',(48.8407231755555,3.22182813286781,48.5));
#85122=CARTESIAN_POINT('Ctrl Pts',(48.7671898193657,3.04324695467949,48.5));
#85123=CARTESIAN_POINT('',(48.9682811386883,3.31487038731575,48.35));
#85124=CARTESIAN_POINT('',(48.9682811386883,3.31487038731575,48.5));
#85125=CARTESIAN_POINT('Ctrl Pts',(48.9682811386883,3.31487038731575,48.35));
#85126=CARTESIAN_POINT('Ctrl Pts',(48.8407231755555,3.22182813286781,48.35));
#85127=CARTESIAN_POINT('Ctrl Pts',(48.7671898193657,3.04324695467949,48.35));
#85128=CARTESIAN_POINT('Ctrl Pts',(49.1948841400445,3.38690319657326,48.5));
#85129=CARTESIAN_POINT('Ctrl Pts',(49.1948841400445,3.38690319657326,48.35));
#85130=CARTESIAN_POINT('Ctrl Pts',(49.0658254809678,3.38690319657326,48.5));
#85131=CARTESIAN_POINT('Ctrl Pts',(49.0658254809678,3.38690319657326,48.35));
#85132=CARTESIAN_POINT('Ctrl Pts',(48.9682811386883,3.31487038731575,48.5));
#85133=CARTESIAN_POINT('Ctrl Pts',(48.9682811386883,3.31487038731575,48.35));
#85134=CARTESIAN_POINT('',(49.1948841400445,3.38690319657326,48.5));
#85135=CARTESIAN_POINT('Ctrl Pts',(49.1948841400445,3.38690319657326,48.5));
#85136=CARTESIAN_POINT('Ctrl Pts',(49.0658254809678,3.38690319657326,48.5));
#85137=CARTESIAN_POINT('Ctrl Pts',(48.9682811386883,3.31487038731575,48.5));
#85138=CARTESIAN_POINT('',(49.1948841400445,3.38690319657326,48.35));
#85139=CARTESIAN_POINT('',(49.1948841400445,3.38690319657326,48.5));
#85140=CARTESIAN_POINT('Ctrl Pts',(49.1948841400445,3.38690319657326,48.35));
#85141=CARTESIAN_POINT('Ctrl Pts',(49.0658254809678,3.38690319657326,48.35));
#85142=CARTESIAN_POINT('Ctrl Pts',(48.9682811386883,3.31487038731575,48.35));
#85143=CARTESIAN_POINT('Ctrl Pts',(49.4650070257485,3.27135065197945,48.5));
#85144=CARTESIAN_POINT('Ctrl Pts',(49.4650070257485,3.27135065197945,48.35));
#85145=CARTESIAN_POINT('Ctrl Pts',(49.35545726493,3.38690319657326,48.5));
#85146=CARTESIAN_POINT('Ctrl Pts',(49.35545726493,3.38690319657326,48.35));
#85147=CARTESIAN_POINT('Ctrl Pts',(49.1948841400445,3.38690319657326,48.5));
#85148=CARTESIAN_POINT('Ctrl Pts',(49.1948841400445,3.38690319657326,48.35));
#85149=CARTESIAN_POINT('',(49.4650070257485,3.27135065197945,48.5));
#85150=CARTESIAN_POINT('Ctrl Pts',(49.4650070257485,3.27135065197945,48.5));
#85151=CARTESIAN_POINT('Ctrl Pts',(49.35545726493,3.38690319657326,48.5));
#85152=CARTESIAN_POINT('Ctrl Pts',(49.1948841400445,3.38690319657326,48.5));
#85153=CARTESIAN_POINT('',(49.4650070257485,3.27135065197945,48.35));
#85154=CARTESIAN_POINT('',(49.4650070257485,3.27135065197945,48.5));
#85155=CARTESIAN_POINT('Ctrl Pts',(49.4650070257485,3.27135065197945,48.35));
#85156=CARTESIAN_POINT('Ctrl Pts',(49.35545726493,3.38690319657326,48.35));
#85157=CARTESIAN_POINT('Ctrl Pts',(49.1948841400445,3.38690319657326,48.35));
#85158=CARTESIAN_POINT('Ctrl Pts',(49.5670534558594,3.04024556279182,48.5));
#85159=CARTESIAN_POINT('Ctrl Pts',(49.5670534558594,3.04024556279182,48.35));
#85160=CARTESIAN_POINT('Ctrl Pts',(49.5310370512307,3.19931784272194,48.5));
#85161=CARTESIAN_POINT('Ctrl Pts',(49.5310370512307,3.19931784272194,48.35));
#85162=CARTESIAN_POINT('Ctrl Pts',(49.4650070257485,3.27135065197945,48.5));
#85163=CARTESIAN_POINT('Ctrl Pts',(49.4650070257485,3.27135065197945,48.35));
#85164=CARTESIAN_POINT('',(49.5670534558594,3.04024556279182,48.5));
#85165=CARTESIAN_POINT('Ctrl Pts',(49.5670534558594,3.04024556279182,48.5));
#85166=CARTESIAN_POINT('Ctrl Pts',(49.5310370512307,3.19931784272194,48.5));
#85167=CARTESIAN_POINT('Ctrl Pts',(49.4650070257485,3.27135065197945,48.5));
#85168=CARTESIAN_POINT('',(49.5670534558594,3.04024556279182,48.35));
#85169=CARTESIAN_POINT('',(49.5670534558594,3.04024556279182,48.5));
#85170=CARTESIAN_POINT('Ctrl Pts',(49.5670534558594,3.04024556279182,48.35));
#85171=CARTESIAN_POINT('Ctrl Pts',(49.5310370512307,3.19931784272194,48.35));
#85172=CARTESIAN_POINT('Ctrl Pts',(49.4650070257485,3.27135065197945,48.35));
#85173=CARTESIAN_POINT('Origin',(49.835675496608,3.06125515699387,48.5));
#85174=CARTESIAN_POINT('',(49.835675496608,3.06125515699387,48.5));
#85175=CARTESIAN_POINT('',(25.2612996235975,1.13923243904573,48.5));
#85176=CARTESIAN_POINT('',(49.835675496608,3.06125515699387,48.35));
#85177=CARTESIAN_POINT('',(49.835675496608,3.06125515699387,48.5));
#85178=CARTESIAN_POINT('',(49.835675496608,3.06125515699387,48.35));
#85179=CARTESIAN_POINT('Ctrl Pts',(49.6368349976838,3.46343794465065,48.5));
#85180=CARTESIAN_POINT('Ctrl Pts',(49.6368349976838,3.46343794465065,48.35));
#85181=CARTESIAN_POINT('Ctrl Pts',(49.8026604838669,3.31787177920341,48.5));
#85182=CARTESIAN_POINT('Ctrl Pts',(49.8026604838669,3.31787177920341,48.35));
#85183=CARTESIAN_POINT('Ctrl Pts',(49.835675496608,3.06125515699387,48.5));
#85184=CARTESIAN_POINT('Ctrl Pts',(49.835675496608,3.06125515699387,48.35));
#85185=CARTESIAN_POINT('Ctrl Pts',(49.6368349976838,3.46343794465065,48.5));
#85186=CARTESIAN_POINT('Ctrl Pts',(49.8026604838669,3.31787177920341,48.5));
#85187=CARTESIAN_POINT('Ctrl Pts',(49.835675496608,3.06125515699387,48.5));
#85188=CARTESIAN_POINT('Ctrl Pts',(49.6368349976838,3.46343794465065,48.35));
#85189=CARTESIAN_POINT('Ctrl Pts',(49.8026604838669,3.31787177920341,48.35));
#85190=CARTESIAN_POINT('Ctrl Pts',(49.835675496608,3.06125515699387,48.35));
#85191=CARTESIAN_POINT('Origin',(49.9999999143183,2.48574362695217,48.35));
#85192=CARTESIAN_POINT('Origin',(0.,8.,48.5));
#85193=CARTESIAN_POINT('Origin',(0.,8.,48.5));
#85194=CARTESIAN_POINT('Ctrl Pts',(40.8426330685616,3.38540250062943,48.5));
#85195=CARTESIAN_POINT('Ctrl Pts',(40.8426330685616,3.38540250062943,48.35));
#85196=CARTESIAN_POINT('Ctrl Pts',(40.6565482616425,3.38540250062943,48.5));
#85197=CARTESIAN_POINT('Ctrl Pts',(40.6565482616425,3.38540250062943,48.35));
#85198=CARTESIAN_POINT('Ctrl Pts',(40.5454979538918,3.22783091664314,48.5));
#85199=CARTESIAN_POINT('Ctrl Pts',(40.5454979538918,3.22783091664314,48.35));
#85200=CARTESIAN_POINT('',(40.8426330685616,3.38540250062943,48.5));
#85201=CARTESIAN_POINT('',(40.5454979538918,3.22783091664314,48.5));
#85202=CARTESIAN_POINT('Ctrl Pts',(40.8426330685616,3.38540250062943,48.5));
#85203=CARTESIAN_POINT('Ctrl Pts',(40.6565482616425,3.38540250062943,48.5));
#85204=CARTESIAN_POINT('Ctrl Pts',(40.5454979538918,3.22783091664314,48.5));
#85205=CARTESIAN_POINT('',(40.8426330685616,3.38540250062943,48.35));
#85206=CARTESIAN_POINT('',(40.8426330685616,3.38540250062943,48.5));
#85207=CARTESIAN_POINT('',(40.5454979538918,3.22783091664314,48.35));
#85208=CARTESIAN_POINT('Ctrl Pts',(40.8426330685616,3.38540250062943,48.35));
#85209=CARTESIAN_POINT('Ctrl Pts',(40.6565482616425,3.38540250062943,48.35));
#85210=CARTESIAN_POINT('Ctrl Pts',(40.5454979538918,3.22783091664314,48.35));
#85211=CARTESIAN_POINT('',(40.5454979538918,3.22783091664314,48.5));
#85212=CARTESIAN_POINT('Ctrl Pts',(41.1585263609886,3.2068213224411,48.5));
#85213=CARTESIAN_POINT('Ctrl Pts',(41.1585263609886,3.2068213224411,48.35));
#85214=CARTESIAN_POINT('Ctrl Pts',(41.0317186713219,3.38540250062943,48.5));
#85215=CARTESIAN_POINT('Ctrl Pts',(41.0317186713219,3.38540250062943,48.35));
#85216=CARTESIAN_POINT('Ctrl Pts',(40.8426330685616,3.38540250062943,48.5));
#85217=CARTESIAN_POINT('Ctrl Pts',(40.8426330685616,3.38540250062943,48.35));
#85218=CARTESIAN_POINT('',(41.1585263609886,3.2068213224411,48.5));
#85219=CARTESIAN_POINT('Ctrl Pts',(41.1585263609886,3.2068213224411,48.5));
#85220=CARTESIAN_POINT('Ctrl Pts',(41.0317186713219,3.38540250062943,48.5));
#85221=CARTESIAN_POINT('Ctrl Pts',(40.8426330685616,3.38540250062943,48.5));
#85222=CARTESIAN_POINT('',(41.1585263609886,3.2068213224411,48.35));
#85223=CARTESIAN_POINT('',(41.1585263609886,3.2068213224411,48.5));
#85224=CARTESIAN_POINT('Ctrl Pts',(41.1585263609886,3.2068213224411,48.35));
#85225=CARTESIAN_POINT('Ctrl Pts',(41.0317186713219,3.38540250062943,48.35));
#85226=CARTESIAN_POINT('Ctrl Pts',(40.8426330685616,3.38540250062943,48.35));
#85227=CARTESIAN_POINT('Ctrl Pts',(41.2853340506554,2.48499327898026,48.5));
#85228=CARTESIAN_POINT('Ctrl Pts',(41.2853340506554,2.48499327898026,48.35));
#85229=CARTESIAN_POINT('Ctrl Pts',(41.2853340506554,3.02824014425278,48.5));
#85230=CARTESIAN_POINT('Ctrl Pts',(41.2853340506554,3.02824014425278,48.35));
#85231=CARTESIAN_POINT('Ctrl Pts',(41.1585263609886,3.2068213224411,48.5));
#85232=CARTESIAN_POINT('Ctrl Pts',(41.1585263609886,3.2068213224411,48.35));
#85233=CARTESIAN_POINT('',(41.2853340506554,2.48499327898026,48.5));
#85234=CARTESIAN_POINT('Ctrl Pts',(41.2853340506554,2.48499327898026,48.5));
#85235=CARTESIAN_POINT('Ctrl Pts',(41.2853340506554,3.02824014425278,48.5));
#85236=CARTESIAN_POINT('Ctrl Pts',(41.1585263609886,3.2068213224411,48.5));
#85237=CARTESIAN_POINT('',(41.2853340506554,2.48499327898026,48.35));
#85238=CARTESIAN_POINT('',(41.2853340506554,2.48499327898026,48.5));
#85239=CARTESIAN_POINT('Ctrl Pts',(41.2853340506554,2.48499327898026,48.35));
#85240=CARTESIAN_POINT('Ctrl Pts',(41.2853340506554,3.02824014425278,48.35));
#85241=CARTESIAN_POINT('Ctrl Pts',(41.1585263609886,3.2068213224411,48.35));
#85242=CARTESIAN_POINT('Ctrl Pts',(41.1585263609886,1.76466578245163,48.5));
#85243=CARTESIAN_POINT('Ctrl Pts',(41.1585263609886,1.76466578245163,48.35));
#85244=CARTESIAN_POINT('Ctrl Pts',(41.2853340506554,1.9447478055954,48.5));
#85245=CARTESIAN_POINT('Ctrl Pts',(41.2853340506554,1.9447478055954,48.35));
#85246=CARTESIAN_POINT('Ctrl Pts',(41.2853340506554,2.48499327898026,48.5));
#85247=CARTESIAN_POINT('Ctrl Pts',(41.2853340506554,2.48499327898026,48.35));
#85248=CARTESIAN_POINT('',(41.1585263609886,1.76466578245163,48.5));
#85249=CARTESIAN_POINT('Ctrl Pts',(41.1585263609886,1.76466578245163,48.5));
#85250=CARTESIAN_POINT('Ctrl Pts',(41.2853340506554,1.9447478055954,48.5));
#85251=CARTESIAN_POINT('Ctrl Pts',(41.2853340506554,2.48499327898026,48.5));
#85252=CARTESIAN_POINT('',(41.1585263609886,1.76466578245163,48.35));
#85253=CARTESIAN_POINT('',(41.1585263609886,1.76466578245163,48.5));
#85254=CARTESIAN_POINT('Ctrl Pts',(41.1585263609886,1.76466578245163,48.35));
#85255=CARTESIAN_POINT('Ctrl Pts',(41.2853340506554,1.9447478055954,48.35));
#85256=CARTESIAN_POINT('Ctrl Pts',(41.2853340506554,2.48499327898026,48.35));
#85257=CARTESIAN_POINT('Ctrl Pts',(40.845634162426,1.58458405733109,48.5));
#85258=CARTESIAN_POINT('Ctrl Pts',(40.845634162426,1.58458405733109,48.35));
#85259=CARTESIAN_POINT('Ctrl Pts',(41.0317186713219,1.58458405733109,48.5));
#85260=CARTESIAN_POINT('Ctrl Pts',(41.0317186713219,1.58458405733109,48.35));
#85261=CARTESIAN_POINT('Ctrl Pts',(41.1585263609886,1.76466578245163,48.5));
#85262=CARTESIAN_POINT('Ctrl Pts',(41.1585263609886,1.76466578245163,48.35));
#85263=CARTESIAN_POINT('',(40.845634162426,1.58458405733109,48.5));
#85264=CARTESIAN_POINT('Ctrl Pts',(40.845634162426,1.58458405733109,48.5));
#85265=CARTESIAN_POINT('Ctrl Pts',(41.0317186713219,1.58458405733109,48.5));
#85266=CARTESIAN_POINT('Ctrl Pts',(41.1585263609886,1.76466578245163,48.5));
#85267=CARTESIAN_POINT('',(40.845634162426,1.58458405733109,48.35));
#85268=CARTESIAN_POINT('',(40.845634162426,1.58458405733109,48.5));
#85269=CARTESIAN_POINT('Ctrl Pts',(40.845634162426,1.58458405733109,48.35));
#85270=CARTESIAN_POINT('Ctrl Pts',(41.0317186713219,1.58458405733109,48.35));
#85271=CARTESIAN_POINT('Ctrl Pts',(41.1585263609886,1.76466578245163,48.35));
#85272=CARTESIAN_POINT('Ctrl Pts',(40.5327419638634,1.76391565799713,48.5));
#85273=CARTESIAN_POINT('Ctrl Pts',(40.5327419638634,1.76391565799713,48.35));
#85274=CARTESIAN_POINT('Ctrl Pts',(40.6595496535301,1.58458405733109,48.5));
#85275=CARTESIAN_POINT('Ctrl Pts',(40.6595496535301,1.58458405733109,48.35));
#85276=CARTESIAN_POINT('Ctrl Pts',(40.845634162426,1.58458405733109,48.5));
#85277=CARTESIAN_POINT('Ctrl Pts',(40.845634162426,1.58458405733109,48.35));
#85278=CARTESIAN_POINT('',(40.5327419638634,1.76391565799713,48.5));
#85279=CARTESIAN_POINT('Ctrl Pts',(40.5327419638634,1.76391565799713,48.5));
#85280=CARTESIAN_POINT('Ctrl Pts',(40.6595496535301,1.58458405733109,48.5));
#85281=CARTESIAN_POINT('Ctrl Pts',(40.845634162426,1.58458405733109,48.5));
#85282=CARTESIAN_POINT('',(40.5327419638634,1.76391565799713,48.35));
#85283=CARTESIAN_POINT('',(40.5327419638634,1.76391565799713,48.5));
#85284=CARTESIAN_POINT('Ctrl Pts',(40.5327419638634,1.76391565799713,48.35));
#85285=CARTESIAN_POINT('Ctrl Pts',(40.6595496535301,1.58458405733109,48.35));
#85286=CARTESIAN_POINT('Ctrl Pts',(40.845634162426,1.58458405733109,48.35));
#85287=CARTESIAN_POINT('Ctrl Pts',(40.4059342741966,2.48499327898026,48.5));
#85288=CARTESIAN_POINT('Ctrl Pts',(40.4059342741966,2.48499327898026,48.35));
#85289=CARTESIAN_POINT('Ctrl Pts',(40.4059342741966,1.94324696063995,48.5));
#85290=CARTESIAN_POINT('Ctrl Pts',(40.4059342741966,1.94324696063995,48.35));
#85291=CARTESIAN_POINT('Ctrl Pts',(40.5327419638634,1.76391565799713,48.5));
#85292=CARTESIAN_POINT('Ctrl Pts',(40.5327419638634,1.76391565799713,48.35));
#85293=CARTESIAN_POINT('',(40.4059342741966,2.48499327898026,48.5));
#85294=CARTESIAN_POINT('Ctrl Pts',(40.4059342741966,2.48499327898026,48.5));
#85295=CARTESIAN_POINT('Ctrl Pts',(40.4059342741966,1.94324696063995,48.5));
#85296=CARTESIAN_POINT('Ctrl Pts',(40.5327419638634,1.76391565799713,48.5));
#85297=CARTESIAN_POINT('',(40.4059342741966,2.48499327898026,48.35));
#85298=CARTESIAN_POINT('',(40.4059342741966,2.48499327898026,48.5));
#85299=CARTESIAN_POINT('Ctrl Pts',(40.4059342741966,2.48499327898026,48.35));
#85300=CARTESIAN_POINT('Ctrl Pts',(40.4059342741966,1.94324696063995,48.35));
#85301=CARTESIAN_POINT('Ctrl Pts',(40.5327419638634,1.76391565799713,48.35));
#85302=CARTESIAN_POINT('Ctrl Pts',(40.5454979538918,3.22783091664314,48.5));
#85303=CARTESIAN_POINT('Ctrl Pts',(40.5454979538918,3.22783091664314,48.35));
#85304=CARTESIAN_POINT('Ctrl Pts',(40.4059342741966,3.02673944830894,48.5));
#85305=CARTESIAN_POINT('Ctrl Pts',(40.4059342741966,3.02673944830894,48.35));
#85306=CARTESIAN_POINT('Ctrl Pts',(40.4059342741966,2.48499327898026,48.5));
#85307=CARTESIAN_POINT('Ctrl Pts',(40.4059342741966,2.48499327898026,48.35));
#85308=CARTESIAN_POINT('Ctrl Pts',(40.5454979538918,3.22783091664314,48.5));
#85309=CARTESIAN_POINT('Ctrl Pts',(40.4059342741966,3.02673944830894,48.5));
#85310=CARTESIAN_POINT('Ctrl Pts',(40.4059342741966,2.48499327898026,48.5));
#85311=CARTESIAN_POINT('Ctrl Pts',(40.5454979538918,3.22783091664314,48.35));
#85312=CARTESIAN_POINT('Ctrl Pts',(40.4059342741966,3.02673944830894,48.35));
#85313=CARTESIAN_POINT('Ctrl Pts',(40.4059342741966,2.48499327898026,48.35));
#85314=CARTESIAN_POINT('Ctrl Pts',(40.845634162426,1.36248314380646,48.5));
#85315=CARTESIAN_POINT('Ctrl Pts',(40.845634162426,1.36248314380646,48.35));
#85316=CARTESIAN_POINT('Ctrl Pts',(40.5274896025658,1.36248314380646,48.5));
#85317=CARTESIAN_POINT('Ctrl Pts',(40.5274896025658,1.36248314380646,48.35));
#85318=CARTESIAN_POINT('Ctrl Pts',(40.3459070324898,1.59058684110642,48.5));
#85319=CARTESIAN_POINT('Ctrl Pts',(40.3459070324898,1.59058684110642,48.35));
#85320=CARTESIAN_POINT('',(40.845634162426,1.36248314380646,48.5));
#85321=CARTESIAN_POINT('',(40.3459070324898,1.59058684110642,48.5));
#85322=CARTESIAN_POINT('Ctrl Pts',(40.845634162426,1.36248314380646,48.5));
#85323=CARTESIAN_POINT('Ctrl Pts',(40.5274896025658,1.36248314380646,48.5));
#85324=CARTESIAN_POINT('Ctrl Pts',(40.3459070324898,1.59058684110642,48.5));
#85325=CARTESIAN_POINT('',(40.845634162426,1.36248314380646,48.35));
#85326=CARTESIAN_POINT('',(40.845634162426,1.36248314380646,48.5));
#85327=CARTESIAN_POINT('',(40.3459070324898,1.59058684110642,48.35));
#85328=CARTESIAN_POINT('Ctrl Pts',(40.845634162426,1.36248314380646,48.35));
#85329=CARTESIAN_POINT('Ctrl Pts',(40.5274896025658,1.36248314380646,48.35));
#85330=CARTESIAN_POINT('Ctrl Pts',(40.3459070324898,1.59058684110642,48.35));
#85331=CARTESIAN_POINT('',(40.3459070324898,1.59058684110642,48.5));
#85332=CARTESIAN_POINT('Ctrl Pts',(41.2455658316612,1.49229192733765,48.5));
#85333=CARTESIAN_POINT('Ctrl Pts',(41.2455658316612,1.49229192733765,48.35));
#85334=CARTESIAN_POINT('Ctrl Pts',(41.0872439742088,1.36248314380646,48.5));
#85335=CARTESIAN_POINT('Ctrl Pts',(41.0872439742088,1.36248314380646,48.35));
#85336=CARTESIAN_POINT('Ctrl Pts',(40.845634162426,1.36248314380646,48.5));
#85337=CARTESIAN_POINT('Ctrl Pts',(40.845634162426,1.36248314380646,48.35));
#85338=CARTESIAN_POINT('',(41.2455658316612,1.49229192733765,48.5));
#85339=CARTESIAN_POINT('Ctrl Pts',(41.2455658316612,1.49229192733765,48.5));
#85340=CARTESIAN_POINT('Ctrl Pts',(41.0872439742088,1.36248314380646,48.5));
#85341=CARTESIAN_POINT('Ctrl Pts',(40.845634162426,1.36248314380646,48.5));
#85342=CARTESIAN_POINT('',(41.2455658316612,1.49229192733765,48.35));
#85343=CARTESIAN_POINT('',(41.2455658316612,1.49229192733765,48.5));
#85344=CARTESIAN_POINT('Ctrl Pts',(41.2455658316612,1.49229192733765,48.35));
#85345=CARTESIAN_POINT('Ctrl Pts',(41.0872439742088,1.36248314380646,48.35));
#85346=CARTESIAN_POINT('Ctrl Pts',(40.845634162426,1.36248314380646,48.35));
#85347=CARTESIAN_POINT('Ctrl Pts',(41.4834241271019,1.85995900630951,48.5));
#85348=CARTESIAN_POINT('Ctrl Pts',(41.4834241271019,1.85995900630951,48.35));
#85349=CARTESIAN_POINT('Ctrl Pts',(41.4038876891136,1.62210100889206,48.5));
#85350=CARTESIAN_POINT('Ctrl Pts',(41.4038876891136,1.62210100889206,48.35));
#85351=CARTESIAN_POINT('Ctrl Pts',(41.2455658316612,1.49229192733765,48.5));
#85352=CARTESIAN_POINT('Ctrl Pts',(41.2455658316612,1.49229192733765,48.35));
#85353=CARTESIAN_POINT('',(41.4834241271019,1.85995900630951,48.5));
#85354=CARTESIAN_POINT('Ctrl Pts',(41.4834241271019,1.85995900630951,48.5));
#85355=CARTESIAN_POINT('Ctrl Pts',(41.4038876891136,1.62210100889206,48.5));
#85356=CARTESIAN_POINT('Ctrl Pts',(41.2455658316612,1.49229192733765,48.5));
#85357=CARTESIAN_POINT('',(41.4834241271019,1.85995900630951,48.35));
#85358=CARTESIAN_POINT('',(41.4834241271019,1.85995900630951,48.5));
#85359=CARTESIAN_POINT('Ctrl Pts',(41.4834241271019,1.85995900630951,48.35));
#85360=CARTESIAN_POINT('Ctrl Pts',(41.4038876891136,1.62210100889206,48.35));
#85361=CARTESIAN_POINT('Ctrl Pts',(41.2455658316612,1.49229192733765,48.35));
#85362=CARTESIAN_POINT('Ctrl Pts',(41.5629599690437,2.48499327898026,48.5));
#85363=CARTESIAN_POINT('Ctrl Pts',(41.5629599690437,2.48499327898026,48.35));
#85364=CARTESIAN_POINT('Ctrl Pts',(41.5629599690437,2.09781730175018,48.5));
#85365=CARTESIAN_POINT('Ctrl Pts',(41.5629599690437,2.09781730175018,48.35));
#85366=CARTESIAN_POINT('Ctrl Pts',(41.4834241271019,1.85995900630951,48.5));
#85367=CARTESIAN_POINT('Ctrl Pts',(41.4834241271019,1.85995900630951,48.35));
#85368=CARTESIAN_POINT('',(41.5629599690437,2.48499327898026,48.5));
#85369=CARTESIAN_POINT('Ctrl Pts',(41.5629599690437,2.48499327898026,48.5));
#85370=CARTESIAN_POINT('Ctrl Pts',(41.5629599690437,2.09781730175018,48.5));
#85371=CARTESIAN_POINT('Ctrl Pts',(41.4834241271019,1.85995900630951,48.5));
#85372=CARTESIAN_POINT('',(41.5629599690437,2.48499327898026,48.35));
#85373=CARTESIAN_POINT('',(41.5629599690437,2.48499327898026,48.5));
#85374=CARTESIAN_POINT('Ctrl Pts',(41.5629599690437,2.48499327898026,48.35));
#85375=CARTESIAN_POINT('Ctrl Pts',(41.5629599690437,2.09781730175018,48.35));
#85376=CARTESIAN_POINT('Ctrl Pts',(41.4834241271019,1.85995900630951,48.35));
#85377=CARTESIAN_POINT('Ctrl Pts',(41.5134374499321,3.00497958064079,48.5));
#85378=CARTESIAN_POINT('Ctrl Pts',(41.5134374499321,3.00497958064079,48.35));
#85379=CARTESIAN_POINT('Ctrl Pts',(41.5629599690437,2.81214186549187,48.5));
#85380=CARTESIAN_POINT('Ctrl Pts',(41.5629599690437,2.81214186549187,48.35));
#85381=CARTESIAN_POINT('Ctrl Pts',(41.5629599690437,2.48499327898026,48.5));
#85382=CARTESIAN_POINT('Ctrl Pts',(41.5629599690437,2.48499327898026,48.35));
#85383=CARTESIAN_POINT('',(41.5134374499321,3.00497958064079,48.5));
#85384=CARTESIAN_POINT('Ctrl Pts',(41.5134374499321,3.00497958064079,48.5));
#85385=CARTESIAN_POINT('Ctrl Pts',(41.5629599690437,2.81214186549187,48.5));
#85386=CARTESIAN_POINT('Ctrl Pts',(41.5629599690437,2.48499327898026,48.5));
#85387=CARTESIAN_POINT('',(41.5134374499321,3.00497958064079,48.35));
#85388=CARTESIAN_POINT('',(41.5134374499321,3.00497958064079,48.5));
#85389=CARTESIAN_POINT('Ctrl Pts',(41.5134374499321,3.00497958064079,48.35));
#85390=CARTESIAN_POINT('Ctrl Pts',(41.5629599690437,2.81214186549187,48.35));
#85391=CARTESIAN_POINT('Ctrl Pts',(41.5629599690437,2.48499327898026,48.35));
#85392=CARTESIAN_POINT('Ctrl Pts',(41.3768754601479,3.33212831616402,48.5));
#85393=CARTESIAN_POINT('Ctrl Pts',(41.3768754601479,3.33212831616402,48.35));
#85394=CARTESIAN_POINT('Ctrl Pts',(41.4639149308205,3.19781729578972,48.5));
#85395=CARTESIAN_POINT('Ctrl Pts',(41.4639149308205,3.19781729578972,48.35));
#85396=CARTESIAN_POINT('Ctrl Pts',(41.5134374499321,3.00497958064079,48.5));
#85397=CARTESIAN_POINT('Ctrl Pts',(41.5134374499321,3.00497958064079,48.35));
#85398=CARTESIAN_POINT('',(41.3768754601479,3.33212831616402,48.5));
#85399=CARTESIAN_POINT('Ctrl Pts',(41.3768754601479,3.33212831616402,48.5));
#85400=CARTESIAN_POINT('Ctrl Pts',(41.4639149308205,3.19781729578972,48.5));
#85401=CARTESIAN_POINT('Ctrl Pts',(41.5134374499321,3.00497958064079,48.5));
#85402=CARTESIAN_POINT('',(41.3768754601479,3.33212831616402,48.35));
#85403=CARTESIAN_POINT('',(41.3768754601479,3.33212831616402,48.5));
#85404=CARTESIAN_POINT('Ctrl Pts',(41.3768754601479,3.33212831616402,48.35));
#85405=CARTESIAN_POINT('Ctrl Pts',(41.4639149308205,3.19781729578972,48.35));
#85406=CARTESIAN_POINT('Ctrl Pts',(41.5134374499321,3.00497958064079,48.35));
#85407=CARTESIAN_POINT('Ctrl Pts',(41.1562756896019,3.5377217233181,48.5));
#85408=CARTESIAN_POINT('Ctrl Pts',(41.1562756896019,3.5377217233181,48.35));
#85409=CARTESIAN_POINT('Ctrl Pts',(41.2898359894753,3.46643933653831,48.5));
#85410=CARTESIAN_POINT('Ctrl Pts',(41.2898359894753,3.46643933653831,48.35));
#85411=CARTESIAN_POINT('Ctrl Pts',(41.3768754601479,3.33212831616402,48.5));
#85412=CARTESIAN_POINT('Ctrl Pts',(41.3768754601479,3.33212831616402,48.35));
#85413=CARTESIAN_POINT('',(41.1562756896019,3.5377217233181,48.5));
#85414=CARTESIAN_POINT('Ctrl Pts',(41.1562756896019,3.5377217233181,48.5));
#85415=CARTESIAN_POINT('Ctrl Pts',(41.2898359894753,3.46643933653831,48.5));
#85416=CARTESIAN_POINT('Ctrl Pts',(41.3768754601479,3.33212831616402,48.5));
#85417=CARTESIAN_POINT('',(41.1562756896019,3.5377217233181,48.35));
#85418=CARTESIAN_POINT('',(41.1562756896019,3.5377217233181,48.5));
#85419=CARTESIAN_POINT('Ctrl Pts',(41.1562756896019,3.5377217233181,48.35));
#85420=CARTESIAN_POINT('Ctrl Pts',(41.2898359894753,3.46643933653831,48.35));
#85421=CARTESIAN_POINT('Ctrl Pts',(41.3768754601479,3.33212831616402,48.35));
#85422=CARTESIAN_POINT('Ctrl Pts',(40.845634162426,3.60900411009789,48.5));
#85423=CARTESIAN_POINT('Ctrl Pts',(40.845634162426,3.60900411009789,48.35));
#85424=CARTESIAN_POINT('Ctrl Pts',(41.0227147936821,3.60900411009789,48.5));
#85425=CARTESIAN_POINT('Ctrl Pts',(41.0227147936821,3.60900411009789,48.35));
#85426=CARTESIAN_POINT('Ctrl Pts',(41.1562756896019,3.5377217233181,48.5));
#85427=CARTESIAN_POINT('Ctrl Pts',(41.1562756896019,3.5377217233181,48.35));
#85428=CARTESIAN_POINT('',(40.845634162426,3.60900411009789,48.5));
#85429=CARTESIAN_POINT('Ctrl Pts',(40.845634162426,3.60900411009789,48.5));
#85430=CARTESIAN_POINT('Ctrl Pts',(41.0227147936821,3.60900411009789,48.5));
#85431=CARTESIAN_POINT('Ctrl Pts',(41.1562756896019,3.5377217233181,48.5));
#85432=CARTESIAN_POINT('',(40.845634162426,3.60900411009789,48.35));
#85433=CARTESIAN_POINT('',(40.845634162426,3.60900411009789,48.5));
#85434=CARTESIAN_POINT('Ctrl Pts',(40.845634162426,3.60900411009789,48.35));
#85435=CARTESIAN_POINT('Ctrl Pts',(41.0227147936821,3.60900411009789,48.35));
#85436=CARTESIAN_POINT('Ctrl Pts',(41.1562756896019,3.5377217233181,48.35));
#85437=CARTESIAN_POINT('Ctrl Pts',(40.4472033381462,3.47994545102119,48.5));
#85438=CARTESIAN_POINT('Ctrl Pts',(40.4472033381462,3.47994545102119,48.35));
#85439=CARTESIAN_POINT('Ctrl Pts',(40.6055251955986,3.60900411009789,48.5));
#85440=CARTESIAN_POINT('Ctrl Pts',(40.6055251955986,3.60900411009789,48.35));
#85441=CARTESIAN_POINT('Ctrl Pts',(40.845634162426,3.60900411009789,48.5));
#85442=CARTESIAN_POINT('Ctrl Pts',(40.845634162426,3.60900411009789,48.35));
#85443=CARTESIAN_POINT('',(40.4472033381462,3.47994545102119,48.5));
#85444=CARTESIAN_POINT('Ctrl Pts',(40.4472033381462,3.47994545102119,48.5));
#85445=CARTESIAN_POINT('Ctrl Pts',(40.6055251955986,3.60900411009789,48.5));
#85446=CARTESIAN_POINT('Ctrl Pts',(40.845634162426,3.60900411009789,48.5));
#85447=CARTESIAN_POINT('',(40.4472033381462,3.47994545102119,48.35));
#85448=CARTESIAN_POINT('',(40.4472033381462,3.47994545102119,48.5));
#85449=CARTESIAN_POINT('Ctrl Pts',(40.4472033381462,3.47994545102119,48.35));
#85450=CARTESIAN_POINT('Ctrl Pts',(40.6055251955986,3.60900411009789,48.35));
#85451=CARTESIAN_POINT('Ctrl Pts',(40.845634162426,3.60900411009789,48.35));
#85452=CARTESIAN_POINT('Ctrl Pts',(40.2085946202278,3.11302864551544,48.5));
#85453=CARTESIAN_POINT('Ctrl Pts',(40.2085946202278,3.11302864551544,48.35));
#85454=CARTESIAN_POINT('Ctrl Pts',(40.2888811826706,3.3508867919445,48.5));
#85455=CARTESIAN_POINT('Ctrl Pts',(40.2888811826706,3.3508867919445,48.35));
#85456=CARTESIAN_POINT('Ctrl Pts',(40.4472033381462,3.47994545102119,48.5));
#85457=CARTESIAN_POINT('Ctrl Pts',(40.4472033381462,3.47994545102119,48.35));
#85458=CARTESIAN_POINT('',(40.2085946202278,3.11302864551544,48.5));
#85459=CARTESIAN_POINT('Ctrl Pts',(40.2085946202278,3.11302864551544,48.5));
#85460=CARTESIAN_POINT('Ctrl Pts',(40.2888811826706,3.3508867919445,48.5));
#85461=CARTESIAN_POINT('Ctrl Pts',(40.4472033381462,3.47994545102119,48.5));
#85462=CARTESIAN_POINT('',(40.2085946202278,3.11302864551544,48.35));
#85463=CARTESIAN_POINT('',(40.2085946202278,3.11302864551544,48.5));
#85464=CARTESIAN_POINT('Ctrl Pts',(40.2085946202278,3.11302864551544,48.35));
#85465=CARTESIAN_POINT('Ctrl Pts',(40.2888811826706,3.3508867919445,48.35));
#85466=CARTESIAN_POINT('Ctrl Pts',(40.4472033381462,3.47994545102119,48.35));
#85467=CARTESIAN_POINT('Ctrl Pts',(40.1283083558083,2.48499327898026,48.5));
#85468=CARTESIAN_POINT('Ctrl Pts',(40.1283083558083,2.48499327898026,48.35));
#85469=CARTESIAN_POINT('Ctrl Pts',(40.1283083558083,2.87517049908638,48.5));
#85470=CARTESIAN_POINT('Ctrl Pts',(40.1283083558083,2.87517049908638,48.35));
#85471=CARTESIAN_POINT('Ctrl Pts',(40.2085946202278,3.11302864551544,48.5));
#85472=CARTESIAN_POINT('Ctrl Pts',(40.2085946202278,3.11302864551544,48.35));
#85473=CARTESIAN_POINT('',(40.1283083558083,2.48499327898026,48.5));
#85474=CARTESIAN_POINT('Ctrl Pts',(40.1283083558083,2.48499327898026,48.5));
#85475=CARTESIAN_POINT('Ctrl Pts',(40.1283083558083,2.87517049908638,48.5));
#85476=CARTESIAN_POINT('Ctrl Pts',(40.2085946202278,3.11302864551544,48.5));
#85477=CARTESIAN_POINT('',(40.1283083558083,2.48499327898026,48.35));
#85478=CARTESIAN_POINT('',(40.1283083558083,2.48499327898026,48.5));
#85479=CARTESIAN_POINT('Ctrl Pts',(40.1283083558083,2.48499327898026,48.35));
#85480=CARTESIAN_POINT('Ctrl Pts',(40.1283083558083,2.87517049908638,48.35));
#85481=CARTESIAN_POINT('Ctrl Pts',(40.2085946202278,3.11302864551544,48.35));
#85482=CARTESIAN_POINT('Ctrl Pts',(40.3459070324898,1.59058684110642,48.5));
#85483=CARTESIAN_POINT('Ctrl Pts',(40.3459070324898,1.59058684110642,48.35));
#85484=CARTESIAN_POINT('Ctrl Pts',(40.1283083558083,1.86521166563034,48.5));
#85485=CARTESIAN_POINT('Ctrl Pts',(40.1283083558083,1.86521166563034,48.35));
#85486=CARTESIAN_POINT('Ctrl Pts',(40.1283083558083,2.48499327898026,48.5));
#85487=CARTESIAN_POINT('Ctrl Pts',(40.1283083558083,2.48499327898026,48.35));
#85488=CARTESIAN_POINT('Ctrl Pts',(40.3459070324898,1.59058684110642,48.5));
#85489=CARTESIAN_POINT('Ctrl Pts',(40.1283083558083,1.86521166563034,48.5));
#85490=CARTESIAN_POINT('Ctrl Pts',(40.1283083558083,2.48499327898026,48.5));
#85491=CARTESIAN_POINT('Ctrl Pts',(40.3459070324898,1.59058684110642,48.35));
#85492=CARTESIAN_POINT('Ctrl Pts',(40.1283083558083,1.86521166563034,48.35));
#85493=CARTESIAN_POINT('Ctrl Pts',(40.1283083558083,2.48499327898026,48.35));
#85494=CARTESIAN_POINT('Origin',(39.9999997466803,2.48574362695217,48.35));
#85495=CARTESIAN_POINT('Ctrl Pts',(39.1266029775143,2.7363575398922,48.5));
#85496=CARTESIAN_POINT('Ctrl Pts',(39.1266029775143,2.7363575398922,48.35));
#85497=CARTESIAN_POINT('Ctrl Pts',(39.3089358210564,3.07776266336441,48.5));
#85498=CARTESIAN_POINT('Ctrl Pts',(39.3089358210564,3.07776266336441,48.35));
#85499=CARTESIAN_POINT('Ctrl Pts',(39.5145292282104,3.3118691444397,48.5));
#85500=CARTESIAN_POINT('Ctrl Pts',(39.5145292282104,3.3118691444397,48.35));
#85501=CARTESIAN_POINT('',(39.1266029775143,2.7363575398922,48.5));
#85502=CARTESIAN_POINT('',(39.5145292282104,3.3118691444397,48.5));
#85503=CARTESIAN_POINT('Ctrl Pts',(39.1266029775143,2.7363575398922,48.5));
#85504=CARTESIAN_POINT('Ctrl Pts',(39.3089358210564,3.07776266336441,48.5));
#85505=CARTESIAN_POINT('Ctrl Pts',(39.5145292282104,3.3118691444397,48.5));
#85506=CARTESIAN_POINT('',(39.1266029775143,2.7363575398922,48.35));
#85507=CARTESIAN_POINT('',(39.1266029775143,2.7363575398922,48.5));
#85508=CARTESIAN_POINT('',(39.5145292282104,3.3118691444397,48.35));
#85509=CARTESIAN_POINT('Ctrl Pts',(39.1266029775143,2.7363575398922,48.35));
#85510=CARTESIAN_POINT('Ctrl Pts',(39.3089358210564,3.07776266336441,48.35));
#85511=CARTESIAN_POINT('Ctrl Pts',(39.5145292282104,3.3118691444397,48.35));
#85512=CARTESIAN_POINT('',(39.5145292282104,3.3118691444397,48.5));
#85513=CARTESIAN_POINT('Ctrl Pts',(38.8467257916927,2.02728533744812,48.5));
#85514=CARTESIAN_POINT('Ctrl Pts',(38.8467257916927,2.02728533744812,48.35));
#85515=CARTESIAN_POINT('Ctrl Pts',(38.9442701339722,2.39495241641998,48.5));
#85516=CARTESIAN_POINT('Ctrl Pts',(38.9442701339722,2.39495241641998,48.35));
#85517=CARTESIAN_POINT('Ctrl Pts',(39.1266029775143,2.7363575398922,48.5));
#85518=CARTESIAN_POINT('Ctrl Pts',(39.1266029775143,2.7363575398922,48.35));
#85519=CARTESIAN_POINT('',(38.8467257916927,2.02728533744812,48.5));
#85520=CARTESIAN_POINT('Ctrl Pts',(38.8467257916927,2.02728533744812,48.5));
#85521=CARTESIAN_POINT('Ctrl Pts',(38.9442701339722,2.39495241641998,48.5));
#85522=CARTESIAN_POINT('Ctrl Pts',(39.1266029775143,2.7363575398922,48.5));
#85523=CARTESIAN_POINT('',(38.8467257916927,2.02728533744812,48.35));
#85524=CARTESIAN_POINT('',(38.8467257916927,2.02728533744812,48.5));
#85525=CARTESIAN_POINT('Ctrl Pts',(38.8467257916927,2.02728533744812,48.35));
#85526=CARTESIAN_POINT('Ctrl Pts',(38.9442701339722,2.39495241641998,48.35));
#85527=CARTESIAN_POINT('Ctrl Pts',(39.1266029775143,2.7363575398922,48.35));
#85528=CARTESIAN_POINT('Ctrl Pts',(38.7446793615818,1.40000009536743,48.5));
#85529=CARTESIAN_POINT('Ctrl Pts',(38.7446793615818,1.40000009536743,48.35));
#85530=CARTESIAN_POINT('Ctrl Pts',(38.7491814494133,1.65961825847626,48.5));
#85531=CARTESIAN_POINT('Ctrl Pts',(38.7491814494133,1.65961825847626,48.35));
#85532=CARTESIAN_POINT('Ctrl Pts',(38.8467257916927,2.02728533744812,48.5));
#85533=CARTESIAN_POINT('Ctrl Pts',(38.8467257916927,2.02728533744812,48.35));
#85534=CARTESIAN_POINT('',(38.7446793615818,1.40000009536743,48.5));
#85535=CARTESIAN_POINT('Ctrl Pts',(38.7446793615818,1.40000009536743,48.5));
#85536=CARTESIAN_POINT('Ctrl Pts',(38.7491814494133,1.65961825847626,48.5));
#85537=CARTESIAN_POINT('Ctrl Pts',(38.8467257916927,2.02728533744812,48.5));
#85538=CARTESIAN_POINT('',(38.7446793615818,1.40000009536743,48.35));
#85539=CARTESIAN_POINT('',(38.7446793615818,1.40000009536743,48.5));
#85540=CARTESIAN_POINT('Ctrl Pts',(38.7446793615818,1.40000009536743,48.35));
#85541=CARTESIAN_POINT('Ctrl Pts',(38.7491814494133,1.65961825847626,48.35));
#85542=CARTESIAN_POINT('Ctrl Pts',(38.8467257916927,2.02728533744812,48.35));
#85543=CARTESIAN_POINT('Origin',(39.0223055779934,1.40000009536743,48.5));
#85544=CARTESIAN_POINT('',(39.0223055779934,1.40000009536743,48.5));
#85545=CARTESIAN_POINT('',(19.5111527889967,1.40000009536743,48.5));
#85546=CARTESIAN_POINT('',(39.0223055779934,1.40000009536743,48.35));
#85547=CARTESIAN_POINT('',(39.0223055779934,1.40000009536743,48.5));
#85548=CARTESIAN_POINT('',(39.0223055779934,1.40000009536743,48.35));
#85549=CARTESIAN_POINT('Ctrl Pts',(39.1258527040482,2.00477504730225,48.5));
#85550=CARTESIAN_POINT('Ctrl Pts',(39.1258527040482,2.00477504730225,48.35));
#85551=CARTESIAN_POINT('Ctrl Pts',(39.0448157191277,1.72864937782288,48.5));
#85552=CARTESIAN_POINT('Ctrl Pts',(39.0448157191277,1.72864937782288,48.35));
#85553=CARTESIAN_POINT('Ctrl Pts',(39.0223055779934,1.40000009536743,48.5));
#85554=CARTESIAN_POINT('Ctrl Pts',(39.0223055779934,1.40000009536743,48.35));
#85555=CARTESIAN_POINT('',(39.1258527040482,2.00477504730225,48.5));
#85556=CARTESIAN_POINT('Ctrl Pts',(39.1258527040482,2.00477504730225,48.5));
#85557=CARTESIAN_POINT('Ctrl Pts',(39.0448157191277,1.72864937782288,48.5));
#85558=CARTESIAN_POINT('Ctrl Pts',(39.0223055779934,1.40000009536743,48.5));
#85559=CARTESIAN_POINT('',(39.1258527040482,2.00477504730225,48.35));
#85560=CARTESIAN_POINT('',(39.1258527040482,2.00477504730225,48.5));
#85561=CARTESIAN_POINT('Ctrl Pts',(39.1258527040482,2.00477504730225,48.35));
#85562=CARTESIAN_POINT('Ctrl Pts',(39.0448157191277,1.72864937782288,48.35));
#85563=CARTESIAN_POINT('Ctrl Pts',(39.0223055779934,1.40000009536743,48.35));
#85564=CARTESIAN_POINT('Ctrl Pts',(39.4447473883629,2.76712143421173,48.5));
#85565=CARTESIAN_POINT('Ctrl Pts',(39.4447473883629,2.76712143421173,48.35));
#85566=CARTESIAN_POINT('Ctrl Pts',(39.2384038567543,2.3964529633522,48.5));
#85567=CARTESIAN_POINT('Ctrl Pts',(39.2384038567543,2.3964529633522,48.35));
#85568=CARTESIAN_POINT('Ctrl Pts',(39.1258527040482,2.00477504730225,48.5));
#85569=CARTESIAN_POINT('Ctrl Pts',(39.1258527040482,2.00477504730225,48.35));
#85570=CARTESIAN_POINT('',(39.4447473883629,2.76712143421173,48.5));
#85571=CARTESIAN_POINT('Ctrl Pts',(39.4447473883629,2.76712143421173,48.5));
#85572=CARTESIAN_POINT('Ctrl Pts',(39.2384038567543,2.3964529633522,48.5));
#85573=CARTESIAN_POINT('Ctrl Pts',(39.1258527040482,2.00477504730225,48.5));
#85574=CARTESIAN_POINT('',(39.4447473883629,2.76712143421173,48.35));
#85575=CARTESIAN_POINT('',(39.4447473883629,2.76712143421173,48.5));
#85576=CARTESIAN_POINT('Ctrl Pts',(39.4447473883629,2.76712143421173,48.35));
#85577=CARTESIAN_POINT('Ctrl Pts',(39.2384038567543,2.3964529633522,48.35));
#85578=CARTESIAN_POINT('Ctrl Pts',(39.1258527040482,2.00477504730225,48.35));
#85579=CARTESIAN_POINT('Ctrl Pts',(39.8611868619919,3.36139166355133,48.5));
#85580=CARTESIAN_POINT('Ctrl Pts',(39.8611868619919,3.36139166355133,48.35));
#85581=CARTESIAN_POINT('Ctrl Pts',(39.6510915160179,3.13779005408287,48.5));
#85582=CARTESIAN_POINT('Ctrl Pts',(39.6510915160179,3.13779005408287,48.35));
#85583=CARTESIAN_POINT('Ctrl Pts',(39.4447473883629,2.76712143421173,48.5));
#85584=CARTESIAN_POINT('Ctrl Pts',(39.4447473883629,2.76712143421173,48.35));
#85585=CARTESIAN_POINT('',(39.8611868619919,3.36139166355133,48.5));
#85586=CARTESIAN_POINT('Ctrl Pts',(39.8611868619919,3.36139166355133,48.5));
#85587=CARTESIAN_POINT('Ctrl Pts',(39.6510915160179,3.13779005408287,48.5));
#85588=CARTESIAN_POINT('Ctrl Pts',(39.4447473883629,2.76712143421173,48.5));
#85589=CARTESIAN_POINT('',(39.8611868619919,3.36139166355133,48.35));
#85590=CARTESIAN_POINT('',(39.8611868619919,3.36139166355133,48.5));
#85591=CARTESIAN_POINT('Ctrl Pts',(39.8611868619919,3.36139166355133,48.35));
#85592=CARTESIAN_POINT('Ctrl Pts',(39.6510915160179,3.13779005408287,48.35));
#85593=CARTESIAN_POINT('Ctrl Pts',(39.4447473883629,2.76712143421173,48.35));
#85594=CARTESIAN_POINT('Origin',(39.8611868619919,3.57148715853691,48.5));
#85595=CARTESIAN_POINT('',(39.8611868619919,3.57148715853691,48.5));
#85596=CARTESIAN_POINT('',(39.8611868619919,5.78574357926846,48.5));
#85597=CARTESIAN_POINT('',(39.8611868619919,3.57148715853691,48.35));
#85598=CARTESIAN_POINT('',(39.8611868619919,3.57148715853691,48.5));
#85599=CARTESIAN_POINT('',(39.8611868619919,3.57148715853691,48.35));
#85600=CARTESIAN_POINT('Origin',(38.4370395243168,3.57148715853691,48.5));
#85601=CARTESIAN_POINT('',(38.4370395243168,3.57148715853691,48.5));
#85602=CARTESIAN_POINT('',(19.2185197621584,3.57148715853691,48.5));
#85603=CARTESIAN_POINT('',(38.4370395243168,3.57148715853691,48.35));
#85604=CARTESIAN_POINT('',(38.4370395243168,3.57148715853691,48.5));
#85605=CARTESIAN_POINT('',(38.4370395243168,3.57148715853691,48.35));
#85606=CARTESIAN_POINT('Origin',(38.4370395243168,3.3118691444397,48.5));
#85607=CARTESIAN_POINT('',(38.4370395243168,3.3118691444397,48.5));
#85608=CARTESIAN_POINT('',(38.4370395243168,5.65593457221985,48.5));
#85609=CARTESIAN_POINT('',(38.4370395243168,3.3118691444397,48.35));
#85610=CARTESIAN_POINT('',(38.4370395243168,3.3118691444397,48.5));
#85611=CARTESIAN_POINT('',(38.4370395243168,3.3118691444397,48.35));
#85612=CARTESIAN_POINT('Origin',(39.5145292282104,3.3118691444397,48.5));
#85613=CARTESIAN_POINT('',(19.7572646141052,3.3118691444397,48.5));
#85614=CARTESIAN_POINT('',(39.5145292282104,3.3118691444397,48.35));
#85615=CARTESIAN_POINT('Origin',(39.9999997466803,2.48574362695217,48.35));
#85616=CARTESIAN_POINT('Origin',(0.,8.,48.5));
#85617=CARTESIAN_POINT('Ctrl Pts',(30.8531378936023,3.38540250062943,48.5));
#85618=CARTESIAN_POINT('Ctrl Pts',(30.8531378936023,3.38540250062943,48.35));
#85619=CARTESIAN_POINT('Ctrl Pts',(30.6670530866832,3.38540250062943,48.5));
#85620=CARTESIAN_POINT('Ctrl Pts',(30.6670530866832,3.38540250062943,48.35));
#85621=CARTESIAN_POINT('Ctrl Pts',(30.5560027789325,3.22783091664314,48.5));
#85622=CARTESIAN_POINT('Ctrl Pts',(30.5560027789325,3.22783091664314,48.35));
#85623=CARTESIAN_POINT('',(30.8531378936023,3.38540250062943,48.5));
#85624=CARTESIAN_POINT('',(30.5560027789325,3.22783091664314,48.5));
#85625=CARTESIAN_POINT('Ctrl Pts',(30.8531378936023,3.38540250062943,48.5));
#85626=CARTESIAN_POINT('Ctrl Pts',(30.6670530866832,3.38540250062943,48.5));
#85627=CARTESIAN_POINT('Ctrl Pts',(30.5560027789325,3.22783091664314,48.5));
#85628=CARTESIAN_POINT('',(30.8531378936023,3.38540250062943,48.35));
#85629=CARTESIAN_POINT('',(30.8531378936023,3.38540250062943,48.5));
#85630=CARTESIAN_POINT('',(30.5560027789325,3.22783091664314,48.35));
#85631=CARTESIAN_POINT('Ctrl Pts',(30.8531378936023,3.38540250062943,48.35));
#85632=CARTESIAN_POINT('Ctrl Pts',(30.6670530866832,3.38540250062943,48.35));
#85633=CARTESIAN_POINT('Ctrl Pts',(30.5560027789325,3.22783091664314,48.35));
#85634=CARTESIAN_POINT('',(30.5560027789325,3.22783091664314,48.5));
#85635=CARTESIAN_POINT('Ctrl Pts',(31.1690311860293,3.2068213224411,48.5));
#85636=CARTESIAN_POINT('Ctrl Pts',(31.1690311860293,3.2068213224411,48.35));
#85637=CARTESIAN_POINT('Ctrl Pts',(31.0422234963626,3.38540250062943,48.5));
#85638=CARTESIAN_POINT('Ctrl Pts',(31.0422234963626,3.38540250062943,48.35));
#85639=CARTESIAN_POINT('Ctrl Pts',(30.8531378936023,3.38540250062943,48.5));
#85640=CARTESIAN_POINT('Ctrl Pts',(30.8531378936023,3.38540250062943,48.35));
#85641=CARTESIAN_POINT('',(31.1690311860293,3.2068213224411,48.5));
#85642=CARTESIAN_POINT('Ctrl Pts',(31.1690311860293,3.2068213224411,48.5));
#85643=CARTESIAN_POINT('Ctrl Pts',(31.0422234963626,3.38540250062943,48.5));
#85644=CARTESIAN_POINT('Ctrl Pts',(30.8531378936023,3.38540250062943,48.5));
#85645=CARTESIAN_POINT('',(31.1690311860293,3.2068213224411,48.35));
#85646=CARTESIAN_POINT('',(31.1690311860293,3.2068213224411,48.5));
#85647=CARTESIAN_POINT('Ctrl Pts',(31.1690311860293,3.2068213224411,48.35));
#85648=CARTESIAN_POINT('Ctrl Pts',(31.0422234963626,3.38540250062943,48.35));
#85649=CARTESIAN_POINT('Ctrl Pts',(30.8531378936023,3.38540250062943,48.35));
#85650=CARTESIAN_POINT('Ctrl Pts',(31.2958388756961,2.48499327898026,48.5));
#85651=CARTESIAN_POINT('Ctrl Pts',(31.2958388756961,2.48499327898026,48.35));
#85652=CARTESIAN_POINT('Ctrl Pts',(31.2958388756961,3.02824014425278,48.5));
#85653=CARTESIAN_POINT('Ctrl Pts',(31.2958388756961,3.02824014425278,48.35));
#85654=CARTESIAN_POINT('Ctrl Pts',(31.1690311860293,3.2068213224411,48.5));
#85655=CARTESIAN_POINT('Ctrl Pts',(31.1690311860293,3.2068213224411,48.35));
#85656=CARTESIAN_POINT('',(31.2958388756961,2.48499327898026,48.5));
#85657=CARTESIAN_POINT('Ctrl Pts',(31.2958388756961,2.48499327898026,48.5));
#85658=CARTESIAN_POINT('Ctrl Pts',(31.2958388756961,3.02824014425278,48.5));
#85659=CARTESIAN_POINT('Ctrl Pts',(31.1690311860293,3.2068213224411,48.5));
#85660=CARTESIAN_POINT('',(31.2958388756961,2.48499327898026,48.35));
#85661=CARTESIAN_POINT('',(31.2958388756961,2.48499327898026,48.5));
#85662=CARTESIAN_POINT('Ctrl Pts',(31.2958388756961,2.48499327898026,48.35));
#85663=CARTESIAN_POINT('Ctrl Pts',(31.2958388756961,3.02824014425278,48.35));
#85664=CARTESIAN_POINT('Ctrl Pts',(31.1690311860293,3.2068213224411,48.35));
#85665=CARTESIAN_POINT('Ctrl Pts',(31.1690311860293,1.76466578245163,48.5));
#85666=CARTESIAN_POINT('Ctrl Pts',(31.1690311860293,1.76466578245163,48.35));
#85667=CARTESIAN_POINT('Ctrl Pts',(31.2958388756961,1.9447478055954,48.5));
#85668=CARTESIAN_POINT('Ctrl Pts',(31.2958388756961,1.9447478055954,48.35));
#85669=CARTESIAN_POINT('Ctrl Pts',(31.2958388756961,2.48499327898026,48.5));
#85670=CARTESIAN_POINT('Ctrl Pts',(31.2958388756961,2.48499327898026,48.35));
#85671=CARTESIAN_POINT('',(31.1690311860293,1.76466578245163,48.5));
#85672=CARTESIAN_POINT('Ctrl Pts',(31.1690311860293,1.76466578245163,48.5));
#85673=CARTESIAN_POINT('Ctrl Pts',(31.2958388756961,1.9447478055954,48.5));
#85674=CARTESIAN_POINT('Ctrl Pts',(31.2958388756961,2.48499327898026,48.5));
#85675=CARTESIAN_POINT('',(31.1690311860293,1.76466578245163,48.35));
#85676=CARTESIAN_POINT('',(31.1690311860293,1.76466578245163,48.5));
#85677=CARTESIAN_POINT('Ctrl Pts',(31.1690311860293,1.76466578245163,48.35));
#85678=CARTESIAN_POINT('Ctrl Pts',(31.2958388756961,1.9447478055954,48.35));
#85679=CARTESIAN_POINT('Ctrl Pts',(31.2958388756961,2.48499327898026,48.35));
#85680=CARTESIAN_POINT('Ctrl Pts',(30.8561389874667,1.58458405733109,48.5));
#85681=CARTESIAN_POINT('Ctrl Pts',(30.8561389874667,1.58458405733109,48.35));
#85682=CARTESIAN_POINT('Ctrl Pts',(31.0422234963626,1.58458405733109,48.5));
#85683=CARTESIAN_POINT('Ctrl Pts',(31.0422234963626,1.58458405733109,48.35));
#85684=CARTESIAN_POINT('Ctrl Pts',(31.1690311860293,1.76466578245163,48.5));
#85685=CARTESIAN_POINT('Ctrl Pts',(31.1690311860293,1.76466578245163,48.35));
#85686=CARTESIAN_POINT('',(30.8561389874667,1.58458405733109,48.5));
#85687=CARTESIAN_POINT('Ctrl Pts',(30.8561389874667,1.58458405733109,48.5));
#85688=CARTESIAN_POINT('Ctrl Pts',(31.0422234963626,1.58458405733109,48.5));
#85689=CARTESIAN_POINT('Ctrl Pts',(31.1690311860293,1.76466578245163,48.5));
#85690=CARTESIAN_POINT('',(30.8561389874667,1.58458405733109,48.35));
#85691=CARTESIAN_POINT('',(30.8561389874667,1.58458405733109,48.5));
#85692=CARTESIAN_POINT('Ctrl Pts',(30.8561389874667,1.58458405733109,48.35));
#85693=CARTESIAN_POINT('Ctrl Pts',(31.0422234963626,1.58458405733109,48.35));
#85694=CARTESIAN_POINT('Ctrl Pts',(31.1690311860293,1.76466578245163,48.35));
#85695=CARTESIAN_POINT('Ctrl Pts',(30.5432467889041,1.76391565799713,48.5));
#85696=CARTESIAN_POINT('Ctrl Pts',(30.5432467889041,1.76391565799713,48.35));
#85697=CARTESIAN_POINT('Ctrl Pts',(30.6700544785708,1.58458405733109,48.5));
#85698=CARTESIAN_POINT('Ctrl Pts',(30.6700544785708,1.58458405733109,48.35));
#85699=CARTESIAN_POINT('Ctrl Pts',(30.8561389874667,1.58458405733109,48.5));
#85700=CARTESIAN_POINT('Ctrl Pts',(30.8561389874667,1.58458405733109,48.35));
#85701=CARTESIAN_POINT('',(30.5432467889041,1.76391565799713,48.5));
#85702=CARTESIAN_POINT('Ctrl Pts',(30.5432467889041,1.76391565799713,48.5));
#85703=CARTESIAN_POINT('Ctrl Pts',(30.6700544785708,1.58458405733109,48.5));
#85704=CARTESIAN_POINT('Ctrl Pts',(30.8561389874667,1.58458405733109,48.5));
#85705=CARTESIAN_POINT('',(30.5432467889041,1.76391565799713,48.35));
#85706=CARTESIAN_POINT('',(30.5432467889041,1.76391565799713,48.5));
#85707=CARTESIAN_POINT('Ctrl Pts',(30.5432467889041,1.76391565799713,48.35));
#85708=CARTESIAN_POINT('Ctrl Pts',(30.6700544785708,1.58458405733109,48.35));
#85709=CARTESIAN_POINT('Ctrl Pts',(30.8561389874667,1.58458405733109,48.35));
#85710=CARTESIAN_POINT('Ctrl Pts',(30.4164390992373,2.48499327898026,48.5));
#85711=CARTESIAN_POINT('Ctrl Pts',(30.4164390992373,2.48499327898026,48.35));
#85712=CARTESIAN_POINT('Ctrl Pts',(30.4164390992373,1.94324696063995,48.5));
#85713=CARTESIAN_POINT('Ctrl Pts',(30.4164390992373,1.94324696063995,48.35));
#85714=CARTESIAN_POINT('Ctrl Pts',(30.5432467889041,1.76391565799713,48.5));
#85715=CARTESIAN_POINT('Ctrl Pts',(30.5432467889041,1.76391565799713,48.35));
#85716=CARTESIAN_POINT('',(30.4164390992373,2.48499327898026,48.5));
#85717=CARTESIAN_POINT('Ctrl Pts',(30.4164390992373,2.48499327898026,48.5));
#85718=CARTESIAN_POINT('Ctrl Pts',(30.4164390992373,1.94324696063995,48.5));
#85719=CARTESIAN_POINT('Ctrl Pts',(30.5432467889041,1.76391565799713,48.5));
#85720=CARTESIAN_POINT('',(30.4164390992373,2.48499327898026,48.35));
#85721=CARTESIAN_POINT('',(30.4164390992373,2.48499327898026,48.5));
#85722=CARTESIAN_POINT('Ctrl Pts',(30.4164390992373,2.48499327898026,48.35));
#85723=CARTESIAN_POINT('Ctrl Pts',(30.4164390992373,1.94324696063995,48.35));
#85724=CARTESIAN_POINT('Ctrl Pts',(30.5432467889041,1.76391565799713,48.35));
#85725=CARTESIAN_POINT('Ctrl Pts',(30.5560027789325,3.22783091664314,48.5));
#85726=CARTESIAN_POINT('Ctrl Pts',(30.5560027789325,3.22783091664314,48.35));
#85727=CARTESIAN_POINT('Ctrl Pts',(30.4164390992373,3.02673944830894,48.5));
#85728=CARTESIAN_POINT('Ctrl Pts',(30.4164390992373,3.02673944830894,48.35));
#85729=CARTESIAN_POINT('Ctrl Pts',(30.4164390992373,2.48499327898026,48.5));
#85730=CARTESIAN_POINT('Ctrl Pts',(30.4164390992373,2.48499327898026,48.35));
#85731=CARTESIAN_POINT('Ctrl Pts',(30.5560027789325,3.22783091664314,48.5));
#85732=CARTESIAN_POINT('Ctrl Pts',(30.4164390992373,3.02673944830894,48.5));
#85733=CARTESIAN_POINT('Ctrl Pts',(30.4164390992373,2.48499327898026,48.5));
#85734=CARTESIAN_POINT('Ctrl Pts',(30.5560027789325,3.22783091664314,48.35));
#85735=CARTESIAN_POINT('Ctrl Pts',(30.4164390992373,3.02673944830894,48.35));
#85736=CARTESIAN_POINT('Ctrl Pts',(30.4164390992373,2.48499327898026,48.35));
#85737=CARTESIAN_POINT('Ctrl Pts',(30.8561389874667,1.36248314380646,48.5));
#85738=CARTESIAN_POINT('Ctrl Pts',(30.8561389874667,1.36248314380646,48.35));
#85739=CARTESIAN_POINT('Ctrl Pts',(30.5379944276065,1.36248314380646,48.5));
#85740=CARTESIAN_POINT('Ctrl Pts',(30.5379944276065,1.36248314380646,48.35));
#85741=CARTESIAN_POINT('Ctrl Pts',(30.3564118575305,1.59058684110642,48.5));
#85742=CARTESIAN_POINT('Ctrl Pts',(30.3564118575305,1.59058684110642,48.35));
#85743=CARTESIAN_POINT('',(30.8561389874667,1.36248314380646,48.5));
#85744=CARTESIAN_POINT('',(30.3564118575305,1.59058684110642,48.5));
#85745=CARTESIAN_POINT('Ctrl Pts',(30.8561389874667,1.36248314380646,48.5));
#85746=CARTESIAN_POINT('Ctrl Pts',(30.5379944276065,1.36248314380646,48.5));
#85747=CARTESIAN_POINT('Ctrl Pts',(30.3564118575305,1.59058684110642,48.5));
#85748=CARTESIAN_POINT('',(30.8561389874667,1.36248314380646,48.35));
#85749=CARTESIAN_POINT('',(30.8561389874667,1.36248314380646,48.5));
#85750=CARTESIAN_POINT('',(30.3564118575305,1.59058684110642,48.35));
#85751=CARTESIAN_POINT('Ctrl Pts',(30.8561389874667,1.36248314380646,48.35));
#85752=CARTESIAN_POINT('Ctrl Pts',(30.5379944276065,1.36248314380646,48.35));
#85753=CARTESIAN_POINT('Ctrl Pts',(30.3564118575305,1.59058684110642,48.35));
#85754=CARTESIAN_POINT('',(30.3564118575305,1.59058684110642,48.5));
#85755=CARTESIAN_POINT('Ctrl Pts',(31.2560706567019,1.49229192733765,48.5));
#85756=CARTESIAN_POINT('Ctrl Pts',(31.2560706567019,1.49229192733765,48.35));
#85757=CARTESIAN_POINT('Ctrl Pts',(31.0977487992495,1.36248314380646,48.5));
#85758=CARTESIAN_POINT('Ctrl Pts',(31.0977487992495,1.36248314380646,48.35));
#85759=CARTESIAN_POINT('Ctrl Pts',(30.8561389874667,1.36248314380646,48.5));
#85760=CARTESIAN_POINT('Ctrl Pts',(30.8561389874667,1.36248314380646,48.35));
#85761=CARTESIAN_POINT('',(31.2560706567019,1.49229192733765,48.5));
#85762=CARTESIAN_POINT('Ctrl Pts',(31.2560706567019,1.49229192733765,48.5));
#85763=CARTESIAN_POINT('Ctrl Pts',(31.0977487992495,1.36248314380646,48.5));
#85764=CARTESIAN_POINT('Ctrl Pts',(30.8561389874667,1.36248314380646,48.5));
#85765=CARTESIAN_POINT('',(31.2560706567019,1.49229192733765,48.35));
#85766=CARTESIAN_POINT('',(31.2560706567019,1.49229192733765,48.5));
#85767=CARTESIAN_POINT('Ctrl Pts',(31.2560706567019,1.49229192733765,48.35));
#85768=CARTESIAN_POINT('Ctrl Pts',(31.0977487992495,1.36248314380646,48.35));
#85769=CARTESIAN_POINT('Ctrl Pts',(30.8561389874667,1.36248314380646,48.35));
#85770=CARTESIAN_POINT('Ctrl Pts',(31.4939289521426,1.85995900630951,48.5));
#85771=CARTESIAN_POINT('Ctrl Pts',(31.4939289521426,1.85995900630951,48.35));
#85772=CARTESIAN_POINT('Ctrl Pts',(31.4143925141543,1.62210100889206,48.5));
#85773=CARTESIAN_POINT('Ctrl Pts',(31.4143925141543,1.62210100889206,48.35));
#85774=CARTESIAN_POINT('Ctrl Pts',(31.2560706567019,1.49229192733765,48.5));
#85775=CARTESIAN_POINT('Ctrl Pts',(31.2560706567019,1.49229192733765,48.35));
#85776=CARTESIAN_POINT('',(31.4939289521426,1.85995900630951,48.5));
#85777=CARTESIAN_POINT('Ctrl Pts',(31.4939289521426,1.85995900630951,48.5));
#85778=CARTESIAN_POINT('Ctrl Pts',(31.4143925141543,1.62210100889206,48.5));
#85779=CARTESIAN_POINT('Ctrl Pts',(31.2560706567019,1.49229192733765,48.5));
#85780=CARTESIAN_POINT('',(31.4939289521426,1.85995900630951,48.35));
#85781=CARTESIAN_POINT('',(31.4939289521426,1.85995900630951,48.5));
#85782=CARTESIAN_POINT('Ctrl Pts',(31.4939289521426,1.85995900630951,48.35));
#85783=CARTESIAN_POINT('Ctrl Pts',(31.4143925141543,1.62210100889206,48.35));
#85784=CARTESIAN_POINT('Ctrl Pts',(31.2560706567019,1.49229192733765,48.35));
#85785=CARTESIAN_POINT('Ctrl Pts',(31.5734647940844,2.48499327898026,48.5));
#85786=CARTESIAN_POINT('Ctrl Pts',(31.5734647940844,2.48499327898026,48.35));
#85787=CARTESIAN_POINT('Ctrl Pts',(31.5734647940844,2.09781730175018,48.5));
#85788=CARTESIAN_POINT('Ctrl Pts',(31.5734647940844,2.09781730175018,48.35));
#85789=CARTESIAN_POINT('Ctrl Pts',(31.4939289521426,1.85995900630951,48.5));
#85790=CARTESIAN_POINT('Ctrl Pts',(31.4939289521426,1.85995900630951,48.35));
#85791=CARTESIAN_POINT('',(31.5734647940844,2.48499327898026,48.5));
#85792=CARTESIAN_POINT('Ctrl Pts',(31.5734647940844,2.48499327898026,48.5));
#85793=CARTESIAN_POINT('Ctrl Pts',(31.5734647940844,2.09781730175018,48.5));
#85794=CARTESIAN_POINT('Ctrl Pts',(31.4939289521426,1.85995900630951,48.5));
#85795=CARTESIAN_POINT('',(31.5734647940844,2.48499327898026,48.35));
#85796=CARTESIAN_POINT('',(31.5734647940844,2.48499327898026,48.5));
#85797=CARTESIAN_POINT('Ctrl Pts',(31.5734647940844,2.48499327898026,48.35));
#85798=CARTESIAN_POINT('Ctrl Pts',(31.5734647940844,2.09781730175018,48.35));
#85799=CARTESIAN_POINT('Ctrl Pts',(31.4939289521426,1.85995900630951,48.35));
#85800=CARTESIAN_POINT('Ctrl Pts',(31.5239422749728,3.00497958064079,48.5));
#85801=CARTESIAN_POINT('Ctrl Pts',(31.5239422749728,3.00497958064079,48.35));
#85802=CARTESIAN_POINT('Ctrl Pts',(31.5734647940844,2.81214186549187,48.5));
#85803=CARTESIAN_POINT('Ctrl Pts',(31.5734647940844,2.81214186549187,48.35));
#85804=CARTESIAN_POINT('Ctrl Pts',(31.5734647940844,2.48499327898026,48.5));
#85805=CARTESIAN_POINT('Ctrl Pts',(31.5734647940844,2.48499327898026,48.35));
#85806=CARTESIAN_POINT('',(31.5239422749728,3.00497958064079,48.5));
#85807=CARTESIAN_POINT('Ctrl Pts',(31.5239422749728,3.00497958064079,48.5));
#85808=CARTESIAN_POINT('Ctrl Pts',(31.5734647940844,2.81214186549187,48.5));
#85809=CARTESIAN_POINT('Ctrl Pts',(31.5734647940844,2.48499327898026,48.5));
#85810=CARTESIAN_POINT('',(31.5239422749728,3.00497958064079,48.35));
#85811=CARTESIAN_POINT('',(31.5239422749728,3.00497958064079,48.5));
#85812=CARTESIAN_POINT('Ctrl Pts',(31.5239422749728,3.00497958064079,48.35));
#85813=CARTESIAN_POINT('Ctrl Pts',(31.5734647940844,2.81214186549187,48.35));
#85814=CARTESIAN_POINT('Ctrl Pts',(31.5734647940844,2.48499327898026,48.35));
#85815=CARTESIAN_POINT('Ctrl Pts',(31.3873802851886,3.33212831616402,48.5));
#85816=CARTESIAN_POINT('Ctrl Pts',(31.3873802851886,3.33212831616402,48.35));
#85817=CARTESIAN_POINT('Ctrl Pts',(31.4744197558612,3.19781729578972,48.5));
#85818=CARTESIAN_POINT('Ctrl Pts',(31.4744197558612,3.19781729578972,48.35));
#85819=CARTESIAN_POINT('Ctrl Pts',(31.5239422749728,3.00497958064079,48.5));
#85820=CARTESIAN_POINT('Ctrl Pts',(31.5239422749728,3.00497958064079,48.35));
#85821=CARTESIAN_POINT('',(31.3873802851886,3.33212831616402,48.5));
#85822=CARTESIAN_POINT('Ctrl Pts',(31.3873802851886,3.33212831616402,48.5));
#85823=CARTESIAN_POINT('Ctrl Pts',(31.4744197558612,3.19781729578972,48.5));
#85824=CARTESIAN_POINT('Ctrl Pts',(31.5239422749728,3.00497958064079,48.5));
#85825=CARTESIAN_POINT('',(31.3873802851886,3.33212831616402,48.35));
#85826=CARTESIAN_POINT('',(31.3873802851886,3.33212831616402,48.5));
#85827=CARTESIAN_POINT('Ctrl Pts',(31.3873802851886,3.33212831616402,48.35));
#85828=CARTESIAN_POINT('Ctrl Pts',(31.4744197558612,3.19781729578972,48.35));
#85829=CARTESIAN_POINT('Ctrl Pts',(31.5239422749728,3.00497958064079,48.35));
#85830=CARTESIAN_POINT('Ctrl Pts',(31.1667805146426,3.5377217233181,48.5));
#85831=CARTESIAN_POINT('Ctrl Pts',(31.1667805146426,3.5377217233181,48.35));
#85832=CARTESIAN_POINT('Ctrl Pts',(31.3003408145159,3.46643933653831,48.5));
#85833=CARTESIAN_POINT('Ctrl Pts',(31.3003408145159,3.46643933653831,48.35));
#85834=CARTESIAN_POINT('Ctrl Pts',(31.3873802851886,3.33212831616402,48.5));
#85835=CARTESIAN_POINT('Ctrl Pts',(31.3873802851886,3.33212831616402,48.35));
#85836=CARTESIAN_POINT('',(31.1667805146426,3.5377217233181,48.5));
#85837=CARTESIAN_POINT('Ctrl Pts',(31.1667805146426,3.5377217233181,48.5));
#85838=CARTESIAN_POINT('Ctrl Pts',(31.3003408145159,3.46643933653831,48.5));
#85839=CARTESIAN_POINT('Ctrl Pts',(31.3873802851886,3.33212831616402,48.5));
#85840=CARTESIAN_POINT('',(31.1667805146426,3.5377217233181,48.35));
#85841=CARTESIAN_POINT('',(31.1667805146426,3.5377217233181,48.5));
#85842=CARTESIAN_POINT('Ctrl Pts',(31.1667805146426,3.5377217233181,48.35));
#85843=CARTESIAN_POINT('Ctrl Pts',(31.3003408145159,3.46643933653831,48.35));
#85844=CARTESIAN_POINT('Ctrl Pts',(31.3873802851886,3.33212831616402,48.35));
#85845=CARTESIAN_POINT('Ctrl Pts',(30.8561389874667,3.60900411009789,48.5));
#85846=CARTESIAN_POINT('Ctrl Pts',(30.8561389874667,3.60900411009789,48.35));
#85847=CARTESIAN_POINT('Ctrl Pts',(31.0332196187228,3.60900411009789,48.5));
#85848=CARTESIAN_POINT('Ctrl Pts',(31.0332196187228,3.60900411009789,48.35));
#85849=CARTESIAN_POINT('Ctrl Pts',(31.1667805146426,3.5377217233181,48.5));
#85850=CARTESIAN_POINT('Ctrl Pts',(31.1667805146426,3.5377217233181,48.35));
#85851=CARTESIAN_POINT('',(30.8561389874667,3.60900411009789,48.5));
#85852=CARTESIAN_POINT('Ctrl Pts',(30.8561389874667,3.60900411009789,48.5));
#85853=CARTESIAN_POINT('Ctrl Pts',(31.0332196187228,3.60900411009789,48.5));
#85854=CARTESIAN_POINT('Ctrl Pts',(31.1667805146426,3.5377217233181,48.5));
#85855=CARTESIAN_POINT('',(30.8561389874667,3.60900411009789,48.35));
#85856=CARTESIAN_POINT('',(30.8561389874667,3.60900411009789,48.5));
#85857=CARTESIAN_POINT('Ctrl Pts',(30.8561389874667,3.60900411009789,48.35));
#85858=CARTESIAN_POINT('Ctrl Pts',(31.0332196187228,3.60900411009789,48.35));
#85859=CARTESIAN_POINT('Ctrl Pts',(31.1667805146426,3.5377217233181,48.35));
#85860=CARTESIAN_POINT('Ctrl Pts',(30.4577081631869,3.47994545102119,48.5));
#85861=CARTESIAN_POINT('Ctrl Pts',(30.4577081631869,3.47994545102119,48.35));
#85862=CARTESIAN_POINT('Ctrl Pts',(30.6160300206393,3.60900411009789,48.5));
#85863=CARTESIAN_POINT('Ctrl Pts',(30.6160300206393,3.60900411009789,48.35));
#85864=CARTESIAN_POINT('Ctrl Pts',(30.8561389874667,3.60900411009789,48.5));
#85865=CARTESIAN_POINT('Ctrl Pts',(30.8561389874667,3.60900411009789,48.35));
#85866=CARTESIAN_POINT('',(30.4577081631869,3.47994545102119,48.5));
#85867=CARTESIAN_POINT('Ctrl Pts',(30.4577081631869,3.47994545102119,48.5));
#85868=CARTESIAN_POINT('Ctrl Pts',(30.6160300206393,3.60900411009789,48.5));
#85869=CARTESIAN_POINT('Ctrl Pts',(30.8561389874667,3.60900411009789,48.5));
#85870=CARTESIAN_POINT('',(30.4577081631869,3.47994545102119,48.35));
#85871=CARTESIAN_POINT('',(30.4577081631869,3.47994545102119,48.5));
#85872=CARTESIAN_POINT('Ctrl Pts',(30.4577081631869,3.47994545102119,48.35));
#85873=CARTESIAN_POINT('Ctrl Pts',(30.6160300206393,3.60900411009789,48.35));
#85874=CARTESIAN_POINT('Ctrl Pts',(30.8561389874667,3.60900411009789,48.35));
#85875=CARTESIAN_POINT('Ctrl Pts',(30.2190994452685,3.11302864551544,48.5));
#85876=CARTESIAN_POINT('Ctrl Pts',(30.2190994452685,3.11302864551544,48.35));
#85877=CARTESIAN_POINT('Ctrl Pts',(30.2993860077113,3.3508867919445,48.5));
#85878=CARTESIAN_POINT('Ctrl Pts',(30.2993860077113,3.3508867919445,48.35));
#85879=CARTESIAN_POINT('Ctrl Pts',(30.4577081631869,3.47994545102119,48.5));
#85880=CARTESIAN_POINT('Ctrl Pts',(30.4577081631869,3.47994545102119,48.35));
#85881=CARTESIAN_POINT('',(30.2190994452685,3.11302864551544,48.5));
#85882=CARTESIAN_POINT('Ctrl Pts',(30.2190994452685,3.11302864551544,48.5));
#85883=CARTESIAN_POINT('Ctrl Pts',(30.2993860077113,3.3508867919445,48.5));
#85884=CARTESIAN_POINT('Ctrl Pts',(30.4577081631869,3.47994545102119,48.5));
#85885=CARTESIAN_POINT('',(30.2190994452685,3.11302864551544,48.35));
#85886=CARTESIAN_POINT('',(30.2190994452685,3.11302864551544,48.5));
#85887=CARTESIAN_POINT('Ctrl Pts',(30.2190994452685,3.11302864551544,48.35));
#85888=CARTESIAN_POINT('Ctrl Pts',(30.2993860077113,3.3508867919445,48.35));
#85889=CARTESIAN_POINT('Ctrl Pts',(30.4577081631869,3.47994545102119,48.35));
#85890=CARTESIAN_POINT('Ctrl Pts',(30.138813180849,2.48499327898026,48.5));
#85891=CARTESIAN_POINT('Ctrl Pts',(30.138813180849,2.48499327898026,48.35));
#85892=CARTESIAN_POINT('Ctrl Pts',(30.138813180849,2.87517049908638,48.5));
#85893=CARTESIAN_POINT('Ctrl Pts',(30.138813180849,2.87517049908638,48.35));
#85894=CARTESIAN_POINT('Ctrl Pts',(30.2190994452685,3.11302864551544,48.5));
#85895=CARTESIAN_POINT('Ctrl Pts',(30.2190994452685,3.11302864551544,48.35));
#85896=CARTESIAN_POINT('',(30.138813180849,2.48499327898026,48.5));
#85897=CARTESIAN_POINT('Ctrl Pts',(30.138813180849,2.48499327898026,48.5));
#85898=CARTESIAN_POINT('Ctrl Pts',(30.138813180849,2.87517049908638,48.5));
#85899=CARTESIAN_POINT('Ctrl Pts',(30.2190994452685,3.11302864551544,48.5));
#85900=CARTESIAN_POINT('',(30.138813180849,2.48499327898026,48.35));
#85901=CARTESIAN_POINT('',(30.138813180849,2.48499327898026,48.5));
#85902=CARTESIAN_POINT('Ctrl Pts',(30.138813180849,2.48499327898026,48.35));
#85903=CARTESIAN_POINT('Ctrl Pts',(30.138813180849,2.87517049908638,48.35));
#85904=CARTESIAN_POINT('Ctrl Pts',(30.2190994452685,3.11302864551544,48.35));
#85905=CARTESIAN_POINT('Ctrl Pts',(30.3564118575305,1.59058684110642,48.5));
#85906=CARTESIAN_POINT('Ctrl Pts',(30.3564118575305,1.59058684110642,48.35));
#85907=CARTESIAN_POINT('Ctrl Pts',(30.138813180849,1.86521166563034,48.5));
#85908=CARTESIAN_POINT('Ctrl Pts',(30.138813180849,1.86521166563034,48.35));
#85909=CARTESIAN_POINT('Ctrl Pts',(30.138813180849,2.48499327898026,48.5));
#85910=CARTESIAN_POINT('Ctrl Pts',(30.138813180849,2.48499327898026,48.35));
#85911=CARTESIAN_POINT('Ctrl Pts',(30.3564118575305,1.59058684110642,48.5));
#85912=CARTESIAN_POINT('Ctrl Pts',(30.138813180849,1.86521166563034,48.5));
#85913=CARTESIAN_POINT('Ctrl Pts',(30.138813180849,2.48499327898026,48.5));
#85914=CARTESIAN_POINT('Ctrl Pts',(30.3564118575305,1.59058684110642,48.35));
#85915=CARTESIAN_POINT('Ctrl Pts',(30.138813180849,1.86521166563034,48.35));
#85916=CARTESIAN_POINT('Ctrl Pts',(30.138813180849,2.48499327898026,48.35));
#85917=CARTESIAN_POINT('Origin',(29.9999997746199,2.48574362695217,48.35));
#85918=CARTESIAN_POINT('Ctrl Pts',(29.1498636435717,3.38690319657326,48.5));
#85919=CARTESIAN_POINT('Ctrl Pts',(29.1498636435717,3.38690319657326,48.35));
#85920=CARTESIAN_POINT('Ctrl Pts',(28.9952933024615,3.38690319657326,48.5));
#85921=CARTESIAN_POINT('Ctrl Pts',(28.9952933024615,3.38690319657326,48.35));
#85922=CARTESIAN_POINT('Ctrl Pts',(28.8932468723506,3.28785815834999,48.5));
#85923=CARTESIAN_POINT('Ctrl Pts',(28.8932468723506,3.28785815834999,48.35));
#85924=CARTESIAN_POINT('',(29.1498636435717,3.38690319657326,48.5));
#85925=CARTESIAN_POINT('',(28.8932468723506,3.28785815834999,48.5));
#85926=CARTESIAN_POINT('Ctrl Pts',(29.1498636435717,3.38690319657326,48.5));
#85927=CARTESIAN_POINT('Ctrl Pts',(28.9952933024615,3.38690319657326,48.5));
#85928=CARTESIAN_POINT('Ctrl Pts',(28.8932468723506,3.28785815834999,48.5));
#85929=CARTESIAN_POINT('',(29.1498636435717,3.38690319657326,48.35));
#85930=CARTESIAN_POINT('',(29.1498636435717,3.38690319657326,48.5));
#85931=CARTESIAN_POINT('',(28.8932468723506,3.28785815834999,48.35));
#85932=CARTESIAN_POINT('Ctrl Pts',(29.1498636435717,3.38690319657326,48.35));
#85933=CARTESIAN_POINT('Ctrl Pts',(28.9952933024615,3.38690319657326,48.35));
#85934=CARTESIAN_POINT('Ctrl Pts',(28.8932468723506,3.28785815834999,48.35));
#85935=CARTESIAN_POINT('',(28.8932468723506,3.28785815834999,48.5));
#85936=CARTESIAN_POINT('Ctrl Pts',(29.4057299923152,3.28560718894005,48.5));
#85937=CARTESIAN_POINT('Ctrl Pts',(29.4057299923152,3.28560718894005,48.35));
#85938=CARTESIAN_POINT('Ctrl Pts',(29.3029331397265,3.38690319657326,48.5));
#85939=CARTESIAN_POINT('Ctrl Pts',(29.3029331397265,3.38690319657326,48.35));
#85940=CARTESIAN_POINT('Ctrl Pts',(29.1498636435717,3.38690319657326,48.5));
#85941=CARTESIAN_POINT('Ctrl Pts',(29.1498636435717,3.38690319657326,48.35));
#85942=CARTESIAN_POINT('',(29.4057299923152,3.28560718894005,48.5));
#85943=CARTESIAN_POINT('Ctrl Pts',(29.4057299923152,3.28560718894005,48.5));
#85944=CARTESIAN_POINT('Ctrl Pts',(29.3029331397265,3.38690319657326,48.5));
#85945=CARTESIAN_POINT('Ctrl Pts',(29.1498636435717,3.38690319657326,48.5));
#85946=CARTESIAN_POINT('',(29.4057299923152,3.28560718894005,48.35));
#85947=CARTESIAN_POINT('',(29.4057299923152,3.28560718894005,48.5));
#85948=CARTESIAN_POINT('Ctrl Pts',(29.4057299923152,3.28560718894005,48.35));
#85949=CARTESIAN_POINT('Ctrl Pts',(29.3029331397265,3.38690319657326,48.35));
#85950=CARTESIAN_POINT('Ctrl Pts',(29.1498636435717,3.38690319657326,48.35));
#85951=CARTESIAN_POINT('Ctrl Pts',(29.5085265468806,3.03574362397194,48.5));
#85952=CARTESIAN_POINT('Ctrl Pts',(29.5085265468806,3.03574362397194,48.35));
#85953=CARTESIAN_POINT('Ctrl Pts',(29.5085265468806,3.18431103229523,48.5));
#85954=CARTESIAN_POINT('Ctrl Pts',(29.5085265468806,3.18431103229523,48.35));
#85955=CARTESIAN_POINT('Ctrl Pts',(29.4057299923152,3.28560718894005,48.5));
#85956=CARTESIAN_POINT('Ctrl Pts',(29.4057299923152,3.28560718894005,48.35));
#85957=CARTESIAN_POINT('',(29.5085265468806,3.03574362397194,48.5));
#85958=CARTESIAN_POINT('Ctrl Pts',(29.5085265468806,3.03574362397194,48.5));
#85959=CARTESIAN_POINT('Ctrl Pts',(29.5085265468806,3.18431103229523,48.5));
#85960=CARTESIAN_POINT('Ctrl Pts',(29.4057299923152,3.28560718894005,48.5));
#85961=CARTESIAN_POINT('',(29.5085265468806,3.03574362397194,48.35));
#85962=CARTESIAN_POINT('',(29.5085265468806,3.03574362397194,48.5));
#85963=CARTESIAN_POINT('Ctrl Pts',(29.5085265468806,3.03574362397194,48.35));
#85964=CARTESIAN_POINT('Ctrl Pts',(29.5085265468806,3.18431103229523,48.35));
#85965=CARTESIAN_POINT('Ctrl Pts',(29.4057299923152,3.28560718894005,48.35));
#85966=CARTESIAN_POINT('Ctrl Pts',(29.4087313842028,2.79488408565521,48.5));
#85967=CARTESIAN_POINT('Ctrl Pts',(29.4087313842028,2.79488408565521,48.35));
#85968=CARTESIAN_POINT('Ctrl Pts',(29.5085265468806,2.89317870140076,48.5));
#85969=CARTESIAN_POINT('Ctrl Pts',(29.5085265468806,2.89317870140076,48.35));
#85970=CARTESIAN_POINT('Ctrl Pts',(29.5085265468806,3.03574362397194,48.5));
#85971=CARTESIAN_POINT('Ctrl Pts',(29.5085265468806,3.03574362397194,48.35));
#85972=CARTESIAN_POINT('',(29.4087313842028,2.79488408565521,48.5));
#85973=CARTESIAN_POINT('Ctrl Pts',(29.4087313842028,2.79488408565521,48.5));
#85974=CARTESIAN_POINT('Ctrl Pts',(29.5085265468806,2.89317870140076,48.5));
#85975=CARTESIAN_POINT('Ctrl Pts',(29.5085265468806,3.03574362397194,48.5));
#85976=CARTESIAN_POINT('',(29.4087313842028,2.79488408565521,48.35));
#85977=CARTESIAN_POINT('',(29.4087313842028,2.79488408565521,48.5));
#85978=CARTESIAN_POINT('Ctrl Pts',(29.4087313842028,2.79488408565521,48.35));
#85979=CARTESIAN_POINT('Ctrl Pts',(29.5085265468806,2.89317870140076,48.35));
#85980=CARTESIAN_POINT('Ctrl Pts',(29.5085265468806,3.03574362397194,48.35));
#85981=CARTESIAN_POINT('Ctrl Pts',(29.1528650354594,2.69658946990967,48.5));
#85982=CARTESIAN_POINT('Ctrl Pts',(29.1528650354594,2.69658946990967,48.35));
#85983=CARTESIAN_POINT('Ctrl Pts',(29.3089359235018,2.69658946990967,48.5));
#85984=CARTESIAN_POINT('Ctrl Pts',(29.3089359235018,2.69658946990967,48.35));
#85985=CARTESIAN_POINT('Ctrl Pts',(29.4087313842028,2.79488408565521,48.5));
#85986=CARTESIAN_POINT('Ctrl Pts',(29.4087313842028,2.79488408565521,48.35));
#85987=CARTESIAN_POINT('',(29.1528650354594,2.69658946990967,48.5));
#85988=CARTESIAN_POINT('Ctrl Pts',(29.1528650354594,2.69658946990967,48.5));
#85989=CARTESIAN_POINT('Ctrl Pts',(29.3089359235018,2.69658946990967,48.5));
#85990=CARTESIAN_POINT('Ctrl Pts',(29.4087313842028,2.79488408565521,48.5));
#85991=CARTESIAN_POINT('',(29.1528650354594,2.69658946990967,48.35));
#85992=CARTESIAN_POINT('',(29.1528650354594,2.69658946990967,48.5));
#85993=CARTESIAN_POINT('Ctrl Pts',(29.1528650354594,2.69658946990967,48.35));
#85994=CARTESIAN_POINT('Ctrl Pts',(29.3089359235018,2.69658946990967,48.35));
#85995=CARTESIAN_POINT('Ctrl Pts',(29.4087313842028,2.79488408565521,48.35));
#85996=CARTESIAN_POINT('Ctrl Pts',(28.8917463254184,2.79563435912132,48.5));
#85997=CARTESIAN_POINT('Ctrl Pts',(28.8917463254184,2.79563435912132,48.35));
#85998=CARTESIAN_POINT('Ctrl Pts',(28.9922919105738,2.69658946990967,48.5));
#85999=CARTESIAN_POINT('Ctrl Pts',(28.9922919105738,2.69658946990967,48.35));
#86000=CARTESIAN_POINT('Ctrl Pts',(29.1528650354594,2.69658946990967,48.5));
#86001=CARTESIAN_POINT('Ctrl Pts',(29.1528650354594,2.69658946990967,48.35));
#86002=CARTESIAN_POINT('',(28.8917463254184,2.79563435912132,48.5));
#86003=CARTESIAN_POINT('Ctrl Pts',(28.8917463254184,2.79563435912132,48.5));
#86004=CARTESIAN_POINT('Ctrl Pts',(28.9922919105738,2.69658946990967,48.5));
#86005=CARTESIAN_POINT('Ctrl Pts',(29.1528650354594,2.69658946990967,48.5));
#86006=CARTESIAN_POINT('',(28.8917463254184,2.79563435912132,48.35));
#86007=CARTESIAN_POINT('',(28.8917463254184,2.79563435912132,48.5));
#86008=CARTESIAN_POINT('Ctrl Pts',(28.8917463254184,2.79563435912132,48.35));
#86009=CARTESIAN_POINT('Ctrl Pts',(28.9922919105738,2.69658946990967,48.35));
#86010=CARTESIAN_POINT('Ctrl Pts',(29.1528650354594,2.69658946990967,48.35));
#86011=CARTESIAN_POINT('Ctrl Pts',(28.7912005912513,3.05075043439865,48.5));
#86012=CARTESIAN_POINT('Ctrl Pts',(28.7912005912513,3.05075043439865,48.35));
#86013=CARTESIAN_POINT('Ctrl Pts',(28.7912005912513,2.89467939734459,48.5));
#86014=CARTESIAN_POINT('Ctrl Pts',(28.7912005912513,2.89467939734459,48.35));
#86015=CARTESIAN_POINT('Ctrl Pts',(28.8917463254184,2.79563435912132,48.5));
#86016=CARTESIAN_POINT('Ctrl Pts',(28.8917463254184,2.79563435912132,48.35));
#86017=CARTESIAN_POINT('',(28.7912005912513,3.05075043439865,48.5));
#86018=CARTESIAN_POINT('Ctrl Pts',(28.7912005912513,3.05075043439865,48.5));
#86019=CARTESIAN_POINT('Ctrl Pts',(28.7912005912513,2.89467939734459,48.5));
#86020=CARTESIAN_POINT('Ctrl Pts',(28.8917463254184,2.79563435912132,48.5));
#86021=CARTESIAN_POINT('',(28.7912005912513,3.05075043439865,48.35));
#86022=CARTESIAN_POINT('',(28.7912005912513,3.05075043439865,48.5));
#86023=CARTESIAN_POINT('Ctrl Pts',(28.7912005912513,3.05075043439865,48.35));
#86024=CARTESIAN_POINT('Ctrl Pts',(28.7912005912513,2.89467939734459,48.35));
#86025=CARTESIAN_POINT('Ctrl Pts',(28.8917463254184,2.79563435912132,48.35));
#86026=CARTESIAN_POINT('Ctrl Pts',(28.8932468723506,3.28785815834999,48.5));
#86027=CARTESIAN_POINT('Ctrl Pts',(28.8932468723506,3.28785815834999,48.35));
#86028=CARTESIAN_POINT('Ctrl Pts',(28.7912005912513,3.18881312012672,48.5));
#86029=CARTESIAN_POINT('Ctrl Pts',(28.7912005912513,3.18881312012672,48.35));
#86030=CARTESIAN_POINT('Ctrl Pts',(28.7912005912513,3.05075043439865,48.5));
#86031=CARTESIAN_POINT('Ctrl Pts',(28.7912005912513,3.05075043439865,48.35));
#86032=CARTESIAN_POINT('Ctrl Pts',(28.8932468723506,3.28785815834999,48.5));
#86033=CARTESIAN_POINT('Ctrl Pts',(28.7912005912513,3.18881312012672,48.5));
#86034=CARTESIAN_POINT('Ctrl Pts',(28.7912005912513,3.05075043439865,48.5));
#86035=CARTESIAN_POINT('Ctrl Pts',(28.8932468723506,3.28785815834999,48.35));
#86036=CARTESIAN_POINT('Ctrl Pts',(28.7912005912513,3.18881312012672,48.35));
#86037=CARTESIAN_POINT('Ctrl Pts',(28.7912005912513,3.05075043439865,48.35));
#86038=CARTESIAN_POINT('Ctrl Pts',(29.1453615557402,2.47598910331726,48.5));
#86039=CARTESIAN_POINT('Ctrl Pts',(29.1453615557402,2.47598910331726,48.35));
#86040=CARTESIAN_POINT('Ctrl Pts',(28.9547749590129,2.47598910331726,48.5));
#86041=CARTESIAN_POINT('Ctrl Pts',(28.9547749590129,2.47598910331726,48.35));
#86042=CARTESIAN_POINT('Ctrl Pts',(28.82946796529,2.34993183612823,48.5));
#86043=CARTESIAN_POINT('Ctrl Pts',(28.82946796529,2.34993183612823,48.35));
#86044=CARTESIAN_POINT('',(29.1453615557402,2.47598910331726,48.5));
#86045=CARTESIAN_POINT('',(28.82946796529,2.34993183612823,48.5));
#86046=CARTESIAN_POINT('Ctrl Pts',(29.1453615557402,2.47598910331726,48.5));
#86047=CARTESIAN_POINT('Ctrl Pts',(28.9547749590129,2.47598910331726,48.5));
#86048=CARTESIAN_POINT('Ctrl Pts',(28.82946796529,2.34993183612823,48.5));
#86049=CARTESIAN_POINT('',(29.1453615557402,2.47598910331726,48.35));
#86050=CARTESIAN_POINT('',(29.1453615557402,2.47598910331726,48.5));
#86051=CARTESIAN_POINT('',(28.82946796529,2.34993183612823,48.35));
#86052=CARTESIAN_POINT('Ctrl Pts',(29.1453615557402,2.47598910331726,48.35));
#86053=CARTESIAN_POINT('Ctrl Pts',(28.9547749590129,2.47598910331726,48.35));
#86054=CARTESIAN_POINT('Ctrl Pts',(28.82946796529,2.34993183612823,48.35));
#86055=CARTESIAN_POINT('',(28.82946796529,2.34993183612823,48.5));
#86056=CARTESIAN_POINT('Ctrl Pts',(29.4702591728419,2.34843128919601,48.5));
#86057=CARTESIAN_POINT('Ctrl Pts',(29.4702591728419,2.34843128919601,48.35));
#86058=CARTESIAN_POINT('Ctrl Pts',(29.3404502402991,2.47598910331726,48.5));
#86059=CARTESIAN_POINT('Ctrl Pts',(29.3404502402991,2.47598910331726,48.35));
#86060=CARTESIAN_POINT('Ctrl Pts',(29.1453615557402,2.47598910331726,48.5));
#86061=CARTESIAN_POINT('Ctrl Pts',(29.1453615557402,2.47598910331726,48.35));
#86062=CARTESIAN_POINT('',(29.4702591728419,2.34843128919601,48.5));
#86063=CARTESIAN_POINT('Ctrl Pts',(29.4702591728419,2.34843128919601,48.5));
#86064=CARTESIAN_POINT('Ctrl Pts',(29.3404502402991,2.47598910331726,48.5));
#86065=CARTESIAN_POINT('Ctrl Pts',(29.1453615557402,2.47598910331726,48.5));
#86066=CARTESIAN_POINT('',(29.4702591728419,2.34843128919601,48.35));
#86067=CARTESIAN_POINT('',(29.4702591728419,2.34843128919601,48.5));
#86068=CARTESIAN_POINT('Ctrl Pts',(29.4702591728419,2.34843128919601,48.35));
#86069=CARTESIAN_POINT('Ctrl Pts',(29.3404502402991,2.47598910331726,48.35));
#86070=CARTESIAN_POINT('Ctrl Pts',(29.1453615557402,2.47598910331726,48.35));
#86071=CARTESIAN_POINT('Ctrl Pts',(29.6000682543963,2.02578449249268,48.5));
#86072=CARTESIAN_POINT('Ctrl Pts',(29.6000682543963,2.02578449249268,48.35));
#86073=CARTESIAN_POINT('Ctrl Pts',(29.6000682543963,2.22087317705154,48.5));
#86074=CARTESIAN_POINT('Ctrl Pts',(29.6000682543963,2.22087317705154,48.35));
#86075=CARTESIAN_POINT('Ctrl Pts',(29.4702591728419,2.34843128919601,48.5));
#86076=CARTESIAN_POINT('Ctrl Pts',(29.4702591728419,2.34843128919601,48.35));
#86077=CARTESIAN_POINT('',(29.6000682543963,2.02578449249268,48.5));
#86078=CARTESIAN_POINT('Ctrl Pts',(29.6000682543963,2.02578449249268,48.5));
#86079=CARTESIAN_POINT('Ctrl Pts',(29.6000682543963,2.22087317705154,48.5));
#86080=CARTESIAN_POINT('Ctrl Pts',(29.4702591728419,2.34843128919601,48.5));
#86081=CARTESIAN_POINT('',(29.6000682543963,2.02578449249268,48.35));
#86082=CARTESIAN_POINT('',(29.6000682543963,2.02578449249268,48.5));
#86083=CARTESIAN_POINT('Ctrl Pts',(29.6000682543963,2.02578449249268,48.35));
#86084=CARTESIAN_POINT('Ctrl Pts',(29.6000682543963,2.22087317705154,48.35));
#86085=CARTESIAN_POINT('Ctrl Pts',(29.4702591728419,2.34843128919601,48.35));
#86086=CARTESIAN_POINT('Ctrl Pts',(29.4740109872073,1.70914047956467,48.5));
#86087=CARTESIAN_POINT('Ctrl Pts',(29.4740109872073,1.70914047956467,48.35));
#86088=CARTESIAN_POINT('Ctrl Pts',(29.6000682543963,1.83369719982147,48.5));
#86089=CARTESIAN_POINT('Ctrl Pts',(29.6000682543963,1.83369719982147,48.35));
#86090=CARTESIAN_POINT('Ctrl Pts',(29.6000682543963,2.02578449249268,48.5));
#86091=CARTESIAN_POINT('Ctrl Pts',(29.6000682543963,2.02578449249268,48.35));
#86092=CARTESIAN_POINT('',(29.4740109872073,1.70914047956467,48.5));
#86093=CARTESIAN_POINT('Ctrl Pts',(29.4740109872073,1.70914047956467,48.5));
#86094=CARTESIAN_POINT('Ctrl Pts',(29.6000682543963,1.83369719982147,48.5));
#86095=CARTESIAN_POINT('Ctrl Pts',(29.6000682543963,2.02578449249268,48.5));
#86096=CARTESIAN_POINT('',(29.4740109872073,1.70914047956467,48.35));
#86097=CARTESIAN_POINT('',(29.4740109872073,1.70914047956467,48.5));
#86098=CARTESIAN_POINT('Ctrl Pts',(29.4740109872073,1.70914047956467,48.35));
#86099=CARTESIAN_POINT('Ctrl Pts',(29.6000682543963,1.83369719982147,48.35));
#86100=CARTESIAN_POINT('Ctrl Pts',(29.6000682543963,2.02578449249268,48.35));
#86101=CARTESIAN_POINT('Ctrl Pts',(29.1543655823916,1.58458405733109,48.5));
#86102=CARTESIAN_POINT('Ctrl Pts',(29.1543655823916,1.58458405733109,48.35));
#86103=CARTESIAN_POINT('Ctrl Pts',(29.3479537200183,1.58458405733109,48.5));
#86104=CARTESIAN_POINT('Ctrl Pts',(29.3479537200183,1.58458405733109,48.35));
#86105=CARTESIAN_POINT('Ctrl Pts',(29.4740109872073,1.70914047956467,48.5));
#86106=CARTESIAN_POINT('Ctrl Pts',(29.4740109872073,1.70914047956467,48.35));
#86107=CARTESIAN_POINT('',(29.1543655823916,1.58458405733109,48.5));
#86108=CARTESIAN_POINT('Ctrl Pts',(29.1543655823916,1.58458405733109,48.5));
#86109=CARTESIAN_POINT('Ctrl Pts',(29.3479537200183,1.58458405733109,48.5));
#86110=CARTESIAN_POINT('Ctrl Pts',(29.4740109872073,1.70914047956467,48.5));
#86111=CARTESIAN_POINT('',(29.1543655823916,1.58458405733109,48.35));
#86112=CARTESIAN_POINT('',(29.1543655823916,1.58458405733109,48.5));
#86113=CARTESIAN_POINT('Ctrl Pts',(29.1543655823916,1.58458405733109,48.35));
#86114=CARTESIAN_POINT('Ctrl Pts',(29.3479537200183,1.58458405733109,48.35));
#86115=CARTESIAN_POINT('Ctrl Pts',(29.4740109872073,1.70914047956467,48.35));
#86116=CARTESIAN_POINT('Ctrl Pts',(28.9217599462718,1.64386087656021,48.5));
#86117=CARTESIAN_POINT('Ctrl Pts',(28.9217599462718,1.64386087656021,48.35));
#86118=CARTESIAN_POINT('Ctrl Pts',(29.0298090111464,1.58458405733109,48.5));
#86119=CARTESIAN_POINT('Ctrl Pts',(29.0298090111464,1.58458405733109,48.35));
#86120=CARTESIAN_POINT('Ctrl Pts',(29.1543655823916,1.58458405733109,48.5));
#86121=CARTESIAN_POINT('Ctrl Pts',(29.1543655823916,1.58458405733109,48.35));
#86122=CARTESIAN_POINT('',(28.9217599462718,1.64386087656021,48.5));
#86123=CARTESIAN_POINT('Ctrl Pts',(28.9217599462718,1.64386087656021,48.5));
#86124=CARTESIAN_POINT('Ctrl Pts',(29.0298090111464,1.58458405733109,48.5));
#86125=CARTESIAN_POINT('Ctrl Pts',(29.1543655823916,1.58458405733109,48.5));
#86126=CARTESIAN_POINT('',(28.9217599462718,1.64386087656021,48.35));
#86127=CARTESIAN_POINT('',(28.9217599462718,1.64386087656021,48.5));
#86128=CARTESIAN_POINT('Ctrl Pts',(28.9217599462718,1.64386087656021,48.35));
#86129=CARTESIAN_POINT('Ctrl Pts',(29.0298090111464,1.58458405733109,48.35));
#86130=CARTESIAN_POINT('Ctrl Pts',(29.1543655823916,1.58458405733109,48.35));
#86131=CARTESIAN_POINT('Ctrl Pts',(28.7589358519763,1.8111869096756,48.5));
#86132=CARTESIAN_POINT('Ctrl Pts',(28.7589358519763,1.8111869096756,48.35));
#86133=CARTESIAN_POINT('Ctrl Pts',(28.8137107323855,1.70313799381256,48.5));
#86134=CARTESIAN_POINT('Ctrl Pts',(28.8137107323855,1.70313799381256,48.35));
#86135=CARTESIAN_POINT('Ctrl Pts',(28.9217599462718,1.64386087656021,48.5));
#86136=CARTESIAN_POINT('Ctrl Pts',(28.9217599462718,1.64386087656021,48.35));
#86137=CARTESIAN_POINT('',(28.7589358519763,1.8111869096756,48.5));
#86138=CARTESIAN_POINT('Ctrl Pts',(28.7589358519763,1.8111869096756,48.5));
#86139=CARTESIAN_POINT('Ctrl Pts',(28.8137107323855,1.70313799381256,48.5));
#86140=CARTESIAN_POINT('Ctrl Pts',(28.9217599462718,1.64386087656021,48.5));
#86141=CARTESIAN_POINT('',(28.7589358519763,1.8111869096756,48.35));
#86142=CARTESIAN_POINT('',(28.7589358519763,1.8111869096756,48.5));
#86143=CARTESIAN_POINT('Ctrl Pts',(28.7589358519763,1.8111869096756,48.35));
#86144=CARTESIAN_POINT('Ctrl Pts',(28.8137107323855,1.70313799381256,48.35));
#86145=CARTESIAN_POINT('Ctrl Pts',(28.9217599462718,1.64386087656021,48.35));
#86146=CARTESIAN_POINT('Ctrl Pts',(28.704160971567,2.03478866815567,48.5));
#86147=CARTESIAN_POINT('Ctrl Pts',(28.704160971567,2.03478866815567,48.35));
#86148=CARTESIAN_POINT('Ctrl Pts',(28.704160971567,1.91923612356186,48.5));
#86149=CARTESIAN_POINT('Ctrl Pts',(28.704160971567,1.91923612356186,48.35));
#86150=CARTESIAN_POINT('Ctrl Pts',(28.7589358519763,1.8111869096756,48.5));
#86151=CARTESIAN_POINT('Ctrl Pts',(28.7589358519763,1.8111869096756,48.35));
#86152=CARTESIAN_POINT('',(28.704160971567,2.03478866815567,48.5));
#86153=CARTESIAN_POINT('Ctrl Pts',(28.704160971567,2.03478866815567,48.5));
#86154=CARTESIAN_POINT('Ctrl Pts',(28.704160971567,1.91923612356186,48.5));
#86155=CARTESIAN_POINT('Ctrl Pts',(28.7589358519763,1.8111869096756,48.5));
#86156=CARTESIAN_POINT('',(28.704160971567,2.03478866815567,48.35));
#86157=CARTESIAN_POINT('',(28.704160971567,2.03478866815567,48.5));
#86158=CARTESIAN_POINT('Ctrl Pts',(28.704160971567,2.03478866815567,48.35));
#86159=CARTESIAN_POINT('Ctrl Pts',(28.704160971567,1.91923612356186,48.35));
#86160=CARTESIAN_POINT('Ctrl Pts',(28.7589358519763,1.8111869096756,48.35));
#86161=CARTESIAN_POINT('Ctrl Pts',(28.82946796529,2.34993183612823,48.5));
#86162=CARTESIAN_POINT('Ctrl Pts',(28.82946796529,2.34993183612823,48.35));
#86163=CARTESIAN_POINT('Ctrl Pts',(28.704160971567,2.22387456893921,48.5));
#86164=CARTESIAN_POINT('Ctrl Pts',(28.704160971567,2.22387456893921,48.35));
#86165=CARTESIAN_POINT('Ctrl Pts',(28.704160971567,2.03478866815567,48.5));
#86166=CARTESIAN_POINT('Ctrl Pts',(28.704160971567,2.03478866815567,48.35));
#86167=CARTESIAN_POINT('Ctrl Pts',(28.82946796529,2.34993183612823,48.5));
#86168=CARTESIAN_POINT('Ctrl Pts',(28.704160971567,2.22387456893921,48.5));
#86169=CARTESIAN_POINT('Ctrl Pts',(28.704160971567,2.03478866815567,48.5));
#86170=CARTESIAN_POINT('Ctrl Pts',(28.82946796529,2.34993183612823,48.35));
#86171=CARTESIAN_POINT('Ctrl Pts',(28.704160971567,2.22387456893921,48.35));
#86172=CARTESIAN_POINT('Ctrl Pts',(28.704160971567,2.03478866815567,48.35));
#86173=CARTESIAN_POINT('Ctrl Pts',(28.4265347551554,2.03628921508789,48.5));
#86174=CARTESIAN_POINT('Ctrl Pts',(28.4265347551554,2.03628921508789,48.35));
#86175=CARTESIAN_POINT('Ctrl Pts',(28.4265347551554,2.25088679790497,48.5));
#86176=CARTESIAN_POINT('Ctrl Pts',(28.4265347551554,2.25088679790497,48.35));
#86177=CARTESIAN_POINT('Ctrl Pts',(28.5353342425078,2.39570268988609,48.5));
#86178=CARTESIAN_POINT('Ctrl Pts',(28.5353342425078,2.39570268988609,48.35));
#86179=CARTESIAN_POINT('',(28.4265347551554,2.03628921508789,48.5));
#86180=CARTESIAN_POINT('',(28.5353342425078,2.39570268988609,48.5));
#86181=CARTESIAN_POINT('Ctrl Pts',(28.4265347551554,2.03628921508789,48.5));
#86182=CARTESIAN_POINT('Ctrl Pts',(28.4265347551554,2.25088679790497,48.5));
#86183=CARTESIAN_POINT('Ctrl Pts',(28.5353342425078,2.39570268988609,48.5));
#86184=CARTESIAN_POINT('',(28.4265347551554,2.03628921508789,48.35));
#86185=CARTESIAN_POINT('',(28.4265347551554,2.03628921508789,48.5));
#86186=CARTESIAN_POINT('',(28.5353342425078,2.39570268988609,48.35));
#86187=CARTESIAN_POINT('Ctrl Pts',(28.4265347551554,2.03628921508789,48.35));
#86188=CARTESIAN_POINT('Ctrl Pts',(28.4265347551554,2.25088679790497,48.35));
#86189=CARTESIAN_POINT('Ctrl Pts',(28.5353342425078,2.39570268988609,48.35));
#86190=CARTESIAN_POINT('',(28.5353342425078,2.39570268988609,48.5));
#86191=CARTESIAN_POINT('Ctrl Pts',(28.6261255275458,1.55532056093216,48.5));
#86192=CARTESIAN_POINT('Ctrl Pts',(28.6261255275458,1.55532056093216,48.35));
#86193=CARTESIAN_POINT('Ctrl Pts',(28.4265347551554,1.74815827608109,48.5));
#86194=CARTESIAN_POINT('Ctrl Pts',(28.4265347551554,1.74815827608109,48.35));
#86195=CARTESIAN_POINT('Ctrl Pts',(28.4265347551554,2.03628921508789,48.5));
#86196=CARTESIAN_POINT('Ctrl Pts',(28.4265347551554,2.03628921508789,48.35));
#86197=CARTESIAN_POINT('',(28.6261255275458,1.55532056093216,48.5));
#86198=CARTESIAN_POINT('Ctrl Pts',(28.6261255275458,1.55532056093216,48.5));
#86199=CARTESIAN_POINT('Ctrl Pts',(28.4265347551554,1.74815827608109,48.5));
#86200=CARTESIAN_POINT('Ctrl Pts',(28.4265347551554,2.03628921508789,48.5));
#86201=CARTESIAN_POINT('',(28.6261255275458,1.55532056093216,48.35));
#86202=CARTESIAN_POINT('',(28.6261255275458,1.55532056093216,48.5));
#86203=CARTESIAN_POINT('Ctrl Pts',(28.6261255275458,1.55532056093216,48.35));
#86204=CARTESIAN_POINT('Ctrl Pts',(28.4265347551554,1.74815827608109,48.35));
#86205=CARTESIAN_POINT('Ctrl Pts',(28.4265347551554,2.03628921508789,48.35));
#86206=CARTESIAN_POINT('Ctrl Pts',(29.151364190504,1.36248314380646,48.5));
#86207=CARTESIAN_POINT('Ctrl Pts',(29.151364190504,1.36248314380646,48.35));
#86208=CARTESIAN_POINT('Ctrl Pts',(28.8257162999362,1.36248314380646,48.5));
#86209=CARTESIAN_POINT('Ctrl Pts',(28.8257162999362,1.36248314380646,48.35));
#86210=CARTESIAN_POINT('Ctrl Pts',(28.6261255275458,1.55532056093216,48.5));
#86211=CARTESIAN_POINT('Ctrl Pts',(28.6261255275458,1.55532056093216,48.35));
#86212=CARTESIAN_POINT('',(29.151364190504,1.36248314380646,48.5));
#86213=CARTESIAN_POINT('Ctrl Pts',(29.151364190504,1.36248314380646,48.5));
#86214=CARTESIAN_POINT('Ctrl Pts',(28.8257162999362,1.36248314380646,48.5));
#86215=CARTESIAN_POINT('Ctrl Pts',(28.6261255275458,1.55532056093216,48.5));
#86216=CARTESIAN_POINT('',(29.151364190504,1.36248314380646,48.35));
#86217=CARTESIAN_POINT('',(29.151364190504,1.36248314380646,48.5));
#86218=CARTESIAN_POINT('Ctrl Pts',(29.151364190504,1.36248314380646,48.35));
#86219=CARTESIAN_POINT('Ctrl Pts',(28.8257162999362,1.36248314380646,48.35));
#86220=CARTESIAN_POINT('Ctrl Pts',(28.6261255275458,1.55532056093216,48.35));
#86221=CARTESIAN_POINT('Ctrl Pts',(29.6766030024737,1.55457043647766,48.5));
#86222=CARTESIAN_POINT('Ctrl Pts',(29.6766030024737,1.55457043647766,48.35));
#86223=CARTESIAN_POINT('Ctrl Pts',(29.477012379095,1.36248314380646,48.5));
#86224=CARTESIAN_POINT('Ctrl Pts',(29.477012379095,1.36248314380646,48.35));
#86225=CARTESIAN_POINT('Ctrl Pts',(29.151364190504,1.36248314380646,48.5));
#86226=CARTESIAN_POINT('Ctrl Pts',(29.151364190504,1.36248314380646,48.35));
#86227=CARTESIAN_POINT('',(29.6766030024737,1.55457043647766,48.5));
#86228=CARTESIAN_POINT('Ctrl Pts',(29.6766030024737,1.55457043647766,48.5));
#86229=CARTESIAN_POINT('Ctrl Pts',(29.477012379095,1.36248314380646,48.5));
#86230=CARTESIAN_POINT('Ctrl Pts',(29.151364190504,1.36248314380646,48.5));
#86231=CARTESIAN_POINT('',(29.6766030024737,1.55457043647766,48.35));
#86232=CARTESIAN_POINT('',(29.6766030024737,1.55457043647766,48.5));
#86233=CARTESIAN_POINT('Ctrl Pts',(29.6766030024737,1.55457043647766,48.35));
#86234=CARTESIAN_POINT('Ctrl Pts',(29.477012379095,1.36248314380646,48.35));
#86235=CARTESIAN_POINT('Ctrl Pts',(29.151364190504,1.36248314380646,48.35));
#86236=CARTESIAN_POINT('Ctrl Pts',(29.8761936258525,2.02878588438034,48.5));
#86237=CARTESIAN_POINT('Ctrl Pts',(29.8761936258525,2.02878588438034,48.35));
#86238=CARTESIAN_POINT('Ctrl Pts',(29.8761936258525,1.74665772914886,48.5));
#86239=CARTESIAN_POINT('Ctrl Pts',(29.8761936258525,1.74665772914886,48.35));
#86240=CARTESIAN_POINT('Ctrl Pts',(29.6766030024737,1.55457043647766,48.5));
#86241=CARTESIAN_POINT('Ctrl Pts',(29.6766030024737,1.55457043647766,48.35));
#86242=CARTESIAN_POINT('',(29.8761936258525,2.02878588438034,48.5));
#86243=CARTESIAN_POINT('Ctrl Pts',(29.8761936258525,2.02878588438034,48.5));
#86244=CARTESIAN_POINT('Ctrl Pts',(29.8761936258525,1.74665772914886,48.5));
#86245=CARTESIAN_POINT('Ctrl Pts',(29.6766030024737,1.55457043647766,48.5));
#86246=CARTESIAN_POINT('',(29.8761936258525,2.02878588438034,48.35));
#86247=CARTESIAN_POINT('',(29.8761936258525,2.02878588438034,48.5));
#86248=CARTESIAN_POINT('Ctrl Pts',(29.8761936258525,2.02878588438034,48.35));
#86249=CARTESIAN_POINT('Ctrl Pts',(29.8761936258525,1.74665772914886,48.35));
#86250=CARTESIAN_POINT('Ctrl Pts',(29.6766030024737,1.55457043647766,48.35));
#86251=CARTESIAN_POINT('Ctrl Pts',(29.7703956793994,2.37994545698166,48.5));
#86252=CARTESIAN_POINT('Ctrl Pts',(29.7703956793994,2.37994545698166,48.35));
#86253=CARTESIAN_POINT('Ctrl Pts',(29.8761936258525,2.2328787446022,48.5));
#86254=CARTESIAN_POINT('Ctrl Pts',(29.8761936258525,2.2328787446022,48.35));
#86255=CARTESIAN_POINT('Ctrl Pts',(29.8761936258525,2.02878588438034,48.5));
#86256=CARTESIAN_POINT('Ctrl Pts',(29.8761936258525,2.02878588438034,48.35));
#86257=CARTESIAN_POINT('',(29.7703956793994,2.37994545698166,48.5));
#86258=CARTESIAN_POINT('Ctrl Pts',(29.7703956793994,2.37994545698166,48.5));
#86259=CARTESIAN_POINT('Ctrl Pts',(29.8761936258525,2.2328787446022,48.5));
#86260=CARTESIAN_POINT('Ctrl Pts',(29.8761936258525,2.02878588438034,48.5));
#86261=CARTESIAN_POINT('',(29.7703956793994,2.37994545698166,48.35));
#86262=CARTESIAN_POINT('',(29.7703956793994,2.37994545698166,48.5));
#86263=CARTESIAN_POINT('Ctrl Pts',(29.7703956793994,2.37994545698166,48.35));
#86264=CARTESIAN_POINT('Ctrl Pts',(29.8761936258525,2.2328787446022,48.35));
#86265=CARTESIAN_POINT('Ctrl Pts',(29.8761936258525,2.02878588438034,48.35));
#86266=CARTESIAN_POINT('Ctrl Pts',(29.4620054196566,2.59304249286652,48.5));
#86267=CARTESIAN_POINT('Ctrl Pts',(29.4620054196566,2.59304249286652,48.35));
#86268=CARTESIAN_POINT('Ctrl Pts',(29.6645974349231,2.52701246738434,48.5));
#86269=CARTESIAN_POINT('Ctrl Pts',(29.6645974349231,2.52701246738434,48.35));
#86270=CARTESIAN_POINT('Ctrl Pts',(29.7703956793994,2.37994545698166,48.5));
#86271=CARTESIAN_POINT('Ctrl Pts',(29.7703956793994,2.37994545698166,48.35));
#86272=CARTESIAN_POINT('',(29.4620054196566,2.59304249286652,48.5));
#86273=CARTESIAN_POINT('Ctrl Pts',(29.4620054196566,2.59304249286652,48.5));
#86274=CARTESIAN_POINT('Ctrl Pts',(29.6645974349231,2.52701246738434,48.5));
#86275=CARTESIAN_POINT('Ctrl Pts',(29.7703956793994,2.37994545698166,48.5));
#86276=CARTESIAN_POINT('',(29.4620054196566,2.59304249286652,48.35));
#86277=CARTESIAN_POINT('',(29.4620054196566,2.59304249286652,48.5));
#86278=CARTESIAN_POINT('Ctrl Pts',(29.4620054196566,2.59304249286652,48.35));
#86279=CARTESIAN_POINT('Ctrl Pts',(29.6645974349231,2.52701246738434,48.35));
#86280=CARTESIAN_POINT('Ctrl Pts',(29.7703956793994,2.37994545698166,48.35));
#86281=CARTESIAN_POINT('Ctrl Pts',(29.7058662008494,2.76787185668945,48.5));
#86282=CARTESIAN_POINT('Ctrl Pts',(29.7058662008494,2.76787185668945,48.35));
#86283=CARTESIAN_POINT('Ctrl Pts',(29.6255796384066,2.65457028150558,48.5));
#86284=CARTESIAN_POINT('Ctrl Pts',(29.6255796384066,2.65457028150558,48.35));
#86285=CARTESIAN_POINT('Ctrl Pts',(29.4620054196566,2.59304249286652,48.5));
#86286=CARTESIAN_POINT('Ctrl Pts',(29.4620054196566,2.59304249286652,48.35));
#86287=CARTESIAN_POINT('',(29.7058662008494,2.76787185668945,48.5));
#86288=CARTESIAN_POINT('Ctrl Pts',(29.7058662008494,2.76787185668945,48.5));
#86289=CARTESIAN_POINT('Ctrl Pts',(29.6255796384066,2.65457028150558,48.5));
#86290=CARTESIAN_POINT('Ctrl Pts',(29.4620054196566,2.59304249286652,48.5));
#86291=CARTESIAN_POINT('',(29.7058662008494,2.76787185668945,48.35));
#86292=CARTESIAN_POINT('',(29.7058662008494,2.76787185668945,48.5));
#86293=CARTESIAN_POINT('Ctrl Pts',(29.7058662008494,2.76787185668945,48.35));
#86294=CARTESIAN_POINT('Ctrl Pts',(29.6255796384066,2.65457028150558,48.35));
#86295=CARTESIAN_POINT('Ctrl Pts',(29.4620054196566,2.59304249286652,48.35));
#86296=CARTESIAN_POINT('Ctrl Pts',(29.7861527632922,3.03424292802811,48.5));
#86297=CARTESIAN_POINT('Ctrl Pts',(29.7861527632922,3.03424292802811,48.35));
#86298=CARTESIAN_POINT('Ctrl Pts',(29.7861527632922,2.88117328286171,48.5));
#86299=CARTESIAN_POINT('Ctrl Pts',(29.7861527632922,2.88117328286171,48.35));
#86300=CARTESIAN_POINT('Ctrl Pts',(29.7058662008494,2.76787185668945,48.5));
#86301=CARTESIAN_POINT('Ctrl Pts',(29.7058662008494,2.76787185668945,48.35));
#86302=CARTESIAN_POINT('',(29.7861527632922,3.03424292802811,48.5));
#86303=CARTESIAN_POINT('Ctrl Pts',(29.7861527632922,3.03424292802811,48.5));
#86304=CARTESIAN_POINT('Ctrl Pts',(29.7861527632922,2.88117328286171,48.5));
#86305=CARTESIAN_POINT('Ctrl Pts',(29.7058662008494,2.76787185668945,48.5));
#86306=CARTESIAN_POINT('',(29.7861527632922,3.03424292802811,48.35));
#86307=CARTESIAN_POINT('',(29.7861527632922,3.03424292802811,48.5));
#86308=CARTESIAN_POINT('Ctrl Pts',(29.7861527632922,3.03424292802811,48.35));
#86309=CARTESIAN_POINT('Ctrl Pts',(29.7861527632922,2.88117328286171,48.35));
#86310=CARTESIAN_POINT('Ctrl Pts',(29.7058662008494,2.76787185668945,48.35));
#86311=CARTESIAN_POINT('Ctrl Pts',(29.6105729769915,3.4416780769825,48.5));
#86312=CARTESIAN_POINT('Ctrl Pts',(29.6105729769915,3.4416780769825,48.35));
#86313=CARTESIAN_POINT('Ctrl Pts',(29.7861527632922,3.27435204386711,48.5));
#86314=CARTESIAN_POINT('Ctrl Pts',(29.7861527632922,3.27435204386711,48.35));
#86315=CARTESIAN_POINT('Ctrl Pts',(29.7861527632922,3.03424292802811,48.5));
#86316=CARTESIAN_POINT('Ctrl Pts',(29.7861527632922,3.03424292802811,48.35));
#86317=CARTESIAN_POINT('',(29.6105729769915,3.4416780769825,48.5));
#86318=CARTESIAN_POINT('Ctrl Pts',(29.6105729769915,3.4416780769825,48.5));
#86319=CARTESIAN_POINT('Ctrl Pts',(29.7861527632922,3.27435204386711,48.5));
#86320=CARTESIAN_POINT('Ctrl Pts',(29.7861527632922,3.03424292802811,48.5));
#86321=CARTESIAN_POINT('',(29.6105729769915,3.4416780769825,48.35));
#86322=CARTESIAN_POINT('',(29.6105729769915,3.4416780769825,48.5));
#86323=CARTESIAN_POINT('Ctrl Pts',(29.6105729769915,3.4416780769825,48.35));
#86324=CARTESIAN_POINT('Ctrl Pts',(29.7861527632922,3.27435204386711,48.35));
#86325=CARTESIAN_POINT('Ctrl Pts',(29.7861527632922,3.03424292802811,48.35));
#86326=CARTESIAN_POINT('Ctrl Pts',(29.1468622516841,3.60900411009789,48.5));
#86327=CARTESIAN_POINT('Ctrl Pts',(29.1468622516841,3.60900411009789,48.35));
#86328=CARTESIAN_POINT('Ctrl Pts',(29.4349931906909,3.60900411009789,48.5));
#86329=CARTESIAN_POINT('Ctrl Pts',(29.4349931906909,3.60900411009789,48.35));
#86330=CARTESIAN_POINT('Ctrl Pts',(29.6105729769915,3.4416780769825,48.5));
#86331=CARTESIAN_POINT('Ctrl Pts',(29.6105729769915,3.4416780769825,48.35));
#86332=CARTESIAN_POINT('',(29.1468622516841,3.60900411009789,48.5));
#86333=CARTESIAN_POINT('Ctrl Pts',(29.1468622516841,3.60900411009789,48.5));
#86334=CARTESIAN_POINT('Ctrl Pts',(29.4349931906909,3.60900411009789,48.5));
#86335=CARTESIAN_POINT('Ctrl Pts',(29.6105729769915,3.4416780769825,48.5));
#86336=CARTESIAN_POINT('',(29.1468622516841,3.60900411009789,48.35));
#86337=CARTESIAN_POINT('',(29.1468622516841,3.60900411009789,48.5));
#86338=CARTESIAN_POINT('Ctrl Pts',(29.1468622516841,3.60900411009789,48.35));
#86339=CARTESIAN_POINT('Ctrl Pts',(29.4349931906909,3.60900411009789,48.35));
#86340=CARTESIAN_POINT('Ctrl Pts',(29.6105729769915,3.4416780769825,48.35));
#86341=CARTESIAN_POINT('Ctrl Pts',(28.6876534651965,3.44542974233627,48.5));
#86342=CARTESIAN_POINT('Ctrl Pts',(28.6876534651965,3.44542974233627,48.35));
#86343=CARTESIAN_POINT('Ctrl Pts',(28.8602318596095,3.60900411009789,48.5));
#86344=CARTESIAN_POINT('Ctrl Pts',(28.8602318596095,3.60900411009789,48.35));
#86345=CARTESIAN_POINT('Ctrl Pts',(29.1468622516841,3.60900411009789,48.5));
#86346=CARTESIAN_POINT('Ctrl Pts',(29.1468622516841,3.60900411009789,48.35));
#86347=CARTESIAN_POINT('',(28.6876534651965,3.44542974233627,48.5));
#86348=CARTESIAN_POINT('Ctrl Pts',(28.6876534651965,3.44542974233627,48.5));
#86349=CARTESIAN_POINT('Ctrl Pts',(28.8602318596095,3.60900411009789,48.5));
#86350=CARTESIAN_POINT('Ctrl Pts',(29.1468622516841,3.60900411009789,48.5));
#86351=CARTESIAN_POINT('',(28.6876534651965,3.44542974233627,48.35));
#86352=CARTESIAN_POINT('',(28.6876534651965,3.44542974233627,48.5));
#86353=CARTESIAN_POINT('Ctrl Pts',(28.6876534651965,3.44542974233627,48.35));
#86354=CARTESIAN_POINT('Ctrl Pts',(28.8602318596095,3.60900411009789,48.35));
#86355=CARTESIAN_POINT('Ctrl Pts',(29.1468622516841,3.60900411009789,48.35));
#86356=CARTESIAN_POINT('Ctrl Pts',(28.5150750707835,3.04174625873566,48.5));
#86357=CARTESIAN_POINT('Ctrl Pts',(28.5150750707835,3.04174625873566,48.35));
#86358=CARTESIAN_POINT('Ctrl Pts',(28.5150750707835,3.28185537457466,48.5));
#86359=CARTESIAN_POINT('Ctrl Pts',(28.5150750707835,3.28185537457466,48.35));
#86360=CARTESIAN_POINT('Ctrl Pts',(28.6876534651965,3.44542974233627,48.5));
#86361=CARTESIAN_POINT('Ctrl Pts',(28.6876534651965,3.44542974233627,48.35));
#86362=CARTESIAN_POINT('',(28.5150750707835,3.04174625873566,48.5));
#86363=CARTESIAN_POINT('Ctrl Pts',(28.5150750707835,3.04174625873566,48.5));
#86364=CARTESIAN_POINT('Ctrl Pts',(28.5150750707835,3.28185537457466,48.5));
#86365=CARTESIAN_POINT('Ctrl Pts',(28.6876534651965,3.44542974233627,48.5));
#86366=CARTESIAN_POINT('',(28.5150750707835,3.04174625873566,48.35));
#86367=CARTESIAN_POINT('',(28.5150750707835,3.04174625873566,48.5));
#86368=CARTESIAN_POINT('Ctrl Pts',(28.5150750707835,3.04174625873566,48.35));
#86369=CARTESIAN_POINT('Ctrl Pts',(28.5150750707835,3.28185537457466,48.35));
#86370=CARTESIAN_POINT('Ctrl Pts',(28.6876534651965,3.44542974233627,48.35));
#86371=CARTESIAN_POINT('Ctrl Pts',(28.5961119066924,2.76862213015556,48.5));
#86372=CARTESIAN_POINT('Ctrl Pts',(28.5961119066924,2.76862213015556,48.35));
#86373=CARTESIAN_POINT('Ctrl Pts',(28.5150750707835,2.88267397880554,48.5));
#86374=CARTESIAN_POINT('Ctrl Pts',(28.5150750707835,2.88267397880554,48.35));
#86375=CARTESIAN_POINT('Ctrl Pts',(28.5150750707835,3.04174625873566,48.5));
#86376=CARTESIAN_POINT('Ctrl Pts',(28.5150750707835,3.04174625873566,48.35));
#86377=CARTESIAN_POINT('',(28.5961119066924,2.76862213015556,48.5));
#86378=CARTESIAN_POINT('Ctrl Pts',(28.5961119066924,2.76862213015556,48.5));
#86379=CARTESIAN_POINT('Ctrl Pts',(28.5150750707835,2.88267397880554,48.5));
#86380=CARTESIAN_POINT('Ctrl Pts',(28.5150750707835,3.04174625873566,48.5));
#86381=CARTESIAN_POINT('',(28.5961119066924,2.76862213015556,48.35));
#86382=CARTESIAN_POINT('',(28.5961119066924,2.76862213015556,48.5));
#86383=CARTESIAN_POINT('Ctrl Pts',(28.5961119066924,2.76862213015556,48.35));
#86384=CARTESIAN_POINT('Ctrl Pts',(28.5150750707835,2.88267397880554,48.35));
#86385=CARTESIAN_POINT('Ctrl Pts',(28.5150750707835,3.04174625873566,48.35));
#86386=CARTESIAN_POINT('Ctrl Pts',(28.8452250491828,2.59304249286652,48.5));
#86387=CARTESIAN_POINT('Ctrl Pts',(28.8452250491828,2.59304249286652,48.35));
#86388=CARTESIAN_POINT('Ctrl Pts',(28.6771487426013,2.65457028150558,48.5));
#86389=CARTESIAN_POINT('Ctrl Pts',(28.6771487426013,2.65457028150558,48.35));
#86390=CARTESIAN_POINT('Ctrl Pts',(28.5961119066924,2.76862213015556,48.5));
#86391=CARTESIAN_POINT('Ctrl Pts',(28.5961119066924,2.76862213015556,48.35));
#86392=CARTESIAN_POINT('',(28.8452250491828,2.59304249286652,48.5));
#86393=CARTESIAN_POINT('Ctrl Pts',(28.8452250491828,2.59304249286652,48.5));
#86394=CARTESIAN_POINT('Ctrl Pts',(28.6771487426013,2.65457028150558,48.5));
#86395=CARTESIAN_POINT('Ctrl Pts',(28.5961119066924,2.76862213015556,48.5));
#86396=CARTESIAN_POINT('',(28.8452250491828,2.59304249286652,48.35));
#86397=CARTESIAN_POINT('',(28.8452250491828,2.59304249286652,48.5));
#86398=CARTESIAN_POINT('Ctrl Pts',(28.8452250491828,2.59304249286652,48.35));
#86399=CARTESIAN_POINT('Ctrl Pts',(28.6771487426013,2.65457028150558,48.35));
#86400=CARTESIAN_POINT('Ctrl Pts',(28.5961119066924,2.76862213015556,48.35));
#86401=CARTESIAN_POINT('Ctrl Pts',(28.5353342425078,2.39570268988609,48.5));
#86402=CARTESIAN_POINT('Ctrl Pts',(28.5353342425078,2.39570268988609,48.35));
#86403=CARTESIAN_POINT('Ctrl Pts',(28.6441337298602,2.54051858186722,48.5));
#86404=CARTESIAN_POINT('Ctrl Pts',(28.6441337298602,2.54051858186722,48.35));
#86405=CARTESIAN_POINT('Ctrl Pts',(28.8452250491828,2.59304249286652,48.5));
#86406=CARTESIAN_POINT('Ctrl Pts',(28.8452250491828,2.59304249286652,48.35));
#86407=CARTESIAN_POINT('Ctrl Pts',(28.5353342425078,2.39570268988609,48.5));
#86408=CARTESIAN_POINT('Ctrl Pts',(28.6441337298602,2.54051858186722,48.5));
#86409=CARTESIAN_POINT('Ctrl Pts',(28.8452250491828,2.59304249286652,48.5));
#86410=CARTESIAN_POINT('Ctrl Pts',(28.5353342425078,2.39570268988609,48.35));
#86411=CARTESIAN_POINT('Ctrl Pts',(28.6441337298602,2.54051858186722,48.35));
#86412=CARTESIAN_POINT('Ctrl Pts',(28.8452250491828,2.59304249286652,48.35));
#86413=CARTESIAN_POINT('Origin',(29.9999997746199,2.48574362695217,48.35));
#86414=CARTESIAN_POINT('Origin',(0.,8.,48.5));
#86415=CARTESIAN_POINT('Origin',(0.,8.,48.5));
#86416=CARTESIAN_POINT('Origin',(0.,8.,48.5));
#86417=CARTESIAN_POINT('Ctrl Pts',(20.8516373746097,3.38540250062943,48.5));
#86418=CARTESIAN_POINT('Ctrl Pts',(20.8516373746097,3.38540250062943,48.35));
#86419=CARTESIAN_POINT('Ctrl Pts',(20.6655525676906,3.38540250062943,48.5));
#86420=CARTESIAN_POINT('Ctrl Pts',(20.6655525676906,3.38540250062943,48.35));
#86421=CARTESIAN_POINT('Ctrl Pts',(20.5545022599399,3.22783091664314,48.5));
#86422=CARTESIAN_POINT('Ctrl Pts',(20.5545022599399,3.22783091664314,48.35));
#86423=CARTESIAN_POINT('',(20.8516373746097,3.38540250062943,48.5));
#86424=CARTESIAN_POINT('',(20.5545022599399,3.22783091664314,48.5));
#86425=CARTESIAN_POINT('Ctrl Pts',(20.8516373746097,3.38540250062943,48.5));
#86426=CARTESIAN_POINT('Ctrl Pts',(20.6655525676906,3.38540250062943,48.5));
#86427=CARTESIAN_POINT('Ctrl Pts',(20.5545022599399,3.22783091664314,48.5));
#86428=CARTESIAN_POINT('',(20.8516373746097,3.38540250062943,48.35));
#86429=CARTESIAN_POINT('',(20.8516373746097,3.38540250062943,48.5));
#86430=CARTESIAN_POINT('',(20.5545022599399,3.22783091664314,48.35));
#86431=CARTESIAN_POINT('Ctrl Pts',(20.8516373746097,3.38540250062943,48.35));
#86432=CARTESIAN_POINT('Ctrl Pts',(20.6655525676906,3.38540250062943,48.35));
#86433=CARTESIAN_POINT('Ctrl Pts',(20.5545022599399,3.22783091664314,48.35));
#86434=CARTESIAN_POINT('',(20.5545022599399,3.22783091664314,48.5));
#86435=CARTESIAN_POINT('Ctrl Pts',(21.1675306670368,3.2068213224411,48.5));
#86436=CARTESIAN_POINT('Ctrl Pts',(21.1675306670368,3.2068213224411,48.35));
#86437=CARTESIAN_POINT('Ctrl Pts',(21.04072297737,3.38540250062943,48.5));
#86438=CARTESIAN_POINT('Ctrl Pts',(21.04072297737,3.38540250062943,48.35));
#86439=CARTESIAN_POINT('Ctrl Pts',(20.8516373746097,3.38540250062943,48.5));
#86440=CARTESIAN_POINT('Ctrl Pts',(20.8516373746097,3.38540250062943,48.35));
#86441=CARTESIAN_POINT('',(21.1675306670368,3.2068213224411,48.5));
#86442=CARTESIAN_POINT('Ctrl Pts',(21.1675306670368,3.2068213224411,48.5));
#86443=CARTESIAN_POINT('Ctrl Pts',(21.04072297737,3.38540250062943,48.5));
#86444=CARTESIAN_POINT('Ctrl Pts',(20.8516373746097,3.38540250062943,48.5));
#86445=CARTESIAN_POINT('',(21.1675306670368,3.2068213224411,48.35));
#86446=CARTESIAN_POINT('',(21.1675306670368,3.2068213224411,48.5));
#86447=CARTESIAN_POINT('Ctrl Pts',(21.1675306670368,3.2068213224411,48.35));
#86448=CARTESIAN_POINT('Ctrl Pts',(21.04072297737,3.38540250062943,48.35));
#86449=CARTESIAN_POINT('Ctrl Pts',(20.8516373746097,3.38540250062943,48.35));
#86450=CARTESIAN_POINT('Ctrl Pts',(21.2943383567035,2.48499327898026,48.5));
#86451=CARTESIAN_POINT('Ctrl Pts',(21.2943383567035,2.48499327898026,48.35));
#86452=CARTESIAN_POINT('Ctrl Pts',(21.2943383567035,3.02824014425278,48.5));
#86453=CARTESIAN_POINT('Ctrl Pts',(21.2943383567035,3.02824014425278,48.35));
#86454=CARTESIAN_POINT('Ctrl Pts',(21.1675306670368,3.2068213224411,48.5));
#86455=CARTESIAN_POINT('Ctrl Pts',(21.1675306670368,3.2068213224411,48.35));
#86456=CARTESIAN_POINT('',(21.2943383567035,2.48499327898026,48.5));
#86457=CARTESIAN_POINT('Ctrl Pts',(21.2943383567035,2.48499327898026,48.5));
#86458=CARTESIAN_POINT('Ctrl Pts',(21.2943383567035,3.02824014425278,48.5));
#86459=CARTESIAN_POINT('Ctrl Pts',(21.1675306670368,3.2068213224411,48.5));
#86460=CARTESIAN_POINT('',(21.2943383567035,2.48499327898026,48.35));
#86461=CARTESIAN_POINT('',(21.2943383567035,2.48499327898026,48.5));
#86462=CARTESIAN_POINT('Ctrl Pts',(21.2943383567035,2.48499327898026,48.35));
#86463=CARTESIAN_POINT('Ctrl Pts',(21.2943383567035,3.02824014425278,48.35));
#86464=CARTESIAN_POINT('Ctrl Pts',(21.1675306670368,3.2068213224411,48.35));
#86465=CARTESIAN_POINT('Ctrl Pts',(21.1675306670368,1.76466578245163,48.5));
#86466=CARTESIAN_POINT('Ctrl Pts',(21.1675306670368,1.76466578245163,48.35));
#86467=CARTESIAN_POINT('Ctrl Pts',(21.2943383567035,1.9447478055954,48.5));
#86468=CARTESIAN_POINT('Ctrl Pts',(21.2943383567035,1.9447478055954,48.35));
#86469=CARTESIAN_POINT('Ctrl Pts',(21.2943383567035,2.48499327898026,48.5));
#86470=CARTESIAN_POINT('Ctrl Pts',(21.2943383567035,2.48499327898026,48.35));
#86471=CARTESIAN_POINT('',(21.1675306670368,1.76466578245163,48.5));
#86472=CARTESIAN_POINT('Ctrl Pts',(21.1675306670368,1.76466578245163,48.5));
#86473=CARTESIAN_POINT('Ctrl Pts',(21.2943383567035,1.9447478055954,48.5));
#86474=CARTESIAN_POINT('Ctrl Pts',(21.2943383567035,2.48499327898026,48.5));
#86475=CARTESIAN_POINT('',(21.1675306670368,1.76466578245163,48.35));
#86476=CARTESIAN_POINT('',(21.1675306670368,1.76466578245163,48.5));
#86477=CARTESIAN_POINT('Ctrl Pts',(21.1675306670368,1.76466578245163,48.35));
#86478=CARTESIAN_POINT('Ctrl Pts',(21.2943383567035,1.9447478055954,48.35));
#86479=CARTESIAN_POINT('Ctrl Pts',(21.2943383567035,2.48499327898026,48.35));
#86480=CARTESIAN_POINT('Ctrl Pts',(20.8546384684741,1.58458405733109,48.5));
#86481=CARTESIAN_POINT('Ctrl Pts',(20.8546384684741,1.58458405733109,48.35));
#86482=CARTESIAN_POINT('Ctrl Pts',(21.04072297737,1.58458405733109,48.5));
#86483=CARTESIAN_POINT('Ctrl Pts',(21.04072297737,1.58458405733109,48.35));
#86484=CARTESIAN_POINT('Ctrl Pts',(21.1675306670368,1.76466578245163,48.5));
#86485=CARTESIAN_POINT('Ctrl Pts',(21.1675306670368,1.76466578245163,48.35));
#86486=CARTESIAN_POINT('',(20.8546384684741,1.58458405733109,48.5));
#86487=CARTESIAN_POINT('Ctrl Pts',(20.8546384684741,1.58458405733109,48.5));
#86488=CARTESIAN_POINT('Ctrl Pts',(21.04072297737,1.58458405733109,48.5));
#86489=CARTESIAN_POINT('Ctrl Pts',(21.1675306670368,1.76466578245163,48.5));
#86490=CARTESIAN_POINT('',(20.8546384684741,1.58458405733109,48.35));
#86491=CARTESIAN_POINT('',(20.8546384684741,1.58458405733109,48.5));
#86492=CARTESIAN_POINT('Ctrl Pts',(20.8546384684741,1.58458405733109,48.35));
#86493=CARTESIAN_POINT('Ctrl Pts',(21.04072297737,1.58458405733109,48.35));
#86494=CARTESIAN_POINT('Ctrl Pts',(21.1675306670368,1.76466578245163,48.35));
#86495=CARTESIAN_POINT('Ctrl Pts',(20.5417462699115,1.76391565799713,48.5));
#86496=CARTESIAN_POINT('Ctrl Pts',(20.5417462699115,1.76391565799713,48.35));
#86497=CARTESIAN_POINT('Ctrl Pts',(20.6685539595783,1.58458405733109,48.5));
#86498=CARTESIAN_POINT('Ctrl Pts',(20.6685539595783,1.58458405733109,48.35));
#86499=CARTESIAN_POINT('Ctrl Pts',(20.8546384684741,1.58458405733109,48.5));
#86500=CARTESIAN_POINT('Ctrl Pts',(20.8546384684741,1.58458405733109,48.35));
#86501=CARTESIAN_POINT('',(20.5417462699115,1.76391565799713,48.5));
#86502=CARTESIAN_POINT('Ctrl Pts',(20.5417462699115,1.76391565799713,48.5));
#86503=CARTESIAN_POINT('Ctrl Pts',(20.6685539595783,1.58458405733109,48.5));
#86504=CARTESIAN_POINT('Ctrl Pts',(20.8546384684741,1.58458405733109,48.5));
#86505=CARTESIAN_POINT('',(20.5417462699115,1.76391565799713,48.35));
#86506=CARTESIAN_POINT('',(20.5417462699115,1.76391565799713,48.5));
#86507=CARTESIAN_POINT('Ctrl Pts',(20.5417462699115,1.76391565799713,48.35));
#86508=CARTESIAN_POINT('Ctrl Pts',(20.6685539595783,1.58458405733109,48.35));
#86509=CARTESIAN_POINT('Ctrl Pts',(20.8546384684741,1.58458405733109,48.35));
#86510=CARTESIAN_POINT('Ctrl Pts',(20.4149385802448,2.48499327898026,48.5));
#86511=CARTESIAN_POINT('Ctrl Pts',(20.4149385802448,2.48499327898026,48.35));
#86512=CARTESIAN_POINT('Ctrl Pts',(20.4149385802448,1.94324696063995,48.5));
#86513=CARTESIAN_POINT('Ctrl Pts',(20.4149385802448,1.94324696063995,48.35));
#86514=CARTESIAN_POINT('Ctrl Pts',(20.5417462699115,1.76391565799713,48.5));
#86515=CARTESIAN_POINT('Ctrl Pts',(20.5417462699115,1.76391565799713,48.35));
#86516=CARTESIAN_POINT('',(20.4149385802448,2.48499327898026,48.5));
#86517=CARTESIAN_POINT('Ctrl Pts',(20.4149385802448,2.48499327898026,48.5));
#86518=CARTESIAN_POINT('Ctrl Pts',(20.4149385802448,1.94324696063995,48.5));
#86519=CARTESIAN_POINT('Ctrl Pts',(20.5417462699115,1.76391565799713,48.5));
#86520=CARTESIAN_POINT('',(20.4149385802448,2.48499327898026,48.35));
#86521=CARTESIAN_POINT('',(20.4149385802448,2.48499327898026,48.5));
#86522=CARTESIAN_POINT('Ctrl Pts',(20.4149385802448,2.48499327898026,48.35));
#86523=CARTESIAN_POINT('Ctrl Pts',(20.4149385802448,1.94324696063995,48.35));
#86524=CARTESIAN_POINT('Ctrl Pts',(20.5417462699115,1.76391565799713,48.35));
#86525=CARTESIAN_POINT('Ctrl Pts',(20.5545022599399,3.22783091664314,48.5));
#86526=CARTESIAN_POINT('Ctrl Pts',(20.5545022599399,3.22783091664314,48.35));
#86527=CARTESIAN_POINT('Ctrl Pts',(20.4149385802448,3.02673944830894,48.5));
#86528=CARTESIAN_POINT('Ctrl Pts',(20.4149385802448,3.02673944830894,48.35));
#86529=CARTESIAN_POINT('Ctrl Pts',(20.4149385802448,2.48499327898026,48.5));
#86530=CARTESIAN_POINT('Ctrl Pts',(20.4149385802448,2.48499327898026,48.35));
#86531=CARTESIAN_POINT('Ctrl Pts',(20.5545022599399,3.22783091664314,48.5));
#86532=CARTESIAN_POINT('Ctrl Pts',(20.4149385802448,3.02673944830894,48.5));
#86533=CARTESIAN_POINT('Ctrl Pts',(20.4149385802448,2.48499327898026,48.5));
#86534=CARTESIAN_POINT('Ctrl Pts',(20.5545022599399,3.22783091664314,48.35));
#86535=CARTESIAN_POINT('Ctrl Pts',(20.4149385802448,3.02673944830894,48.35));
#86536=CARTESIAN_POINT('Ctrl Pts',(20.4149385802448,2.48499327898026,48.35));
#86537=CARTESIAN_POINT('Ctrl Pts',(20.8546384684741,1.36248314380646,48.5));
#86538=CARTESIAN_POINT('Ctrl Pts',(20.8546384684741,1.36248314380646,48.35));
#86539=CARTESIAN_POINT('Ctrl Pts',(20.5364939086139,1.36248314380646,48.5));
#86540=CARTESIAN_POINT('Ctrl Pts',(20.5364939086139,1.36248314380646,48.35));
#86541=CARTESIAN_POINT('Ctrl Pts',(20.3549113385379,1.59058684110642,48.5));
#86542=CARTESIAN_POINT('Ctrl Pts',(20.3549113385379,1.59058684110642,48.35));
#86543=CARTESIAN_POINT('',(20.8546384684741,1.36248314380646,48.5));
#86544=CARTESIAN_POINT('',(20.3549113385379,1.59058684110642,48.5));
#86545=CARTESIAN_POINT('Ctrl Pts',(20.8546384684741,1.36248314380646,48.5));
#86546=CARTESIAN_POINT('Ctrl Pts',(20.5364939086139,1.36248314380646,48.5));
#86547=CARTESIAN_POINT('Ctrl Pts',(20.3549113385379,1.59058684110642,48.5));
#86548=CARTESIAN_POINT('',(20.8546384684741,1.36248314380646,48.35));
#86549=CARTESIAN_POINT('',(20.8546384684741,1.36248314380646,48.5));
#86550=CARTESIAN_POINT('',(20.3549113385379,1.59058684110642,48.35));
#86551=CARTESIAN_POINT('Ctrl Pts',(20.8546384684741,1.36248314380646,48.35));
#86552=CARTESIAN_POINT('Ctrl Pts',(20.5364939086139,1.36248314380646,48.35));
#86553=CARTESIAN_POINT('Ctrl Pts',(20.3549113385379,1.59058684110642,48.35));
#86554=CARTESIAN_POINT('',(20.3549113385379,1.59058684110642,48.5));
#86555=CARTESIAN_POINT('Ctrl Pts',(21.2545701377094,1.49229192733765,48.5));
#86556=CARTESIAN_POINT('Ctrl Pts',(21.2545701377094,1.49229192733765,48.35));
#86557=CARTESIAN_POINT('Ctrl Pts',(21.096248280257,1.36248314380646,48.5));
#86558=CARTESIAN_POINT('Ctrl Pts',(21.096248280257,1.36248314380646,48.35));
#86559=CARTESIAN_POINT('Ctrl Pts',(20.8546384684741,1.36248314380646,48.5));
#86560=CARTESIAN_POINT('Ctrl Pts',(20.8546384684741,1.36248314380646,48.35));
#86561=CARTESIAN_POINT('',(21.2545701377094,1.49229192733765,48.5));
#86562=CARTESIAN_POINT('Ctrl Pts',(21.2545701377094,1.49229192733765,48.5));
#86563=CARTESIAN_POINT('Ctrl Pts',(21.096248280257,1.36248314380646,48.5));
#86564=CARTESIAN_POINT('Ctrl Pts',(20.8546384684741,1.36248314380646,48.5));
#86565=CARTESIAN_POINT('',(21.2545701377094,1.49229192733765,48.35));
#86566=CARTESIAN_POINT('',(21.2545701377094,1.49229192733765,48.5));
#86567=CARTESIAN_POINT('Ctrl Pts',(21.2545701377094,1.49229192733765,48.35));
#86568=CARTESIAN_POINT('Ctrl Pts',(21.096248280257,1.36248314380646,48.35));
#86569=CARTESIAN_POINT('Ctrl Pts',(20.8546384684741,1.36248314380646,48.35));
#86570=CARTESIAN_POINT('Ctrl Pts',(21.4924284331501,1.85995900630951,48.5));
#86571=CARTESIAN_POINT('Ctrl Pts',(21.4924284331501,1.85995900630951,48.35));
#86572=CARTESIAN_POINT('Ctrl Pts',(21.4128919951618,1.62210100889206,48.5));
#86573=CARTESIAN_POINT('Ctrl Pts',(21.4128919951618,1.62210100889206,48.35));
#86574=CARTESIAN_POINT('Ctrl Pts',(21.2545701377094,1.49229192733765,48.5));
#86575=CARTESIAN_POINT('Ctrl Pts',(21.2545701377094,1.49229192733765,48.35));
#86576=CARTESIAN_POINT('',(21.4924284331501,1.85995900630951,48.5));
#86577=CARTESIAN_POINT('Ctrl Pts',(21.4924284331501,1.85995900630951,48.5));
#86578=CARTESIAN_POINT('Ctrl Pts',(21.4128919951618,1.62210100889206,48.5));
#86579=CARTESIAN_POINT('Ctrl Pts',(21.2545701377094,1.49229192733765,48.5));
#86580=CARTESIAN_POINT('',(21.4924284331501,1.85995900630951,48.35));
#86581=CARTESIAN_POINT('',(21.4924284331501,1.85995900630951,48.5));
#86582=CARTESIAN_POINT('Ctrl Pts',(21.4924284331501,1.85995900630951,48.35));
#86583=CARTESIAN_POINT('Ctrl Pts',(21.4128919951618,1.62210100889206,48.35));
#86584=CARTESIAN_POINT('Ctrl Pts',(21.2545701377094,1.49229192733765,48.35));
#86585=CARTESIAN_POINT('Ctrl Pts',(21.5719642750919,2.48499327898026,48.5));
#86586=CARTESIAN_POINT('Ctrl Pts',(21.5719642750919,2.48499327898026,48.35));
#86587=CARTESIAN_POINT('Ctrl Pts',(21.5719642750919,2.09781730175018,48.5));
#86588=CARTESIAN_POINT('Ctrl Pts',(21.5719642750919,2.09781730175018,48.35));
#86589=CARTESIAN_POINT('Ctrl Pts',(21.4924284331501,1.85995900630951,48.5));
#86590=CARTESIAN_POINT('Ctrl Pts',(21.4924284331501,1.85995900630951,48.35));
#86591=CARTESIAN_POINT('',(21.5719642750919,2.48499327898026,48.5));
#86592=CARTESIAN_POINT('Ctrl Pts',(21.5719642750919,2.48499327898026,48.5));
#86593=CARTESIAN_POINT('Ctrl Pts',(21.5719642750919,2.09781730175018,48.5));
#86594=CARTESIAN_POINT('Ctrl Pts',(21.4924284331501,1.85995900630951,48.5));
#86595=CARTESIAN_POINT('',(21.5719642750919,2.48499327898026,48.35));
#86596=CARTESIAN_POINT('',(21.5719642750919,2.48499327898026,48.5));
#86597=CARTESIAN_POINT('Ctrl Pts',(21.5719642750919,2.48499327898026,48.35));
#86598=CARTESIAN_POINT('Ctrl Pts',(21.5719642750919,2.09781730175018,48.35));
#86599=CARTESIAN_POINT('Ctrl Pts',(21.4924284331501,1.85995900630951,48.35));
#86600=CARTESIAN_POINT('Ctrl Pts',(21.5224417559803,3.00497958064079,48.5));
#86601=CARTESIAN_POINT('Ctrl Pts',(21.5224417559803,3.00497958064079,48.35));
#86602=CARTESIAN_POINT('Ctrl Pts',(21.5719642750919,2.81214186549187,48.5));
#86603=CARTESIAN_POINT('Ctrl Pts',(21.5719642750919,2.81214186549187,48.35));
#86604=CARTESIAN_POINT('Ctrl Pts',(21.5719642750919,2.48499327898026,48.5));
#86605=CARTESIAN_POINT('Ctrl Pts',(21.5719642750919,2.48499327898026,48.35));
#86606=CARTESIAN_POINT('',(21.5224417559803,3.00497958064079,48.5));
#86607=CARTESIAN_POINT('Ctrl Pts',(21.5224417559803,3.00497958064079,48.5));
#86608=CARTESIAN_POINT('Ctrl Pts',(21.5719642750919,2.81214186549187,48.5));
#86609=CARTESIAN_POINT('Ctrl Pts',(21.5719642750919,2.48499327898026,48.5));
#86610=CARTESIAN_POINT('',(21.5224417559803,3.00497958064079,48.35));
#86611=CARTESIAN_POINT('',(21.5224417559803,3.00497958064079,48.5));
#86612=CARTESIAN_POINT('Ctrl Pts',(21.5224417559803,3.00497958064079,48.35));
#86613=CARTESIAN_POINT('Ctrl Pts',(21.5719642750919,2.81214186549187,48.35));
#86614=CARTESIAN_POINT('Ctrl Pts',(21.5719642750919,2.48499327898026,48.35));
#86615=CARTESIAN_POINT('Ctrl Pts',(21.385879766196,3.33212831616402,48.5));
#86616=CARTESIAN_POINT('Ctrl Pts',(21.385879766196,3.33212831616402,48.35));
#86617=CARTESIAN_POINT('Ctrl Pts',(21.4729192368686,3.19781729578972,48.5));
#86618=CARTESIAN_POINT('Ctrl Pts',(21.4729192368686,3.19781729578972,48.35));
#86619=CARTESIAN_POINT('Ctrl Pts',(21.5224417559803,3.00497958064079,48.5));
#86620=CARTESIAN_POINT('Ctrl Pts',(21.5224417559803,3.00497958064079,48.35));
#86621=CARTESIAN_POINT('',(21.385879766196,3.33212831616402,48.5));
#86622=CARTESIAN_POINT('Ctrl Pts',(21.385879766196,3.33212831616402,48.5));
#86623=CARTESIAN_POINT('Ctrl Pts',(21.4729192368686,3.19781729578972,48.5));
#86624=CARTESIAN_POINT('Ctrl Pts',(21.5224417559803,3.00497958064079,48.5));
#86625=CARTESIAN_POINT('',(21.385879766196,3.33212831616402,48.35));
#86626=CARTESIAN_POINT('',(21.385879766196,3.33212831616402,48.5));
#86627=CARTESIAN_POINT('Ctrl Pts',(21.385879766196,3.33212831616402,48.35));
#86628=CARTESIAN_POINT('Ctrl Pts',(21.4729192368686,3.19781729578972,48.35));
#86629=CARTESIAN_POINT('Ctrl Pts',(21.5224417559803,3.00497958064079,48.35));
#86630=CARTESIAN_POINT('Ctrl Pts',(21.1652799956501,3.5377217233181,48.5));
#86631=CARTESIAN_POINT('Ctrl Pts',(21.1652799956501,3.5377217233181,48.35));
#86632=CARTESIAN_POINT('Ctrl Pts',(21.2988402955234,3.46643933653831,48.5));
#86633=CARTESIAN_POINT('Ctrl Pts',(21.2988402955234,3.46643933653831,48.35));
#86634=CARTESIAN_POINT('Ctrl Pts',(21.385879766196,3.33212831616402,48.5));
#86635=CARTESIAN_POINT('Ctrl Pts',(21.385879766196,3.33212831616402,48.35));
#86636=CARTESIAN_POINT('',(21.1652799956501,3.5377217233181,48.5));
#86637=CARTESIAN_POINT('Ctrl Pts',(21.1652799956501,3.5377217233181,48.5));
#86638=CARTESIAN_POINT('Ctrl Pts',(21.2988402955234,3.46643933653831,48.5));
#86639=CARTESIAN_POINT('Ctrl Pts',(21.385879766196,3.33212831616402,48.5));
#86640=CARTESIAN_POINT('',(21.1652799956501,3.5377217233181,48.35));
#86641=CARTESIAN_POINT('',(21.1652799956501,3.5377217233181,48.5));
#86642=CARTESIAN_POINT('Ctrl Pts',(21.1652799956501,3.5377217233181,48.35));
#86643=CARTESIAN_POINT('Ctrl Pts',(21.2988402955234,3.46643933653831,48.35));
#86644=CARTESIAN_POINT('Ctrl Pts',(21.385879766196,3.33212831616402,48.35));
#86645=CARTESIAN_POINT('Ctrl Pts',(20.8546384684741,3.60900411009789,48.5));
#86646=CARTESIAN_POINT('Ctrl Pts',(20.8546384684741,3.60900411009789,48.35));
#86647=CARTESIAN_POINT('Ctrl Pts',(21.0317190997303,3.60900411009789,48.5));
#86648=CARTESIAN_POINT('Ctrl Pts',(21.0317190997303,3.60900411009789,48.35));
#86649=CARTESIAN_POINT('Ctrl Pts',(21.1652799956501,3.5377217233181,48.5));
#86650=CARTESIAN_POINT('Ctrl Pts',(21.1652799956501,3.5377217233181,48.35));
#86651=CARTESIAN_POINT('',(20.8546384684741,3.60900411009789,48.5));
#86652=CARTESIAN_POINT('Ctrl Pts',(20.8546384684741,3.60900411009789,48.5));
#86653=CARTESIAN_POINT('Ctrl Pts',(21.0317190997303,3.60900411009789,48.5));
#86654=CARTESIAN_POINT('Ctrl Pts',(21.1652799956501,3.5377217233181,48.5));
#86655=CARTESIAN_POINT('',(20.8546384684741,3.60900411009789,48.35));
#86656=CARTESIAN_POINT('',(20.8546384684741,3.60900411009789,48.5));
#86657=CARTESIAN_POINT('Ctrl Pts',(20.8546384684741,3.60900411009789,48.35));
#86658=CARTESIAN_POINT('Ctrl Pts',(21.0317190997303,3.60900411009789,48.35));
#86659=CARTESIAN_POINT('Ctrl Pts',(21.1652799956501,3.5377217233181,48.35));
#86660=CARTESIAN_POINT('Ctrl Pts',(20.4562076441944,3.47994545102119,48.5));
#86661=CARTESIAN_POINT('Ctrl Pts',(20.4562076441944,3.47994545102119,48.35));
#86662=CARTESIAN_POINT('Ctrl Pts',(20.6145295016468,3.60900411009789,48.5));
#86663=CARTESIAN_POINT('Ctrl Pts',(20.6145295016468,3.60900411009789,48.35));
#86664=CARTESIAN_POINT('Ctrl Pts',(20.8546384684741,3.60900411009789,48.5));
#86665=CARTESIAN_POINT('Ctrl Pts',(20.8546384684741,3.60900411009789,48.35));
#86666=CARTESIAN_POINT('',(20.4562076441944,3.47994545102119,48.5));
#86667=CARTESIAN_POINT('Ctrl Pts',(20.4562076441944,3.47994545102119,48.5));
#86668=CARTESIAN_POINT('Ctrl Pts',(20.6145295016468,3.60900411009789,48.5));
#86669=CARTESIAN_POINT('Ctrl Pts',(20.8546384684741,3.60900411009789,48.5));
#86670=CARTESIAN_POINT('',(20.4562076441944,3.47994545102119,48.35));
#86671=CARTESIAN_POINT('',(20.4562076441944,3.47994545102119,48.5));
#86672=CARTESIAN_POINT('Ctrl Pts',(20.4562076441944,3.47994545102119,48.35));
#86673=CARTESIAN_POINT('Ctrl Pts',(20.6145295016468,3.60900411009789,48.35));
#86674=CARTESIAN_POINT('Ctrl Pts',(20.8546384684741,3.60900411009789,48.35));
#86675=CARTESIAN_POINT('Ctrl Pts',(20.217598926276,3.11302864551544,48.5));
#86676=CARTESIAN_POINT('Ctrl Pts',(20.217598926276,3.11302864551544,48.35));
#86677=CARTESIAN_POINT('Ctrl Pts',(20.2978854887187,3.3508867919445,48.5));
#86678=CARTESIAN_POINT('Ctrl Pts',(20.2978854887187,3.3508867919445,48.35));
#86679=CARTESIAN_POINT('Ctrl Pts',(20.4562076441944,3.47994545102119,48.5));
#86680=CARTESIAN_POINT('Ctrl Pts',(20.4562076441944,3.47994545102119,48.35));
#86681=CARTESIAN_POINT('',(20.217598926276,3.11302864551544,48.5));
#86682=CARTESIAN_POINT('Ctrl Pts',(20.217598926276,3.11302864551544,48.5));
#86683=CARTESIAN_POINT('Ctrl Pts',(20.2978854887187,3.3508867919445,48.5));
#86684=CARTESIAN_POINT('Ctrl Pts',(20.4562076441944,3.47994545102119,48.5));
#86685=CARTESIAN_POINT('',(20.217598926276,3.11302864551544,48.35));
#86686=CARTESIAN_POINT('',(20.217598926276,3.11302864551544,48.5));
#86687=CARTESIAN_POINT('Ctrl Pts',(20.217598926276,3.11302864551544,48.35));
#86688=CARTESIAN_POINT('Ctrl Pts',(20.2978854887187,3.3508867919445,48.35));
#86689=CARTESIAN_POINT('Ctrl Pts',(20.4562076441944,3.47994545102119,48.35));
#86690=CARTESIAN_POINT('Ctrl Pts',(20.1373126618564,2.48499327898026,48.5));
#86691=CARTESIAN_POINT('Ctrl Pts',(20.1373126618564,2.48499327898026,48.35));
#86692=CARTESIAN_POINT('Ctrl Pts',(20.1373126618564,2.87517049908638,48.5));
#86693=CARTESIAN_POINT('Ctrl Pts',(20.1373126618564,2.87517049908638,48.35));
#86694=CARTESIAN_POINT('Ctrl Pts',(20.217598926276,3.11302864551544,48.5));
#86695=CARTESIAN_POINT('Ctrl Pts',(20.217598926276,3.11302864551544,48.35));
#86696=CARTESIAN_POINT('',(20.1373126618564,2.48499327898026,48.5));
#86697=CARTESIAN_POINT('Ctrl Pts',(20.1373126618564,2.48499327898026,48.5));
#86698=CARTESIAN_POINT('Ctrl Pts',(20.1373126618564,2.87517049908638,48.5));
#86699=CARTESIAN_POINT('Ctrl Pts',(20.217598926276,3.11302864551544,48.5));
#86700=CARTESIAN_POINT('',(20.1373126618564,2.48499327898026,48.35));
#86701=CARTESIAN_POINT('',(20.1373126618564,2.48499327898026,48.5));
#86702=CARTESIAN_POINT('Ctrl Pts',(20.1373126618564,2.48499327898026,48.35));
#86703=CARTESIAN_POINT('Ctrl Pts',(20.1373126618564,2.87517049908638,48.35));
#86704=CARTESIAN_POINT('Ctrl Pts',(20.217598926276,3.11302864551544,48.35));
#86705=CARTESIAN_POINT('Ctrl Pts',(20.3549113385379,1.59058684110642,48.5));
#86706=CARTESIAN_POINT('Ctrl Pts',(20.3549113385379,1.59058684110642,48.35));
#86707=CARTESIAN_POINT('Ctrl Pts',(20.1373126618564,1.86521166563034,48.5));
#86708=CARTESIAN_POINT('Ctrl Pts',(20.1373126618564,1.86521166563034,48.35));
#86709=CARTESIAN_POINT('Ctrl Pts',(20.1373126618564,2.48499327898026,48.5));
#86710=CARTESIAN_POINT('Ctrl Pts',(20.1373126618564,2.48499327898026,48.35));
#86711=CARTESIAN_POINT('Ctrl Pts',(20.3549113385379,1.59058684110642,48.5));
#86712=CARTESIAN_POINT('Ctrl Pts',(20.1373126618564,1.86521166563034,48.5));
#86713=CARTESIAN_POINT('Ctrl Pts',(20.1373126618564,2.48499327898026,48.5));
#86714=CARTESIAN_POINT('Ctrl Pts',(20.3549113385379,1.59058684110642,48.35));
#86715=CARTESIAN_POINT('Ctrl Pts',(20.1373126618564,1.86521166563034,48.35));
#86716=CARTESIAN_POINT('Ctrl Pts',(20.1373126618564,2.48499327898026,48.35));
#86717=CARTESIAN_POINT('Origin',(19.9999999515712,2.48574362695217,48.35));
#86718=CARTESIAN_POINT('Ctrl Pts',(19.1453617326915,2.38444769382477,48.5));
#86719=CARTESIAN_POINT('Ctrl Pts',(19.1453617326915,2.38444769382477,48.35));
#86720=CARTESIAN_POINT('Ctrl Pts',(19.3329469375312,2.38444769382477,48.5));
#86721=CARTESIAN_POINT('Ctrl Pts',(19.3329469375312,2.38444769382477,48.35));
#86722=CARTESIAN_POINT('Ctrl Pts',(19.453751694411,2.5157573223114,48.5));
#86723=CARTESIAN_POINT('Ctrl Pts',(19.453751694411,2.5157573223114,48.35));
#86724=CARTESIAN_POINT('',(19.1453617326915,2.38444769382477,48.5));
#86725=CARTESIAN_POINT('',(19.453751694411,2.5157573223114,48.5));
#86726=CARTESIAN_POINT('Ctrl Pts',(19.1453617326915,2.38444769382477,48.5));
#86727=CARTESIAN_POINT('Ctrl Pts',(19.3329469375312,2.38444769382477,48.5));
#86728=CARTESIAN_POINT('Ctrl Pts',(19.453751694411,2.5157573223114,48.5));
#86729=CARTESIAN_POINT('',(19.1453617326915,2.38444769382477,48.35));
#86730=CARTESIAN_POINT('',(19.1453617326915,2.38444769382477,48.5));
#86731=CARTESIAN_POINT('',(19.453751694411,2.5157573223114,48.35));
#86732=CARTESIAN_POINT('Ctrl Pts',(19.1453617326915,2.38444769382477,48.35));
#86733=CARTESIAN_POINT('Ctrl Pts',(19.3329469375312,2.38444769382477,48.35));
#86734=CARTESIAN_POINT('Ctrl Pts',(19.453751694411,2.5157573223114,48.35));
#86735=CARTESIAN_POINT('',(19.453751694411,2.5157573223114,48.5));
#86736=CARTESIAN_POINT('Ctrl Pts',(18.8324695341289,2.5157573223114,48.5));
#86737=CARTESIAN_POINT('Ctrl Pts',(18.8324695341289,2.5157573223114,48.35));
#86738=CARTESIAN_POINT('Ctrl Pts',(18.9592772237957,2.38444769382477,48.5));
#86739=CARTESIAN_POINT('Ctrl Pts',(18.9592772237957,2.38444769382477,48.35));
#86740=CARTESIAN_POINT('Ctrl Pts',(19.1453617326915,2.38444769382477,48.5));
#86741=CARTESIAN_POINT('Ctrl Pts',(19.1453617326915,2.38444769382477,48.35));
#86742=CARTESIAN_POINT('',(18.8324695341289,2.5157573223114,48.5));
#86743=CARTESIAN_POINT('Ctrl Pts',(18.8324695341289,2.5157573223114,48.5));
#86744=CARTESIAN_POINT('Ctrl Pts',(18.9592772237957,2.38444769382477,48.5));
#86745=CARTESIAN_POINT('Ctrl Pts',(19.1453617326915,2.38444769382477,48.5));
#86746=CARTESIAN_POINT('',(18.8324695341289,2.5157573223114,48.35));
#86747=CARTESIAN_POINT('',(18.8324695341289,2.5157573223114,48.5));
#86748=CARTESIAN_POINT('Ctrl Pts',(18.8324695341289,2.5157573223114,48.35));
#86749=CARTESIAN_POINT('Ctrl Pts',(18.9592772237957,2.38444769382477,48.35));
#86750=CARTESIAN_POINT('Ctrl Pts',(19.1453617326915,2.38444769382477,48.35));
#86751=CARTESIAN_POINT('Ctrl Pts',(18.7056618444622,2.85716244578362,48.5));
#86752=CARTESIAN_POINT('Ctrl Pts',(18.7056618444622,2.85716244578362,48.35));
#86753=CARTESIAN_POINT('Ctrl Pts',(18.7056618444622,2.64706695079803,48.5));
#86754=CARTESIAN_POINT('Ctrl Pts',(18.7056618444622,2.64706695079803,48.35));
#86755=CARTESIAN_POINT('Ctrl Pts',(18.8324695341289,2.5157573223114,48.5));
#86756=CARTESIAN_POINT('Ctrl Pts',(18.8324695341289,2.5157573223114,48.35));
#86757=CARTESIAN_POINT('',(18.7056618444622,2.85716244578362,48.5));
#86758=CARTESIAN_POINT('Ctrl Pts',(18.7056618444622,2.85716244578362,48.5));
#86759=CARTESIAN_POINT('Ctrl Pts',(18.7056618444622,2.64706695079803,48.5));
#86760=CARTESIAN_POINT('Ctrl Pts',(18.8324695341289,2.5157573223114,48.5));
#86761=CARTESIAN_POINT('',(18.7056618444622,2.85716244578362,48.35));
#86762=CARTESIAN_POINT('',(18.7056618444622,2.85716244578362,48.5));
#86763=CARTESIAN_POINT('Ctrl Pts',(18.7056618444622,2.85716244578362,48.35));
#86764=CARTESIAN_POINT('Ctrl Pts',(18.7056618444622,2.64706695079803,48.35));
#86765=CARTESIAN_POINT('Ctrl Pts',(18.8324695341289,2.5157573223114,48.35));
#86766=CARTESIAN_POINT('Ctrl Pts',(18.8392224423587,3.23833563923836,48.5));
#86767=CARTESIAN_POINT('Ctrl Pts',(18.8392224423587,3.23833563923836,48.35));
#86768=CARTESIAN_POINT('Ctrl Pts',(18.7056618444622,3.09126877784729,48.5));
#86769=CARTESIAN_POINT('Ctrl Pts',(18.7056618444622,3.09126877784729,48.35));
#86770=CARTESIAN_POINT('Ctrl Pts',(18.7056618444622,2.85716244578362,48.5));
#86771=CARTESIAN_POINT('Ctrl Pts',(18.7056618444622,2.85716244578362,48.35));
#86772=CARTESIAN_POINT('',(18.8392224423587,3.23833563923836,48.5));
#86773=CARTESIAN_POINT('Ctrl Pts',(18.8392224423587,3.23833563923836,48.5));
#86774=CARTESIAN_POINT('Ctrl Pts',(18.7056618444622,3.09126877784729,48.5));
#86775=CARTESIAN_POINT('Ctrl Pts',(18.7056618444622,2.85716244578362,48.5));
#86776=CARTESIAN_POINT('',(18.8392224423587,3.23833563923836,48.35));
#86777=CARTESIAN_POINT('',(18.8392224423587,3.23833563923836,48.5));
#86778=CARTESIAN_POINT('Ctrl Pts',(18.8392224423587,3.23833563923836,48.35));
#86779=CARTESIAN_POINT('Ctrl Pts',(18.7056618444622,3.09126877784729,48.35));
#86780=CARTESIAN_POINT('Ctrl Pts',(18.7056618444622,2.85716244578362,48.35));
#86781=CARTESIAN_POINT('Ctrl Pts',(19.1528650633991,3.38540250062943,48.5));
#86782=CARTESIAN_POINT('Ctrl Pts',(19.1528650633991,3.38540250062943,48.35));
#86783=CARTESIAN_POINT('Ctrl Pts',(18.9727833382785,3.38540250062943,48.5));
#86784=CARTESIAN_POINT('Ctrl Pts',(18.9727833382785,3.38540250062943,48.35));
#86785=CARTESIAN_POINT('Ctrl Pts',(18.8392224423587,3.23833563923836,48.5));
#86786=CARTESIAN_POINT('Ctrl Pts',(18.8392224423587,3.23833563923836,48.35));
#86787=CARTESIAN_POINT('',(19.1528650633991,3.38540250062943,48.5));
#86788=CARTESIAN_POINT('Ctrl Pts',(19.1528650633991,3.38540250062943,48.5));
#86789=CARTESIAN_POINT('Ctrl Pts',(18.9727833382785,3.38540250062943,48.5));
#86790=CARTESIAN_POINT('Ctrl Pts',(18.8392224423587,3.23833563923836,48.5));
#86791=CARTESIAN_POINT('',(19.1528650633991,3.38540250062943,48.35));
#86792=CARTESIAN_POINT('',(19.1528650633991,3.38540250062943,48.5));
#86793=CARTESIAN_POINT('Ctrl Pts',(19.1528650633991,3.38540250062943,48.35));
#86794=CARTESIAN_POINT('Ctrl Pts',(18.9727833382785,3.38540250062943,48.35));
#86795=CARTESIAN_POINT('Ctrl Pts',(18.8392224423587,3.23833563923836,48.35));
#86796=CARTESIAN_POINT('Ctrl Pts',(19.4507506005466,3.24884036183357,48.5));
#86797=CARTESIAN_POINT('Ctrl Pts',(19.4507506005466,3.24884036183357,48.35));
#86798=CARTESIAN_POINT('Ctrl Pts',(19.3269443027675,3.38540250062943,48.5));
#86799=CARTESIAN_POINT('Ctrl Pts',(19.3269443027675,3.38540250062943,48.35));
#86800=CARTESIAN_POINT('Ctrl Pts',(19.1528650633991,3.38540250062943,48.5));
#86801=CARTESIAN_POINT('Ctrl Pts',(19.1528650633991,3.38540250062943,48.35));
#86802=CARTESIAN_POINT('',(19.4507506005466,3.24884036183357,48.5));
#86803=CARTESIAN_POINT('Ctrl Pts',(19.4507506005466,3.24884036183357,48.5));
#86804=CARTESIAN_POINT('Ctrl Pts',(19.3269443027675,3.38540250062943,48.5));
#86805=CARTESIAN_POINT('Ctrl Pts',(19.1528650633991,3.38540250062943,48.5));
#86806=CARTESIAN_POINT('',(19.4507506005466,3.24884036183357,48.35));
#86807=CARTESIAN_POINT('',(19.4507506005466,3.24884036183357,48.5));
#86808=CARTESIAN_POINT('Ctrl Pts',(19.4507506005466,3.24884036183357,48.35));
#86809=CARTESIAN_POINT('Ctrl Pts',(19.3269443027675,3.38540250062943,48.35));
#86810=CARTESIAN_POINT('Ctrl Pts',(19.1528650633991,3.38540250062943,48.35));
#86811=CARTESIAN_POINT('Ctrl Pts',(19.5745566003025,2.87967258691788,48.5));
#86812=CARTESIAN_POINT('Ctrl Pts',(19.5745566003025,2.87967258691788,48.35));
#86813=CARTESIAN_POINT('Ctrl Pts',(19.5745566003025,3.11227837204933,48.5));
#86814=CARTESIAN_POINT('Ctrl Pts',(19.5745566003025,3.11227837204933,48.35));
#86815=CARTESIAN_POINT('Ctrl Pts',(19.4507506005466,3.24884036183357,48.5));
#86816=CARTESIAN_POINT('Ctrl Pts',(19.4507506005466,3.24884036183357,48.35));
#86817=CARTESIAN_POINT('',(19.5745566003025,2.87967258691788,48.5));
#86818=CARTESIAN_POINT('Ctrl Pts',(19.5745566003025,2.87967258691788,48.5));
#86819=CARTESIAN_POINT('Ctrl Pts',(19.5745566003025,3.11227837204933,48.5));
#86820=CARTESIAN_POINT('Ctrl Pts',(19.4507506005466,3.24884036183357,48.5));
#86821=CARTESIAN_POINT('',(19.5745566003025,2.87967258691788,48.35));
#86822=CARTESIAN_POINT('',(19.5745566003025,2.87967258691788,48.5));
#86823=CARTESIAN_POINT('Ctrl Pts',(19.5745566003025,2.87967258691788,48.35));
#86824=CARTESIAN_POINT('Ctrl Pts',(19.5745566003025,3.11227837204933,48.35));
#86825=CARTESIAN_POINT('Ctrl Pts',(19.4507506005466,3.24884036183357,48.35));
#86826=CARTESIAN_POINT('Ctrl Pts',(19.453751694411,2.5157573223114,48.5));
#86827=CARTESIAN_POINT('Ctrl Pts',(19.453751694411,2.5157573223114,48.35));
#86828=CARTESIAN_POINT('Ctrl Pts',(19.5745566003025,2.64706695079803,48.5));
#86829=CARTESIAN_POINT('Ctrl Pts',(19.5745566003025,2.64706695079803,48.35));
#86830=CARTESIAN_POINT('Ctrl Pts',(19.5745566003025,2.87967258691788,48.5));
#86831=CARTESIAN_POINT('Ctrl Pts',(19.5745566003025,2.87967258691788,48.35));
#86832=CARTESIAN_POINT('Ctrl Pts',(19.453751694411,2.5157573223114,48.5));
#86833=CARTESIAN_POINT('Ctrl Pts',(19.5745566003025,2.64706695079803,48.5));
#86834=CARTESIAN_POINT('Ctrl Pts',(19.5745566003025,2.87967258691788,48.5));
#86835=CARTESIAN_POINT('Ctrl Pts',(19.453751694411,2.5157573223114,48.35));
#86836=CARTESIAN_POINT('Ctrl Pts',(19.5745566003025,2.64706695079803,48.35));
#86837=CARTESIAN_POINT('Ctrl Pts',(19.5745566003025,2.87967258691788,48.35));
#86838=CARTESIAN_POINT('Ctrl Pts',(19.0868350379169,1.36248314380646,48.5));
#86839=CARTESIAN_POINT('Ctrl Pts',(19.0868350379169,1.36248314380646,48.35));
#86840=CARTESIAN_POINT('Ctrl Pts',(18.8287177197635,1.36248314380646,48.5));
#86841=CARTESIAN_POINT('Ctrl Pts',(18.8287177197635,1.36248314380646,48.35));
#86842=CARTESIAN_POINT('Ctrl Pts',(18.6651435010135,1.50579804182053,48.5));
#86843=CARTESIAN_POINT('Ctrl Pts',(18.6651435010135,1.50579804182053,48.35));
#86844=CARTESIAN_POINT('',(19.0868350379169,1.36248314380646,48.5));
#86845=CARTESIAN_POINT('',(18.6651435010135,1.50579804182053,48.5));
#86846=CARTESIAN_POINT('Ctrl Pts',(19.0868350379169,1.36248314380646,48.5));
#86847=CARTESIAN_POINT('Ctrl Pts',(18.8287177197635,1.36248314380646,48.5));
#86848=CARTESIAN_POINT('Ctrl Pts',(18.6651435010135,1.50579804182053,48.5));
#86849=CARTESIAN_POINT('',(19.0868350379169,1.36248314380646,48.35));
#86850=CARTESIAN_POINT('',(19.0868350379169,1.36248314380646,48.5));
#86851=CARTESIAN_POINT('',(18.6651435010135,1.50579804182053,48.35));
#86852=CARTESIAN_POINT('Ctrl Pts',(19.0868350379169,1.36248314380646,48.35));
#86853=CARTESIAN_POINT('Ctrl Pts',(18.8287177197635,1.36248314380646,48.35));
#86854=CARTESIAN_POINT('Ctrl Pts',(18.6651435010135,1.50579804182053,48.35));
#86855=CARTESIAN_POINT('',(18.6651435010135,1.50579804182053,48.5));
#86856=CARTESIAN_POINT('Ctrl Pts',(19.5107778422534,1.49304234981537,48.5));
#86857=CARTESIAN_POINT('Ctrl Pts',(19.5107778422534,1.49304234981537,48.35));
#86858=CARTESIAN_POINT('Ctrl Pts',(19.3299455456436,1.36248314380646,48.5));
#86859=CARTESIAN_POINT('Ctrl Pts',(19.3299455456436,1.36248314380646,48.35));
#86860=CARTESIAN_POINT('Ctrl Pts',(19.0868350379169,1.36248314380646,48.5));
#86861=CARTESIAN_POINT('Ctrl Pts',(19.0868350379169,1.36248314380646,48.35));
#86862=CARTESIAN_POINT('',(19.5107778422534,1.49304234981537,48.5));
#86863=CARTESIAN_POINT('Ctrl Pts',(19.5107778422534,1.49304234981537,48.5));
#86864=CARTESIAN_POINT('Ctrl Pts',(19.3299455456436,1.36248314380646,48.5));
#86865=CARTESIAN_POINT('Ctrl Pts',(19.0868350379169,1.36248314380646,48.5));
#86866=CARTESIAN_POINT('',(19.5107778422534,1.49304234981537,48.35));
#86867=CARTESIAN_POINT('',(19.5107778422534,1.49304234981537,48.5));
#86868=CARTESIAN_POINT('Ctrl Pts',(19.5107778422534,1.49304234981537,48.35));
#86869=CARTESIAN_POINT('Ctrl Pts',(19.3299455456436,1.36248314380646,48.35));
#86870=CARTESIAN_POINT('Ctrl Pts',(19.0868350379169,1.36248314380646,48.35));
#86871=CARTESIAN_POINT('Ctrl Pts',(19.7831513993442,1.87346541881561,48.5));
#86872=CARTESIAN_POINT('Ctrl Pts',(19.7831513993442,1.87346541881561,48.35));
#86873=CARTESIAN_POINT('Ctrl Pts',(19.6916099898517,1.6236018538475,48.5));
#86874=CARTESIAN_POINT('Ctrl Pts',(19.6916099898517,1.6236018538475,48.35));
#86875=CARTESIAN_POINT('Ctrl Pts',(19.5107778422534,1.49304234981537,48.5));
#86876=CARTESIAN_POINT('Ctrl Pts',(19.5107778422534,1.49304234981537,48.35));
#86877=CARTESIAN_POINT('',(19.7831513993442,1.87346541881561,48.5));
#86878=CARTESIAN_POINT('Ctrl Pts',(19.7831513993442,1.87346541881561,48.5));
#86879=CARTESIAN_POINT('Ctrl Pts',(19.6916099898517,1.6236018538475,48.5));
#86880=CARTESIAN_POINT('Ctrl Pts',(19.5107778422534,1.49304234981537,48.5));
#86881=CARTESIAN_POINT('',(19.7831513993442,1.87346541881561,48.35));
#86882=CARTESIAN_POINT('',(19.7831513993442,1.87346541881561,48.5));
#86883=CARTESIAN_POINT('Ctrl Pts',(19.7831513993442,1.87346541881561,48.35));
#86884=CARTESIAN_POINT('Ctrl Pts',(19.6916099898517,1.6236018538475,48.35));
#86885=CARTESIAN_POINT('Ctrl Pts',(19.5107778422534,1.49304234981537,48.35));
#86886=CARTESIAN_POINT('Ctrl Pts',(19.8746934048831,2.5450205206871,48.5));
#86887=CARTESIAN_POINT('Ctrl Pts',(19.8746934048831,2.5450205206871,48.35));
#86888=CARTESIAN_POINT('Ctrl Pts',(19.8746934048831,2.12332898378372,48.5));
#86889=CARTESIAN_POINT('Ctrl Pts',(19.8746934048831,2.12332898378372,48.35));
#86890=CARTESIAN_POINT('Ctrl Pts',(19.7831513993442,1.87346541881561,48.5));
#86891=CARTESIAN_POINT('Ctrl Pts',(19.7831513993442,1.87346541881561,48.35));
#86892=CARTESIAN_POINT('',(19.8746934048831,2.5450205206871,48.5));
#86893=CARTESIAN_POINT('Ctrl Pts',(19.8746934048831,2.5450205206871,48.5));
#86894=CARTESIAN_POINT('Ctrl Pts',(19.8746934048831,2.12332898378372,48.5));
#86895=CARTESIAN_POINT('Ctrl Pts',(19.7831513993442,1.87346541881561,48.5));
#86896=CARTESIAN_POINT('',(19.8746934048831,2.5450205206871,48.35));
#86897=CARTESIAN_POINT('',(19.8746934048831,2.5450205206871,48.5));
#86898=CARTESIAN_POINT('Ctrl Pts',(19.8746934048831,2.5450205206871,48.35));
#86899=CARTESIAN_POINT('Ctrl Pts',(19.8746934048831,2.12332898378372,48.35));
#86900=CARTESIAN_POINT('Ctrl Pts',(19.7831513993442,1.87346541881561,48.35));
#86901=CARTESIAN_POINT('Ctrl Pts',(19.7824012748897,3.16405186057091,48.5));
#86902=CARTESIAN_POINT('Ctrl Pts',(19.7824012748897,3.16405186057091,48.35));
#86903=CARTESIAN_POINT('Ctrl Pts',(19.8746934048831,2.95020470023155,48.5));
#86904=CARTESIAN_POINT('Ctrl Pts',(19.8746934048831,2.95020470023155,48.35));
#86905=CARTESIAN_POINT('Ctrl Pts',(19.8746934048831,2.5450205206871,48.5));
#86906=CARTESIAN_POINT('Ctrl Pts',(19.8746934048831,2.5450205206871,48.35));
#86907=CARTESIAN_POINT('',(19.7824012748897,3.16405186057091,48.5));
#86908=CARTESIAN_POINT('Ctrl Pts',(19.7824012748897,3.16405186057091,48.5));
#86909=CARTESIAN_POINT('Ctrl Pts',(19.8746934048831,2.95020470023155,48.5));
#86910=CARTESIAN_POINT('Ctrl Pts',(19.8746934048831,2.5450205206871,48.5));
#86911=CARTESIAN_POINT('',(19.7824012748897,3.16405186057091,48.35));
#86912=CARTESIAN_POINT('',(19.7824012748897,3.16405186057091,48.5));
#86913=CARTESIAN_POINT('Ctrl Pts',(19.7824012748897,3.16405186057091,48.35));
#86914=CARTESIAN_POINT('Ctrl Pts',(19.8746934048831,2.95020470023155,48.35));
#86915=CARTESIAN_POINT('Ctrl Pts',(19.8746934048831,2.5450205206871,48.35));
#86916=CARTESIAN_POINT('Ctrl Pts',(19.5122783891857,3.49345156550407,48.5));
#86917=CARTESIAN_POINT('Ctrl Pts',(19.5122783891857,3.49345156550407,48.35));
#86918=CARTESIAN_POINT('Ctrl Pts',(19.6901091448963,3.37789902091026,48.5));
#86919=CARTESIAN_POINT('Ctrl Pts',(19.6901091448963,3.37789902091026,48.35));
#86920=CARTESIAN_POINT('Ctrl Pts',(19.7824012748897,3.16405186057091,48.5));
#86921=CARTESIAN_POINT('Ctrl Pts',(19.7824012748897,3.16405186057091,48.35));
#86922=CARTESIAN_POINT('',(19.5122783891857,3.49345156550407,48.5));
#86923=CARTESIAN_POINT('Ctrl Pts',(19.5122783891857,3.49345156550407,48.5));
#86924=CARTESIAN_POINT('Ctrl Pts',(19.6901091448963,3.37789902091026,48.5));
#86925=CARTESIAN_POINT('Ctrl Pts',(19.7824012748897,3.16405186057091,48.5));
#86926=CARTESIAN_POINT('',(19.5122783891857,3.49345156550407,48.35));
#86927=CARTESIAN_POINT('',(19.5122783891857,3.49345156550407,48.5));
#86928=CARTESIAN_POINT('Ctrl Pts',(19.5122783891857,3.49345156550407,48.35));
#86929=CARTESIAN_POINT('Ctrl Pts',(19.6901091448963,3.37789902091026,48.35));
#86930=CARTESIAN_POINT('Ctrl Pts',(19.7824012748897,3.16405186057091,48.35));
#86931=CARTESIAN_POINT('Ctrl Pts',(19.119850050658,3.60900411009789,48.5));
#86932=CARTESIAN_POINT('Ctrl Pts',(19.119850050658,3.60900411009789,48.35));
#86933=CARTESIAN_POINT('Ctrl Pts',(19.3344476334751,3.60900411009789,48.5));
#86934=CARTESIAN_POINT('Ctrl Pts',(19.3344476334751,3.60900411009789,48.35));
#86935=CARTESIAN_POINT('Ctrl Pts',(19.5122783891857,3.49345156550407,48.5));
#86936=CARTESIAN_POINT('Ctrl Pts',(19.5122783891857,3.49345156550407,48.35));
#86937=CARTESIAN_POINT('',(19.119850050658,3.60900411009789,48.5));
#86938=CARTESIAN_POINT('Ctrl Pts',(19.119850050658,3.60900411009789,48.5));
#86939=CARTESIAN_POINT('Ctrl Pts',(19.3344476334751,3.60900411009789,48.5));
#86940=CARTESIAN_POINT('Ctrl Pts',(19.5122783891857,3.49345156550407,48.5));
#86941=CARTESIAN_POINT('',(19.119850050658,3.60900411009789,48.35));
#86942=CARTESIAN_POINT('',(19.119850050658,3.60900411009789,48.5));
#86943=CARTESIAN_POINT('Ctrl Pts',(19.119850050658,3.60900411009789,48.35));
#86944=CARTESIAN_POINT('Ctrl Pts',(19.3344476334751,3.60900411009789,48.35));
#86945=CARTESIAN_POINT('Ctrl Pts',(19.5122783891857,3.49345156550407,48.35));
#86946=CARTESIAN_POINT('Ctrl Pts',(18.6253752820194,3.40491139888763,48.5));
#86947=CARTESIAN_POINT('Ctrl Pts',(18.6253752820194,3.40491139888763,48.35));
#86948=CARTESIAN_POINT('Ctrl Pts',(18.8227149359882,3.60900411009789,48.5));
#86949=CARTESIAN_POINT('Ctrl Pts',(18.8227149359882,3.60900411009789,48.35));
#86950=CARTESIAN_POINT('Ctrl Pts',(19.119850050658,3.60900411009789,48.5));
#86951=CARTESIAN_POINT('Ctrl Pts',(19.119850050658,3.60900411009789,48.35));
#86952=CARTESIAN_POINT('',(18.6253752820194,3.40491139888763,48.5));
#86953=CARTESIAN_POINT('Ctrl Pts',(18.6253752820194,3.40491139888763,48.5));
#86954=CARTESIAN_POINT('Ctrl Pts',(18.8227149359882,3.60900411009789,48.5));
#86955=CARTESIAN_POINT('Ctrl Pts',(19.119850050658,3.60900411009789,48.5));
#86956=CARTESIAN_POINT('',(18.6253752820194,3.40491139888763,48.35));
#86957=CARTESIAN_POINT('',(18.6253752820194,3.40491139888763,48.5));
#86958=CARTESIAN_POINT('Ctrl Pts',(18.6253752820194,3.40491139888763,48.35));
#86959=CARTESIAN_POINT('Ctrl Pts',(18.8227149359882,3.60900411009789,48.35));
#86960=CARTESIAN_POINT('Ctrl Pts',(19.119850050658,3.60900411009789,48.35));
#86961=CARTESIAN_POINT('Ctrl Pts',(18.4280356280506,2.866166472435,48.5));
#86962=CARTESIAN_POINT('Ctrl Pts',(18.4280356280506,2.866166472435,48.35));
#86963=CARTESIAN_POINT('Ctrl Pts',(18.4280356280506,3.20081853866577,48.5));
#86964=CARTESIAN_POINT('Ctrl Pts',(18.4280356280506,3.20081853866577,48.35));
#86965=CARTESIAN_POINT('Ctrl Pts',(18.6253752820194,3.40491139888763,48.5));
#86966=CARTESIAN_POINT('Ctrl Pts',(18.6253752820194,3.40491139888763,48.35));
#86967=CARTESIAN_POINT('',(18.4280356280506,2.866166472435,48.5));
#86968=CARTESIAN_POINT('Ctrl Pts',(18.4280356280506,2.866166472435,48.5));
#86969=CARTESIAN_POINT('Ctrl Pts',(18.4280356280506,3.20081853866577,48.5));
#86970=CARTESIAN_POINT('Ctrl Pts',(18.6253752820194,3.40491139888763,48.5));
#86971=CARTESIAN_POINT('',(18.4280356280506,2.866166472435,48.35));
#86972=CARTESIAN_POINT('',(18.4280356280506,2.866166472435,48.5));
#86973=CARTESIAN_POINT('Ctrl Pts',(18.4280356280506,2.866166472435,48.35));
#86974=CARTESIAN_POINT('Ctrl Pts',(18.4280356280506,3.20081853866577,48.35));
#86975=CARTESIAN_POINT('Ctrl Pts',(18.6253752820194,3.40491139888763,48.35));
#86976=CARTESIAN_POINT('Ctrl Pts',(18.6171215288341,2.34392920136452,48.5));
#86977=CARTESIAN_POINT('Ctrl Pts',(18.6171215288341,2.34392920136452,48.35));
#86978=CARTESIAN_POINT('Ctrl Pts',(18.4280356280506,2.54201912879944,48.5));
#86979=CARTESIAN_POINT('Ctrl Pts',(18.4280356280506,2.54201912879944,48.35));
#86980=CARTESIAN_POINT('Ctrl Pts',(18.4280356280506,2.866166472435,48.5));
#86981=CARTESIAN_POINT('Ctrl Pts',(18.4280356280506,2.866166472435,48.35));
#86982=CARTESIAN_POINT('',(18.6171215288341,2.34392920136452,48.5));
#86983=CARTESIAN_POINT('Ctrl Pts',(18.6171215288341,2.34392920136452,48.5));
#86984=CARTESIAN_POINT('Ctrl Pts',(18.4280356280506,2.54201912879944,48.5));
#86985=CARTESIAN_POINT('Ctrl Pts',(18.4280356280506,2.866166472435,48.5));
#86986=CARTESIAN_POINT('',(18.6171215288341,2.34392920136452,48.35));
#86987=CARTESIAN_POINT('',(18.6171215288341,2.34392920136452,48.5));
#86988=CARTESIAN_POINT('Ctrl Pts',(18.6171215288341,2.34392920136452,48.35));
#86989=CARTESIAN_POINT('Ctrl Pts',(18.4280356280506,2.54201912879944,48.35));
#86990=CARTESIAN_POINT('Ctrl Pts',(18.4280356280506,2.866166472435,48.35));
#86991=CARTESIAN_POINT('Ctrl Pts',(19.0793317072093,2.14583912491798,48.5));
#86992=CARTESIAN_POINT('Ctrl Pts',(19.0793317072093,2.14583912491798,48.35));
#86993=CARTESIAN_POINT('Ctrl Pts',(18.8062074296176,2.14583912491798,48.5));
#86994=CARTESIAN_POINT('Ctrl Pts',(18.8062074296176,2.14583912491798,48.35));
#86995=CARTESIAN_POINT('Ctrl Pts',(18.6171215288341,2.34392920136452,48.5));
#86996=CARTESIAN_POINT('Ctrl Pts',(18.6171215288341,2.34392920136452,48.35));
#86997=CARTESIAN_POINT('',(19.0793317072093,2.14583912491798,48.5));
#86998=CARTESIAN_POINT('Ctrl Pts',(19.0793317072093,2.14583912491798,48.5));
#86999=CARTESIAN_POINT('Ctrl Pts',(18.8062074296176,2.14583912491798,48.5));
#87000=CARTESIAN_POINT('Ctrl Pts',(18.6171215288341,2.34392920136452,48.5));
#87001=CARTESIAN_POINT('',(19.0793317072093,2.14583912491798,48.35));
#87002=CARTESIAN_POINT('',(19.0793317072093,2.14583912491798,48.5));
#87003=CARTESIAN_POINT('Ctrl Pts',(19.0793317072093,2.14583912491798,48.35));
#87004=CARTESIAN_POINT('Ctrl Pts',(18.8062074296176,2.14583912491798,48.35));
#87005=CARTESIAN_POINT('Ctrl Pts',(18.6171215288341,2.34392920136452,48.35));
#87006=CARTESIAN_POINT('Ctrl Pts',(19.383219730109,2.22612553834915,48.5));
#87007=CARTESIAN_POINT('Ctrl Pts',(19.383219730109,2.22612553834915,48.35));
#87008=CARTESIAN_POINT('Ctrl Pts',(19.2429059259593,2.14583912491798,48.5));
#87009=CARTESIAN_POINT('Ctrl Pts',(19.2429059259593,2.14583912491798,48.35));
#87010=CARTESIAN_POINT('Ctrl Pts',(19.0793317072093,2.14583912491798,48.5));
#87011=CARTESIAN_POINT('Ctrl Pts',(19.0793317072093,2.14583912491798,48.35));
#87012=CARTESIAN_POINT('',(19.383219730109,2.22612553834915,48.5));
#87013=CARTESIAN_POINT('Ctrl Pts',(19.383219730109,2.22612553834915,48.5));
#87014=CARTESIAN_POINT('Ctrl Pts',(19.2429059259593,2.14583912491798,48.5));
#87015=CARTESIAN_POINT('Ctrl Pts',(19.0793317072093,2.14583912491798,48.5));
#87016=CARTESIAN_POINT('',(19.383219730109,2.22612553834915,48.35));
#87017=CARTESIAN_POINT('',(19.383219730109,2.22612553834915,48.5));
#87018=CARTESIAN_POINT('Ctrl Pts',(19.383219730109,2.22612553834915,48.35));
#87019=CARTESIAN_POINT('Ctrl Pts',(19.2429059259593,2.14583912491798,48.35));
#87020=CARTESIAN_POINT('Ctrl Pts',(19.0793317072093,2.14583912491798,48.35));
#87021=CARTESIAN_POINT('Ctrl Pts',(19.6045705191791,2.43547075986862,48.5));
#87022=CARTESIAN_POINT('Ctrl Pts',(19.6045705191791,2.43547075986862,48.35));
#87023=CARTESIAN_POINT('Ctrl Pts',(19.5235335342586,2.30641210079193,48.5));
#87024=CARTESIAN_POINT('Ctrl Pts',(19.5235335342586,2.30641210079193,48.35));
#87025=CARTESIAN_POINT('Ctrl Pts',(19.383219730109,2.22612553834915,48.5));
#87026=CARTESIAN_POINT('Ctrl Pts',(19.383219730109,2.22612553834915,48.35));
#87027=CARTESIAN_POINT('',(19.6045705191791,2.43547075986862,48.5));
#87028=CARTESIAN_POINT('Ctrl Pts',(19.6045705191791,2.43547075986862,48.5));
#87029=CARTESIAN_POINT('Ctrl Pts',(19.5235335342586,2.30641210079193,48.5));
#87030=CARTESIAN_POINT('Ctrl Pts',(19.383219730109,2.22612553834915,48.5));
#87031=CARTESIAN_POINT('',(19.6045705191791,2.43547075986862,48.35));
#87032=CARTESIAN_POINT('',(19.6045705191791,2.43547075986862,48.5));
#87033=CARTESIAN_POINT('Ctrl Pts',(19.6045705191791,2.43547075986862,48.35));
#87034=CARTESIAN_POINT('Ctrl Pts',(19.5235335342586,2.30641210079193,48.35));
#87035=CARTESIAN_POINT('Ctrl Pts',(19.383219730109,2.22612553834915,48.35));
#87036=CARTESIAN_POINT('Ctrl Pts',(19.6060710661113,2.3814463019371,48.5));
#87037=CARTESIAN_POINT('Ctrl Pts',(19.6060710661113,2.3814463019371,48.35));
#87038=CARTESIAN_POINT('Ctrl Pts',(19.6060710661113,2.39945435523987,48.5));
#87039=CARTESIAN_POINT('Ctrl Pts',(19.6060710661113,2.39945435523987,48.35));
#87040=CARTESIAN_POINT('Ctrl Pts',(19.6045705191791,2.43547075986862,48.5));
#87041=CARTESIAN_POINT('Ctrl Pts',(19.6045705191791,2.43547075986862,48.35));
#87042=CARTESIAN_POINT('',(19.6060710661113,2.3814463019371,48.5));
#87043=CARTESIAN_POINT('Ctrl Pts',(19.6060710661113,2.3814463019371,48.5));
#87044=CARTESIAN_POINT('Ctrl Pts',(19.6060710661113,2.39945435523987,48.5));
#87045=CARTESIAN_POINT('Ctrl Pts',(19.6045705191791,2.43547075986862,48.5));
#87046=CARTESIAN_POINT('',(19.6060710661113,2.3814463019371,48.35));
#87047=CARTESIAN_POINT('',(19.6060710661113,2.3814463019371,48.5));
#87048=CARTESIAN_POINT('Ctrl Pts',(19.6060710661113,2.3814463019371,48.35));
#87049=CARTESIAN_POINT('Ctrl Pts',(19.6060710661113,2.39945435523987,48.35));
#87050=CARTESIAN_POINT('Ctrl Pts',(19.6045705191791,2.43547075986862,48.35));
#87051=CARTESIAN_POINT('Ctrl Pts',(19.5655527226627,2.05129617452621,48.5));
#87052=CARTESIAN_POINT('Ctrl Pts',(19.5655527226627,2.05129617452621,48.35));
#87053=CARTESIAN_POINT('Ctrl Pts',(19.6060710661113,2.21336984634399,48.5));
#87054=CARTESIAN_POINT('Ctrl Pts',(19.6060710661113,2.21336984634399,48.35));
#87055=CARTESIAN_POINT('Ctrl Pts',(19.6060710661113,2.3814463019371,48.5));
#87056=CARTESIAN_POINT('Ctrl Pts',(19.6060710661113,2.3814463019371,48.35));
#87057=CARTESIAN_POINT('',(19.5655527226627,2.05129617452621,48.5));
#87058=CARTESIAN_POINT('Ctrl Pts',(19.5655527226627,2.05129617452621,48.5));
#87059=CARTESIAN_POINT('Ctrl Pts',(19.6060710661113,2.21336984634399,48.5));
#87060=CARTESIAN_POINT('Ctrl Pts',(19.6060710661113,2.3814463019371,48.5));
#87061=CARTESIAN_POINT('',(19.5655527226627,2.05129617452621,48.35));
#87062=CARTESIAN_POINT('',(19.5655527226627,2.05129617452621,48.5));
#87063=CARTESIAN_POINT('Ctrl Pts',(19.5655527226627,2.05129617452621,48.35));
#87064=CARTESIAN_POINT('Ctrl Pts',(19.6060710661113,2.21336984634399,48.35));
#87065=CARTESIAN_POINT('Ctrl Pts',(19.6060710661113,2.3814463019371,48.35));
#87066=CARTESIAN_POINT('Ctrl Pts',(19.465006839484,1.79392898082733,48.5));
#87067=CARTESIAN_POINT('Ctrl Pts',(19.465006839484,1.79392898082733,48.35));
#87068=CARTESIAN_POINT('Ctrl Pts',(19.5250340811908,1.88922250270844,48.5));
#87069=CARTESIAN_POINT('Ctrl Pts',(19.5250340811908,1.88922250270844,48.35));
#87070=CARTESIAN_POINT('Ctrl Pts',(19.5655527226627,2.05129617452621,48.5));
#87071=CARTESIAN_POINT('Ctrl Pts',(19.5655527226627,2.05129617452621,48.35));
#87072=CARTESIAN_POINT('',(19.465006839484,1.79392898082733,48.5));
#87073=CARTESIAN_POINT('Ctrl Pts',(19.465006839484,1.79392898082733,48.5));
#87074=CARTESIAN_POINT('Ctrl Pts',(19.5250340811908,1.88922250270844,48.5));
#87075=CARTESIAN_POINT('Ctrl Pts',(19.5655527226627,2.05129617452621,48.5));
#87076=CARTESIAN_POINT('',(19.465006839484,1.79392898082733,48.35));
#87077=CARTESIAN_POINT('',(19.465006839484,1.79392898082733,48.5));
#87078=CARTESIAN_POINT('Ctrl Pts',(19.465006839484,1.79392898082733,48.35));
#87079=CARTESIAN_POINT('Ctrl Pts',(19.5250340811908,1.88922250270844,48.35));
#87080=CARTESIAN_POINT('Ctrl Pts',(19.5655527226627,2.05129617452621,48.35));
#87081=CARTESIAN_POINT('Ctrl Pts',(19.3111870698631,1.64160990715027,48.5));
#87082=CARTESIAN_POINT('Ctrl Pts',(19.3111870698631,1.64160990715027,48.35));
#87083=CARTESIAN_POINT('Ctrl Pts',(19.4049795977771,1.69863575696945,48.5));
#87084=CARTESIAN_POINT('Ctrl Pts',(19.4049795977771,1.69863575696945,48.35));
#87085=CARTESIAN_POINT('Ctrl Pts',(19.465006839484,1.79392898082733,48.5));
#87086=CARTESIAN_POINT('Ctrl Pts',(19.465006839484,1.79392898082733,48.35));
#87087=CARTESIAN_POINT('',(19.3111870698631,1.64160990715027,48.5));
#87088=CARTESIAN_POINT('Ctrl Pts',(19.3111870698631,1.64160990715027,48.5));
#87089=CARTESIAN_POINT('Ctrl Pts',(19.4049795977771,1.69863575696945,48.5));
#87090=CARTESIAN_POINT('Ctrl Pts',(19.465006839484,1.79392898082733,48.5));
#87091=CARTESIAN_POINT('',(19.3111870698631,1.64160990715027,48.35));
#87092=CARTESIAN_POINT('',(19.3111870698631,1.64160990715027,48.5));
#87093=CARTESIAN_POINT('Ctrl Pts',(19.3111870698631,1.64160990715027,48.35));
#87094=CARTESIAN_POINT('Ctrl Pts',(19.4049795977771,1.69863575696945,48.35));
#87095=CARTESIAN_POINT('Ctrl Pts',(19.465006839484,1.79392898082733,48.35));
#87096=CARTESIAN_POINT('Ctrl Pts',(19.0928378216922,1.58458405733109,48.5));
#87097=CARTESIAN_POINT('Ctrl Pts',(19.0928378216922,1.58458405733109,48.35));
#87098=CARTESIAN_POINT('Ctrl Pts',(19.2173943929374,1.58458405733109,48.5));
#87099=CARTESIAN_POINT('Ctrl Pts',(19.2173943929374,1.58458405733109,48.35));
#87100=CARTESIAN_POINT('Ctrl Pts',(19.3111870698631,1.64160990715027,48.5));
#87101=CARTESIAN_POINT('Ctrl Pts',(19.3111870698631,1.64160990715027,48.35));
#87102=CARTESIAN_POINT('',(19.0928378216922,1.58458405733109,48.5));
#87103=CARTESIAN_POINT('Ctrl Pts',(19.0928378216922,1.58458405733109,48.5));
#87104=CARTESIAN_POINT('Ctrl Pts',(19.2173943929374,1.58458405733109,48.5));
#87105=CARTESIAN_POINT('Ctrl Pts',(19.3111870698631,1.64160990715027,48.5));
#87106=CARTESIAN_POINT('',(19.0928378216922,1.58458405733109,48.35));
#87107=CARTESIAN_POINT('',(19.0928378216922,1.58458405733109,48.5));
#87108=CARTESIAN_POINT('Ctrl Pts',(19.0928378216922,1.58458405733109,48.35));
#87109=CARTESIAN_POINT('Ctrl Pts',(19.2173943929374,1.58458405733109,48.35));
#87110=CARTESIAN_POINT('Ctrl Pts',(19.3111870698631,1.64160990715027,48.35));
#87111=CARTESIAN_POINT('Ctrl Pts',(18.8542294017971,1.66712158918381,48.5));
#87112=CARTESIAN_POINT('Ctrl Pts',(18.8542294017971,1.66712158918381,48.35));
#87113=CARTESIAN_POINT('Ctrl Pts',(18.947271656245,1.58458405733109,48.5));
#87114=CARTESIAN_POINT('Ctrl Pts',(18.947271656245,1.58458405733109,48.35));
#87115=CARTESIAN_POINT('Ctrl Pts',(19.0928378216922,1.58458405733109,48.5));
#87116=CARTESIAN_POINT('Ctrl Pts',(19.0928378216922,1.58458405733109,48.35));
#87117=CARTESIAN_POINT('',(18.8542294017971,1.66712158918381,48.5));
#87118=CARTESIAN_POINT('Ctrl Pts',(18.8542294017971,1.66712158918381,48.5));
#87119=CARTESIAN_POINT('Ctrl Pts',(18.947271656245,1.58458405733109,48.5));
#87120=CARTESIAN_POINT('Ctrl Pts',(19.0928378216922,1.58458405733109,48.5));
#87121=CARTESIAN_POINT('',(18.8542294017971,1.66712158918381,48.35));
#87122=CARTESIAN_POINT('',(18.8542294017971,1.66712158918381,48.5));
#87123=CARTESIAN_POINT('Ctrl Pts',(18.8542294017971,1.66712158918381,48.35));
#87124=CARTESIAN_POINT('Ctrl Pts',(18.947271656245,1.58458405733109,48.35));
#87125=CARTESIAN_POINT('Ctrl Pts',(19.0928378216922,1.58458405733109,48.35));
#87126=CARTESIAN_POINT('Ctrl Pts',(18.728172134608,1.93274223804474,48.5));
#87127=CARTESIAN_POINT('Ctrl Pts',(18.728172134608,1.93274223804474,48.35));
#87128=CARTESIAN_POINT('Ctrl Pts',(18.7611871473491,1.74965912103653,48.5));
#87129=CARTESIAN_POINT('Ctrl Pts',(18.7611871473491,1.74965912103653,48.35));
#87130=CARTESIAN_POINT('Ctrl Pts',(18.8542294017971,1.66712158918381,48.5));
#87131=CARTESIAN_POINT('Ctrl Pts',(18.8542294017971,1.66712158918381,48.35));
#87132=CARTESIAN_POINT('',(18.728172134608,1.93274223804474,48.5));
#87133=CARTESIAN_POINT('Ctrl Pts',(18.728172134608,1.93274223804474,48.5));
#87134=CARTESIAN_POINT('Ctrl Pts',(18.7611871473491,1.74965912103653,48.5));
#87135=CARTESIAN_POINT('Ctrl Pts',(18.8542294017971,1.66712158918381,48.5));
#87136=CARTESIAN_POINT('',(18.728172134608,1.93274223804474,48.35));
#87137=CARTESIAN_POINT('',(18.728172134608,1.93274223804474,48.5));
#87138=CARTESIAN_POINT('Ctrl Pts',(18.728172134608,1.93274223804474,48.35));
#87139=CARTESIAN_POINT('Ctrl Pts',(18.7611871473491,1.74965912103653,48.35));
#87140=CARTESIAN_POINT('Ctrl Pts',(18.8542294017971,1.66712158918381,48.35));
#87141=CARTESIAN_POINT('Origin',(18.4685541205108,1.90873140096664,48.5));
#87142=CARTESIAN_POINT('',(18.4685541205108,1.90873140096664,48.5));
#87143=CARTESIAN_POINT('',(9.5918801338843,1.08776998336471,48.5));
#87144=CARTESIAN_POINT('',(18.4685541205108,1.90873140096664,48.35));
#87145=CARTESIAN_POINT('',(18.4685541205108,1.90873140096664,48.5));
#87146=CARTESIAN_POINT('',(18.4685541205108,1.90873140096664,48.35));
#87147=CARTESIAN_POINT('Ctrl Pts',(18.6651435010135,1.50579804182053,48.5));
#87148=CARTESIAN_POINT('Ctrl Pts',(18.6651435010135,1.50579804182053,48.35));
#87149=CARTESIAN_POINT('Ctrl Pts',(18.5015691332519,1.64911323785782,48.5));
#87150=CARTESIAN_POINT('Ctrl Pts',(18.5015691332519,1.64911323785782,48.35));
#87151=CARTESIAN_POINT('Ctrl Pts',(18.4685541205108,1.90873140096664,48.5));
#87152=CARTESIAN_POINT('Ctrl Pts',(18.4685541205108,1.90873140096664,48.35));
#87153=CARTESIAN_POINT('Ctrl Pts',(18.6651435010135,1.50579804182053,48.5));
#87154=CARTESIAN_POINT('Ctrl Pts',(18.5015691332519,1.64911323785782,48.5));
#87155=CARTESIAN_POINT('Ctrl Pts',(18.4685541205108,1.90873140096664,48.5));
#87156=CARTESIAN_POINT('Ctrl Pts',(18.6651435010135,1.50579804182053,48.35));
#87157=CARTESIAN_POINT('Ctrl Pts',(18.5015691332519,1.64911323785782,48.35));
#87158=CARTESIAN_POINT('Ctrl Pts',(18.4685541205108,1.90873140096664,48.35));
#87159=CARTESIAN_POINT('Origin',(19.9999999515712,2.48574362695217,48.35));
#87160=CARTESIAN_POINT('Origin',(0.,8.,48.5));
#87161=CARTESIAN_POINT('Origin',(0.,8.,48.5));
#87162=CARTESIAN_POINT('Origin',(199.1,6.,48.5));
#87163=CARTESIAN_POINT('',(199.1,6.,48.5));
#87164=CARTESIAN_POINT('',(198.9,6.,48.5));
#87165=CARTESIAN_POINT('',(99.55,6.,48.5));
#87166=CARTESIAN_POINT('',(199.1,6.,48.35));
#87167=CARTESIAN_POINT('',(199.1,6.,48.5));
#87168=CARTESIAN_POINT('',(198.9,6.,48.35));
#87169=CARTESIAN_POINT('',(198.9,6.,48.35));
#87170=CARTESIAN_POINT('',(198.9,6.,48.5));
#87171=CARTESIAN_POINT('Origin',(199.1,7.4,48.5));
#87172=CARTESIAN_POINT('',(199.1,7.4,48.5));
#87173=CARTESIAN_POINT('',(199.1,7.7,48.5));
#87174=CARTESIAN_POINT('',(199.1,7.4,48.35));
#87175=CARTESIAN_POINT('',(199.1,7.4,48.5));
#87176=CARTESIAN_POINT('',(199.1,6.,48.35));
#87177=CARTESIAN_POINT('Origin',(198.9,7.4,48.5));
#87178=CARTESIAN_POINT('',(198.9,7.4,48.5));
#87179=CARTESIAN_POINT('',(99.45,7.4,48.5));
#87180=CARTESIAN_POINT('',(198.9,7.4,48.35));
#87181=CARTESIAN_POINT('',(198.9,7.4,48.5));
#87182=CARTESIAN_POINT('',(199.1,7.4,48.35));
#87183=CARTESIAN_POINT('Origin',(198.9,6.,48.5));
#87184=CARTESIAN_POINT('',(198.9,7.,48.5));
#87185=CARTESIAN_POINT('',(198.9,7.4,48.35));
#87186=CARTESIAN_POINT('Origin',(199.,6.7,48.35));
#87187=CARTESIAN_POINT('Origin',(197.1,6.,48.5));
#87188=CARTESIAN_POINT('',(197.1,6.,48.5));
#87189=CARTESIAN_POINT('',(196.9,6.,48.5));
#87190=CARTESIAN_POINT('',(98.55,6.,48.5));
#87191=CARTESIAN_POINT('',(197.1,6.,48.35));
#87192=CARTESIAN_POINT('',(197.1,6.,48.5));
#87193=CARTESIAN_POINT('',(196.9,6.,48.35));
#87194=CARTESIAN_POINT('',(196.9,6.,48.35));
#87195=CARTESIAN_POINT('',(196.9,6.,48.5));
#87196=CARTESIAN_POINT('Origin',(197.1,7.4,48.5));
#87197=CARTESIAN_POINT('',(197.1,7.4,48.5));
#87198=CARTESIAN_POINT('',(197.1,7.7,48.5));
#87199=CARTESIAN_POINT('',(197.1,7.4,48.35));
#87200=CARTESIAN_POINT('',(197.1,7.4,48.5));
#87201=CARTESIAN_POINT('',(197.1,6.,48.35));
#87202=CARTESIAN_POINT('Origin',(196.9,7.4,48.5));
#87203=CARTESIAN_POINT('',(196.9,7.4,48.5));
#87204=CARTESIAN_POINT('',(98.45,7.4,48.5));
#87205=CARTESIAN_POINT('',(196.9,7.4,48.35));
#87206=CARTESIAN_POINT('',(196.9,7.4,48.5));
#87207=CARTESIAN_POINT('',(197.1,7.4,48.35));
#87208=CARTESIAN_POINT('Origin',(196.9,6.,48.5));
#87209=CARTESIAN_POINT('',(196.9,7.,48.5));
#87210=CARTESIAN_POINT('',(196.9,7.4,48.35));
#87211=CARTESIAN_POINT('Origin',(197.,6.7,48.35));
#87212=CARTESIAN_POINT('Origin',(195.1,5.2,48.5));
#87213=CARTESIAN_POINT('',(195.1,5.2,48.5));
#87214=CARTESIAN_POINT('',(194.9,5.2,48.5));
#87215=CARTESIAN_POINT('',(97.55,5.2,48.5));
#87216=CARTESIAN_POINT('',(195.1,5.2,48.35));
#87217=CARTESIAN_POINT('',(195.1,5.2,48.5));
#87218=CARTESIAN_POINT('',(194.9,5.2,48.35));
#87219=CARTESIAN_POINT('',(194.9,5.2,48.35));
#87220=CARTESIAN_POINT('',(194.9,5.2,48.5));
#87221=CARTESIAN_POINT('Origin',(195.1,7.4,48.5));
#87222=CARTESIAN_POINT('',(195.1,7.4,48.5));
#87223=CARTESIAN_POINT('',(195.1,7.7,48.5));
#87224=CARTESIAN_POINT('',(195.1,7.4,48.35));
#87225=CARTESIAN_POINT('',(195.1,7.4,48.5));
#87226=CARTESIAN_POINT('',(195.1,5.2,48.35));
#87227=CARTESIAN_POINT('Origin',(194.9,7.4,48.5));
#87228=CARTESIAN_POINT('',(194.9,7.4,48.5));
#87229=CARTESIAN_POINT('',(97.45,7.4,48.5));
#87230=CARTESIAN_POINT('',(194.9,7.4,48.35));
#87231=CARTESIAN_POINT('',(194.9,7.4,48.5));
#87232=CARTESIAN_POINT('',(195.1,7.4,48.35));
#87233=CARTESIAN_POINT('Origin',(194.9,5.2,48.5));
#87234=CARTESIAN_POINT('',(194.9,6.6,48.5));
#87235=CARTESIAN_POINT('',(194.9,7.4,48.35));
#87236=CARTESIAN_POINT('Origin',(195.,6.3,48.35));
#87237=CARTESIAN_POINT('Origin',(193.1,6.,48.5));
#87238=CARTESIAN_POINT('',(193.1,6.,48.5));
#87239=CARTESIAN_POINT('',(192.9,6.,48.5));
#87240=CARTESIAN_POINT('',(96.55,6.,48.5));
#87241=CARTESIAN_POINT('',(193.1,6.,48.35));
#87242=CARTESIAN_POINT('',(193.1,6.,48.5));
#87243=CARTESIAN_POINT('',(192.9,6.,48.35));
#87244=CARTESIAN_POINT('',(192.9,6.,48.35));
#87245=CARTESIAN_POINT('',(192.9,6.,48.5));
#87246=CARTESIAN_POINT('Origin',(193.1,7.4,48.5));
#87247=CARTESIAN_POINT('',(193.1,7.4,48.5));
#87248=CARTESIAN_POINT('',(193.1,7.7,48.5));
#87249=CARTESIAN_POINT('',(193.1,7.4,48.35));
#87250=CARTESIAN_POINT('',(193.1,7.4,48.5));
#87251=CARTESIAN_POINT('',(193.1,6.,48.35));
#87252=CARTESIAN_POINT('Origin',(192.9,7.4,48.5));
#87253=CARTESIAN_POINT('',(192.9,7.4,48.5));
#87254=CARTESIAN_POINT('',(96.45,7.4,48.5));
#87255=CARTESIAN_POINT('',(192.9,7.4,48.35));
#87256=CARTESIAN_POINT('',(192.9,7.4,48.5));
#87257=CARTESIAN_POINT('',(193.1,7.4,48.35));
#87258=CARTESIAN_POINT('Origin',(192.9,6.,48.5));
#87259=CARTESIAN_POINT('',(192.9,7.,48.5));
#87260=CARTESIAN_POINT('',(192.9,7.4,48.35));
#87261=CARTESIAN_POINT('Origin',(193.,6.7,48.35));
#87262=CARTESIAN_POINT('Origin',(191.1,6.,48.5));
#87263=CARTESIAN_POINT('',(191.1,6.,48.5));
#87264=CARTESIAN_POINT('',(190.9,6.,48.5));
#87265=CARTESIAN_POINT('',(95.55,6.,48.5));
#87266=CARTESIAN_POINT('',(191.1,6.,48.35));
#87267=CARTESIAN_POINT('',(191.1,6.,48.5));
#87268=CARTESIAN_POINT('',(190.9,6.,48.35));
#87269=CARTESIAN_POINT('',(190.9,6.,48.35));
#87270=CARTESIAN_POINT('',(190.9,6.,48.5));
#87271=CARTESIAN_POINT('Origin',(191.1,7.4,48.5));
#87272=CARTESIAN_POINT('',(191.1,7.4,48.5));
#87273=CARTESIAN_POINT('',(191.1,7.7,48.5));
#87274=CARTESIAN_POINT('',(191.1,7.4,48.35));
#87275=CARTESIAN_POINT('',(191.1,7.4,48.5));
#87276=CARTESIAN_POINT('',(191.1,6.,48.35));
#87277=CARTESIAN_POINT('Origin',(190.9,7.4,48.5));
#87278=CARTESIAN_POINT('',(190.9,7.4,48.5));
#87279=CARTESIAN_POINT('',(95.45,7.4,48.5));
#87280=CARTESIAN_POINT('',(190.9,7.4,48.35));
#87281=CARTESIAN_POINT('',(190.9,7.4,48.5));
#87282=CARTESIAN_POINT('',(191.1,7.4,48.35));
#87283=CARTESIAN_POINT('Origin',(190.9,6.,48.5));
#87284=CARTESIAN_POINT('',(190.9,7.,48.5));
#87285=CARTESIAN_POINT('',(190.9,7.4,48.35));
#87286=CARTESIAN_POINT('Origin',(191.,6.7,48.35));
#87287=CARTESIAN_POINT('Origin',(189.1,6.,48.5));
#87288=CARTESIAN_POINT('',(189.1,6.,48.5));
#87289=CARTESIAN_POINT('',(188.9,6.,48.5));
#87290=CARTESIAN_POINT('',(94.55,6.,48.5));
#87291=CARTESIAN_POINT('',(189.1,6.,48.35));
#87292=CARTESIAN_POINT('',(189.1,6.,48.5));
#87293=CARTESIAN_POINT('',(188.9,6.,48.35));
#87294=CARTESIAN_POINT('',(188.9,6.,48.35));
#87295=CARTESIAN_POINT('',(188.9,6.,48.5));
#87296=CARTESIAN_POINT('Origin',(189.1,7.4,48.5));
#87297=CARTESIAN_POINT('',(189.1,7.4,48.5));
#87298=CARTESIAN_POINT('',(189.1,7.7,48.5));
#87299=CARTESIAN_POINT('',(189.1,7.4,48.35));
#87300=CARTESIAN_POINT('',(189.1,7.4,48.5));
#87301=CARTESIAN_POINT('',(189.1,6.,48.35));
#87302=CARTESIAN_POINT('Origin',(188.9,7.4,48.5));
#87303=CARTESIAN_POINT('',(188.9,7.4,48.5));
#87304=CARTESIAN_POINT('',(94.45,7.4,48.5));
#87305=CARTESIAN_POINT('',(188.9,7.4,48.35));
#87306=CARTESIAN_POINT('',(188.9,7.4,48.5));
#87307=CARTESIAN_POINT('',(189.1,7.4,48.35));
#87308=CARTESIAN_POINT('Origin',(188.9,6.,48.5));
#87309=CARTESIAN_POINT('',(188.9,7.,48.5));
#87310=CARTESIAN_POINT('',(188.9,7.4,48.35));
#87311=CARTESIAN_POINT('Origin',(189.,6.7,48.35));
#87312=CARTESIAN_POINT('Origin',(187.1,6.,48.5));
#87313=CARTESIAN_POINT('',(187.1,6.,48.5));
#87314=CARTESIAN_POINT('',(186.9,6.,48.5));
#87315=CARTESIAN_POINT('',(93.55,6.,48.5));
#87316=CARTESIAN_POINT('',(187.1,6.,48.35));
#87317=CARTESIAN_POINT('',(187.1,6.,48.5));
#87318=CARTESIAN_POINT('',(186.9,6.,48.35));
#87319=CARTESIAN_POINT('',(186.9,6.,48.35));
#87320=CARTESIAN_POINT('',(186.9,6.,48.5));
#87321=CARTESIAN_POINT('Origin',(187.1,7.4,48.5));
#87322=CARTESIAN_POINT('',(187.1,7.4,48.5));
#87323=CARTESIAN_POINT('',(187.1,7.7,48.5));
#87324=CARTESIAN_POINT('',(187.1,7.4,48.35));
#87325=CARTESIAN_POINT('',(187.1,7.4,48.5));
#87326=CARTESIAN_POINT('',(187.1,6.,48.35));
#87327=CARTESIAN_POINT('Origin',(186.9,7.4,48.5));
#87328=CARTESIAN_POINT('',(186.9,7.4,48.5));
#87329=CARTESIAN_POINT('',(93.45,7.4,48.5));
#87330=CARTESIAN_POINT('',(186.9,7.4,48.35));
#87331=CARTESIAN_POINT('',(186.9,7.4,48.5));
#87332=CARTESIAN_POINT('',(187.1,7.4,48.35));
#87333=CARTESIAN_POINT('Origin',(186.9,6.,48.5));
#87334=CARTESIAN_POINT('',(186.9,7.,48.5));
#87335=CARTESIAN_POINT('',(186.9,7.4,48.35));
#87336=CARTESIAN_POINT('Origin',(187.,6.7,48.35));
#87337=CARTESIAN_POINT('Origin',(185.1,5.2,48.5));
#87338=CARTESIAN_POINT('',(185.1,5.2,48.5));
#87339=CARTESIAN_POINT('',(184.9,5.2,48.5));
#87340=CARTESIAN_POINT('',(92.55,5.2,48.5));
#87341=CARTESIAN_POINT('',(185.1,5.2,48.35));
#87342=CARTESIAN_POINT('',(185.1,5.2,48.5));
#87343=CARTESIAN_POINT('',(184.9,5.2,48.35));
#87344=CARTESIAN_POINT('',(184.9,5.2,48.35));
#87345=CARTESIAN_POINT('',(184.9,5.2,48.5));
#87346=CARTESIAN_POINT('Origin',(185.1,7.4,48.5));
#87347=CARTESIAN_POINT('',(185.1,7.4,48.5));
#87348=CARTESIAN_POINT('',(185.1,7.7,48.5));
#87349=CARTESIAN_POINT('',(185.1,7.4,48.35));
#87350=CARTESIAN_POINT('',(185.1,7.4,48.5));
#87351=CARTESIAN_POINT('',(185.1,5.2,48.35));
#87352=CARTESIAN_POINT('Origin',(184.9,7.4,48.5));
#87353=CARTESIAN_POINT('',(184.9,7.4,48.5));
#87354=CARTESIAN_POINT('',(92.45,7.4,48.5));
#87355=CARTESIAN_POINT('',(184.9,7.4,48.35));
#87356=CARTESIAN_POINT('',(184.9,7.4,48.5));
#87357=CARTESIAN_POINT('',(185.1,7.4,48.35));
#87358=CARTESIAN_POINT('Origin',(184.9,5.2,48.5));
#87359=CARTESIAN_POINT('',(184.9,6.6,48.5));
#87360=CARTESIAN_POINT('',(184.9,7.4,48.35));
#87361=CARTESIAN_POINT('Origin',(185.,6.3,48.35));
#87362=CARTESIAN_POINT('Origin',(183.1,6.,48.5));
#87363=CARTESIAN_POINT('',(183.1,6.,48.5));
#87364=CARTESIAN_POINT('',(182.9,6.,48.5));
#87365=CARTESIAN_POINT('',(91.55,6.,48.5));
#87366=CARTESIAN_POINT('',(183.1,6.,48.35));
#87367=CARTESIAN_POINT('',(183.1,6.,48.5));
#87368=CARTESIAN_POINT('',(182.9,6.,48.35));
#87369=CARTESIAN_POINT('',(182.9,6.,48.35));
#87370=CARTESIAN_POINT('',(182.9,6.,48.5));
#87371=CARTESIAN_POINT('Origin',(183.1,7.4,48.5));
#87372=CARTESIAN_POINT('',(183.1,7.4,48.5));
#87373=CARTESIAN_POINT('',(183.1,7.7,48.5));
#87374=CARTESIAN_POINT('',(183.1,7.4,48.35));
#87375=CARTESIAN_POINT('',(183.1,7.4,48.5));
#87376=CARTESIAN_POINT('',(183.1,6.,48.35));
#87377=CARTESIAN_POINT('Origin',(182.9,7.4,48.5));
#87378=CARTESIAN_POINT('',(182.9,7.4,48.5));
#87379=CARTESIAN_POINT('',(91.45,7.4,48.5));
#87380=CARTESIAN_POINT('',(182.9,7.4,48.35));
#87381=CARTESIAN_POINT('',(182.9,7.4,48.5));
#87382=CARTESIAN_POINT('',(183.1,7.4,48.35));
#87383=CARTESIAN_POINT('Origin',(182.9,6.,48.5));
#87384=CARTESIAN_POINT('',(182.9,7.,48.5));
#87385=CARTESIAN_POINT('',(182.9,7.4,48.35));
#87386=CARTESIAN_POINT('Origin',(183.,6.7,48.35));
#87387=CARTESIAN_POINT('Origin',(181.1,6.,48.5));
#87388=CARTESIAN_POINT('',(181.1,6.,48.5));
#87389=CARTESIAN_POINT('',(180.9,6.,48.5));
#87390=CARTESIAN_POINT('',(90.55,6.,48.5));
#87391=CARTESIAN_POINT('',(181.1,6.,48.35));
#87392=CARTESIAN_POINT('',(181.1,6.,48.5));
#87393=CARTESIAN_POINT('',(180.9,6.,48.35));
#87394=CARTESIAN_POINT('',(180.9,6.,48.35));
#87395=CARTESIAN_POINT('',(180.9,6.,48.5));
#87396=CARTESIAN_POINT('Origin',(181.1,7.4,48.5));
#87397=CARTESIAN_POINT('',(181.1,7.4,48.5));
#87398=CARTESIAN_POINT('',(181.1,7.7,48.5));
#87399=CARTESIAN_POINT('',(181.1,7.4,48.35));
#87400=CARTESIAN_POINT('',(181.1,7.4,48.5));
#87401=CARTESIAN_POINT('',(181.1,6.,48.35));
#87402=CARTESIAN_POINT('Origin',(180.9,7.4,48.5));
#87403=CARTESIAN_POINT('',(180.9,7.4,48.5));
#87404=CARTESIAN_POINT('',(90.45,7.4,48.5));
#87405=CARTESIAN_POINT('',(180.9,7.4,48.35));
#87406=CARTESIAN_POINT('',(180.9,7.4,48.5));
#87407=CARTESIAN_POINT('',(181.1,7.4,48.35));
#87408=CARTESIAN_POINT('Origin',(180.9,6.,48.5));
#87409=CARTESIAN_POINT('',(180.9,7.,48.5));
#87410=CARTESIAN_POINT('',(180.9,7.4,48.35));
#87411=CARTESIAN_POINT('Origin',(181.,6.7,48.35));
#87412=CARTESIAN_POINT('Origin',(179.1,6.,48.5));
#87413=CARTESIAN_POINT('',(179.1,6.,48.5));
#87414=CARTESIAN_POINT('',(178.9,6.,48.5));
#87415=CARTESIAN_POINT('',(89.55,6.,48.5));
#87416=CARTESIAN_POINT('',(179.1,6.,48.35));
#87417=CARTESIAN_POINT('',(179.1,6.,48.5));
#87418=CARTESIAN_POINT('',(178.9,6.,48.35));
#87419=CARTESIAN_POINT('',(178.9,6.,48.35));
#87420=CARTESIAN_POINT('',(178.9,6.,48.5));
#87421=CARTESIAN_POINT('Origin',(179.1,7.4,48.5));
#87422=CARTESIAN_POINT('',(179.1,7.4,48.5));
#87423=CARTESIAN_POINT('',(179.1,7.7,48.5));
#87424=CARTESIAN_POINT('',(179.1,7.4,48.35));
#87425=CARTESIAN_POINT('',(179.1,7.4,48.5));
#87426=CARTESIAN_POINT('',(179.1,6.,48.35));
#87427=CARTESIAN_POINT('Origin',(178.9,7.4,48.5));
#87428=CARTESIAN_POINT('',(178.9,7.4,48.5));
#87429=CARTESIAN_POINT('',(89.45,7.4,48.5));
#87430=CARTESIAN_POINT('',(178.9,7.4,48.35));
#87431=CARTESIAN_POINT('',(178.9,7.4,48.5));
#87432=CARTESIAN_POINT('',(179.1,7.4,48.35));
#87433=CARTESIAN_POINT('Origin',(178.9,6.,48.5));
#87434=CARTESIAN_POINT('',(178.9,7.,48.5));
#87435=CARTESIAN_POINT('',(178.9,7.4,48.35));
#87436=CARTESIAN_POINT('Origin',(179.,6.7,48.35));
#87437=CARTESIAN_POINT('Origin',(177.1,6.,48.5));
#87438=CARTESIAN_POINT('',(177.1,6.,48.5));
#87439=CARTESIAN_POINT('',(176.9,6.,48.5));
#87440=CARTESIAN_POINT('',(88.55,6.,48.5));
#87441=CARTESIAN_POINT('',(177.1,6.,48.35));
#87442=CARTESIAN_POINT('',(177.1,6.,48.5));
#87443=CARTESIAN_POINT('',(176.9,6.,48.35));
#87444=CARTESIAN_POINT('',(176.9,6.,48.35));
#87445=CARTESIAN_POINT('',(176.9,6.,48.5));
#87446=CARTESIAN_POINT('Origin',(177.1,7.4,48.5));
#87447=CARTESIAN_POINT('',(177.1,7.4,48.5));
#87448=CARTESIAN_POINT('',(177.1,7.7,48.5));
#87449=CARTESIAN_POINT('',(177.1,7.4,48.35));
#87450=CARTESIAN_POINT('',(177.1,7.4,48.5));
#87451=CARTESIAN_POINT('',(177.1,6.,48.35));
#87452=CARTESIAN_POINT('Origin',(176.9,7.4,48.5));
#87453=CARTESIAN_POINT('',(176.9,7.4,48.5));
#87454=CARTESIAN_POINT('',(88.45,7.4,48.5));
#87455=CARTESIAN_POINT('',(176.9,7.4,48.35));
#87456=CARTESIAN_POINT('',(176.9,7.4,48.5));
#87457=CARTESIAN_POINT('',(177.1,7.4,48.35));
#87458=CARTESIAN_POINT('Origin',(176.9,6.,48.5));
#87459=CARTESIAN_POINT('',(176.9,7.,48.5));
#87460=CARTESIAN_POINT('',(176.9,7.4,48.35));
#87461=CARTESIAN_POINT('Origin',(177.,6.7,48.35));
#87462=CARTESIAN_POINT('Origin',(175.1,5.2,48.5));
#87463=CARTESIAN_POINT('',(175.1,5.2,48.5));
#87464=CARTESIAN_POINT('',(174.9,5.2,48.5));
#87465=CARTESIAN_POINT('',(87.55,5.2,48.5));
#87466=CARTESIAN_POINT('',(175.1,5.2,48.35));
#87467=CARTESIAN_POINT('',(175.1,5.2,48.5));
#87468=CARTESIAN_POINT('',(174.9,5.2,48.35));
#87469=CARTESIAN_POINT('',(174.9,5.2,48.35));
#87470=CARTESIAN_POINT('',(174.9,5.2,48.5));
#87471=CARTESIAN_POINT('Origin',(175.1,7.4,48.5));
#87472=CARTESIAN_POINT('',(175.1,7.4,48.5));
#87473=CARTESIAN_POINT('',(175.1,7.7,48.5));
#87474=CARTESIAN_POINT('',(175.1,7.4,48.35));
#87475=CARTESIAN_POINT('',(175.1,7.4,48.5));
#87476=CARTESIAN_POINT('',(175.1,5.2,48.35));
#87477=CARTESIAN_POINT('Origin',(174.9,7.4,48.5));
#87478=CARTESIAN_POINT('',(174.9,7.4,48.5));
#87479=CARTESIAN_POINT('',(87.45,7.4,48.5));
#87480=CARTESIAN_POINT('',(174.9,7.4,48.35));
#87481=CARTESIAN_POINT('',(174.9,7.4,48.5));
#87482=CARTESIAN_POINT('',(175.1,7.4,48.35));
#87483=CARTESIAN_POINT('Origin',(174.9,5.2,48.5));
#87484=CARTESIAN_POINT('',(174.9,6.6,48.5));
#87485=CARTESIAN_POINT('',(174.9,7.4,48.35));
#87486=CARTESIAN_POINT('Origin',(175.,6.3,48.35));
#87487=CARTESIAN_POINT('Origin',(173.1,6.,48.5));
#87488=CARTESIAN_POINT('',(173.1,6.,48.5));
#87489=CARTESIAN_POINT('',(172.9,6.,48.5));
#87490=CARTESIAN_POINT('',(86.55,6.,48.5));
#87491=CARTESIAN_POINT('',(173.1,6.,48.35));
#87492=CARTESIAN_POINT('',(173.1,6.,48.5));
#87493=CARTESIAN_POINT('',(172.9,6.,48.35));
#87494=CARTESIAN_POINT('',(172.9,6.,48.35));
#87495=CARTESIAN_POINT('',(172.9,6.,48.5));
#87496=CARTESIAN_POINT('Origin',(173.1,7.4,48.5));
#87497=CARTESIAN_POINT('',(173.1,7.4,48.5));
#87498=CARTESIAN_POINT('',(173.1,7.7,48.5));
#87499=CARTESIAN_POINT('',(173.1,7.4,48.35));
#87500=CARTESIAN_POINT('',(173.1,7.4,48.5));
#87501=CARTESIAN_POINT('',(173.1,6.,48.35));
#87502=CARTESIAN_POINT('Origin',(172.9,7.4,48.5));
#87503=CARTESIAN_POINT('',(172.9,7.4,48.5));
#87504=CARTESIAN_POINT('',(86.45,7.4,48.5));
#87505=CARTESIAN_POINT('',(172.9,7.4,48.35));
#87506=CARTESIAN_POINT('',(172.9,7.4,48.5));
#87507=CARTESIAN_POINT('',(173.1,7.4,48.35));
#87508=CARTESIAN_POINT('Origin',(172.9,6.,48.5));
#87509=CARTESIAN_POINT('',(172.9,7.,48.5));
#87510=CARTESIAN_POINT('',(172.9,7.4,48.35));
#87511=CARTESIAN_POINT('Origin',(173.,6.7,48.35));
#87512=CARTESIAN_POINT('Origin',(171.1,6.,48.5));
#87513=CARTESIAN_POINT('',(171.1,6.,48.5));
#87514=CARTESIAN_POINT('',(170.9,6.,48.5));
#87515=CARTESIAN_POINT('',(85.55,6.,48.5));
#87516=CARTESIAN_POINT('',(171.1,6.,48.35));
#87517=CARTESIAN_POINT('',(171.1,6.,48.5));
#87518=CARTESIAN_POINT('',(170.9,6.,48.35));
#87519=CARTESIAN_POINT('',(170.9,6.,48.35));
#87520=CARTESIAN_POINT('',(170.9,6.,48.5));
#87521=CARTESIAN_POINT('Origin',(171.1,7.4,48.5));
#87522=CARTESIAN_POINT('',(171.1,7.4,48.5));
#87523=CARTESIAN_POINT('',(171.1,7.7,48.5));
#87524=CARTESIAN_POINT('',(171.1,7.4,48.35));
#87525=CARTESIAN_POINT('',(171.1,7.4,48.5));
#87526=CARTESIAN_POINT('',(171.1,6.,48.35));
#87527=CARTESIAN_POINT('Origin',(170.9,7.4,48.5));
#87528=CARTESIAN_POINT('',(170.9,7.4,48.5));
#87529=CARTESIAN_POINT('',(85.45,7.4,48.5));
#87530=CARTESIAN_POINT('',(170.9,7.4,48.35));
#87531=CARTESIAN_POINT('',(170.9,7.4,48.5));
#87532=CARTESIAN_POINT('',(171.1,7.4,48.35));
#87533=CARTESIAN_POINT('Origin',(170.9,6.,48.5));
#87534=CARTESIAN_POINT('',(170.9,7.,48.5));
#87535=CARTESIAN_POINT('',(170.9,7.4,48.35));
#87536=CARTESIAN_POINT('Origin',(171.,6.7,48.35));
#87537=CARTESIAN_POINT('Origin',(169.1,6.,48.5));
#87538=CARTESIAN_POINT('',(169.1,6.,48.5));
#87539=CARTESIAN_POINT('',(168.9,6.,48.5));
#87540=CARTESIAN_POINT('',(84.55,6.,48.5));
#87541=CARTESIAN_POINT('',(169.1,6.,48.35));
#87542=CARTESIAN_POINT('',(169.1,6.,48.5));
#87543=CARTESIAN_POINT('',(168.9,6.,48.35));
#87544=CARTESIAN_POINT('',(168.9,6.,48.35));
#87545=CARTESIAN_POINT('',(168.9,6.,48.5));
#87546=CARTESIAN_POINT('Origin',(169.1,7.4,48.5));
#87547=CARTESIAN_POINT('',(169.1,7.4,48.5));
#87548=CARTESIAN_POINT('',(169.1,7.7,48.5));
#87549=CARTESIAN_POINT('',(169.1,7.4,48.35));
#87550=CARTESIAN_POINT('',(169.1,7.4,48.5));
#87551=CARTESIAN_POINT('',(169.1,6.,48.35));
#87552=CARTESIAN_POINT('Origin',(168.9,7.4,48.5));
#87553=CARTESIAN_POINT('',(168.9,7.4,48.5));
#87554=CARTESIAN_POINT('',(84.45,7.4,48.5));
#87555=CARTESIAN_POINT('',(168.9,7.4,48.35));
#87556=CARTESIAN_POINT('',(168.9,7.4,48.5));
#87557=CARTESIAN_POINT('',(169.1,7.4,48.35));
#87558=CARTESIAN_POINT('Origin',(168.9,6.,48.5));
#87559=CARTESIAN_POINT('',(168.9,7.,48.5));
#87560=CARTESIAN_POINT('',(168.9,7.4,48.35));
#87561=CARTESIAN_POINT('Origin',(169.,6.7,48.35));
#87562=CARTESIAN_POINT('Origin',(167.1,6.,48.5));
#87563=CARTESIAN_POINT('',(167.1,6.,48.5));
#87564=CARTESIAN_POINT('',(166.9,6.,48.5));
#87565=CARTESIAN_POINT('',(83.55,6.,48.5));
#87566=CARTESIAN_POINT('',(167.1,6.,48.35));
#87567=CARTESIAN_POINT('',(167.1,6.,48.5));
#87568=CARTESIAN_POINT('',(166.9,6.,48.35));
#87569=CARTESIAN_POINT('',(166.9,6.,48.35));
#87570=CARTESIAN_POINT('',(166.9,6.,48.5));
#87571=CARTESIAN_POINT('Origin',(167.1,7.4,48.5));
#87572=CARTESIAN_POINT('',(167.1,7.4,48.5));
#87573=CARTESIAN_POINT('',(167.1,7.7,48.5));
#87574=CARTESIAN_POINT('',(167.1,7.4,48.35));
#87575=CARTESIAN_POINT('',(167.1,7.4,48.5));
#87576=CARTESIAN_POINT('',(167.1,6.,48.35));
#87577=CARTESIAN_POINT('Origin',(166.9,7.4,48.5));
#87578=CARTESIAN_POINT('',(166.9,7.4,48.5));
#87579=CARTESIAN_POINT('',(83.45,7.4,48.5));
#87580=CARTESIAN_POINT('',(166.9,7.4,48.35));
#87581=CARTESIAN_POINT('',(166.9,7.4,48.5));
#87582=CARTESIAN_POINT('',(167.1,7.4,48.35));
#87583=CARTESIAN_POINT('Origin',(166.9,6.,48.5));
#87584=CARTESIAN_POINT('',(166.9,7.,48.5));
#87585=CARTESIAN_POINT('',(166.9,7.4,48.35));
#87586=CARTESIAN_POINT('Origin',(167.,6.7,48.35));
#87587=CARTESIAN_POINT('Origin',(165.1,5.2,48.5));
#87588=CARTESIAN_POINT('',(165.1,5.2,48.5));
#87589=CARTESIAN_POINT('',(164.9,5.2,48.5));
#87590=CARTESIAN_POINT('',(82.55,5.2,48.5));
#87591=CARTESIAN_POINT('',(165.1,5.2,48.35));
#87592=CARTESIAN_POINT('',(165.1,5.2,48.5));
#87593=CARTESIAN_POINT('',(164.9,5.2,48.35));
#87594=CARTESIAN_POINT('',(164.9,5.2,48.35));
#87595=CARTESIAN_POINT('',(164.9,5.2,48.5));
#87596=CARTESIAN_POINT('Origin',(165.1,7.4,48.5));
#87597=CARTESIAN_POINT('',(165.1,7.4,48.5));
#87598=CARTESIAN_POINT('',(165.1,7.7,48.5));
#87599=CARTESIAN_POINT('',(165.1,7.4,48.35));
#87600=CARTESIAN_POINT('',(165.1,7.4,48.5));
#87601=CARTESIAN_POINT('',(165.1,5.2,48.35));
#87602=CARTESIAN_POINT('Origin',(164.9,7.4,48.5));
#87603=CARTESIAN_POINT('',(164.9,7.4,48.5));
#87604=CARTESIAN_POINT('',(82.45,7.4,48.5));
#87605=CARTESIAN_POINT('',(164.9,7.4,48.35));
#87606=CARTESIAN_POINT('',(164.9,7.4,48.5));
#87607=CARTESIAN_POINT('',(165.1,7.4,48.35));
#87608=CARTESIAN_POINT('Origin',(164.9,5.2,48.5));
#87609=CARTESIAN_POINT('',(164.9,6.6,48.5));
#87610=CARTESIAN_POINT('',(164.9,7.4,48.35));
#87611=CARTESIAN_POINT('Origin',(165.,6.3,48.35));
#87612=CARTESIAN_POINT('Origin',(163.1,6.,48.5));
#87613=CARTESIAN_POINT('',(163.1,6.,48.5));
#87614=CARTESIAN_POINT('',(162.9,6.,48.5));
#87615=CARTESIAN_POINT('',(81.55,6.,48.5));
#87616=CARTESIAN_POINT('',(163.1,6.,48.35));
#87617=CARTESIAN_POINT('',(163.1,6.,48.5));
#87618=CARTESIAN_POINT('',(162.9,6.,48.35));
#87619=CARTESIAN_POINT('',(162.9,6.,48.35));
#87620=CARTESIAN_POINT('',(162.9,6.,48.5));
#87621=CARTESIAN_POINT('Origin',(163.1,7.4,48.5));
#87622=CARTESIAN_POINT('',(163.1,7.4,48.5));
#87623=CARTESIAN_POINT('',(163.1,7.7,48.5));
#87624=CARTESIAN_POINT('',(163.1,7.4,48.35));
#87625=CARTESIAN_POINT('',(163.1,7.4,48.5));
#87626=CARTESIAN_POINT('',(163.1,6.,48.35));
#87627=CARTESIAN_POINT('Origin',(162.9,7.4,48.5));
#87628=CARTESIAN_POINT('',(162.9,7.4,48.5));
#87629=CARTESIAN_POINT('',(81.45,7.4,48.5));
#87630=CARTESIAN_POINT('',(162.9,7.4,48.35));
#87631=CARTESIAN_POINT('',(162.9,7.4,48.5));
#87632=CARTESIAN_POINT('',(163.1,7.4,48.35));
#87633=CARTESIAN_POINT('Origin',(162.9,6.,48.5));
#87634=CARTESIAN_POINT('',(162.9,7.,48.5));
#87635=CARTESIAN_POINT('',(162.9,7.4,48.35));
#87636=CARTESIAN_POINT('Origin',(163.,6.7,48.35));
#87637=CARTESIAN_POINT('Origin',(161.1,6.,48.5));
#87638=CARTESIAN_POINT('',(161.1,6.,48.5));
#87639=CARTESIAN_POINT('',(160.9,6.,48.5));
#87640=CARTESIAN_POINT('',(80.55,6.,48.5));
#87641=CARTESIAN_POINT('',(161.1,6.,48.35));
#87642=CARTESIAN_POINT('',(161.1,6.,48.5));
#87643=CARTESIAN_POINT('',(160.9,6.,48.35));
#87644=CARTESIAN_POINT('',(160.9,6.,48.35));
#87645=CARTESIAN_POINT('',(160.9,6.,48.5));
#87646=CARTESIAN_POINT('Origin',(161.1,7.4,48.5));
#87647=CARTESIAN_POINT('',(161.1,7.4,48.5));
#87648=CARTESIAN_POINT('',(161.1,7.7,48.5));
#87649=CARTESIAN_POINT('',(161.1,7.4,48.35));
#87650=CARTESIAN_POINT('',(161.1,7.4,48.5));
#87651=CARTESIAN_POINT('',(161.1,6.,48.35));
#87652=CARTESIAN_POINT('Origin',(160.9,7.4,48.5));
#87653=CARTESIAN_POINT('',(160.9,7.4,48.5));
#87654=CARTESIAN_POINT('',(80.45,7.4,48.5));
#87655=CARTESIAN_POINT('',(160.9,7.4,48.35));
#87656=CARTESIAN_POINT('',(160.9,7.4,48.5));
#87657=CARTESIAN_POINT('',(161.1,7.4,48.35));
#87658=CARTESIAN_POINT('Origin',(160.9,6.,48.5));
#87659=CARTESIAN_POINT('',(160.9,7.,48.5));
#87660=CARTESIAN_POINT('',(160.9,7.4,48.35));
#87661=CARTESIAN_POINT('Origin',(161.,6.7,48.35));
#87662=CARTESIAN_POINT('Origin',(159.1,6.,48.5));
#87663=CARTESIAN_POINT('',(159.1,6.,48.5));
#87664=CARTESIAN_POINT('',(158.9,6.,48.5));
#87665=CARTESIAN_POINT('',(79.55,6.,48.5));
#87666=CARTESIAN_POINT('',(159.1,6.,48.35));
#87667=CARTESIAN_POINT('',(159.1,6.,48.5));
#87668=CARTESIAN_POINT('',(158.9,6.,48.35));
#87669=CARTESIAN_POINT('',(158.9,6.,48.35));
#87670=CARTESIAN_POINT('',(158.9,6.,48.5));
#87671=CARTESIAN_POINT('Origin',(159.1,7.4,48.5));
#87672=CARTESIAN_POINT('',(159.1,7.4,48.5));
#87673=CARTESIAN_POINT('',(159.1,7.7,48.5));
#87674=CARTESIAN_POINT('',(159.1,7.4,48.35));
#87675=CARTESIAN_POINT('',(159.1,7.4,48.5));
#87676=CARTESIAN_POINT('',(159.1,6.,48.35));
#87677=CARTESIAN_POINT('Origin',(158.9,7.4,48.5));
#87678=CARTESIAN_POINT('',(158.9,7.4,48.5));
#87679=CARTESIAN_POINT('',(79.45,7.4,48.5));
#87680=CARTESIAN_POINT('',(158.9,7.4,48.35));
#87681=CARTESIAN_POINT('',(158.9,7.4,48.5));
#87682=CARTESIAN_POINT('',(159.1,7.4,48.35));
#87683=CARTESIAN_POINT('Origin',(158.9,6.,48.5));
#87684=CARTESIAN_POINT('',(158.9,7.,48.5));
#87685=CARTESIAN_POINT('',(158.9,7.4,48.35));
#87686=CARTESIAN_POINT('Origin',(159.,6.7,48.35));
#87687=CARTESIAN_POINT('Origin',(157.1,6.,48.5));
#87688=CARTESIAN_POINT('',(157.1,6.,48.5));
#87689=CARTESIAN_POINT('',(156.9,6.,48.5));
#87690=CARTESIAN_POINT('',(78.55,6.,48.5));
#87691=CARTESIAN_POINT('',(157.1,6.,48.35));
#87692=CARTESIAN_POINT('',(157.1,6.,48.5));
#87693=CARTESIAN_POINT('',(156.9,6.,48.35));
#87694=CARTESIAN_POINT('',(156.9,6.,48.35));
#87695=CARTESIAN_POINT('',(156.9,6.,48.5));
#87696=CARTESIAN_POINT('Origin',(157.1,7.4,48.5));
#87697=CARTESIAN_POINT('',(157.1,7.4,48.5));
#87698=CARTESIAN_POINT('',(157.1,7.7,48.5));
#87699=CARTESIAN_POINT('',(157.1,7.4,48.35));
#87700=CARTESIAN_POINT('',(157.1,7.4,48.5));
#87701=CARTESIAN_POINT('',(157.1,6.,48.35));
#87702=CARTESIAN_POINT('Origin',(156.9,7.4,48.5));
#87703=CARTESIAN_POINT('',(156.9,7.4,48.5));
#87704=CARTESIAN_POINT('',(78.45,7.4,48.5));
#87705=CARTESIAN_POINT('',(156.9,7.4,48.35));
#87706=CARTESIAN_POINT('',(156.9,7.4,48.5));
#87707=CARTESIAN_POINT('',(157.1,7.4,48.35));
#87708=CARTESIAN_POINT('Origin',(156.9,6.,48.5));
#87709=CARTESIAN_POINT('',(156.9,7.,48.5));
#87710=CARTESIAN_POINT('',(156.9,7.4,48.35));
#87711=CARTESIAN_POINT('Origin',(157.,6.7,48.35));
#87712=CARTESIAN_POINT('Origin',(155.1,5.2,48.5));
#87713=CARTESIAN_POINT('',(155.1,5.2,48.5));
#87714=CARTESIAN_POINT('',(154.9,5.2,48.5));
#87715=CARTESIAN_POINT('',(77.55,5.2,48.5));
#87716=CARTESIAN_POINT('',(155.1,5.2,48.35));
#87717=CARTESIAN_POINT('',(155.1,5.2,48.5));
#87718=CARTESIAN_POINT('',(154.9,5.2,48.35));
#87719=CARTESIAN_POINT('',(154.9,5.2,48.35));
#87720=CARTESIAN_POINT('',(154.9,5.2,48.5));
#87721=CARTESIAN_POINT('Origin',(155.1,7.4,48.5));
#87722=CARTESIAN_POINT('',(155.1,7.4,48.5));
#87723=CARTESIAN_POINT('',(155.1,7.7,48.5));
#87724=CARTESIAN_POINT('',(155.1,7.4,48.35));
#87725=CARTESIAN_POINT('',(155.1,7.4,48.5));
#87726=CARTESIAN_POINT('',(155.1,5.2,48.35));
#87727=CARTESIAN_POINT('Origin',(154.9,7.4,48.5));
#87728=CARTESIAN_POINT('',(154.9,7.4,48.5));
#87729=CARTESIAN_POINT('',(77.45,7.4,48.5));
#87730=CARTESIAN_POINT('',(154.9,7.4,48.35));
#87731=CARTESIAN_POINT('',(154.9,7.4,48.5));
#87732=CARTESIAN_POINT('',(155.1,7.4,48.35));
#87733=CARTESIAN_POINT('Origin',(154.9,5.2,48.5));
#87734=CARTESIAN_POINT('',(154.9,6.6,48.5));
#87735=CARTESIAN_POINT('',(154.9,7.4,48.35));
#87736=CARTESIAN_POINT('Origin',(155.,6.3,48.35));
#87737=CARTESIAN_POINT('Origin',(153.1,6.,48.5));
#87738=CARTESIAN_POINT('',(153.1,6.,48.5));
#87739=CARTESIAN_POINT('',(152.9,6.,48.5));
#87740=CARTESIAN_POINT('',(76.55,6.,48.5));
#87741=CARTESIAN_POINT('',(153.1,6.,48.35));
#87742=CARTESIAN_POINT('',(153.1,6.,48.5));
#87743=CARTESIAN_POINT('',(152.9,6.,48.35));
#87744=CARTESIAN_POINT('',(152.9,6.,48.35));
#87745=CARTESIAN_POINT('',(152.9,6.,48.5));
#87746=CARTESIAN_POINT('Origin',(153.1,7.4,48.5));
#87747=CARTESIAN_POINT('',(153.1,7.4,48.5));
#87748=CARTESIAN_POINT('',(153.1,7.7,48.5));
#87749=CARTESIAN_POINT('',(153.1,7.4,48.35));
#87750=CARTESIAN_POINT('',(153.1,7.4,48.5));
#87751=CARTESIAN_POINT('',(153.1,6.,48.35));
#87752=CARTESIAN_POINT('Origin',(152.9,7.4,48.5));
#87753=CARTESIAN_POINT('',(152.9,7.4,48.5));
#87754=CARTESIAN_POINT('',(76.45,7.4,48.5));
#87755=CARTESIAN_POINT('',(152.9,7.4,48.35));
#87756=CARTESIAN_POINT('',(152.9,7.4,48.5));
#87757=CARTESIAN_POINT('',(153.1,7.4,48.35));
#87758=CARTESIAN_POINT('Origin',(152.9,6.,48.5));
#87759=CARTESIAN_POINT('',(152.9,7.,48.5));
#87760=CARTESIAN_POINT('',(152.9,7.4,48.35));
#87761=CARTESIAN_POINT('Origin',(153.,6.7,48.35));
#87762=CARTESIAN_POINT('Origin',(151.1,6.,48.5));
#87763=CARTESIAN_POINT('',(151.1,6.,48.5));
#87764=CARTESIAN_POINT('',(150.9,6.,48.5));
#87765=CARTESIAN_POINT('',(75.55,6.,48.5));
#87766=CARTESIAN_POINT('',(151.1,6.,48.35));
#87767=CARTESIAN_POINT('',(151.1,6.,48.5));
#87768=CARTESIAN_POINT('',(150.9,6.,48.35));
#87769=CARTESIAN_POINT('',(150.9,6.,48.35));
#87770=CARTESIAN_POINT('',(150.9,6.,48.5));
#87771=CARTESIAN_POINT('Origin',(151.1,7.4,48.5));
#87772=CARTESIAN_POINT('',(151.1,7.4,48.5));
#87773=CARTESIAN_POINT('',(151.1,7.7,48.5));
#87774=CARTESIAN_POINT('',(151.1,7.4,48.35));
#87775=CARTESIAN_POINT('',(151.1,7.4,48.5));
#87776=CARTESIAN_POINT('',(151.1,6.,48.35));
#87777=CARTESIAN_POINT('Origin',(150.9,7.4,48.5));
#87778=CARTESIAN_POINT('',(150.9,7.4,48.5));
#87779=CARTESIAN_POINT('',(75.45,7.4,48.5));
#87780=CARTESIAN_POINT('',(150.9,7.4,48.35));
#87781=CARTESIAN_POINT('',(150.9,7.4,48.5));
#87782=CARTESIAN_POINT('',(151.1,7.4,48.35));
#87783=CARTESIAN_POINT('Origin',(150.9,6.,48.5));
#87784=CARTESIAN_POINT('',(150.9,7.,48.5));
#87785=CARTESIAN_POINT('',(150.9,7.4,48.35));
#87786=CARTESIAN_POINT('Origin',(151.,6.7,48.35));
#87787=CARTESIAN_POINT('Origin',(149.1,6.,48.5));
#87788=CARTESIAN_POINT('',(149.1,6.,48.5));
#87789=CARTESIAN_POINT('',(148.9,6.,48.5));
#87790=CARTESIAN_POINT('',(74.55,6.,48.5));
#87791=CARTESIAN_POINT('',(149.1,6.,48.35));
#87792=CARTESIAN_POINT('',(149.1,6.,48.5));
#87793=CARTESIAN_POINT('',(148.9,6.,48.35));
#87794=CARTESIAN_POINT('',(148.9,6.,48.35));
#87795=CARTESIAN_POINT('',(148.9,6.,48.5));
#87796=CARTESIAN_POINT('Origin',(149.1,7.4,48.5));
#87797=CARTESIAN_POINT('',(149.1,7.4,48.5));
#87798=CARTESIAN_POINT('',(149.1,7.7,48.5));
#87799=CARTESIAN_POINT('',(149.1,7.4,48.35));
#87800=CARTESIAN_POINT('',(149.1,7.4,48.5));
#87801=CARTESIAN_POINT('',(149.1,6.,48.35));
#87802=CARTESIAN_POINT('Origin',(148.9,7.4,48.5));
#87803=CARTESIAN_POINT('',(148.9,7.4,48.5));
#87804=CARTESIAN_POINT('',(74.45,7.4,48.5));
#87805=CARTESIAN_POINT('',(148.9,7.4,48.35));
#87806=CARTESIAN_POINT('',(148.9,7.4,48.5));
#87807=CARTESIAN_POINT('',(149.1,7.4,48.35));
#87808=CARTESIAN_POINT('Origin',(148.9,6.,48.5));
#87809=CARTESIAN_POINT('',(148.9,7.,48.5));
#87810=CARTESIAN_POINT('',(148.9,7.4,48.35));
#87811=CARTESIAN_POINT('Origin',(149.,6.7,48.35));
#87812=CARTESIAN_POINT('Origin',(147.1,6.,48.5));
#87813=CARTESIAN_POINT('',(147.1,6.,48.5));
#87814=CARTESIAN_POINT('',(146.9,6.,48.5));
#87815=CARTESIAN_POINT('',(73.55,6.,48.5));
#87816=CARTESIAN_POINT('',(147.1,6.,48.35));
#87817=CARTESIAN_POINT('',(147.1,6.,48.5));
#87818=CARTESIAN_POINT('',(146.9,6.,48.35));
#87819=CARTESIAN_POINT('',(146.9,6.,48.35));
#87820=CARTESIAN_POINT('',(146.9,6.,48.5));
#87821=CARTESIAN_POINT('Origin',(147.1,7.4,48.5));
#87822=CARTESIAN_POINT('',(147.1,7.4,48.5));
#87823=CARTESIAN_POINT('',(147.1,7.7,48.5));
#87824=CARTESIAN_POINT('',(147.1,7.4,48.35));
#87825=CARTESIAN_POINT('',(147.1,7.4,48.5));
#87826=CARTESIAN_POINT('',(147.1,6.,48.35));
#87827=CARTESIAN_POINT('Origin',(146.9,7.4,48.5));
#87828=CARTESIAN_POINT('',(146.9,7.4,48.5));
#87829=CARTESIAN_POINT('',(73.45,7.4,48.5));
#87830=CARTESIAN_POINT('',(146.9,7.4,48.35));
#87831=CARTESIAN_POINT('',(146.9,7.4,48.5));
#87832=CARTESIAN_POINT('',(147.1,7.4,48.35));
#87833=CARTESIAN_POINT('Origin',(146.9,6.,48.5));
#87834=CARTESIAN_POINT('',(146.9,7.,48.5));
#87835=CARTESIAN_POINT('',(146.9,7.4,48.35));
#87836=CARTESIAN_POINT('Origin',(147.,6.7,48.35));
#87837=CARTESIAN_POINT('Origin',(145.1,5.2,48.5));
#87838=CARTESIAN_POINT('',(145.1,5.2,48.5));
#87839=CARTESIAN_POINT('',(144.9,5.2,48.5));
#87840=CARTESIAN_POINT('',(72.55,5.2,48.5));
#87841=CARTESIAN_POINT('',(145.1,5.2,48.35));
#87842=CARTESIAN_POINT('',(145.1,5.2,48.5));
#87843=CARTESIAN_POINT('',(144.9,5.2,48.35));
#87844=CARTESIAN_POINT('',(144.9,5.2,48.35));
#87845=CARTESIAN_POINT('',(144.9,5.2,48.5));
#87846=CARTESIAN_POINT('Origin',(145.1,7.4,48.5));
#87847=CARTESIAN_POINT('',(145.1,7.4,48.5));
#87848=CARTESIAN_POINT('',(145.1,7.7,48.5));
#87849=CARTESIAN_POINT('',(145.1,7.4,48.35));
#87850=CARTESIAN_POINT('',(145.1,7.4,48.5));
#87851=CARTESIAN_POINT('',(145.1,5.2,48.35));
#87852=CARTESIAN_POINT('Origin',(144.9,7.4,48.5));
#87853=CARTESIAN_POINT('',(144.9,7.4,48.5));
#87854=CARTESIAN_POINT('',(72.45,7.4,48.5));
#87855=CARTESIAN_POINT('',(144.9,7.4,48.35));
#87856=CARTESIAN_POINT('',(144.9,7.4,48.5));
#87857=CARTESIAN_POINT('',(145.1,7.4,48.35));
#87858=CARTESIAN_POINT('Origin',(144.9,5.2,48.5));
#87859=CARTESIAN_POINT('',(144.9,6.6,48.5));
#87860=CARTESIAN_POINT('',(144.9,7.4,48.35));
#87861=CARTESIAN_POINT('Origin',(145.,6.3,48.35));
#87862=CARTESIAN_POINT('Origin',(143.1,6.,48.5));
#87863=CARTESIAN_POINT('',(143.1,6.,48.5));
#87864=CARTESIAN_POINT('',(142.9,6.,48.5));
#87865=CARTESIAN_POINT('',(71.55,6.,48.5));
#87866=CARTESIAN_POINT('',(143.1,6.,48.35));
#87867=CARTESIAN_POINT('',(143.1,6.,48.5));
#87868=CARTESIAN_POINT('',(142.9,6.,48.35));
#87869=CARTESIAN_POINT('',(142.9,6.,48.35));
#87870=CARTESIAN_POINT('',(142.9,6.,48.5));
#87871=CARTESIAN_POINT('Origin',(143.1,7.4,48.5));
#87872=CARTESIAN_POINT('',(143.1,7.4,48.5));
#87873=CARTESIAN_POINT('',(143.1,7.7,48.5));
#87874=CARTESIAN_POINT('',(143.1,7.4,48.35));
#87875=CARTESIAN_POINT('',(143.1,7.4,48.5));
#87876=CARTESIAN_POINT('',(143.1,6.,48.35));
#87877=CARTESIAN_POINT('Origin',(142.9,7.4,48.5));
#87878=CARTESIAN_POINT('',(142.9,7.4,48.5));
#87879=CARTESIAN_POINT('',(71.45,7.4,48.5));
#87880=CARTESIAN_POINT('',(142.9,7.4,48.35));
#87881=CARTESIAN_POINT('',(142.9,7.4,48.5));
#87882=CARTESIAN_POINT('',(143.1,7.4,48.35));
#87883=CARTESIAN_POINT('Origin',(142.9,6.,48.5));
#87884=CARTESIAN_POINT('',(142.9,7.,48.5));
#87885=CARTESIAN_POINT('',(142.9,7.4,48.35));
#87886=CARTESIAN_POINT('Origin',(143.,6.7,48.35));
#87887=CARTESIAN_POINT('Origin',(141.1,6.,48.5));
#87888=CARTESIAN_POINT('',(141.1,6.,48.5));
#87889=CARTESIAN_POINT('',(140.9,6.,48.5));
#87890=CARTESIAN_POINT('',(70.55,6.,48.5));
#87891=CARTESIAN_POINT('',(141.1,6.,48.35));
#87892=CARTESIAN_POINT('',(141.1,6.,48.5));
#87893=CARTESIAN_POINT('',(140.9,6.,48.35));
#87894=CARTESIAN_POINT('',(140.9,6.,48.35));
#87895=CARTESIAN_POINT('',(140.9,6.,48.5));
#87896=CARTESIAN_POINT('Origin',(141.1,7.4,48.5));
#87897=CARTESIAN_POINT('',(141.1,7.4,48.5));
#87898=CARTESIAN_POINT('',(141.1,7.7,48.5));
#87899=CARTESIAN_POINT('',(141.1,7.4,48.35));
#87900=CARTESIAN_POINT('',(141.1,7.4,48.5));
#87901=CARTESIAN_POINT('',(141.1,6.,48.35));
#87902=CARTESIAN_POINT('Origin',(140.9,7.4,48.5));
#87903=CARTESIAN_POINT('',(140.9,7.4,48.5));
#87904=CARTESIAN_POINT('',(70.45,7.4,48.5));
#87905=CARTESIAN_POINT('',(140.9,7.4,48.35));
#87906=CARTESIAN_POINT('',(140.9,7.4,48.5));
#87907=CARTESIAN_POINT('',(141.1,7.4,48.35));
#87908=CARTESIAN_POINT('Origin',(140.9,6.,48.5));
#87909=CARTESIAN_POINT('',(140.9,7.,48.5));
#87910=CARTESIAN_POINT('',(140.9,7.4,48.35));
#87911=CARTESIAN_POINT('Origin',(141.,6.7,48.35));
#87912=CARTESIAN_POINT('Origin',(139.1,6.,48.5));
#87913=CARTESIAN_POINT('',(139.1,6.,48.5));
#87914=CARTESIAN_POINT('',(138.9,6.,48.5));
#87915=CARTESIAN_POINT('',(69.55,6.,48.5));
#87916=CARTESIAN_POINT('',(139.1,6.,48.35));
#87917=CARTESIAN_POINT('',(139.1,6.,48.5));
#87918=CARTESIAN_POINT('',(138.9,6.,48.35));
#87919=CARTESIAN_POINT('',(138.9,6.,48.35));
#87920=CARTESIAN_POINT('',(138.9,6.,48.5));
#87921=CARTESIAN_POINT('Origin',(139.1,7.4,48.5));
#87922=CARTESIAN_POINT('',(139.1,7.4,48.5));
#87923=CARTESIAN_POINT('',(139.1,7.7,48.5));
#87924=CARTESIAN_POINT('',(139.1,7.4,48.35));
#87925=CARTESIAN_POINT('',(139.1,7.4,48.5));
#87926=CARTESIAN_POINT('',(139.1,6.,48.35));
#87927=CARTESIAN_POINT('Origin',(138.9,7.4,48.5));
#87928=CARTESIAN_POINT('',(138.9,7.4,48.5));
#87929=CARTESIAN_POINT('',(69.45,7.4,48.5));
#87930=CARTESIAN_POINT('',(138.9,7.4,48.35));
#87931=CARTESIAN_POINT('',(138.9,7.4,48.5));
#87932=CARTESIAN_POINT('',(139.1,7.4,48.35));
#87933=CARTESIAN_POINT('Origin',(138.9,6.,48.5));
#87934=CARTESIAN_POINT('',(138.9,7.,48.5));
#87935=CARTESIAN_POINT('',(138.9,7.4,48.35));
#87936=CARTESIAN_POINT('Origin',(139.,6.7,48.35));
#87937=CARTESIAN_POINT('Origin',(137.1,6.,48.5));
#87938=CARTESIAN_POINT('',(137.1,6.,48.5));
#87939=CARTESIAN_POINT('',(136.9,6.,48.5));
#87940=CARTESIAN_POINT('',(68.55,6.,48.5));
#87941=CARTESIAN_POINT('',(137.1,6.,48.35));
#87942=CARTESIAN_POINT('',(137.1,6.,48.5));
#87943=CARTESIAN_POINT('',(136.9,6.,48.35));
#87944=CARTESIAN_POINT('',(136.9,6.,48.35));
#87945=CARTESIAN_POINT('',(136.9,6.,48.5));
#87946=CARTESIAN_POINT('Origin',(137.1,7.4,48.5));
#87947=CARTESIAN_POINT('',(137.1,7.4,48.5));
#87948=CARTESIAN_POINT('',(137.1,7.7,48.5));
#87949=CARTESIAN_POINT('',(137.1,7.4,48.35));
#87950=CARTESIAN_POINT('',(137.1,7.4,48.5));
#87951=CARTESIAN_POINT('',(137.1,6.,48.35));
#87952=CARTESIAN_POINT('Origin',(136.9,7.4,48.5));
#87953=CARTESIAN_POINT('',(136.9,7.4,48.5));
#87954=CARTESIAN_POINT('',(68.45,7.4,48.5));
#87955=CARTESIAN_POINT('',(136.9,7.4,48.35));
#87956=CARTESIAN_POINT('',(136.9,7.4,48.5));
#87957=CARTESIAN_POINT('',(137.1,7.4,48.35));
#87958=CARTESIAN_POINT('Origin',(136.9,6.,48.5));
#87959=CARTESIAN_POINT('',(136.9,7.,48.5));
#87960=CARTESIAN_POINT('',(136.9,7.4,48.35));
#87961=CARTESIAN_POINT('Origin',(137.,6.7,48.35));
#87962=CARTESIAN_POINT('Origin',(135.1,5.2,48.5));
#87963=CARTESIAN_POINT('',(135.1,5.2,48.5));
#87964=CARTESIAN_POINT('',(134.9,5.2,48.5));
#87965=CARTESIAN_POINT('',(67.55,5.2,48.5));
#87966=CARTESIAN_POINT('',(135.1,5.2,48.35));
#87967=CARTESIAN_POINT('',(135.1,5.2,48.5));
#87968=CARTESIAN_POINT('',(134.9,5.2,48.35));
#87969=CARTESIAN_POINT('',(134.9,5.2,48.35));
#87970=CARTESIAN_POINT('',(134.9,5.2,48.5));
#87971=CARTESIAN_POINT('Origin',(135.1,7.4,48.5));
#87972=CARTESIAN_POINT('',(135.1,7.4,48.5));
#87973=CARTESIAN_POINT('',(135.1,7.7,48.5));
#87974=CARTESIAN_POINT('',(135.1,7.4,48.35));
#87975=CARTESIAN_POINT('',(135.1,7.4,48.5));
#87976=CARTESIAN_POINT('',(135.1,5.2,48.35));
#87977=CARTESIAN_POINT('Origin',(134.9,7.4,48.5));
#87978=CARTESIAN_POINT('',(134.9,7.4,48.5));
#87979=CARTESIAN_POINT('',(67.45,7.4,48.5));
#87980=CARTESIAN_POINT('',(134.9,7.4,48.35));
#87981=CARTESIAN_POINT('',(134.9,7.4,48.5));
#87982=CARTESIAN_POINT('',(135.1,7.4,48.35));
#87983=CARTESIAN_POINT('Origin',(134.9,5.2,48.5));
#87984=CARTESIAN_POINT('',(134.9,6.6,48.5));
#87985=CARTESIAN_POINT('',(134.9,7.4,48.35));
#87986=CARTESIAN_POINT('Origin',(135.,6.3,48.35));
#87987=CARTESIAN_POINT('Origin',(133.1,6.,48.5));
#87988=CARTESIAN_POINT('',(133.1,6.,48.5));
#87989=CARTESIAN_POINT('',(132.9,6.,48.5));
#87990=CARTESIAN_POINT('',(66.55,6.,48.5));
#87991=CARTESIAN_POINT('',(133.1,6.,48.35));
#87992=CARTESIAN_POINT('',(133.1,6.,48.5));
#87993=CARTESIAN_POINT('',(132.9,6.,48.35));
#87994=CARTESIAN_POINT('',(132.9,6.,48.35));
#87995=CARTESIAN_POINT('',(132.9,6.,48.5));
#87996=CARTESIAN_POINT('Origin',(133.1,7.4,48.5));
#87997=CARTESIAN_POINT('',(133.1,7.4,48.5));
#87998=CARTESIAN_POINT('',(133.1,7.7,48.5));
#87999=CARTESIAN_POINT('',(133.1,7.4,48.35));
#88000=CARTESIAN_POINT('',(133.1,7.4,48.5));
#88001=CARTESIAN_POINT('',(133.1,6.,48.35));
#88002=CARTESIAN_POINT('Origin',(132.9,7.4,48.5));
#88003=CARTESIAN_POINT('',(132.9,7.4,48.5));
#88004=CARTESIAN_POINT('',(66.45,7.4,48.5));
#88005=CARTESIAN_POINT('',(132.9,7.4,48.35));
#88006=CARTESIAN_POINT('',(132.9,7.4,48.5));
#88007=CARTESIAN_POINT('',(133.1,7.4,48.35));
#88008=CARTESIAN_POINT('Origin',(132.9,6.,48.5));
#88009=CARTESIAN_POINT('',(132.9,7.,48.5));
#88010=CARTESIAN_POINT('',(132.9,7.4,48.35));
#88011=CARTESIAN_POINT('Origin',(133.,6.7,48.35));
#88012=CARTESIAN_POINT('Origin',(131.1,6.,48.5));
#88013=CARTESIAN_POINT('',(131.1,6.,48.5));
#88014=CARTESIAN_POINT('',(130.9,6.,48.5));
#88015=CARTESIAN_POINT('',(65.55,6.,48.5));
#88016=CARTESIAN_POINT('',(131.1,6.,48.35));
#88017=CARTESIAN_POINT('',(131.1,6.,48.5));
#88018=CARTESIAN_POINT('',(130.9,6.,48.35));
#88019=CARTESIAN_POINT('',(130.9,6.,48.35));
#88020=CARTESIAN_POINT('',(130.9,6.,48.5));
#88021=CARTESIAN_POINT('Origin',(131.1,7.4,48.5));
#88022=CARTESIAN_POINT('',(131.1,7.4,48.5));
#88023=CARTESIAN_POINT('',(131.1,7.7,48.5));
#88024=CARTESIAN_POINT('',(131.1,7.4,48.35));
#88025=CARTESIAN_POINT('',(131.1,7.4,48.5));
#88026=CARTESIAN_POINT('',(131.1,6.,48.35));
#88027=CARTESIAN_POINT('Origin',(130.9,7.4,48.5));
#88028=CARTESIAN_POINT('',(130.9,7.4,48.5));
#88029=CARTESIAN_POINT('',(65.45,7.4,48.5));
#88030=CARTESIAN_POINT('',(130.9,7.4,48.35));
#88031=CARTESIAN_POINT('',(130.9,7.4,48.5));
#88032=CARTESIAN_POINT('',(131.1,7.4,48.35));
#88033=CARTESIAN_POINT('Origin',(130.9,6.,48.5));
#88034=CARTESIAN_POINT('',(130.9,7.,48.5));
#88035=CARTESIAN_POINT('',(130.9,7.4,48.35));
#88036=CARTESIAN_POINT('Origin',(131.,6.7,48.35));
#88037=CARTESIAN_POINT('Origin',(129.1,6.,48.5));
#88038=CARTESIAN_POINT('',(129.1,6.,48.5));
#88039=CARTESIAN_POINT('',(128.9,6.,48.5));
#88040=CARTESIAN_POINT('',(64.55,6.,48.5));
#88041=CARTESIAN_POINT('',(129.1,6.,48.35));
#88042=CARTESIAN_POINT('',(129.1,6.,48.5));
#88043=CARTESIAN_POINT('',(128.9,6.,48.35));
#88044=CARTESIAN_POINT('',(128.9,6.,48.35));
#88045=CARTESIAN_POINT('',(128.9,6.,48.5));
#88046=CARTESIAN_POINT('Origin',(129.1,7.4,48.5));
#88047=CARTESIAN_POINT('',(129.1,7.4,48.5));
#88048=CARTESIAN_POINT('',(129.1,7.7,48.5));
#88049=CARTESIAN_POINT('',(129.1,7.4,48.35));
#88050=CARTESIAN_POINT('',(129.1,7.4,48.5));
#88051=CARTESIAN_POINT('',(129.1,6.,48.35));
#88052=CARTESIAN_POINT('Origin',(128.9,7.4,48.5));
#88053=CARTESIAN_POINT('',(128.9,7.4,48.5));
#88054=CARTESIAN_POINT('',(64.45,7.4,48.5));
#88055=CARTESIAN_POINT('',(128.9,7.4,48.35));
#88056=CARTESIAN_POINT('',(128.9,7.4,48.5));
#88057=CARTESIAN_POINT('',(129.1,7.4,48.35));
#88058=CARTESIAN_POINT('Origin',(128.9,6.,48.5));
#88059=CARTESIAN_POINT('',(128.9,7.,48.5));
#88060=CARTESIAN_POINT('',(128.9,7.4,48.35));
#88061=CARTESIAN_POINT('Origin',(129.,6.7,48.35));
#88062=CARTESIAN_POINT('Origin',(127.1,6.,48.5));
#88063=CARTESIAN_POINT('',(127.1,6.,48.5));
#88064=CARTESIAN_POINT('',(126.9,6.,48.5));
#88065=CARTESIAN_POINT('',(63.55,6.,48.5));
#88066=CARTESIAN_POINT('',(127.1,6.,48.35));
#88067=CARTESIAN_POINT('',(127.1,6.,48.5));
#88068=CARTESIAN_POINT('',(126.9,6.,48.35));
#88069=CARTESIAN_POINT('',(126.9,6.,48.35));
#88070=CARTESIAN_POINT('',(126.9,6.,48.5));
#88071=CARTESIAN_POINT('Origin',(127.1,7.4,48.5));
#88072=CARTESIAN_POINT('',(127.1,7.4,48.5));
#88073=CARTESIAN_POINT('',(127.1,7.7,48.5));
#88074=CARTESIAN_POINT('',(127.1,7.4,48.35));
#88075=CARTESIAN_POINT('',(127.1,7.4,48.5));
#88076=CARTESIAN_POINT('',(127.1,6.,48.35));
#88077=CARTESIAN_POINT('Origin',(126.9,7.4,48.5));
#88078=CARTESIAN_POINT('',(126.9,7.4,48.5));
#88079=CARTESIAN_POINT('',(63.45,7.4,48.5));
#88080=CARTESIAN_POINT('',(126.9,7.4,48.35));
#88081=CARTESIAN_POINT('',(126.9,7.4,48.5));
#88082=CARTESIAN_POINT('',(127.1,7.4,48.35));
#88083=CARTESIAN_POINT('Origin',(126.9,6.,48.5));
#88084=CARTESIAN_POINT('',(126.9,7.,48.5));
#88085=CARTESIAN_POINT('',(126.9,7.4,48.35));
#88086=CARTESIAN_POINT('Origin',(127.,6.7,48.35));
#88087=CARTESIAN_POINT('Origin',(125.1,5.2,48.5));
#88088=CARTESIAN_POINT('',(125.1,5.2,48.5));
#88089=CARTESIAN_POINT('',(124.9,5.2,48.5));
#88090=CARTESIAN_POINT('',(62.55,5.2,48.5));
#88091=CARTESIAN_POINT('',(125.1,5.2,48.35));
#88092=CARTESIAN_POINT('',(125.1,5.2,48.5));
#88093=CARTESIAN_POINT('',(124.9,5.2,48.35));
#88094=CARTESIAN_POINT('',(124.9,5.2,48.35));
#88095=CARTESIAN_POINT('',(124.9,5.2,48.5));
#88096=CARTESIAN_POINT('Origin',(125.1,7.4,48.5));
#88097=CARTESIAN_POINT('',(125.1,7.4,48.5));
#88098=CARTESIAN_POINT('',(125.1,7.7,48.5));
#88099=CARTESIAN_POINT('',(125.1,7.4,48.35));
#88100=CARTESIAN_POINT('',(125.1,7.4,48.5));
#88101=CARTESIAN_POINT('',(125.1,5.2,48.35));
#88102=CARTESIAN_POINT('Origin',(124.9,7.4,48.5));
#88103=CARTESIAN_POINT('',(124.9,7.4,48.5));
#88104=CARTESIAN_POINT('',(62.45,7.4,48.5));
#88105=CARTESIAN_POINT('',(124.9,7.4,48.35));
#88106=CARTESIAN_POINT('',(124.9,7.4,48.5));
#88107=CARTESIAN_POINT('',(125.1,7.4,48.35));
#88108=CARTESIAN_POINT('Origin',(124.9,5.2,48.5));
#88109=CARTESIAN_POINT('',(124.9,6.6,48.5));
#88110=CARTESIAN_POINT('',(124.9,7.4,48.35));
#88111=CARTESIAN_POINT('Origin',(125.,6.3,48.35));
#88112=CARTESIAN_POINT('Origin',(123.1,6.,48.5));
#88113=CARTESIAN_POINT('',(123.1,6.,48.5));
#88114=CARTESIAN_POINT('',(122.9,6.,48.5));
#88115=CARTESIAN_POINT('',(61.55,6.,48.5));
#88116=CARTESIAN_POINT('',(123.1,6.,48.35));
#88117=CARTESIAN_POINT('',(123.1,6.,48.5));
#88118=CARTESIAN_POINT('',(122.9,6.,48.35));
#88119=CARTESIAN_POINT('',(122.9,6.,48.35));
#88120=CARTESIAN_POINT('',(122.9,6.,48.5));
#88121=CARTESIAN_POINT('Origin',(123.1,7.4,48.5));
#88122=CARTESIAN_POINT('',(123.1,7.4,48.5));
#88123=CARTESIAN_POINT('',(123.1,7.7,48.5));
#88124=CARTESIAN_POINT('',(123.1,7.4,48.35));
#88125=CARTESIAN_POINT('',(123.1,7.4,48.5));
#88126=CARTESIAN_POINT('',(123.1,6.,48.35));
#88127=CARTESIAN_POINT('Origin',(122.9,7.4,48.5));
#88128=CARTESIAN_POINT('',(122.9,7.4,48.5));
#88129=CARTESIAN_POINT('',(61.45,7.4,48.5));
#88130=CARTESIAN_POINT('',(122.9,7.4,48.35));
#88131=CARTESIAN_POINT('',(122.9,7.4,48.5));
#88132=CARTESIAN_POINT('',(123.1,7.4,48.35));
#88133=CARTESIAN_POINT('Origin',(122.9,6.,48.5));
#88134=CARTESIAN_POINT('',(122.9,7.,48.5));
#88135=CARTESIAN_POINT('',(122.9,7.4,48.35));
#88136=CARTESIAN_POINT('Origin',(123.,6.7,48.35));
#88137=CARTESIAN_POINT('Origin',(121.1,6.,48.5));
#88138=CARTESIAN_POINT('',(121.1,6.,48.5));
#88139=CARTESIAN_POINT('',(120.9,6.,48.5));
#88140=CARTESIAN_POINT('',(60.55,6.,48.5));
#88141=CARTESIAN_POINT('',(121.1,6.,48.35));
#88142=CARTESIAN_POINT('',(121.1,6.,48.5));
#88143=CARTESIAN_POINT('',(120.9,6.,48.35));
#88144=CARTESIAN_POINT('',(120.9,6.,48.35));
#88145=CARTESIAN_POINT('',(120.9,6.,48.5));
#88146=CARTESIAN_POINT('Origin',(121.1,7.4,48.5));
#88147=CARTESIAN_POINT('',(121.1,7.4,48.5));
#88148=CARTESIAN_POINT('',(121.1,7.7,48.5));
#88149=CARTESIAN_POINT('',(121.1,7.4,48.35));
#88150=CARTESIAN_POINT('',(121.1,7.4,48.5));
#88151=CARTESIAN_POINT('',(121.1,6.,48.35));
#88152=CARTESIAN_POINT('Origin',(120.9,7.4,48.5));
#88153=CARTESIAN_POINT('',(120.9,7.4,48.5));
#88154=CARTESIAN_POINT('',(60.45,7.4,48.5));
#88155=CARTESIAN_POINT('',(120.9,7.4,48.35));
#88156=CARTESIAN_POINT('',(120.9,7.4,48.5));
#88157=CARTESIAN_POINT('',(121.1,7.4,48.35));
#88158=CARTESIAN_POINT('Origin',(120.9,6.,48.5));
#88159=CARTESIAN_POINT('',(120.9,7.,48.5));
#88160=CARTESIAN_POINT('',(120.9,7.4,48.35));
#88161=CARTESIAN_POINT('Origin',(121.,6.7,48.35));
#88162=CARTESIAN_POINT('Origin',(119.1,6.,48.5));
#88163=CARTESIAN_POINT('',(119.1,6.,48.5));
#88164=CARTESIAN_POINT('',(118.9,6.,48.5));
#88165=CARTESIAN_POINT('',(59.55,6.,48.5));
#88166=CARTESIAN_POINT('',(119.1,6.,48.35));
#88167=CARTESIAN_POINT('',(119.1,6.,48.5));
#88168=CARTESIAN_POINT('',(118.9,6.,48.35));
#88169=CARTESIAN_POINT('',(118.9,6.,48.35));
#88170=CARTESIAN_POINT('',(118.9,6.,48.5));
#88171=CARTESIAN_POINT('Origin',(119.1,7.4,48.5));
#88172=CARTESIAN_POINT('',(119.1,7.4,48.5));
#88173=CARTESIAN_POINT('',(119.1,7.7,48.5));
#88174=CARTESIAN_POINT('',(119.1,7.4,48.35));
#88175=CARTESIAN_POINT('',(119.1,7.4,48.5));
#88176=CARTESIAN_POINT('',(119.1,6.,48.35));
#88177=CARTESIAN_POINT('Origin',(118.9,7.4,48.5));
#88178=CARTESIAN_POINT('',(118.9,7.4,48.5));
#88179=CARTESIAN_POINT('',(59.45,7.4,48.5));
#88180=CARTESIAN_POINT('',(118.9,7.4,48.35));
#88181=CARTESIAN_POINT('',(118.9,7.4,48.5));
#88182=CARTESIAN_POINT('',(119.1,7.4,48.35));
#88183=CARTESIAN_POINT('Origin',(118.9,6.,48.5));
#88184=CARTESIAN_POINT('',(118.9,7.,48.5));
#88185=CARTESIAN_POINT('',(118.9,7.4,48.35));
#88186=CARTESIAN_POINT('Origin',(119.,6.7,48.35));
#88187=CARTESIAN_POINT('Origin',(117.1,6.,48.5));
#88188=CARTESIAN_POINT('',(117.1,6.,48.5));
#88189=CARTESIAN_POINT('',(116.9,6.,48.5));
#88190=CARTESIAN_POINT('',(58.55,6.,48.5));
#88191=CARTESIAN_POINT('',(117.1,6.,48.35));
#88192=CARTESIAN_POINT('',(117.1,6.,48.5));
#88193=CARTESIAN_POINT('',(116.9,6.,48.35));
#88194=CARTESIAN_POINT('',(116.9,6.,48.35));
#88195=CARTESIAN_POINT('',(116.9,6.,48.5));
#88196=CARTESIAN_POINT('Origin',(117.1,7.4,48.5));
#88197=CARTESIAN_POINT('',(117.1,7.4,48.5));
#88198=CARTESIAN_POINT('',(117.1,7.7,48.5));
#88199=CARTESIAN_POINT('',(117.1,7.4,48.35));
#88200=CARTESIAN_POINT('',(117.1,7.4,48.5));
#88201=CARTESIAN_POINT('',(117.1,6.,48.35));
#88202=CARTESIAN_POINT('Origin',(116.9,7.4,48.5));
#88203=CARTESIAN_POINT('',(116.9,7.4,48.5));
#88204=CARTESIAN_POINT('',(58.45,7.4,48.5));
#88205=CARTESIAN_POINT('',(116.9,7.4,48.35));
#88206=CARTESIAN_POINT('',(116.9,7.4,48.5));
#88207=CARTESIAN_POINT('',(117.1,7.4,48.35));
#88208=CARTESIAN_POINT('Origin',(116.9,6.,48.5));
#88209=CARTESIAN_POINT('',(116.9,7.,48.5));
#88210=CARTESIAN_POINT('',(116.9,7.4,48.35));
#88211=CARTESIAN_POINT('Origin',(117.,6.7,48.35));
#88212=CARTESIAN_POINT('Origin',(115.1,5.2,48.5));
#88213=CARTESIAN_POINT('',(115.1,5.2,48.5));
#88214=CARTESIAN_POINT('',(114.9,5.2,48.5));
#88215=CARTESIAN_POINT('',(57.55,5.2,48.5));
#88216=CARTESIAN_POINT('',(115.1,5.2,48.35));
#88217=CARTESIAN_POINT('',(115.1,5.2,48.5));
#88218=CARTESIAN_POINT('',(114.9,5.2,48.35));
#88219=CARTESIAN_POINT('',(114.9,5.2,48.35));
#88220=CARTESIAN_POINT('',(114.9,5.2,48.5));
#88221=CARTESIAN_POINT('Origin',(115.1,7.4,48.5));
#88222=CARTESIAN_POINT('',(115.1,7.4,48.5));
#88223=CARTESIAN_POINT('',(115.1,7.7,48.5));
#88224=CARTESIAN_POINT('',(115.1,7.4,48.35));
#88225=CARTESIAN_POINT('',(115.1,7.4,48.5));
#88226=CARTESIAN_POINT('',(115.1,5.2,48.35));
#88227=CARTESIAN_POINT('Origin',(114.9,7.4,48.5));
#88228=CARTESIAN_POINT('',(114.9,7.4,48.5));
#88229=CARTESIAN_POINT('',(57.45,7.4,48.5));
#88230=CARTESIAN_POINT('',(114.9,7.4,48.35));
#88231=CARTESIAN_POINT('',(114.9,7.4,48.5));
#88232=CARTESIAN_POINT('',(115.1,7.4,48.35));
#88233=CARTESIAN_POINT('Origin',(114.9,5.2,48.5));
#88234=CARTESIAN_POINT('',(114.9,6.6,48.5));
#88235=CARTESIAN_POINT('',(114.9,7.4,48.35));
#88236=CARTESIAN_POINT('Origin',(115.,6.3,48.35));
#88237=CARTESIAN_POINT('Origin',(113.1,6.,48.5));
#88238=CARTESIAN_POINT('',(113.1,6.,48.5));
#88239=CARTESIAN_POINT('',(112.9,6.,48.5));
#88240=CARTESIAN_POINT('',(56.55,6.,48.5));
#88241=CARTESIAN_POINT('',(113.1,6.,48.35));
#88242=CARTESIAN_POINT('',(113.1,6.,48.5));
#88243=CARTESIAN_POINT('',(112.9,6.,48.35));
#88244=CARTESIAN_POINT('',(112.9,6.,48.35));
#88245=CARTESIAN_POINT('',(112.9,6.,48.5));
#88246=CARTESIAN_POINT('Origin',(113.1,7.4,48.5));
#88247=CARTESIAN_POINT('',(113.1,7.4,48.5));
#88248=CARTESIAN_POINT('',(113.1,7.7,48.5));
#88249=CARTESIAN_POINT('',(113.1,7.4,48.35));
#88250=CARTESIAN_POINT('',(113.1,7.4,48.5));
#88251=CARTESIAN_POINT('',(113.1,6.,48.35));
#88252=CARTESIAN_POINT('Origin',(112.9,7.4,48.5));
#88253=CARTESIAN_POINT('',(112.9,7.4,48.5));
#88254=CARTESIAN_POINT('',(56.45,7.4,48.5));
#88255=CARTESIAN_POINT('',(112.9,7.4,48.35));
#88256=CARTESIAN_POINT('',(112.9,7.4,48.5));
#88257=CARTESIAN_POINT('',(113.1,7.4,48.35));
#88258=CARTESIAN_POINT('Origin',(112.9,6.,48.5));
#88259=CARTESIAN_POINT('',(112.9,7.,48.5));
#88260=CARTESIAN_POINT('',(112.9,7.4,48.35));
#88261=CARTESIAN_POINT('Origin',(113.,6.7,48.35));
#88262=CARTESIAN_POINT('Origin',(111.1,6.,48.5));
#88263=CARTESIAN_POINT('',(111.1,6.,48.5));
#88264=CARTESIAN_POINT('',(110.9,6.,48.5));
#88265=CARTESIAN_POINT('',(55.55,6.,48.5));
#88266=CARTESIAN_POINT('',(111.1,6.,48.35));
#88267=CARTESIAN_POINT('',(111.1,6.,48.5));
#88268=CARTESIAN_POINT('',(110.9,6.,48.35));
#88269=CARTESIAN_POINT('',(110.9,6.,48.35));
#88270=CARTESIAN_POINT('',(110.9,6.,48.5));
#88271=CARTESIAN_POINT('Origin',(111.1,7.4,48.5));
#88272=CARTESIAN_POINT('',(111.1,7.4,48.5));
#88273=CARTESIAN_POINT('',(111.1,7.7,48.5));
#88274=CARTESIAN_POINT('',(111.1,7.4,48.35));
#88275=CARTESIAN_POINT('',(111.1,7.4,48.5));
#88276=CARTESIAN_POINT('',(111.1,6.,48.35));
#88277=CARTESIAN_POINT('Origin',(110.9,7.4,48.5));
#88278=CARTESIAN_POINT('',(110.9,7.4,48.5));
#88279=CARTESIAN_POINT('',(55.45,7.4,48.5));
#88280=CARTESIAN_POINT('',(110.9,7.4,48.35));
#88281=CARTESIAN_POINT('',(110.9,7.4,48.5));
#88282=CARTESIAN_POINT('',(111.1,7.4,48.35));
#88283=CARTESIAN_POINT('Origin',(110.9,6.,48.5));
#88284=CARTESIAN_POINT('',(110.9,7.,48.5));
#88285=CARTESIAN_POINT('',(110.9,7.4,48.35));
#88286=CARTESIAN_POINT('Origin',(111.,6.7,48.35));
#88287=CARTESIAN_POINT('Origin',(110.1,4.4,48.5));
#88288=CARTESIAN_POINT('',(110.1,4.4,48.5));
#88289=CARTESIAN_POINT('',(109.9,4.4,48.5));
#88290=CARTESIAN_POINT('',(55.05,4.4,48.5));
#88291=CARTESIAN_POINT('',(110.1,4.4,48.35));
#88292=CARTESIAN_POINT('',(110.1,4.4,48.5));
#88293=CARTESIAN_POINT('',(109.9,4.4,48.35));
#88294=CARTESIAN_POINT('',(109.9,4.4,48.35));
#88295=CARTESIAN_POINT('',(109.9,4.4,48.5));
#88296=CARTESIAN_POINT('Origin',(110.1,7.4,48.5));
#88297=CARTESIAN_POINT('',(110.1,7.4,48.5));
#88298=CARTESIAN_POINT('',(110.1,7.7,48.5));
#88299=CARTESIAN_POINT('',(110.1,7.4,48.35));
#88300=CARTESIAN_POINT('',(110.1,7.4,48.5));
#88301=CARTESIAN_POINT('',(110.1,4.4,48.35));
#88302=CARTESIAN_POINT('Origin',(109.9,7.4,48.5));
#88303=CARTESIAN_POINT('',(109.9,7.4,48.5));
#88304=CARTESIAN_POINT('',(54.95,7.4,48.5));
#88305=CARTESIAN_POINT('',(109.9,7.4,48.35));
#88306=CARTESIAN_POINT('',(109.9,7.4,48.5));
#88307=CARTESIAN_POINT('',(110.1,7.4,48.35));
#88308=CARTESIAN_POINT('Origin',(109.9,4.4,48.5));
#88309=CARTESIAN_POINT('',(109.9,6.2,48.5));
#88310=CARTESIAN_POINT('',(109.9,7.4,48.35));
#88311=CARTESIAN_POINT('Origin',(110.,5.9,48.35));
#88312=CARTESIAN_POINT('Origin',(108.1,6.,48.5));
#88313=CARTESIAN_POINT('',(108.1,6.,48.5));
#88314=CARTESIAN_POINT('',(107.9,6.,48.5));
#88315=CARTESIAN_POINT('',(54.05,6.,48.5));
#88316=CARTESIAN_POINT('',(108.1,6.,48.35));
#88317=CARTESIAN_POINT('',(108.1,6.,48.5));
#88318=CARTESIAN_POINT('',(107.9,6.,48.35));
#88319=CARTESIAN_POINT('',(107.9,6.,48.35));
#88320=CARTESIAN_POINT('',(107.9,6.,48.5));
#88321=CARTESIAN_POINT('Origin',(108.1,7.4,48.5));
#88322=CARTESIAN_POINT('',(108.1,7.4,48.5));
#88323=CARTESIAN_POINT('',(108.1,7.7,48.5));
#88324=CARTESIAN_POINT('',(108.1,7.4,48.35));
#88325=CARTESIAN_POINT('',(108.1,7.4,48.5));
#88326=CARTESIAN_POINT('',(108.1,6.,48.35));
#88327=CARTESIAN_POINT('Origin',(107.9,7.4,48.5));
#88328=CARTESIAN_POINT('',(107.9,7.4,48.5));
#88329=CARTESIAN_POINT('',(53.95,7.4,48.5));
#88330=CARTESIAN_POINT('',(107.9,7.4,48.35));
#88331=CARTESIAN_POINT('',(107.9,7.4,48.5));
#88332=CARTESIAN_POINT('',(108.1,7.4,48.35));
#88333=CARTESIAN_POINT('Origin',(107.9,6.,48.5));
#88334=CARTESIAN_POINT('',(107.9,7.,48.5));
#88335=CARTESIAN_POINT('',(107.9,7.4,48.35));
#88336=CARTESIAN_POINT('Origin',(108.,6.7,48.35));
#88337=CARTESIAN_POINT('Origin',(106.1,6.,48.5));
#88338=CARTESIAN_POINT('',(106.1,6.,48.5));
#88339=CARTESIAN_POINT('',(105.9,6.,48.5));
#88340=CARTESIAN_POINT('',(53.05,6.,48.5));
#88341=CARTESIAN_POINT('',(106.1,6.,48.35));
#88342=CARTESIAN_POINT('',(106.1,6.,48.5));
#88343=CARTESIAN_POINT('',(105.9,6.,48.35));
#88344=CARTESIAN_POINT('',(105.9,6.,48.35));
#88345=CARTESIAN_POINT('',(105.9,6.,48.5));
#88346=CARTESIAN_POINT('Origin',(106.1,7.4,48.5));
#88347=CARTESIAN_POINT('',(106.1,7.4,48.5));
#88348=CARTESIAN_POINT('',(106.1,7.7,48.5));
#88349=CARTESIAN_POINT('',(106.1,7.4,48.35));
#88350=CARTESIAN_POINT('',(106.1,7.4,48.5));
#88351=CARTESIAN_POINT('',(106.1,6.,48.35));
#88352=CARTESIAN_POINT('Origin',(105.9,7.4,48.5));
#88353=CARTESIAN_POINT('',(105.9,7.4,48.5));
#88354=CARTESIAN_POINT('',(52.95,7.4,48.5));
#88355=CARTESIAN_POINT('',(105.9,7.4,48.35));
#88356=CARTESIAN_POINT('',(105.9,7.4,48.5));
#88357=CARTESIAN_POINT('',(106.1,7.4,48.35));
#88358=CARTESIAN_POINT('Origin',(105.9,6.,48.5));
#88359=CARTESIAN_POINT('',(105.9,7.,48.5));
#88360=CARTESIAN_POINT('',(105.9,7.4,48.35));
#88361=CARTESIAN_POINT('Origin',(106.,6.7,48.35));
#88362=CARTESIAN_POINT('Origin',(104.1,6.,48.5));
#88363=CARTESIAN_POINT('',(104.1,6.,48.5));
#88364=CARTESIAN_POINT('',(103.9,6.,48.5));
#88365=CARTESIAN_POINT('',(52.05,6.,48.5));
#88366=CARTESIAN_POINT('',(104.1,6.,48.35));
#88367=CARTESIAN_POINT('',(104.1,6.,48.5));
#88368=CARTESIAN_POINT('',(103.9,6.,48.35));
#88369=CARTESIAN_POINT('',(103.9,6.,48.35));
#88370=CARTESIAN_POINT('',(103.9,6.,48.5));
#88371=CARTESIAN_POINT('Origin',(104.1,7.4,48.5));
#88372=CARTESIAN_POINT('',(104.1,7.4,48.5));
#88373=CARTESIAN_POINT('',(104.1,7.7,48.5));
#88374=CARTESIAN_POINT('',(104.1,7.4,48.35));
#88375=CARTESIAN_POINT('',(104.1,7.4,48.5));
#88376=CARTESIAN_POINT('',(104.1,6.,48.35));
#88377=CARTESIAN_POINT('Origin',(103.9,7.4,48.5));
#88378=CARTESIAN_POINT('',(103.9,7.4,48.5));
#88379=CARTESIAN_POINT('',(51.95,7.4,48.5));
#88380=CARTESIAN_POINT('',(103.9,7.4,48.35));
#88381=CARTESIAN_POINT('',(103.9,7.4,48.5));
#88382=CARTESIAN_POINT('',(104.1,7.4,48.35));
#88383=CARTESIAN_POINT('Origin',(103.9,6.,48.5));
#88384=CARTESIAN_POINT('',(103.9,7.,48.5));
#88385=CARTESIAN_POINT('',(103.9,7.4,48.35));
#88386=CARTESIAN_POINT('Origin',(104.,6.7,48.35));
#88387=CARTESIAN_POINT('Origin',(102.1,6.,48.5));
#88388=CARTESIAN_POINT('',(102.1,6.,48.5));
#88389=CARTESIAN_POINT('',(101.9,6.,48.5));
#88390=CARTESIAN_POINT('',(51.05,6.,48.5));
#88391=CARTESIAN_POINT('',(102.1,6.,48.35));
#88392=CARTESIAN_POINT('',(102.1,6.,48.5));
#88393=CARTESIAN_POINT('',(101.9,6.,48.35));
#88394=CARTESIAN_POINT('',(101.9,6.,48.35));
#88395=CARTESIAN_POINT('',(101.9,6.,48.5));
#88396=CARTESIAN_POINT('Origin',(102.1,7.4,48.5));
#88397=CARTESIAN_POINT('',(102.1,7.4,48.5));
#88398=CARTESIAN_POINT('',(102.1,7.7,48.5));
#88399=CARTESIAN_POINT('',(102.1,7.4,48.35));
#88400=CARTESIAN_POINT('',(102.1,7.4,48.5));
#88401=CARTESIAN_POINT('',(102.1,6.,48.35));
#88402=CARTESIAN_POINT('Origin',(101.9,7.4,48.5));
#88403=CARTESIAN_POINT('',(101.9,7.4,48.5));
#88404=CARTESIAN_POINT('',(50.95,7.4,48.5));
#88405=CARTESIAN_POINT('',(101.9,7.4,48.35));
#88406=CARTESIAN_POINT('',(101.9,7.4,48.5));
#88407=CARTESIAN_POINT('',(102.1,7.4,48.35));
#88408=CARTESIAN_POINT('Origin',(101.9,6.,48.5));
#88409=CARTESIAN_POINT('',(101.9,7.,48.5));
#88410=CARTESIAN_POINT('',(101.9,7.4,48.35));
#88411=CARTESIAN_POINT('Origin',(102.,6.7,48.35));
#88412=CARTESIAN_POINT('Origin',(100.1,4.4,48.5));
#88413=CARTESIAN_POINT('',(100.1,4.4,48.5));
#88414=CARTESIAN_POINT('',(99.9,4.4,48.5));
#88415=CARTESIAN_POINT('',(50.05,4.4,48.5));
#88416=CARTESIAN_POINT('',(100.1,4.4,48.35));
#88417=CARTESIAN_POINT('',(100.1,4.4,48.5));
#88418=CARTESIAN_POINT('',(99.9,4.4,48.35));
#88419=CARTESIAN_POINT('',(99.9,4.4,48.35));
#88420=CARTESIAN_POINT('',(99.9,4.4,48.5));
#88421=CARTESIAN_POINT('Origin',(100.1,7.4,48.5));
#88422=CARTESIAN_POINT('',(100.1,7.4,48.5));
#88423=CARTESIAN_POINT('',(100.1,7.7,48.5));
#88424=CARTESIAN_POINT('',(100.1,7.4,48.35));
#88425=CARTESIAN_POINT('',(100.1,7.4,48.5));
#88426=CARTESIAN_POINT('',(100.1,4.4,48.35));
#88427=CARTESIAN_POINT('Origin',(99.9,7.4,48.5));
#88428=CARTESIAN_POINT('',(99.9,7.4,48.5));
#88429=CARTESIAN_POINT('',(49.95,7.4,48.5));
#88430=CARTESIAN_POINT('',(99.9,7.4,48.35));
#88431=CARTESIAN_POINT('',(99.9,7.4,48.5));
#88432=CARTESIAN_POINT('',(100.1,7.4,48.35));
#88433=CARTESIAN_POINT('Origin',(99.9,4.4,48.5));
#88434=CARTESIAN_POINT('',(99.9,6.2,48.5));
#88435=CARTESIAN_POINT('',(99.9,7.4,48.35));
#88436=CARTESIAN_POINT('Origin',(100.,5.9,48.35));
#88437=CARTESIAN_POINT('Origin',(98.1,6.,48.5));
#88438=CARTESIAN_POINT('',(98.1,6.,48.5));
#88439=CARTESIAN_POINT('',(97.9,6.,48.5));
#88440=CARTESIAN_POINT('',(49.05,6.,48.5));
#88441=CARTESIAN_POINT('',(98.1,6.,48.35));
#88442=CARTESIAN_POINT('',(98.1,6.,48.5));
#88443=CARTESIAN_POINT('',(97.9,6.,48.35));
#88444=CARTESIAN_POINT('',(97.9,6.,48.35));
#88445=CARTESIAN_POINT('',(97.9,6.,48.5));
#88446=CARTESIAN_POINT('Origin',(98.1,7.4,48.5));
#88447=CARTESIAN_POINT('',(98.1,7.4,48.5));
#88448=CARTESIAN_POINT('',(98.1,7.7,48.5));
#88449=CARTESIAN_POINT('',(98.1,7.4,48.35));
#88450=CARTESIAN_POINT('',(98.1,7.4,48.5));
#88451=CARTESIAN_POINT('',(98.1,6.,48.35));
#88452=CARTESIAN_POINT('Origin',(97.9,7.4,48.5));
#88453=CARTESIAN_POINT('',(97.9,7.4,48.5));
#88454=CARTESIAN_POINT('',(48.95,7.4,48.5));
#88455=CARTESIAN_POINT('',(97.9,7.4,48.35));
#88456=CARTESIAN_POINT('',(97.9,7.4,48.5));
#88457=CARTESIAN_POINT('',(98.1,7.4,48.35));
#88458=CARTESIAN_POINT('Origin',(97.9,6.,48.5));
#88459=CARTESIAN_POINT('',(97.9,7.,48.5));
#88460=CARTESIAN_POINT('',(97.9,7.4,48.35));
#88461=CARTESIAN_POINT('Origin',(98.,6.7,48.35));
#88462=CARTESIAN_POINT('Origin',(96.1,6.,48.5));
#88463=CARTESIAN_POINT('',(96.1,6.,48.5));
#88464=CARTESIAN_POINT('',(95.9,6.,48.5));
#88465=CARTESIAN_POINT('',(48.05,6.,48.5));
#88466=CARTESIAN_POINT('',(96.1,6.,48.35));
#88467=CARTESIAN_POINT('',(96.1,6.,48.5));
#88468=CARTESIAN_POINT('',(95.9,6.,48.35));
#88469=CARTESIAN_POINT('',(95.9,6.,48.35));
#88470=CARTESIAN_POINT('',(95.9,6.,48.5));
#88471=CARTESIAN_POINT('Origin',(96.1,7.4,48.5));
#88472=CARTESIAN_POINT('',(96.1,7.4,48.5));
#88473=CARTESIAN_POINT('',(96.1,7.7,48.5));
#88474=CARTESIAN_POINT('',(96.1,7.4,48.35));
#88475=CARTESIAN_POINT('',(96.1,7.4,48.5));
#88476=CARTESIAN_POINT('',(96.1,6.,48.35));
#88477=CARTESIAN_POINT('Origin',(95.9,7.4,48.5));
#88478=CARTESIAN_POINT('',(95.9,7.4,48.5));
#88479=CARTESIAN_POINT('',(47.95,7.4,48.5));
#88480=CARTESIAN_POINT('',(95.9,7.4,48.35));
#88481=CARTESIAN_POINT('',(95.9,7.4,48.5));
#88482=CARTESIAN_POINT('',(96.1,7.4,48.35));
#88483=CARTESIAN_POINT('Origin',(95.9,6.,48.5));
#88484=CARTESIAN_POINT('',(95.9,7.,48.5));
#88485=CARTESIAN_POINT('',(95.9,7.4,48.35));
#88486=CARTESIAN_POINT('Origin',(96.,6.7,48.35));
#88487=CARTESIAN_POINT('Origin',(94.1,6.,48.5));
#88488=CARTESIAN_POINT('',(94.1,6.,48.5));
#88489=CARTESIAN_POINT('',(93.9,6.,48.5));
#88490=CARTESIAN_POINT('',(47.05,6.,48.5));
#88491=CARTESIAN_POINT('',(94.1,6.,48.35));
#88492=CARTESIAN_POINT('',(94.1,6.,48.5));
#88493=CARTESIAN_POINT('',(93.9,6.,48.35));
#88494=CARTESIAN_POINT('',(93.9,6.,48.35));
#88495=CARTESIAN_POINT('',(93.9,6.,48.5));
#88496=CARTESIAN_POINT('Origin',(94.1,7.4,48.5));
#88497=CARTESIAN_POINT('',(94.1,7.4,48.5));
#88498=CARTESIAN_POINT('',(94.1,7.7,48.5));
#88499=CARTESIAN_POINT('',(94.1,7.4,48.35));
#88500=CARTESIAN_POINT('',(94.1,7.4,48.5));
#88501=CARTESIAN_POINT('',(94.1,6.,48.35));
#88502=CARTESIAN_POINT('Origin',(93.9,7.4,48.5));
#88503=CARTESIAN_POINT('',(93.9,7.4,48.5));
#88504=CARTESIAN_POINT('',(46.95,7.4,48.5));
#88505=CARTESIAN_POINT('',(93.9,7.4,48.35));
#88506=CARTESIAN_POINT('',(93.9,7.4,48.5));
#88507=CARTESIAN_POINT('',(94.1,7.4,48.35));
#88508=CARTESIAN_POINT('Origin',(93.9,6.,48.5));
#88509=CARTESIAN_POINT('',(93.9,7.,48.5));
#88510=CARTESIAN_POINT('',(93.9,7.4,48.35));
#88511=CARTESIAN_POINT('Origin',(94.,6.7,48.35));
#88512=CARTESIAN_POINT('Origin',(92.1,6.,48.5));
#88513=CARTESIAN_POINT('',(92.1,6.,48.5));
#88514=CARTESIAN_POINT('',(91.9,6.,48.5));
#88515=CARTESIAN_POINT('',(46.05,6.,48.5));
#88516=CARTESIAN_POINT('',(92.1,6.,48.35));
#88517=CARTESIAN_POINT('',(92.1,6.,48.5));
#88518=CARTESIAN_POINT('',(91.9,6.,48.35));
#88519=CARTESIAN_POINT('',(91.9,6.,48.35));
#88520=CARTESIAN_POINT('',(91.9,6.,48.5));
#88521=CARTESIAN_POINT('Origin',(92.1,7.4,48.5));
#88522=CARTESIAN_POINT('',(92.1,7.4,48.5));
#88523=CARTESIAN_POINT('',(92.1,7.7,48.5));
#88524=CARTESIAN_POINT('',(92.1,7.4,48.35));
#88525=CARTESIAN_POINT('',(92.1,7.4,48.5));
#88526=CARTESIAN_POINT('',(92.1,6.,48.35));
#88527=CARTESIAN_POINT('Origin',(91.9,7.4,48.5));
#88528=CARTESIAN_POINT('',(91.9,7.4,48.5));
#88529=CARTESIAN_POINT('',(45.95,7.4,48.5));
#88530=CARTESIAN_POINT('',(91.9,7.4,48.35));
#88531=CARTESIAN_POINT('',(91.9,7.4,48.5));
#88532=CARTESIAN_POINT('',(92.1,7.4,48.35));
#88533=CARTESIAN_POINT('Origin',(91.9,6.,48.5));
#88534=CARTESIAN_POINT('',(91.9,7.,48.5));
#88535=CARTESIAN_POINT('',(91.9,7.4,48.35));
#88536=CARTESIAN_POINT('Origin',(92.,6.7,48.35));
#88537=CARTESIAN_POINT('Origin',(90.1,4.4,48.5));
#88538=CARTESIAN_POINT('',(90.1,4.4,48.5));
#88539=CARTESIAN_POINT('',(89.9,4.4,48.5));
#88540=CARTESIAN_POINT('',(45.05,4.4,48.5));
#88541=CARTESIAN_POINT('',(90.1,4.4,48.35));
#88542=CARTESIAN_POINT('',(90.1,4.4,48.5));
#88543=CARTESIAN_POINT('',(89.9,4.4,48.35));
#88544=CARTESIAN_POINT('',(89.9,4.4,48.35));
#88545=CARTESIAN_POINT('',(89.9,4.4,48.5));
#88546=CARTESIAN_POINT('Origin',(90.1,7.4,48.5));
#88547=CARTESIAN_POINT('',(90.1,7.4,48.5));
#88548=CARTESIAN_POINT('',(90.1,7.7,48.5));
#88549=CARTESIAN_POINT('',(90.1,7.4,48.35));
#88550=CARTESIAN_POINT('',(90.1,7.4,48.5));
#88551=CARTESIAN_POINT('',(90.1,4.4,48.35));
#88552=CARTESIAN_POINT('Origin',(89.9,7.4,48.5));
#88553=CARTESIAN_POINT('',(89.9,7.4,48.5));
#88554=CARTESIAN_POINT('',(44.95,7.4,48.5));
#88555=CARTESIAN_POINT('',(89.9,7.4,48.35));
#88556=CARTESIAN_POINT('',(89.9,7.4,48.5));
#88557=CARTESIAN_POINT('',(90.1,7.4,48.35));
#88558=CARTESIAN_POINT('Origin',(89.9,4.4,48.5));
#88559=CARTESIAN_POINT('',(89.9,6.2,48.5));
#88560=CARTESIAN_POINT('',(89.9,7.4,48.35));
#88561=CARTESIAN_POINT('Origin',(90.,5.9,48.35));
#88562=CARTESIAN_POINT('Origin',(88.1,6.,48.5));
#88563=CARTESIAN_POINT('',(88.1,6.,48.5));
#88564=CARTESIAN_POINT('',(87.9,6.,48.5));
#88565=CARTESIAN_POINT('',(44.05,6.,48.5));
#88566=CARTESIAN_POINT('',(88.1,6.,48.35));
#88567=CARTESIAN_POINT('',(88.1,6.,48.5));
#88568=CARTESIAN_POINT('',(87.9,6.,48.35));
#88569=CARTESIAN_POINT('',(87.9,6.,48.35));
#88570=CARTESIAN_POINT('',(87.9,6.,48.5));
#88571=CARTESIAN_POINT('Origin',(88.1,7.4,48.5));
#88572=CARTESIAN_POINT('',(88.1,7.4,48.5));
#88573=CARTESIAN_POINT('',(88.1,7.7,48.5));
#88574=CARTESIAN_POINT('',(88.1,7.4,48.35));
#88575=CARTESIAN_POINT('',(88.1,7.4,48.5));
#88576=CARTESIAN_POINT('',(88.1,6.,48.35));
#88577=CARTESIAN_POINT('Origin',(87.9,7.4,48.5));
#88578=CARTESIAN_POINT('',(87.9,7.4,48.5));
#88579=CARTESIAN_POINT('',(43.95,7.4,48.5));
#88580=CARTESIAN_POINT('',(87.9,7.4,48.35));
#88581=CARTESIAN_POINT('',(87.9,7.4,48.5));
#88582=CARTESIAN_POINT('',(88.1,7.4,48.35));
#88583=CARTESIAN_POINT('Origin',(87.9,6.,48.5));
#88584=CARTESIAN_POINT('',(87.9,7.,48.5));
#88585=CARTESIAN_POINT('',(87.9,7.4,48.35));
#88586=CARTESIAN_POINT('Origin',(88.,6.7,48.35));
#88587=CARTESIAN_POINT('Origin',(86.1,6.,48.5));
#88588=CARTESIAN_POINT('',(86.1,6.,48.5));
#88589=CARTESIAN_POINT('',(85.9,6.,48.5));
#88590=CARTESIAN_POINT('',(43.05,6.,48.5));
#88591=CARTESIAN_POINT('',(86.1,6.,48.35));
#88592=CARTESIAN_POINT('',(86.1,6.,48.5));
#88593=CARTESIAN_POINT('',(85.9,6.,48.35));
#88594=CARTESIAN_POINT('',(85.9,6.,48.35));
#88595=CARTESIAN_POINT('',(85.9,6.,48.5));
#88596=CARTESIAN_POINT('Origin',(86.1,7.4,48.5));
#88597=CARTESIAN_POINT('',(86.1,7.4,48.5));
#88598=CARTESIAN_POINT('',(86.1,7.7,48.5));
#88599=CARTESIAN_POINT('',(86.1,7.4,48.35));
#88600=CARTESIAN_POINT('',(86.1,7.4,48.5));
#88601=CARTESIAN_POINT('',(86.1,6.,48.35));
#88602=CARTESIAN_POINT('Origin',(85.9,7.4,48.5));
#88603=CARTESIAN_POINT('',(85.9,7.4,48.5));
#88604=CARTESIAN_POINT('',(42.95,7.4,48.5));
#88605=CARTESIAN_POINT('',(85.9,7.4,48.35));
#88606=CARTESIAN_POINT('',(85.9,7.4,48.5));
#88607=CARTESIAN_POINT('',(86.1,7.4,48.35));
#88608=CARTESIAN_POINT('Origin',(85.9,6.,48.5));
#88609=CARTESIAN_POINT('',(85.9,7.,48.5));
#88610=CARTESIAN_POINT('',(85.9,7.4,48.35));
#88611=CARTESIAN_POINT('Origin',(86.,6.7,48.35));
#88612=CARTESIAN_POINT('Origin',(84.1,6.,48.5));
#88613=CARTESIAN_POINT('',(84.1,6.,48.5));
#88614=CARTESIAN_POINT('',(83.9,6.,48.5));
#88615=CARTESIAN_POINT('',(42.05,6.,48.5));
#88616=CARTESIAN_POINT('',(84.1,6.,48.35));
#88617=CARTESIAN_POINT('',(84.1,6.,48.5));
#88618=CARTESIAN_POINT('',(83.9,6.,48.35));
#88619=CARTESIAN_POINT('',(83.9,6.,48.35));
#88620=CARTESIAN_POINT('',(83.9,6.,48.5));
#88621=CARTESIAN_POINT('Origin',(84.1,7.4,48.5));
#88622=CARTESIAN_POINT('',(84.1,7.4,48.5));
#88623=CARTESIAN_POINT('',(84.1,7.7,48.5));
#88624=CARTESIAN_POINT('',(84.1,7.4,48.35));
#88625=CARTESIAN_POINT('',(84.1,7.4,48.5));
#88626=CARTESIAN_POINT('',(84.1,6.,48.35));
#88627=CARTESIAN_POINT('Origin',(83.9,7.4,48.5));
#88628=CARTESIAN_POINT('',(83.9,7.4,48.5));
#88629=CARTESIAN_POINT('',(41.95,7.4,48.5));
#88630=CARTESIAN_POINT('',(83.9,7.4,48.35));
#88631=CARTESIAN_POINT('',(83.9,7.4,48.5));
#88632=CARTESIAN_POINT('',(84.1,7.4,48.35));
#88633=CARTESIAN_POINT('Origin',(83.9,6.,48.5));
#88634=CARTESIAN_POINT('',(83.9,7.,48.5));
#88635=CARTESIAN_POINT('',(83.9,7.4,48.35));
#88636=CARTESIAN_POINT('Origin',(84.,6.7,48.35));
#88637=CARTESIAN_POINT('Origin',(82.1,6.,48.5));
#88638=CARTESIAN_POINT('',(82.1,6.,48.5));
#88639=CARTESIAN_POINT('',(81.9,6.,48.5));
#88640=CARTESIAN_POINT('',(41.05,6.,48.5));
#88641=CARTESIAN_POINT('',(82.1,6.,48.35));
#88642=CARTESIAN_POINT('',(82.1,6.,48.5));
#88643=CARTESIAN_POINT('',(81.9,6.,48.35));
#88644=CARTESIAN_POINT('',(81.9,6.,48.35));
#88645=CARTESIAN_POINT('',(81.9,6.,48.5));
#88646=CARTESIAN_POINT('Origin',(82.1,7.4,48.5));
#88647=CARTESIAN_POINT('',(82.1,7.4,48.5));
#88648=CARTESIAN_POINT('',(82.1,7.7,48.5));
#88649=CARTESIAN_POINT('',(82.1,7.4,48.35));
#88650=CARTESIAN_POINT('',(82.1,7.4,48.5));
#88651=CARTESIAN_POINT('',(82.1,6.,48.35));
#88652=CARTESIAN_POINT('Origin',(81.9,7.4,48.5));
#88653=CARTESIAN_POINT('',(81.9,7.4,48.5));
#88654=CARTESIAN_POINT('',(40.95,7.4,48.5));
#88655=CARTESIAN_POINT('',(81.9,7.4,48.35));
#88656=CARTESIAN_POINT('',(81.9,7.4,48.5));
#88657=CARTESIAN_POINT('',(82.1,7.4,48.35));
#88658=CARTESIAN_POINT('Origin',(81.9,6.,48.5));
#88659=CARTESIAN_POINT('',(81.9,7.,48.5));
#88660=CARTESIAN_POINT('',(81.9,7.4,48.35));
#88661=CARTESIAN_POINT('Origin',(82.,6.7,48.35));
#88662=CARTESIAN_POINT('Origin',(80.1,4.4,48.5));
#88663=CARTESIAN_POINT('',(80.1,4.4,48.5));
#88664=CARTESIAN_POINT('',(79.9,4.4,48.5));
#88665=CARTESIAN_POINT('',(40.05,4.4,48.5));
#88666=CARTESIAN_POINT('',(80.1,4.4,48.35));
#88667=CARTESIAN_POINT('',(80.1,4.4,48.5));
#88668=CARTESIAN_POINT('',(79.9,4.4,48.35));
#88669=CARTESIAN_POINT('',(79.9,4.4,48.35));
#88670=CARTESIAN_POINT('',(79.9,4.4,48.5));
#88671=CARTESIAN_POINT('Origin',(80.1,7.4,48.5));
#88672=CARTESIAN_POINT('',(80.1,7.4,48.5));
#88673=CARTESIAN_POINT('',(80.1,7.7,48.5));
#88674=CARTESIAN_POINT('',(80.1,7.4,48.35));
#88675=CARTESIAN_POINT('',(80.1,7.4,48.5));
#88676=CARTESIAN_POINT('',(80.1,4.4,48.35));
#88677=CARTESIAN_POINT('Origin',(79.9,7.4,48.5));
#88678=CARTESIAN_POINT('',(79.9,7.4,48.5));
#88679=CARTESIAN_POINT('',(39.95,7.4,48.5));
#88680=CARTESIAN_POINT('',(79.9,7.4,48.35));
#88681=CARTESIAN_POINT('',(79.9,7.4,48.5));
#88682=CARTESIAN_POINT('',(80.1,7.4,48.35));
#88683=CARTESIAN_POINT('Origin',(79.9,4.4,48.5));
#88684=CARTESIAN_POINT('',(79.9,6.2,48.5));
#88685=CARTESIAN_POINT('',(79.9,7.4,48.35));
#88686=CARTESIAN_POINT('Origin',(80.,5.9,48.35));
#88687=CARTESIAN_POINT('Origin',(78.1,6.,48.5));
#88688=CARTESIAN_POINT('',(78.1,6.,48.5));
#88689=CARTESIAN_POINT('',(77.9,6.,48.5));
#88690=CARTESIAN_POINT('',(39.05,6.,48.5));
#88691=CARTESIAN_POINT('',(78.1,6.,48.35));
#88692=CARTESIAN_POINT('',(78.1,6.,48.5));
#88693=CARTESIAN_POINT('',(77.9,6.,48.35));
#88694=CARTESIAN_POINT('',(77.9,6.,48.35));
#88695=CARTESIAN_POINT('',(77.9,6.,48.5));
#88696=CARTESIAN_POINT('Origin',(78.1,7.4,48.5));
#88697=CARTESIAN_POINT('',(78.1,7.4,48.5));
#88698=CARTESIAN_POINT('',(78.1,7.7,48.5));
#88699=CARTESIAN_POINT('',(78.1,7.4,48.35));
#88700=CARTESIAN_POINT('',(78.1,7.4,48.5));
#88701=CARTESIAN_POINT('',(78.1,6.,48.35));
#88702=CARTESIAN_POINT('Origin',(77.9,7.4,48.5));
#88703=CARTESIAN_POINT('',(77.9,7.4,48.5));
#88704=CARTESIAN_POINT('',(38.95,7.4,48.5));
#88705=CARTESIAN_POINT('',(77.9,7.4,48.35));
#88706=CARTESIAN_POINT('',(77.9,7.4,48.5));
#88707=CARTESIAN_POINT('',(78.1,7.4,48.35));
#88708=CARTESIAN_POINT('Origin',(77.9,6.,48.5));
#88709=CARTESIAN_POINT('',(77.9,7.,48.5));
#88710=CARTESIAN_POINT('',(77.9,7.4,48.35));
#88711=CARTESIAN_POINT('Origin',(78.,6.7,48.35));
#88712=CARTESIAN_POINT('Origin',(76.1,6.,48.5));
#88713=CARTESIAN_POINT('',(76.1,6.,48.5));
#88714=CARTESIAN_POINT('',(75.9,6.,48.5));
#88715=CARTESIAN_POINT('',(38.05,6.,48.5));
#88716=CARTESIAN_POINT('',(76.1,6.,48.35));
#88717=CARTESIAN_POINT('',(76.1,6.,48.5));
#88718=CARTESIAN_POINT('',(75.9,6.,48.35));
#88719=CARTESIAN_POINT('',(75.9,6.,48.35));
#88720=CARTESIAN_POINT('',(75.9,6.,48.5));
#88721=CARTESIAN_POINT('Origin',(76.1,7.4,48.5));
#88722=CARTESIAN_POINT('',(76.1,7.4,48.5));
#88723=CARTESIAN_POINT('',(76.1,7.7,48.5));
#88724=CARTESIAN_POINT('',(76.1,7.4,48.35));
#88725=CARTESIAN_POINT('',(76.1,7.4,48.5));
#88726=CARTESIAN_POINT('',(76.1,6.,48.35));
#88727=CARTESIAN_POINT('Origin',(75.9,7.4,48.5));
#88728=CARTESIAN_POINT('',(75.9,7.4,48.5));
#88729=CARTESIAN_POINT('',(37.95,7.4,48.5));
#88730=CARTESIAN_POINT('',(75.9,7.4,48.35));
#88731=CARTESIAN_POINT('',(75.9,7.4,48.5));
#88732=CARTESIAN_POINT('',(76.1,7.4,48.35));
#88733=CARTESIAN_POINT('Origin',(75.9,6.,48.5));
#88734=CARTESIAN_POINT('',(75.9,7.,48.5));
#88735=CARTESIAN_POINT('',(75.9,7.4,48.35));
#88736=CARTESIAN_POINT('Origin',(76.,6.7,48.35));
#88737=CARTESIAN_POINT('Origin',(74.1,6.,48.5));
#88738=CARTESIAN_POINT('',(74.1,6.,48.5));
#88739=CARTESIAN_POINT('',(73.9,6.,48.5));
#88740=CARTESIAN_POINT('',(37.05,6.,48.5));
#88741=CARTESIAN_POINT('',(74.1,6.,48.35));
#88742=CARTESIAN_POINT('',(74.1,6.,48.5));
#88743=CARTESIAN_POINT('',(73.9,6.,48.35));
#88744=CARTESIAN_POINT('',(73.9,6.,48.35));
#88745=CARTESIAN_POINT('',(73.9,6.,48.5));
#88746=CARTESIAN_POINT('Origin',(74.1,7.4,48.5));
#88747=CARTESIAN_POINT('',(74.1,7.4,48.5));
#88748=CARTESIAN_POINT('',(74.1,7.7,48.5));
#88749=CARTESIAN_POINT('',(74.1,7.4,48.35));
#88750=CARTESIAN_POINT('',(74.1,7.4,48.5));
#88751=CARTESIAN_POINT('',(74.1,6.,48.35));
#88752=CARTESIAN_POINT('Origin',(73.9,7.4,48.5));
#88753=CARTESIAN_POINT('',(73.9,7.4,48.5));
#88754=CARTESIAN_POINT('',(36.95,7.4,48.5));
#88755=CARTESIAN_POINT('',(73.9,7.4,48.35));
#88756=CARTESIAN_POINT('',(73.9,7.4,48.5));
#88757=CARTESIAN_POINT('',(74.1,7.4,48.35));
#88758=CARTESIAN_POINT('Origin',(73.9,6.,48.5));
#88759=CARTESIAN_POINT('',(73.9,7.,48.5));
#88760=CARTESIAN_POINT('',(73.9,7.4,48.35));
#88761=CARTESIAN_POINT('Origin',(74.,6.7,48.35));
#88762=CARTESIAN_POINT('Origin',(72.1,6.,48.5));
#88763=CARTESIAN_POINT('',(72.1,6.,48.5));
#88764=CARTESIAN_POINT('',(71.9,6.,48.5));
#88765=CARTESIAN_POINT('',(36.05,6.,48.5));
#88766=CARTESIAN_POINT('',(72.1,6.,48.35));
#88767=CARTESIAN_POINT('',(72.1,6.,48.5));
#88768=CARTESIAN_POINT('',(71.9,6.,48.35));
#88769=CARTESIAN_POINT('',(71.9,6.,48.35));
#88770=CARTESIAN_POINT('',(71.9,6.,48.5));
#88771=CARTESIAN_POINT('Origin',(72.1,7.4,48.5));
#88772=CARTESIAN_POINT('',(72.1,7.4,48.5));
#88773=CARTESIAN_POINT('',(72.1,7.7,48.5));
#88774=CARTESIAN_POINT('',(72.1,7.4,48.35));
#88775=CARTESIAN_POINT('',(72.1,7.4,48.5));
#88776=CARTESIAN_POINT('',(72.1,6.,48.35));
#88777=CARTESIAN_POINT('Origin',(71.9,7.4,48.5));
#88778=CARTESIAN_POINT('',(71.9,7.4,48.5));
#88779=CARTESIAN_POINT('',(35.95,7.4,48.5));
#88780=CARTESIAN_POINT('',(71.9,7.4,48.35));
#88781=CARTESIAN_POINT('',(71.9,7.4,48.5));
#88782=CARTESIAN_POINT('',(72.1,7.4,48.35));
#88783=CARTESIAN_POINT('Origin',(71.9,6.,48.5));
#88784=CARTESIAN_POINT('',(71.9,7.,48.5));
#88785=CARTESIAN_POINT('',(71.9,7.4,48.35));
#88786=CARTESIAN_POINT('Origin',(72.,6.7,48.35));
#88787=CARTESIAN_POINT('Origin',(70.1,4.4,48.5));
#88788=CARTESIAN_POINT('',(70.1,4.4,48.5));
#88789=CARTESIAN_POINT('',(69.9,4.4,48.5));
#88790=CARTESIAN_POINT('',(35.05,4.4,48.5));
#88791=CARTESIAN_POINT('',(70.1,4.4,48.35));
#88792=CARTESIAN_POINT('',(70.1,4.4,48.5));
#88793=CARTESIAN_POINT('',(69.9,4.4,48.35));
#88794=CARTESIAN_POINT('',(69.9,4.4,48.35));
#88795=CARTESIAN_POINT('',(69.9,4.4,48.5));
#88796=CARTESIAN_POINT('Origin',(70.1,7.4,48.5));
#88797=CARTESIAN_POINT('',(70.1,7.4,48.5));
#88798=CARTESIAN_POINT('',(70.1,7.7,48.5));
#88799=CARTESIAN_POINT('',(70.1,7.4,48.35));
#88800=CARTESIAN_POINT('',(70.1,7.4,48.5));
#88801=CARTESIAN_POINT('',(70.1,4.4,48.35));
#88802=CARTESIAN_POINT('Origin',(69.9,7.4,48.5));
#88803=CARTESIAN_POINT('',(69.9,7.4,48.5));
#88804=CARTESIAN_POINT('',(34.95,7.4,48.5));
#88805=CARTESIAN_POINT('',(69.9,7.4,48.35));
#88806=CARTESIAN_POINT('',(69.9,7.4,48.5));
#88807=CARTESIAN_POINT('',(70.1,7.4,48.35));
#88808=CARTESIAN_POINT('Origin',(69.9,4.4,48.5));
#88809=CARTESIAN_POINT('',(69.9,6.2,48.5));
#88810=CARTESIAN_POINT('',(69.9,7.4,48.35));
#88811=CARTESIAN_POINT('Origin',(70.,5.9,48.35));
#88812=CARTESIAN_POINT('Origin',(68.1,6.,48.5));
#88813=CARTESIAN_POINT('',(68.1,6.,48.5));
#88814=CARTESIAN_POINT('',(67.9,6.,48.5));
#88815=CARTESIAN_POINT('',(34.05,6.,48.5));
#88816=CARTESIAN_POINT('',(68.1,6.,48.35));
#88817=CARTESIAN_POINT('',(68.1,6.,48.5));
#88818=CARTESIAN_POINT('',(67.9,6.,48.35));
#88819=CARTESIAN_POINT('',(67.9,6.,48.35));
#88820=CARTESIAN_POINT('',(67.9,6.,48.5));
#88821=CARTESIAN_POINT('Origin',(68.1,7.4,48.5));
#88822=CARTESIAN_POINT('',(68.1,7.4,48.5));
#88823=CARTESIAN_POINT('',(68.1,7.7,48.5));
#88824=CARTESIAN_POINT('',(68.1,7.4,48.35));
#88825=CARTESIAN_POINT('',(68.1,7.4,48.5));
#88826=CARTESIAN_POINT('',(68.1,6.,48.35));
#88827=CARTESIAN_POINT('Origin',(67.9,7.4,48.5));
#88828=CARTESIAN_POINT('',(67.9,7.4,48.5));
#88829=CARTESIAN_POINT('',(33.95,7.4,48.5));
#88830=CARTESIAN_POINT('',(67.9,7.4,48.35));
#88831=CARTESIAN_POINT('',(67.9,7.4,48.5));
#88832=CARTESIAN_POINT('',(68.1,7.4,48.35));
#88833=CARTESIAN_POINT('Origin',(67.9,6.,48.5));
#88834=CARTESIAN_POINT('',(67.9,7.,48.5));
#88835=CARTESIAN_POINT('',(67.9,7.4,48.35));
#88836=CARTESIAN_POINT('Origin',(68.,6.7,48.35));
#88837=CARTESIAN_POINT('Origin',(66.1,6.,48.5));
#88838=CARTESIAN_POINT('',(66.1,6.,48.5));
#88839=CARTESIAN_POINT('',(65.9,6.,48.5));
#88840=CARTESIAN_POINT('',(33.05,6.,48.5));
#88841=CARTESIAN_POINT('',(66.1,6.,48.35));
#88842=CARTESIAN_POINT('',(66.1,6.,48.5));
#88843=CARTESIAN_POINT('',(65.9,6.,48.35));
#88844=CARTESIAN_POINT('',(65.9,6.,48.35));
#88845=CARTESIAN_POINT('',(65.9,6.,48.5));
#88846=CARTESIAN_POINT('Origin',(66.1,7.4,48.5));
#88847=CARTESIAN_POINT('',(66.1,7.4,48.5));
#88848=CARTESIAN_POINT('',(66.1,7.7,48.5));
#88849=CARTESIAN_POINT('',(66.1,7.4,48.35));
#88850=CARTESIAN_POINT('',(66.1,7.4,48.5));
#88851=CARTESIAN_POINT('',(66.1,6.,48.35));
#88852=CARTESIAN_POINT('Origin',(65.9,7.4,48.5));
#88853=CARTESIAN_POINT('',(65.9,7.4,48.5));
#88854=CARTESIAN_POINT('',(32.95,7.4,48.5));
#88855=CARTESIAN_POINT('',(65.9,7.4,48.35));
#88856=CARTESIAN_POINT('',(65.9,7.4,48.5));
#88857=CARTESIAN_POINT('',(66.1,7.4,48.35));
#88858=CARTESIAN_POINT('Origin',(65.9,6.,48.5));
#88859=CARTESIAN_POINT('',(65.9,7.,48.5));
#88860=CARTESIAN_POINT('',(65.9,7.4,48.35));
#88861=CARTESIAN_POINT('Origin',(66.,6.7,48.35));
#88862=CARTESIAN_POINT('Origin',(64.1,6.,48.5));
#88863=CARTESIAN_POINT('',(64.1,6.,48.5));
#88864=CARTESIAN_POINT('',(63.9,6.,48.5));
#88865=CARTESIAN_POINT('',(32.05,6.,48.5));
#88866=CARTESIAN_POINT('',(64.1,6.,48.35));
#88867=CARTESIAN_POINT('',(64.1,6.,48.5));
#88868=CARTESIAN_POINT('',(63.9,6.,48.35));
#88869=CARTESIAN_POINT('',(63.9,6.,48.35));
#88870=CARTESIAN_POINT('',(63.9,6.,48.5));
#88871=CARTESIAN_POINT('Origin',(64.1,7.4,48.5));
#88872=CARTESIAN_POINT('',(64.1,7.4,48.5));
#88873=CARTESIAN_POINT('',(64.1,7.7,48.5));
#88874=CARTESIAN_POINT('',(64.1,7.4,48.35));
#88875=CARTESIAN_POINT('',(64.1,7.4,48.5));
#88876=CARTESIAN_POINT('',(64.1,6.,48.35));
#88877=CARTESIAN_POINT('Origin',(63.9,7.4,48.5));
#88878=CARTESIAN_POINT('',(63.9,7.4,48.5));
#88879=CARTESIAN_POINT('',(31.95,7.4,48.5));
#88880=CARTESIAN_POINT('',(63.9,7.4,48.35));
#88881=CARTESIAN_POINT('',(63.9,7.4,48.5));
#88882=CARTESIAN_POINT('',(64.1,7.4,48.35));
#88883=CARTESIAN_POINT('Origin',(63.9,6.,48.5));
#88884=CARTESIAN_POINT('',(63.9,7.,48.5));
#88885=CARTESIAN_POINT('',(63.9,7.4,48.35));
#88886=CARTESIAN_POINT('Origin',(64.,6.7,48.35));
#88887=CARTESIAN_POINT('Origin',(62.1,6.,48.5));
#88888=CARTESIAN_POINT('',(62.1,6.,48.5));
#88889=CARTESIAN_POINT('',(61.9,6.,48.5));
#88890=CARTESIAN_POINT('',(31.05,6.,48.5));
#88891=CARTESIAN_POINT('',(62.1,6.,48.35));
#88892=CARTESIAN_POINT('',(62.1,6.,48.5));
#88893=CARTESIAN_POINT('',(61.9,6.,48.35));
#88894=CARTESIAN_POINT('',(61.9,6.,48.35));
#88895=CARTESIAN_POINT('',(61.9,6.,48.5));
#88896=CARTESIAN_POINT('Origin',(62.1,7.4,48.5));
#88897=CARTESIAN_POINT('',(62.1,7.4,48.5));
#88898=CARTESIAN_POINT('',(62.1,7.7,48.5));
#88899=CARTESIAN_POINT('',(62.1,7.4,48.35));
#88900=CARTESIAN_POINT('',(62.1,7.4,48.5));
#88901=CARTESIAN_POINT('',(62.1,6.,48.35));
#88902=CARTESIAN_POINT('Origin',(61.9,7.4,48.5));
#88903=CARTESIAN_POINT('',(61.9,7.4,48.5));
#88904=CARTESIAN_POINT('',(30.95,7.4,48.5));
#88905=CARTESIAN_POINT('',(61.9,7.4,48.35));
#88906=CARTESIAN_POINT('',(61.9,7.4,48.5));
#88907=CARTESIAN_POINT('',(62.1,7.4,48.35));
#88908=CARTESIAN_POINT('Origin',(61.9,6.,48.5));
#88909=CARTESIAN_POINT('',(61.9,7.,48.5));
#88910=CARTESIAN_POINT('',(61.9,7.4,48.35));
#88911=CARTESIAN_POINT('Origin',(62.,6.7,48.35));
#88912=CARTESIAN_POINT('Origin',(60.1,4.4,48.5));
#88913=CARTESIAN_POINT('',(60.1,4.4,48.5));
#88914=CARTESIAN_POINT('',(59.9,4.4,48.5));
#88915=CARTESIAN_POINT('',(30.05,4.4,48.5));
#88916=CARTESIAN_POINT('',(60.1,4.4,48.35));
#88917=CARTESIAN_POINT('',(60.1,4.4,48.5));
#88918=CARTESIAN_POINT('',(59.9,4.4,48.35));
#88919=CARTESIAN_POINT('',(59.9,4.4,48.35));
#88920=CARTESIAN_POINT('',(59.9,4.4,48.5));
#88921=CARTESIAN_POINT('Origin',(60.1,7.4,48.5));
#88922=CARTESIAN_POINT('',(60.1,7.4,48.5));
#88923=CARTESIAN_POINT('',(60.1,7.7,48.5));
#88924=CARTESIAN_POINT('',(60.1,7.4,48.35));
#88925=CARTESIAN_POINT('',(60.1,7.4,48.5));
#88926=CARTESIAN_POINT('',(60.1,4.4,48.35));
#88927=CARTESIAN_POINT('Origin',(59.9,7.4,48.5));
#88928=CARTESIAN_POINT('',(59.9,7.4,48.5));
#88929=CARTESIAN_POINT('',(29.95,7.4,48.5));
#88930=CARTESIAN_POINT('',(59.9,7.4,48.35));
#88931=CARTESIAN_POINT('',(59.9,7.4,48.5));
#88932=CARTESIAN_POINT('',(60.1,7.4,48.35));
#88933=CARTESIAN_POINT('Origin',(59.9,4.4,48.5));
#88934=CARTESIAN_POINT('',(59.9,6.2,48.5));
#88935=CARTESIAN_POINT('',(59.9,7.4,48.35));
#88936=CARTESIAN_POINT('Origin',(60.,5.9,48.35));
#88937=CARTESIAN_POINT('Origin',(58.1,6.,48.5));
#88938=CARTESIAN_POINT('',(58.1,6.,48.5));
#88939=CARTESIAN_POINT('',(57.9,6.,48.5));
#88940=CARTESIAN_POINT('',(29.05,6.,48.5));
#88941=CARTESIAN_POINT('',(58.1,6.,48.35));
#88942=CARTESIAN_POINT('',(58.1,6.,48.5));
#88943=CARTESIAN_POINT('',(57.9,6.,48.35));
#88944=CARTESIAN_POINT('',(57.9,6.,48.35));
#88945=CARTESIAN_POINT('',(57.9,6.,48.5));
#88946=CARTESIAN_POINT('Origin',(58.1,7.4,48.5));
#88947=CARTESIAN_POINT('',(58.1,7.4,48.5));
#88948=CARTESIAN_POINT('',(58.1,7.7,48.5));
#88949=CARTESIAN_POINT('',(58.1,7.4,48.35));
#88950=CARTESIAN_POINT('',(58.1,7.4,48.5));
#88951=CARTESIAN_POINT('',(58.1,6.,48.35));
#88952=CARTESIAN_POINT('Origin',(57.9,7.4,48.5));
#88953=CARTESIAN_POINT('',(57.9,7.4,48.5));
#88954=CARTESIAN_POINT('',(28.95,7.4,48.5));
#88955=CARTESIAN_POINT('',(57.9,7.4,48.35));
#88956=CARTESIAN_POINT('',(57.9,7.4,48.5));
#88957=CARTESIAN_POINT('',(58.1,7.4,48.35));
#88958=CARTESIAN_POINT('Origin',(57.9,6.,48.5));
#88959=CARTESIAN_POINT('',(57.9,7.,48.5));
#88960=CARTESIAN_POINT('',(57.9,7.4,48.35));
#88961=CARTESIAN_POINT('Origin',(58.,6.7,48.35));
#88962=CARTESIAN_POINT('Origin',(56.1,6.,48.5));
#88963=CARTESIAN_POINT('',(56.1,6.,48.5));
#88964=CARTESIAN_POINT('',(55.9,6.,48.5));
#88965=CARTESIAN_POINT('',(28.05,6.,48.5));
#88966=CARTESIAN_POINT('',(56.1,6.,48.35));
#88967=CARTESIAN_POINT('',(56.1,6.,48.5));
#88968=CARTESIAN_POINT('',(55.9,6.,48.35));
#88969=CARTESIAN_POINT('',(55.9,6.,48.35));
#88970=CARTESIAN_POINT('',(55.9,6.,48.5));
#88971=CARTESIAN_POINT('Origin',(56.1,7.4,48.5));
#88972=CARTESIAN_POINT('',(56.1,7.4,48.5));
#88973=CARTESIAN_POINT('',(56.1,7.7,48.5));
#88974=CARTESIAN_POINT('',(56.1,7.4,48.35));
#88975=CARTESIAN_POINT('',(56.1,7.4,48.5));
#88976=CARTESIAN_POINT('',(56.1,6.,48.35));
#88977=CARTESIAN_POINT('Origin',(55.9,7.4,48.5));
#88978=CARTESIAN_POINT('',(55.9,7.4,48.5));
#88979=CARTESIAN_POINT('',(27.95,7.4,48.5));
#88980=CARTESIAN_POINT('',(55.9,7.4,48.35));
#88981=CARTESIAN_POINT('',(55.9,7.4,48.5));
#88982=CARTESIAN_POINT('',(56.1,7.4,48.35));
#88983=CARTESIAN_POINT('Origin',(55.9,6.,48.5));
#88984=CARTESIAN_POINT('',(55.9,7.,48.5));
#88985=CARTESIAN_POINT('',(55.9,7.4,48.35));
#88986=CARTESIAN_POINT('Origin',(56.,6.7,48.35));
#88987=CARTESIAN_POINT('Origin',(54.1,6.,48.5));
#88988=CARTESIAN_POINT('',(54.1,6.,48.5));
#88989=CARTESIAN_POINT('',(53.9,6.,48.5));
#88990=CARTESIAN_POINT('',(27.05,6.,48.5));
#88991=CARTESIAN_POINT('',(54.1,6.,48.35));
#88992=CARTESIAN_POINT('',(54.1,6.,48.5));
#88993=CARTESIAN_POINT('',(53.9,6.,48.35));
#88994=CARTESIAN_POINT('',(53.9,6.,48.35));
#88995=CARTESIAN_POINT('',(53.9,6.,48.5));
#88996=CARTESIAN_POINT('Origin',(54.1,7.4,48.5));
#88997=CARTESIAN_POINT('',(54.1,7.4,48.5));
#88998=CARTESIAN_POINT('',(54.1,7.7,48.5));
#88999=CARTESIAN_POINT('',(54.1,7.4,48.35));
#89000=CARTESIAN_POINT('',(54.1,7.4,48.5));
#89001=CARTESIAN_POINT('',(54.1,6.,48.35));
#89002=CARTESIAN_POINT('Origin',(53.9,7.4,48.5));
#89003=CARTESIAN_POINT('',(53.9,7.4,48.5));
#89004=CARTESIAN_POINT('',(26.95,7.4,48.5));
#89005=CARTESIAN_POINT('',(53.9,7.4,48.35));
#89006=CARTESIAN_POINT('',(53.9,7.4,48.5));
#89007=CARTESIAN_POINT('',(54.1,7.4,48.35));
#89008=CARTESIAN_POINT('Origin',(53.9,6.,48.5));
#89009=CARTESIAN_POINT('',(53.9,7.,48.5));
#89010=CARTESIAN_POINT('',(53.9,7.4,48.35));
#89011=CARTESIAN_POINT('Origin',(54.,6.7,48.35));
#89012=CARTESIAN_POINT('Origin',(52.1,6.,48.5));
#89013=CARTESIAN_POINT('',(52.1,6.,48.5));
#89014=CARTESIAN_POINT('',(51.9,6.,48.5));
#89015=CARTESIAN_POINT('',(26.05,6.,48.5));
#89016=CARTESIAN_POINT('',(52.1,6.,48.35));
#89017=CARTESIAN_POINT('',(52.1,6.,48.5));
#89018=CARTESIAN_POINT('',(51.9,6.,48.35));
#89019=CARTESIAN_POINT('',(51.9,6.,48.35));
#89020=CARTESIAN_POINT('',(51.9,6.,48.5));
#89021=CARTESIAN_POINT('Origin',(52.1,7.4,48.5));
#89022=CARTESIAN_POINT('',(52.1,7.4,48.5));
#89023=CARTESIAN_POINT('',(52.1,7.7,48.5));
#89024=CARTESIAN_POINT('',(52.1,7.4,48.35));
#89025=CARTESIAN_POINT('',(52.1,7.4,48.5));
#89026=CARTESIAN_POINT('',(52.1,6.,48.35));
#89027=CARTESIAN_POINT('Origin',(51.9,7.4,48.5));
#89028=CARTESIAN_POINT('',(51.9,7.4,48.5));
#89029=CARTESIAN_POINT('',(25.95,7.4,48.5));
#89030=CARTESIAN_POINT('',(51.9,7.4,48.35));
#89031=CARTESIAN_POINT('',(51.9,7.4,48.5));
#89032=CARTESIAN_POINT('',(52.1,7.4,48.35));
#89033=CARTESIAN_POINT('Origin',(51.9,6.,48.5));
#89034=CARTESIAN_POINT('',(51.9,7.,48.5));
#89035=CARTESIAN_POINT('',(51.9,7.4,48.35));
#89036=CARTESIAN_POINT('Origin',(52.,6.7,48.35));
#89037=CARTESIAN_POINT('Origin',(50.1,4.4,48.5));
#89038=CARTESIAN_POINT('',(50.1,4.4,48.5));
#89039=CARTESIAN_POINT('',(49.9,4.4,48.5));
#89040=CARTESIAN_POINT('',(25.05,4.4,48.5));
#89041=CARTESIAN_POINT('',(50.1,4.4,48.35));
#89042=CARTESIAN_POINT('',(50.1,4.4,48.5));
#89043=CARTESIAN_POINT('',(49.9,4.4,48.35));
#89044=CARTESIAN_POINT('',(49.9,4.4,48.35));
#89045=CARTESIAN_POINT('',(49.9,4.4,48.5));
#89046=CARTESIAN_POINT('Origin',(50.1,7.4,48.5));
#89047=CARTESIAN_POINT('',(50.1,7.4,48.5));
#89048=CARTESIAN_POINT('',(50.1,7.7,48.5));
#89049=CARTESIAN_POINT('',(50.1,7.4,48.35));
#89050=CARTESIAN_POINT('',(50.1,7.4,48.5));
#89051=CARTESIAN_POINT('',(50.1,4.4,48.35));
#89052=CARTESIAN_POINT('Origin',(49.9,7.4,48.5));
#89053=CARTESIAN_POINT('',(49.9,7.4,48.5));
#89054=CARTESIAN_POINT('',(24.95,7.4,48.5));
#89055=CARTESIAN_POINT('',(49.9,7.4,48.35));
#89056=CARTESIAN_POINT('',(49.9,7.4,48.5));
#89057=CARTESIAN_POINT('',(50.1,7.4,48.35));
#89058=CARTESIAN_POINT('Origin',(49.9,4.4,48.5));
#89059=CARTESIAN_POINT('',(49.9,6.2,48.5));
#89060=CARTESIAN_POINT('',(49.9,7.4,48.35));
#89061=CARTESIAN_POINT('Origin',(50.,5.9,48.35));
#89062=CARTESIAN_POINT('Origin',(48.1,6.,48.5));
#89063=CARTESIAN_POINT('',(48.1,6.,48.5));
#89064=CARTESIAN_POINT('',(47.9,6.,48.5));
#89065=CARTESIAN_POINT('',(24.05,6.,48.5));
#89066=CARTESIAN_POINT('',(48.1,6.,48.35));
#89067=CARTESIAN_POINT('',(48.1,6.,48.5));
#89068=CARTESIAN_POINT('',(47.9,6.,48.35));
#89069=CARTESIAN_POINT('',(47.9,6.,48.35));
#89070=CARTESIAN_POINT('',(47.9,6.,48.5));
#89071=CARTESIAN_POINT('Origin',(48.1,7.4,48.5));
#89072=CARTESIAN_POINT('',(48.1,7.4,48.5));
#89073=CARTESIAN_POINT('',(48.1,7.7,48.5));
#89074=CARTESIAN_POINT('',(48.1,7.4,48.35));
#89075=CARTESIAN_POINT('',(48.1,7.4,48.5));
#89076=CARTESIAN_POINT('',(48.1,6.,48.35));
#89077=CARTESIAN_POINT('Origin',(47.9,7.4,48.5));
#89078=CARTESIAN_POINT('',(47.9,7.4,48.5));
#89079=CARTESIAN_POINT('',(23.95,7.4,48.5));
#89080=CARTESIAN_POINT('',(47.9,7.4,48.35));
#89081=CARTESIAN_POINT('',(47.9,7.4,48.5));
#89082=CARTESIAN_POINT('',(48.1,7.4,48.35));
#89083=CARTESIAN_POINT('Origin',(47.9,6.,48.5));
#89084=CARTESIAN_POINT('',(47.9,7.,48.5));
#89085=CARTESIAN_POINT('',(47.9,7.4,48.35));
#89086=CARTESIAN_POINT('Origin',(48.,6.7,48.35));
#89087=CARTESIAN_POINT('Origin',(46.1,6.,48.5));
#89088=CARTESIAN_POINT('',(46.1,6.,48.5));
#89089=CARTESIAN_POINT('',(45.9,6.,48.5));
#89090=CARTESIAN_POINT('',(23.05,6.,48.5));
#89091=CARTESIAN_POINT('',(46.1,6.,48.35));
#89092=CARTESIAN_POINT('',(46.1,6.,48.5));
#89093=CARTESIAN_POINT('',(45.9,6.,48.35));
#89094=CARTESIAN_POINT('',(45.9,6.,48.35));
#89095=CARTESIAN_POINT('',(45.9,6.,48.5));
#89096=CARTESIAN_POINT('Origin',(46.1,7.4,48.5));
#89097=CARTESIAN_POINT('',(46.1,7.4,48.5));
#89098=CARTESIAN_POINT('',(46.1,7.7,48.5));
#89099=CARTESIAN_POINT('',(46.1,7.4,48.35));
#89100=CARTESIAN_POINT('',(46.1,7.4,48.5));
#89101=CARTESIAN_POINT('',(46.1,6.,48.35));
#89102=CARTESIAN_POINT('Origin',(45.9,7.4,48.5));
#89103=CARTESIAN_POINT('',(45.9,7.4,48.5));
#89104=CARTESIAN_POINT('',(22.95,7.4,48.5));
#89105=CARTESIAN_POINT('',(45.9,7.4,48.35));
#89106=CARTESIAN_POINT('',(45.9,7.4,48.5));
#89107=CARTESIAN_POINT('',(46.1,7.4,48.35));
#89108=CARTESIAN_POINT('Origin',(45.9,6.,48.5));
#89109=CARTESIAN_POINT('',(45.9,7.,48.5));
#89110=CARTESIAN_POINT('',(45.9,7.4,48.35));
#89111=CARTESIAN_POINT('Origin',(46.,6.7,48.35));
#89112=CARTESIAN_POINT('Origin',(44.1,6.,48.5));
#89113=CARTESIAN_POINT('',(44.1,6.,48.5));
#89114=CARTESIAN_POINT('',(43.9,6.,48.5));
#89115=CARTESIAN_POINT('',(22.05,6.,48.5));
#89116=CARTESIAN_POINT('',(44.1,6.,48.35));
#89117=CARTESIAN_POINT('',(44.1,6.,48.5));
#89118=CARTESIAN_POINT('',(43.9,6.,48.35));
#89119=CARTESIAN_POINT('',(43.9,6.,48.35));
#89120=CARTESIAN_POINT('',(43.9,6.,48.5));
#89121=CARTESIAN_POINT('Origin',(44.1,7.4,48.5));
#89122=CARTESIAN_POINT('',(44.1,7.4,48.5));
#89123=CARTESIAN_POINT('',(44.1,7.7,48.5));
#89124=CARTESIAN_POINT('',(44.1,7.4,48.35));
#89125=CARTESIAN_POINT('',(44.1,7.4,48.5));
#89126=CARTESIAN_POINT('',(44.1,6.,48.35));
#89127=CARTESIAN_POINT('Origin',(43.9,7.4,48.5));
#89128=CARTESIAN_POINT('',(43.9,7.4,48.5));
#89129=CARTESIAN_POINT('',(21.95,7.4,48.5));
#89130=CARTESIAN_POINT('',(43.9,7.4,48.35));
#89131=CARTESIAN_POINT('',(43.9,7.4,48.5));
#89132=CARTESIAN_POINT('',(44.1,7.4,48.35));
#89133=CARTESIAN_POINT('Origin',(43.9,6.,48.5));
#89134=CARTESIAN_POINT('',(43.9,7.,48.5));
#89135=CARTESIAN_POINT('',(43.9,7.4,48.35));
#89136=CARTESIAN_POINT('Origin',(44.,6.7,48.35));
#89137=CARTESIAN_POINT('Origin',(42.1,6.,48.5));
#89138=CARTESIAN_POINT('',(42.1,6.,48.5));
#89139=CARTESIAN_POINT('',(41.9,6.,48.5));
#89140=CARTESIAN_POINT('',(21.05,6.,48.5));
#89141=CARTESIAN_POINT('',(42.1,6.,48.35));
#89142=CARTESIAN_POINT('',(42.1,6.,48.5));
#89143=CARTESIAN_POINT('',(41.9,6.,48.35));
#89144=CARTESIAN_POINT('',(41.9,6.,48.35));
#89145=CARTESIAN_POINT('',(41.9,6.,48.5));
#89146=CARTESIAN_POINT('Origin',(42.1,7.4,48.5));
#89147=CARTESIAN_POINT('',(42.1,7.4,48.5));
#89148=CARTESIAN_POINT('',(42.1,7.7,48.5));
#89149=CARTESIAN_POINT('',(42.1,7.4,48.35));
#89150=CARTESIAN_POINT('',(42.1,7.4,48.5));
#89151=CARTESIAN_POINT('',(42.1,6.,48.35));
#89152=CARTESIAN_POINT('Origin',(41.9,7.4,48.5));
#89153=CARTESIAN_POINT('',(41.9,7.4,48.5));
#89154=CARTESIAN_POINT('',(20.95,7.4,48.5));
#89155=CARTESIAN_POINT('',(41.9,7.4,48.35));
#89156=CARTESIAN_POINT('',(41.9,7.4,48.5));
#89157=CARTESIAN_POINT('',(42.1,7.4,48.35));
#89158=CARTESIAN_POINT('Origin',(41.9,6.,48.5));
#89159=CARTESIAN_POINT('',(41.9,7.,48.5));
#89160=CARTESIAN_POINT('',(41.9,7.4,48.35));
#89161=CARTESIAN_POINT('Origin',(42.,6.7,48.35));
#89162=CARTESIAN_POINT('Origin',(40.1,4.4,48.5));
#89163=CARTESIAN_POINT('',(40.1,4.4,48.5));
#89164=CARTESIAN_POINT('',(39.9,4.4,48.5));
#89165=CARTESIAN_POINT('',(20.05,4.4,48.5));
#89166=CARTESIAN_POINT('',(40.1,4.4,48.35));
#89167=CARTESIAN_POINT('',(40.1,4.4,48.5));
#89168=CARTESIAN_POINT('',(39.9,4.4,48.35));
#89169=CARTESIAN_POINT('',(39.9,4.4,48.35));
#89170=CARTESIAN_POINT('',(39.9,4.4,48.5));
#89171=CARTESIAN_POINT('Origin',(40.1,7.4,48.5));
#89172=CARTESIAN_POINT('',(40.1,7.4,48.5));
#89173=CARTESIAN_POINT('',(40.1,7.7,48.5));
#89174=CARTESIAN_POINT('',(40.1,7.4,48.35));
#89175=CARTESIAN_POINT('',(40.1,7.4,48.5));
#89176=CARTESIAN_POINT('',(40.1,4.4,48.35));
#89177=CARTESIAN_POINT('Origin',(39.9,7.4,48.5));
#89178=CARTESIAN_POINT('',(39.9,7.4,48.5));
#89179=CARTESIAN_POINT('',(19.95,7.4,48.5));
#89180=CARTESIAN_POINT('',(39.9,7.4,48.35));
#89181=CARTESIAN_POINT('',(39.9,7.4,48.5));
#89182=CARTESIAN_POINT('',(40.1,7.4,48.35));
#89183=CARTESIAN_POINT('Origin',(39.9,4.4,48.5));
#89184=CARTESIAN_POINT('',(39.9,6.2,48.5));
#89185=CARTESIAN_POINT('',(39.9,7.4,48.35));
#89186=CARTESIAN_POINT('Origin',(40.,5.9,48.35));
#89187=CARTESIAN_POINT('Origin',(38.1,6.,48.5));
#89188=CARTESIAN_POINT('',(38.1,6.,48.5));
#89189=CARTESIAN_POINT('',(37.9,6.,48.5));
#89190=CARTESIAN_POINT('',(19.05,6.,48.5));
#89191=CARTESIAN_POINT('',(38.1,6.,48.35));
#89192=CARTESIAN_POINT('',(38.1,6.,48.5));
#89193=CARTESIAN_POINT('',(37.9,6.,48.35));
#89194=CARTESIAN_POINT('',(37.9,6.,48.35));
#89195=CARTESIAN_POINT('',(37.9,6.,48.5));
#89196=CARTESIAN_POINT('Origin',(38.1,7.4,48.5));
#89197=CARTESIAN_POINT('',(38.1,7.4,48.5));
#89198=CARTESIAN_POINT('',(38.1,7.7,48.5));
#89199=CARTESIAN_POINT('',(38.1,7.4,48.35));
#89200=CARTESIAN_POINT('',(38.1,7.4,48.5));
#89201=CARTESIAN_POINT('',(38.1,6.,48.35));
#89202=CARTESIAN_POINT('Origin',(37.9,7.4,48.5));
#89203=CARTESIAN_POINT('',(37.9,7.4,48.5));
#89204=CARTESIAN_POINT('',(18.95,7.4,48.5));
#89205=CARTESIAN_POINT('',(37.9,7.4,48.35));
#89206=CARTESIAN_POINT('',(37.9,7.4,48.5));
#89207=CARTESIAN_POINT('',(38.1,7.4,48.35));
#89208=CARTESIAN_POINT('Origin',(37.9,6.,48.5));
#89209=CARTESIAN_POINT('',(37.9,7.,48.5));
#89210=CARTESIAN_POINT('',(37.9,7.4,48.35));
#89211=CARTESIAN_POINT('Origin',(38.,6.7,48.35));
#89212=CARTESIAN_POINT('Origin',(36.1,6.,48.5));
#89213=CARTESIAN_POINT('',(36.1,6.,48.5));
#89214=CARTESIAN_POINT('',(35.9,6.,48.5));
#89215=CARTESIAN_POINT('',(18.05,6.,48.5));
#89216=CARTESIAN_POINT('',(36.1,6.,48.35));
#89217=CARTESIAN_POINT('',(36.1,6.,48.5));
#89218=CARTESIAN_POINT('',(35.9,6.,48.35));
#89219=CARTESIAN_POINT('',(35.9,6.,48.35));
#89220=CARTESIAN_POINT('',(35.9,6.,48.5));
#89221=CARTESIAN_POINT('Origin',(36.1,7.4,48.5));
#89222=CARTESIAN_POINT('',(36.1,7.4,48.5));
#89223=CARTESIAN_POINT('',(36.1,7.7,48.5));
#89224=CARTESIAN_POINT('',(36.1,7.4,48.35));
#89225=CARTESIAN_POINT('',(36.1,7.4,48.5));
#89226=CARTESIAN_POINT('',(36.1,6.,48.35));
#89227=CARTESIAN_POINT('Origin',(35.9,7.4,48.5));
#89228=CARTESIAN_POINT('',(35.9,7.4,48.5));
#89229=CARTESIAN_POINT('',(17.95,7.4,48.5));
#89230=CARTESIAN_POINT('',(35.9,7.4,48.35));
#89231=CARTESIAN_POINT('',(35.9,7.4,48.5));
#89232=CARTESIAN_POINT('',(36.1,7.4,48.35));
#89233=CARTESIAN_POINT('Origin',(35.9,6.,48.5));
#89234=CARTESIAN_POINT('',(35.9,7.,48.5));
#89235=CARTESIAN_POINT('',(35.9,7.4,48.35));
#89236=CARTESIAN_POINT('Origin',(36.,6.7,48.35));
#89237=CARTESIAN_POINT('Origin',(34.1,6.,48.5));
#89238=CARTESIAN_POINT('',(34.1,6.,48.5));
#89239=CARTESIAN_POINT('',(33.9,6.,48.5));
#89240=CARTESIAN_POINT('',(17.05,6.,48.5));
#89241=CARTESIAN_POINT('',(34.1,6.,48.35));
#89242=CARTESIAN_POINT('',(34.1,6.,48.5));
#89243=CARTESIAN_POINT('',(33.9,6.,48.35));
#89244=CARTESIAN_POINT('',(33.9,6.,48.35));
#89245=CARTESIAN_POINT('',(33.9,6.,48.5));
#89246=CARTESIAN_POINT('Origin',(34.1,7.4,48.5));
#89247=CARTESIAN_POINT('',(34.1,7.4,48.5));
#89248=CARTESIAN_POINT('',(34.1,7.7,48.5));
#89249=CARTESIAN_POINT('',(34.1,7.4,48.35));
#89250=CARTESIAN_POINT('',(34.1,7.4,48.5));
#89251=CARTESIAN_POINT('',(34.1,6.,48.35));
#89252=CARTESIAN_POINT('Origin',(33.9,7.4,48.5));
#89253=CARTESIAN_POINT('',(33.9,7.4,48.5));
#89254=CARTESIAN_POINT('',(16.95,7.4,48.5));
#89255=CARTESIAN_POINT('',(33.9,7.4,48.35));
#89256=CARTESIAN_POINT('',(33.9,7.4,48.5));
#89257=CARTESIAN_POINT('',(34.1,7.4,48.35));
#89258=CARTESIAN_POINT('Origin',(33.9,6.,48.5));
#89259=CARTESIAN_POINT('',(33.9,7.,48.5));
#89260=CARTESIAN_POINT('',(33.9,7.4,48.35));
#89261=CARTESIAN_POINT('Origin',(34.,6.7,48.35));
#89262=CARTESIAN_POINT('Origin',(32.1,6.,48.5));
#89263=CARTESIAN_POINT('',(32.1,6.,48.5));
#89264=CARTESIAN_POINT('',(31.9,6.,48.5));
#89265=CARTESIAN_POINT('',(16.05,6.,48.5));
#89266=CARTESIAN_POINT('',(32.1,6.,48.35));
#89267=CARTESIAN_POINT('',(32.1,6.,48.5));
#89268=CARTESIAN_POINT('',(31.9,6.,48.35));
#89269=CARTESIAN_POINT('',(31.9,6.,48.35));
#89270=CARTESIAN_POINT('',(31.9,6.,48.5));
#89271=CARTESIAN_POINT('Origin',(32.1,7.4,48.5));
#89272=CARTESIAN_POINT('',(32.1,7.4,48.5));
#89273=CARTESIAN_POINT('',(32.1,7.7,48.5));
#89274=CARTESIAN_POINT('',(32.1,7.4,48.35));
#89275=CARTESIAN_POINT('',(32.1,7.4,48.5));
#89276=CARTESIAN_POINT('',(32.1,6.,48.35));
#89277=CARTESIAN_POINT('Origin',(31.9,7.4,48.5));
#89278=CARTESIAN_POINT('',(31.9,7.4,48.5));
#89279=CARTESIAN_POINT('',(15.95,7.4,48.5));
#89280=CARTESIAN_POINT('',(31.9,7.4,48.35));
#89281=CARTESIAN_POINT('',(31.9,7.4,48.5));
#89282=CARTESIAN_POINT('',(32.1,7.4,48.35));
#89283=CARTESIAN_POINT('Origin',(31.9,6.,48.5));
#89284=CARTESIAN_POINT('',(31.9,7.,48.5));
#89285=CARTESIAN_POINT('',(31.9,7.4,48.35));
#89286=CARTESIAN_POINT('Origin',(32.,6.7,48.35));
#89287=CARTESIAN_POINT('Origin',(30.1,4.4,48.5));
#89288=CARTESIAN_POINT('',(30.1,4.4,48.5));
#89289=CARTESIAN_POINT('',(29.9,4.4,48.5));
#89290=CARTESIAN_POINT('',(15.05,4.4,48.5));
#89291=CARTESIAN_POINT('',(30.1,4.4,48.35));
#89292=CARTESIAN_POINT('',(30.1,4.4,48.5));
#89293=CARTESIAN_POINT('',(29.9,4.4,48.35));
#89294=CARTESIAN_POINT('',(29.9,4.4,48.35));
#89295=CARTESIAN_POINT('',(29.9,4.4,48.5));
#89296=CARTESIAN_POINT('Origin',(30.1,7.4,48.5));
#89297=CARTESIAN_POINT('',(30.1,7.4,48.5));
#89298=CARTESIAN_POINT('',(30.1,7.7,48.5));
#89299=CARTESIAN_POINT('',(30.1,7.4,48.35));
#89300=CARTESIAN_POINT('',(30.1,7.4,48.5));
#89301=CARTESIAN_POINT('',(30.1,4.4,48.35));
#89302=CARTESIAN_POINT('Origin',(29.9,7.4,48.5));
#89303=CARTESIAN_POINT('',(29.9,7.4,48.5));
#89304=CARTESIAN_POINT('',(14.95,7.4,48.5));
#89305=CARTESIAN_POINT('',(29.9,7.4,48.35));
#89306=CARTESIAN_POINT('',(29.9,7.4,48.5));
#89307=CARTESIAN_POINT('',(30.1,7.4,48.35));
#89308=CARTESIAN_POINT('Origin',(29.9,4.4,48.5));
#89309=CARTESIAN_POINT('',(29.9,6.2,48.5));
#89310=CARTESIAN_POINT('',(29.9,7.4,48.35));
#89311=CARTESIAN_POINT('Origin',(30.,5.9,48.35));
#89312=CARTESIAN_POINT('Origin',(28.1,6.,48.5));
#89313=CARTESIAN_POINT('',(28.1,6.,48.5));
#89314=CARTESIAN_POINT('',(27.9,6.,48.5));
#89315=CARTESIAN_POINT('',(14.05,6.,48.5));
#89316=CARTESIAN_POINT('',(28.1,6.,48.35));
#89317=CARTESIAN_POINT('',(28.1,6.,48.5));
#89318=CARTESIAN_POINT('',(27.9,6.,48.35));
#89319=CARTESIAN_POINT('',(27.9,6.,48.35));
#89320=CARTESIAN_POINT('',(27.9,6.,48.5));
#89321=CARTESIAN_POINT('Origin',(28.1,7.4,48.5));
#89322=CARTESIAN_POINT('',(28.1,7.4,48.5));
#89323=CARTESIAN_POINT('',(28.1,7.7,48.5));
#89324=CARTESIAN_POINT('',(28.1,7.4,48.35));
#89325=CARTESIAN_POINT('',(28.1,7.4,48.5));
#89326=CARTESIAN_POINT('',(28.1,6.,48.35));
#89327=CARTESIAN_POINT('Origin',(27.9,7.4,48.5));
#89328=CARTESIAN_POINT('',(27.9,7.4,48.5));
#89329=CARTESIAN_POINT('',(13.95,7.4,48.5));
#89330=CARTESIAN_POINT('',(27.9,7.4,48.35));
#89331=CARTESIAN_POINT('',(27.9,7.4,48.5));
#89332=CARTESIAN_POINT('',(28.1,7.4,48.35));
#89333=CARTESIAN_POINT('Origin',(27.9,6.,48.5));
#89334=CARTESIAN_POINT('',(27.9,7.,48.5));
#89335=CARTESIAN_POINT('',(27.9,7.4,48.35));
#89336=CARTESIAN_POINT('Origin',(28.,6.7,48.35));
#89337=CARTESIAN_POINT('Origin',(26.1,6.,48.5));
#89338=CARTESIAN_POINT('',(26.1,6.,48.5));
#89339=CARTESIAN_POINT('',(25.9,6.,48.5));
#89340=CARTESIAN_POINT('',(13.05,6.,48.5));
#89341=CARTESIAN_POINT('',(26.1,6.,48.35));
#89342=CARTESIAN_POINT('',(26.1,6.,48.5));
#89343=CARTESIAN_POINT('',(25.9,6.,48.35));
#89344=CARTESIAN_POINT('',(25.9,6.,48.35));
#89345=CARTESIAN_POINT('',(25.9,6.,48.5));
#89346=CARTESIAN_POINT('Origin',(26.1,7.4,48.5));
#89347=CARTESIAN_POINT('',(26.1,7.4,48.5));
#89348=CARTESIAN_POINT('',(26.1,7.7,48.5));
#89349=CARTESIAN_POINT('',(26.1,7.4,48.35));
#89350=CARTESIAN_POINT('',(26.1,7.4,48.5));
#89351=CARTESIAN_POINT('',(26.1,6.,48.35));
#89352=CARTESIAN_POINT('Origin',(25.9,7.4,48.5));
#89353=CARTESIAN_POINT('',(25.9,7.4,48.5));
#89354=CARTESIAN_POINT('',(12.95,7.4,48.5));
#89355=CARTESIAN_POINT('',(25.9,7.4,48.35));
#89356=CARTESIAN_POINT('',(25.9,7.4,48.5));
#89357=CARTESIAN_POINT('',(26.1,7.4,48.35));
#89358=CARTESIAN_POINT('Origin',(25.9,6.,48.5));
#89359=CARTESIAN_POINT('',(25.9,7.,48.5));
#89360=CARTESIAN_POINT('',(25.9,7.4,48.35));
#89361=CARTESIAN_POINT('Origin',(26.,6.7,48.35));
#89362=CARTESIAN_POINT('Origin',(24.1,6.,48.5));
#89363=CARTESIAN_POINT('',(24.1,6.,48.5));
#89364=CARTESIAN_POINT('',(23.9,6.,48.5));
#89365=CARTESIAN_POINT('',(12.05,6.,48.5));
#89366=CARTESIAN_POINT('',(24.1,6.,48.35));
#89367=CARTESIAN_POINT('',(24.1,6.,48.5));
#89368=CARTESIAN_POINT('',(23.9,6.,48.35));
#89369=CARTESIAN_POINT('',(23.9,6.,48.35));
#89370=CARTESIAN_POINT('',(23.9,6.,48.5));
#89371=CARTESIAN_POINT('Origin',(24.1,7.4,48.5));
#89372=CARTESIAN_POINT('',(24.1,7.4,48.5));
#89373=CARTESIAN_POINT('',(24.1,7.7,48.5));
#89374=CARTESIAN_POINT('',(24.1,7.4,48.35));
#89375=CARTESIAN_POINT('',(24.1,7.4,48.5));
#89376=CARTESIAN_POINT('',(24.1,6.,48.35));
#89377=CARTESIAN_POINT('Origin',(23.9,7.4,48.5));
#89378=CARTESIAN_POINT('',(23.9,7.4,48.5));
#89379=CARTESIAN_POINT('',(11.95,7.4,48.5));
#89380=CARTESIAN_POINT('',(23.9,7.4,48.35));
#89381=CARTESIAN_POINT('',(23.9,7.4,48.5));
#89382=CARTESIAN_POINT('',(24.1,7.4,48.35));
#89383=CARTESIAN_POINT('Origin',(23.9,6.,48.5));
#89384=CARTESIAN_POINT('',(23.9,7.,48.5));
#89385=CARTESIAN_POINT('',(23.9,7.4,48.35));
#89386=CARTESIAN_POINT('Origin',(24.,6.7,48.35));
#89387=CARTESIAN_POINT('Origin',(22.1,6.,48.5));
#89388=CARTESIAN_POINT('',(22.1,6.,48.5));
#89389=CARTESIAN_POINT('',(21.9,6.,48.5));
#89390=CARTESIAN_POINT('',(11.05,6.,48.5));
#89391=CARTESIAN_POINT('',(22.1,6.,48.35));
#89392=CARTESIAN_POINT('',(22.1,6.,48.5));
#89393=CARTESIAN_POINT('',(21.9,6.,48.35));
#89394=CARTESIAN_POINT('',(21.9,6.,48.35));
#89395=CARTESIAN_POINT('',(21.9,6.,48.5));
#89396=CARTESIAN_POINT('Origin',(22.1,7.4,48.5));
#89397=CARTESIAN_POINT('',(22.1,7.4,48.5));
#89398=CARTESIAN_POINT('',(22.1,7.7,48.5));
#89399=CARTESIAN_POINT('',(22.1,7.4,48.35));
#89400=CARTESIAN_POINT('',(22.1,7.4,48.5));
#89401=CARTESIAN_POINT('',(22.1,6.,48.35));
#89402=CARTESIAN_POINT('Origin',(21.9,7.4,48.5));
#89403=CARTESIAN_POINT('',(21.9,7.4,48.5));
#89404=CARTESIAN_POINT('',(10.95,7.4,48.5));
#89405=CARTESIAN_POINT('',(21.9,7.4,48.35));
#89406=CARTESIAN_POINT('',(21.9,7.4,48.5));
#89407=CARTESIAN_POINT('',(22.1,7.4,48.35));
#89408=CARTESIAN_POINT('Origin',(21.9,6.,48.5));
#89409=CARTESIAN_POINT('',(21.9,7.,48.5));
#89410=CARTESIAN_POINT('',(21.9,7.4,48.35));
#89411=CARTESIAN_POINT('Origin',(22.,6.7,48.35));
#89412=CARTESIAN_POINT('Origin',(21.1,6.,48.5));
#89413=CARTESIAN_POINT('',(21.1,6.,48.5));
#89414=CARTESIAN_POINT('',(20.9,6.,48.5));
#89415=CARTESIAN_POINT('',(10.55,6.,48.5));
#89416=CARTESIAN_POINT('',(21.1,6.,48.35));
#89417=CARTESIAN_POINT('',(21.1,6.,48.5));
#89418=CARTESIAN_POINT('',(20.9,6.,48.35));
#89419=CARTESIAN_POINT('',(20.9,6.,48.35));
#89420=CARTESIAN_POINT('',(20.9,6.,48.5));
#89421=CARTESIAN_POINT('Origin',(21.1,7.4,48.5));
#89422=CARTESIAN_POINT('',(21.1,7.4,48.5));
#89423=CARTESIAN_POINT('',(21.1,7.7,48.5));
#89424=CARTESIAN_POINT('',(21.1,7.4,48.35));
#89425=CARTESIAN_POINT('',(21.1,7.4,48.5));
#89426=CARTESIAN_POINT('',(21.1,6.,48.35));
#89427=CARTESIAN_POINT('Origin',(20.9,7.4,48.5));
#89428=CARTESIAN_POINT('',(20.9,7.4,48.5));
#89429=CARTESIAN_POINT('',(10.45,7.4,48.5));
#89430=CARTESIAN_POINT('',(20.9,7.4,48.35));
#89431=CARTESIAN_POINT('',(20.9,7.4,48.5));
#89432=CARTESIAN_POINT('',(21.1,7.4,48.35));
#89433=CARTESIAN_POINT('Origin',(20.9,6.,48.5));
#89434=CARTESIAN_POINT('',(20.9,7.,48.5));
#89435=CARTESIAN_POINT('',(20.9,7.4,48.35));
#89436=CARTESIAN_POINT('Origin',(21.,6.7,48.35));
#89437=CARTESIAN_POINT('Origin',(23.1,6.,48.5));
#89438=CARTESIAN_POINT('',(23.1,6.,48.5));
#89439=CARTESIAN_POINT('',(22.9,6.,48.5));
#89440=CARTESIAN_POINT('',(11.55,6.,48.5));
#89441=CARTESIAN_POINT('',(23.1,6.,48.35));
#89442=CARTESIAN_POINT('',(23.1,6.,48.5));
#89443=CARTESIAN_POINT('',(22.9,6.,48.35));
#89444=CARTESIAN_POINT('',(22.9,6.,48.35));
#89445=CARTESIAN_POINT('',(22.9,6.,48.5));
#89446=CARTESIAN_POINT('Origin',(23.1,7.4,48.5));
#89447=CARTESIAN_POINT('',(23.1,7.4,48.5));
#89448=CARTESIAN_POINT('',(23.1,7.7,48.5));
#89449=CARTESIAN_POINT('',(23.1,7.4,48.35));
#89450=CARTESIAN_POINT('',(23.1,7.4,48.5));
#89451=CARTESIAN_POINT('',(23.1,6.,48.35));
#89452=CARTESIAN_POINT('Origin',(22.9,7.4,48.5));
#89453=CARTESIAN_POINT('',(22.9,7.4,48.5));
#89454=CARTESIAN_POINT('',(11.45,7.4,48.5));
#89455=CARTESIAN_POINT('',(22.9,7.4,48.35));
#89456=CARTESIAN_POINT('',(22.9,7.4,48.5));
#89457=CARTESIAN_POINT('',(23.1,7.4,48.35));
#89458=CARTESIAN_POINT('Origin',(22.9,6.,48.5));
#89459=CARTESIAN_POINT('',(22.9,7.,48.5));
#89460=CARTESIAN_POINT('',(22.9,7.4,48.35));
#89461=CARTESIAN_POINT('Origin',(23.,6.7,48.35));
#89462=CARTESIAN_POINT('Origin',(25.1,5.2,48.5));
#89463=CARTESIAN_POINT('',(25.1,5.2,48.5));
#89464=CARTESIAN_POINT('',(24.9,5.2,48.5));
#89465=CARTESIAN_POINT('',(12.55,5.2,48.5));
#89466=CARTESIAN_POINT('',(25.1,5.2,48.35));
#89467=CARTESIAN_POINT('',(25.1,5.2,48.5));
#89468=CARTESIAN_POINT('',(24.9,5.2,48.35));
#89469=CARTESIAN_POINT('',(24.9,5.2,48.35));
#89470=CARTESIAN_POINT('',(24.9,5.2,48.5));
#89471=CARTESIAN_POINT('Origin',(25.1,7.4,48.5));
#89472=CARTESIAN_POINT('',(25.1,7.4,48.5));
#89473=CARTESIAN_POINT('',(25.1,7.7,48.5));
#89474=CARTESIAN_POINT('',(25.1,7.4,48.35));
#89475=CARTESIAN_POINT('',(25.1,7.4,48.5));
#89476=CARTESIAN_POINT('',(25.1,5.2,48.35));
#89477=CARTESIAN_POINT('Origin',(24.9,7.4,48.5));
#89478=CARTESIAN_POINT('',(24.9,7.4,48.5));
#89479=CARTESIAN_POINT('',(12.45,7.4,48.5));
#89480=CARTESIAN_POINT('',(24.9,7.4,48.35));
#89481=CARTESIAN_POINT('',(24.9,7.4,48.5));
#89482=CARTESIAN_POINT('',(25.1,7.4,48.35));
#89483=CARTESIAN_POINT('Origin',(24.9,5.2,48.5));
#89484=CARTESIAN_POINT('',(24.9,6.6,48.5));
#89485=CARTESIAN_POINT('',(24.9,7.4,48.35));
#89486=CARTESIAN_POINT('Origin',(25.,6.3,48.35));
#89487=CARTESIAN_POINT('Origin',(27.1,6.,48.5));
#89488=CARTESIAN_POINT('',(27.1,6.,48.5));
#89489=CARTESIAN_POINT('',(26.9,6.,48.5));
#89490=CARTESIAN_POINT('',(13.55,6.,48.5));
#89491=CARTESIAN_POINT('',(27.1,6.,48.35));
#89492=CARTESIAN_POINT('',(27.1,6.,48.5));
#89493=CARTESIAN_POINT('',(26.9,6.,48.35));
#89494=CARTESIAN_POINT('',(26.9,6.,48.35));
#89495=CARTESIAN_POINT('',(26.9,6.,48.5));
#89496=CARTESIAN_POINT('Origin',(27.1,7.4,48.5));
#89497=CARTESIAN_POINT('',(27.1,7.4,48.5));
#89498=CARTESIAN_POINT('',(27.1,7.7,48.5));
#89499=CARTESIAN_POINT('',(27.1,7.4,48.35));
#89500=CARTESIAN_POINT('',(27.1,7.4,48.5));
#89501=CARTESIAN_POINT('',(27.1,6.,48.35));
#89502=CARTESIAN_POINT('Origin',(26.9,7.4,48.5));
#89503=CARTESIAN_POINT('',(26.9,7.4,48.5));
#89504=CARTESIAN_POINT('',(13.45,7.4,48.5));
#89505=CARTESIAN_POINT('',(26.9,7.4,48.35));
#89506=CARTESIAN_POINT('',(26.9,7.4,48.5));
#89507=CARTESIAN_POINT('',(27.1,7.4,48.35));
#89508=CARTESIAN_POINT('Origin',(26.9,6.,48.5));
#89509=CARTESIAN_POINT('',(26.9,7.,48.5));
#89510=CARTESIAN_POINT('',(26.9,7.4,48.35));
#89511=CARTESIAN_POINT('Origin',(27.,6.7,48.35));
#89512=CARTESIAN_POINT('Origin',(29.1,6.,48.5));
#89513=CARTESIAN_POINT('',(29.1,6.,48.5));
#89514=CARTESIAN_POINT('',(28.9,6.,48.5));
#89515=CARTESIAN_POINT('',(14.55,6.,48.5));
#89516=CARTESIAN_POINT('',(29.1,6.,48.35));
#89517=CARTESIAN_POINT('',(29.1,6.,48.5));
#89518=CARTESIAN_POINT('',(28.9,6.,48.35));
#89519=CARTESIAN_POINT('',(28.9,6.,48.35));
#89520=CARTESIAN_POINT('',(28.9,6.,48.5));
#89521=CARTESIAN_POINT('Origin',(29.1,7.4,48.5));
#89522=CARTESIAN_POINT('',(29.1,7.4,48.5));
#89523=CARTESIAN_POINT('',(29.1,7.7,48.5));
#89524=CARTESIAN_POINT('',(29.1,7.4,48.35));
#89525=CARTESIAN_POINT('',(29.1,7.4,48.5));
#89526=CARTESIAN_POINT('',(29.1,6.,48.35));
#89527=CARTESIAN_POINT('Origin',(28.9,7.4,48.5));
#89528=CARTESIAN_POINT('',(28.9,7.4,48.5));
#89529=CARTESIAN_POINT('',(14.45,7.4,48.5));
#89530=CARTESIAN_POINT('',(28.9,7.4,48.35));
#89531=CARTESIAN_POINT('',(28.9,7.4,48.5));
#89532=CARTESIAN_POINT('',(29.1,7.4,48.35));
#89533=CARTESIAN_POINT('Origin',(28.9,6.,48.5));
#89534=CARTESIAN_POINT('',(28.9,7.,48.5));
#89535=CARTESIAN_POINT('',(28.9,7.4,48.35));
#89536=CARTESIAN_POINT('Origin',(29.,6.7,48.35));
#89537=CARTESIAN_POINT('Origin',(31.1,6.,48.5));
#89538=CARTESIAN_POINT('',(31.1,6.,48.5));
#89539=CARTESIAN_POINT('',(30.9,6.,48.5));
#89540=CARTESIAN_POINT('',(15.55,6.,48.5));
#89541=CARTESIAN_POINT('',(31.1,6.,48.35));
#89542=CARTESIAN_POINT('',(31.1,6.,48.5));
#89543=CARTESIAN_POINT('',(30.9,6.,48.35));
#89544=CARTESIAN_POINT('',(30.9,6.,48.35));
#89545=CARTESIAN_POINT('',(30.9,6.,48.5));
#89546=CARTESIAN_POINT('Origin',(31.1,7.4,48.5));
#89547=CARTESIAN_POINT('',(31.1,7.4,48.5));
#89548=CARTESIAN_POINT('',(31.1,7.7,48.5));
#89549=CARTESIAN_POINT('',(31.1,7.4,48.35));
#89550=CARTESIAN_POINT('',(31.1,7.4,48.5));
#89551=CARTESIAN_POINT('',(31.1,6.,48.35));
#89552=CARTESIAN_POINT('Origin',(30.9,7.4,48.5));
#89553=CARTESIAN_POINT('',(30.9,7.4,48.5));
#89554=CARTESIAN_POINT('',(15.45,7.4,48.5));
#89555=CARTESIAN_POINT('',(30.9,7.4,48.35));
#89556=CARTESIAN_POINT('',(30.9,7.4,48.5));
#89557=CARTESIAN_POINT('',(31.1,7.4,48.35));
#89558=CARTESIAN_POINT('Origin',(30.9,6.,48.5));
#89559=CARTESIAN_POINT('',(30.9,7.,48.5));
#89560=CARTESIAN_POINT('',(30.9,7.4,48.35));
#89561=CARTESIAN_POINT('Origin',(31.,6.7,48.35));
#89562=CARTESIAN_POINT('Origin',(33.1,6.,48.5));
#89563=CARTESIAN_POINT('',(33.1,6.,48.5));
#89564=CARTESIAN_POINT('',(32.9,6.,48.5));
#89565=CARTESIAN_POINT('',(16.55,6.,48.5));
#89566=CARTESIAN_POINT('',(33.1,6.,48.35));
#89567=CARTESIAN_POINT('',(33.1,6.,48.5));
#89568=CARTESIAN_POINT('',(32.9,6.,48.35));
#89569=CARTESIAN_POINT('',(32.9,6.,48.35));
#89570=CARTESIAN_POINT('',(32.9,6.,48.5));
#89571=CARTESIAN_POINT('Origin',(33.1,7.4,48.5));
#89572=CARTESIAN_POINT('',(33.1,7.4,48.5));
#89573=CARTESIAN_POINT('',(33.1,7.7,48.5));
#89574=CARTESIAN_POINT('',(33.1,7.4,48.35));
#89575=CARTESIAN_POINT('',(33.1,7.4,48.5));
#89576=CARTESIAN_POINT('',(33.1,6.,48.35));
#89577=CARTESIAN_POINT('Origin',(32.9,7.4,48.5));
#89578=CARTESIAN_POINT('',(32.9,7.4,48.5));
#89579=CARTESIAN_POINT('',(16.45,7.4,48.5));
#89580=CARTESIAN_POINT('',(32.9,7.4,48.35));
#89581=CARTESIAN_POINT('',(32.9,7.4,48.5));
#89582=CARTESIAN_POINT('',(33.1,7.4,48.35));
#89583=CARTESIAN_POINT('Origin',(32.9,6.,48.5));
#89584=CARTESIAN_POINT('',(32.9,7.,48.5));
#89585=CARTESIAN_POINT('',(32.9,7.4,48.35));
#89586=CARTESIAN_POINT('Origin',(33.,6.7,48.35));
#89587=CARTESIAN_POINT('Origin',(35.1,5.2,48.5));
#89588=CARTESIAN_POINT('',(35.1,5.2,48.5));
#89589=CARTESIAN_POINT('',(34.9,5.2,48.5));
#89590=CARTESIAN_POINT('',(17.55,5.2,48.5));
#89591=CARTESIAN_POINT('',(35.1,5.2,48.35));
#89592=CARTESIAN_POINT('',(35.1,5.2,48.5));
#89593=CARTESIAN_POINT('',(34.9,5.2,48.35));
#89594=CARTESIAN_POINT('',(34.9,5.2,48.35));
#89595=CARTESIAN_POINT('',(34.9,5.2,48.5));
#89596=CARTESIAN_POINT('Origin',(35.1,7.4,48.5));
#89597=CARTESIAN_POINT('',(35.1,7.4,48.5));
#89598=CARTESIAN_POINT('',(35.1,7.7,48.5));
#89599=CARTESIAN_POINT('',(35.1,7.4,48.35));
#89600=CARTESIAN_POINT('',(35.1,7.4,48.5));
#89601=CARTESIAN_POINT('',(35.1,5.2,48.35));
#89602=CARTESIAN_POINT('Origin',(34.9,7.4,48.5));
#89603=CARTESIAN_POINT('',(34.9,7.4,48.5));
#89604=CARTESIAN_POINT('',(17.45,7.4,48.5));
#89605=CARTESIAN_POINT('',(34.9,7.4,48.35));
#89606=CARTESIAN_POINT('',(34.9,7.4,48.5));
#89607=CARTESIAN_POINT('',(35.1,7.4,48.35));
#89608=CARTESIAN_POINT('Origin',(34.9,5.2,48.5));
#89609=CARTESIAN_POINT('',(34.9,6.6,48.5));
#89610=CARTESIAN_POINT('',(34.9,7.4,48.35));
#89611=CARTESIAN_POINT('Origin',(35.,6.3,48.35));
#89612=CARTESIAN_POINT('Origin',(37.1,6.,48.5));
#89613=CARTESIAN_POINT('',(37.1,6.,48.5));
#89614=CARTESIAN_POINT('',(36.9,6.,48.5));
#89615=CARTESIAN_POINT('',(18.55,6.,48.5));
#89616=CARTESIAN_POINT('',(37.1,6.,48.35));
#89617=CARTESIAN_POINT('',(37.1,6.,48.5));
#89618=CARTESIAN_POINT('',(36.9,6.,48.35));
#89619=CARTESIAN_POINT('',(36.9,6.,48.35));
#89620=CARTESIAN_POINT('',(36.9,6.,48.5));
#89621=CARTESIAN_POINT('Origin',(37.1,7.4,48.5));
#89622=CARTESIAN_POINT('',(37.1,7.4,48.5));
#89623=CARTESIAN_POINT('',(37.1,7.7,48.5));
#89624=CARTESIAN_POINT('',(37.1,7.4,48.35));
#89625=CARTESIAN_POINT('',(37.1,7.4,48.5));
#89626=CARTESIAN_POINT('',(37.1,6.,48.35));
#89627=CARTESIAN_POINT('Origin',(36.9,7.4,48.5));
#89628=CARTESIAN_POINT('',(36.9,7.4,48.5));
#89629=CARTESIAN_POINT('',(18.45,7.4,48.5));
#89630=CARTESIAN_POINT('',(36.9,7.4,48.35));
#89631=CARTESIAN_POINT('',(36.9,7.4,48.5));
#89632=CARTESIAN_POINT('',(37.1,7.4,48.35));
#89633=CARTESIAN_POINT('Origin',(36.9,6.,48.5));
#89634=CARTESIAN_POINT('',(36.9,7.,48.5));
#89635=CARTESIAN_POINT('',(36.9,7.4,48.35));
#89636=CARTESIAN_POINT('Origin',(37.,6.7,48.35));
#89637=CARTESIAN_POINT('Origin',(39.1,6.,48.5));
#89638=CARTESIAN_POINT('',(39.1,6.,48.5));
#89639=CARTESIAN_POINT('',(38.9,6.,48.5));
#89640=CARTESIAN_POINT('',(19.55,6.,48.5));
#89641=CARTESIAN_POINT('',(39.1,6.,48.35));
#89642=CARTESIAN_POINT('',(39.1,6.,48.5));
#89643=CARTESIAN_POINT('',(38.9,6.,48.35));
#89644=CARTESIAN_POINT('',(38.9,6.,48.35));
#89645=CARTESIAN_POINT('',(38.9,6.,48.5));
#89646=CARTESIAN_POINT('Origin',(39.1,7.4,48.5));
#89647=CARTESIAN_POINT('',(39.1,7.4,48.5));
#89648=CARTESIAN_POINT('',(39.1,7.7,48.5));
#89649=CARTESIAN_POINT('',(39.1,7.4,48.35));
#89650=CARTESIAN_POINT('',(39.1,7.4,48.5));
#89651=CARTESIAN_POINT('',(39.1,6.,48.35));
#89652=CARTESIAN_POINT('Origin',(38.9,7.4,48.5));
#89653=CARTESIAN_POINT('',(38.9,7.4,48.5));
#89654=CARTESIAN_POINT('',(19.45,7.4,48.5));
#89655=CARTESIAN_POINT('',(38.9,7.4,48.35));
#89656=CARTESIAN_POINT('',(38.9,7.4,48.5));
#89657=CARTESIAN_POINT('',(39.1,7.4,48.35));
#89658=CARTESIAN_POINT('Origin',(38.9,6.,48.5));
#89659=CARTESIAN_POINT('',(38.9,7.,48.5));
#89660=CARTESIAN_POINT('',(38.9,7.4,48.35));
#89661=CARTESIAN_POINT('Origin',(39.,6.7,48.35));
#89662=CARTESIAN_POINT('Origin',(41.1,6.,48.5));
#89663=CARTESIAN_POINT('',(41.1,6.,48.5));
#89664=CARTESIAN_POINT('',(40.9,6.,48.5));
#89665=CARTESIAN_POINT('',(20.55,6.,48.5));
#89666=CARTESIAN_POINT('',(41.1,6.,48.35));
#89667=CARTESIAN_POINT('',(41.1,6.,48.5));
#89668=CARTESIAN_POINT('',(40.9,6.,48.35));
#89669=CARTESIAN_POINT('',(40.9,6.,48.35));
#89670=CARTESIAN_POINT('',(40.9,6.,48.5));
#89671=CARTESIAN_POINT('Origin',(41.1,7.4,48.5));
#89672=CARTESIAN_POINT('',(41.1,7.4,48.5));
#89673=CARTESIAN_POINT('',(41.1,7.7,48.5));
#89674=CARTESIAN_POINT('',(41.1,7.4,48.35));
#89675=CARTESIAN_POINT('',(41.1,7.4,48.5));
#89676=CARTESIAN_POINT('',(41.1,6.,48.35));
#89677=CARTESIAN_POINT('Origin',(40.9,7.4,48.5));
#89678=CARTESIAN_POINT('',(40.9,7.4,48.5));
#89679=CARTESIAN_POINT('',(20.45,7.4,48.5));
#89680=CARTESIAN_POINT('',(40.9,7.4,48.35));
#89681=CARTESIAN_POINT('',(40.9,7.4,48.5));
#89682=CARTESIAN_POINT('',(41.1,7.4,48.35));
#89683=CARTESIAN_POINT('Origin',(40.9,6.,48.5));
#89684=CARTESIAN_POINT('',(40.9,7.,48.5));
#89685=CARTESIAN_POINT('',(40.9,7.4,48.35));
#89686=CARTESIAN_POINT('Origin',(41.,6.7,48.35));
#89687=CARTESIAN_POINT('Origin',(43.1,6.,48.5));
#89688=CARTESIAN_POINT('',(43.1,6.,48.5));
#89689=CARTESIAN_POINT('',(42.9,6.,48.5));
#89690=CARTESIAN_POINT('',(21.55,6.,48.5));
#89691=CARTESIAN_POINT('',(43.1,6.,48.35));
#89692=CARTESIAN_POINT('',(43.1,6.,48.5));
#89693=CARTESIAN_POINT('',(42.9,6.,48.35));
#89694=CARTESIAN_POINT('',(42.9,6.,48.35));
#89695=CARTESIAN_POINT('',(42.9,6.,48.5));
#89696=CARTESIAN_POINT('Origin',(43.1,7.4,48.5));
#89697=CARTESIAN_POINT('',(43.1,7.4,48.5));
#89698=CARTESIAN_POINT('',(43.1,7.7,48.5));
#89699=CARTESIAN_POINT('',(43.1,7.4,48.35));
#89700=CARTESIAN_POINT('',(43.1,7.4,48.5));
#89701=CARTESIAN_POINT('',(43.1,6.,48.35));
#89702=CARTESIAN_POINT('Origin',(42.9,7.4,48.5));
#89703=CARTESIAN_POINT('',(42.9,7.4,48.5));
#89704=CARTESIAN_POINT('',(21.45,7.4,48.5));
#89705=CARTESIAN_POINT('',(42.9,7.4,48.35));
#89706=CARTESIAN_POINT('',(42.9,7.4,48.5));
#89707=CARTESIAN_POINT('',(43.1,7.4,48.35));
#89708=CARTESIAN_POINT('Origin',(42.9,6.,48.5));
#89709=CARTESIAN_POINT('',(42.9,7.,48.5));
#89710=CARTESIAN_POINT('',(42.9,7.4,48.35));
#89711=CARTESIAN_POINT('Origin',(43.,6.7,48.35));
#89712=CARTESIAN_POINT('Origin',(45.1,5.2,48.5));
#89713=CARTESIAN_POINT('',(45.1,5.2,48.5));
#89714=CARTESIAN_POINT('',(44.9,5.2,48.5));
#89715=CARTESIAN_POINT('',(22.55,5.2,48.5));
#89716=CARTESIAN_POINT('',(45.1,5.2,48.35));
#89717=CARTESIAN_POINT('',(45.1,5.2,48.5));
#89718=CARTESIAN_POINT('',(44.9,5.2,48.35));
#89719=CARTESIAN_POINT('',(44.9,5.2,48.35));
#89720=CARTESIAN_POINT('',(44.9,5.2,48.5));
#89721=CARTESIAN_POINT('Origin',(45.1,7.4,48.5));
#89722=CARTESIAN_POINT('',(45.1,7.4,48.5));
#89723=CARTESIAN_POINT('',(45.1,7.7,48.5));
#89724=CARTESIAN_POINT('',(45.1,7.4,48.35));
#89725=CARTESIAN_POINT('',(45.1,7.4,48.5));
#89726=CARTESIAN_POINT('',(45.1,5.2,48.35));
#89727=CARTESIAN_POINT('Origin',(44.9,7.4,48.5));
#89728=CARTESIAN_POINT('',(44.9,7.4,48.5));
#89729=CARTESIAN_POINT('',(22.45,7.4,48.5));
#89730=CARTESIAN_POINT('',(44.9,7.4,48.35));
#89731=CARTESIAN_POINT('',(44.9,7.4,48.5));
#89732=CARTESIAN_POINT('',(45.1,7.4,48.35));
#89733=CARTESIAN_POINT('Origin',(44.9,5.2,48.5));
#89734=CARTESIAN_POINT('',(44.9,6.6,48.5));
#89735=CARTESIAN_POINT('',(44.9,7.4,48.35));
#89736=CARTESIAN_POINT('Origin',(45.,6.3,48.35));
#89737=CARTESIAN_POINT('Origin',(47.1,6.,48.5));
#89738=CARTESIAN_POINT('',(47.1,6.,48.5));
#89739=CARTESIAN_POINT('',(46.9,6.,48.5));
#89740=CARTESIAN_POINT('',(23.55,6.,48.5));
#89741=CARTESIAN_POINT('',(47.1,6.,48.35));
#89742=CARTESIAN_POINT('',(47.1,6.,48.5));
#89743=CARTESIAN_POINT('',(46.9,6.,48.35));
#89744=CARTESIAN_POINT('',(46.9,6.,48.35));
#89745=CARTESIAN_POINT('',(46.9,6.,48.5));
#89746=CARTESIAN_POINT('Origin',(47.1,7.4,48.5));
#89747=CARTESIAN_POINT('',(47.1,7.4,48.5));
#89748=CARTESIAN_POINT('',(47.1,7.7,48.5));
#89749=CARTESIAN_POINT('',(47.1,7.4,48.35));
#89750=CARTESIAN_POINT('',(47.1,7.4,48.5));
#89751=CARTESIAN_POINT('',(47.1,6.,48.35));
#89752=CARTESIAN_POINT('Origin',(46.9,7.4,48.5));
#89753=CARTESIAN_POINT('',(46.9,7.4,48.5));
#89754=CARTESIAN_POINT('',(23.45,7.4,48.5));
#89755=CARTESIAN_POINT('',(46.9,7.4,48.35));
#89756=CARTESIAN_POINT('',(46.9,7.4,48.5));
#89757=CARTESIAN_POINT('',(47.1,7.4,48.35));
#89758=CARTESIAN_POINT('Origin',(46.9,6.,48.5));
#89759=CARTESIAN_POINT('',(46.9,7.,48.5));
#89760=CARTESIAN_POINT('',(46.9,7.4,48.35));
#89761=CARTESIAN_POINT('Origin',(47.,6.7,48.35));
#89762=CARTESIAN_POINT('Origin',(49.1,6.,48.5));
#89763=CARTESIAN_POINT('',(49.1,6.,48.5));
#89764=CARTESIAN_POINT('',(48.9,6.,48.5));
#89765=CARTESIAN_POINT('',(24.55,6.,48.5));
#89766=CARTESIAN_POINT('',(49.1,6.,48.35));
#89767=CARTESIAN_POINT('',(49.1,6.,48.5));
#89768=CARTESIAN_POINT('',(48.9,6.,48.35));
#89769=CARTESIAN_POINT('',(48.9,6.,48.35));
#89770=CARTESIAN_POINT('',(48.9,6.,48.5));
#89771=CARTESIAN_POINT('Origin',(49.1,7.4,48.5));
#89772=CARTESIAN_POINT('',(49.1,7.4,48.5));
#89773=CARTESIAN_POINT('',(49.1,7.7,48.5));
#89774=CARTESIAN_POINT('',(49.1,7.4,48.35));
#89775=CARTESIAN_POINT('',(49.1,7.4,48.5));
#89776=CARTESIAN_POINT('',(49.1,6.,48.35));
#89777=CARTESIAN_POINT('Origin',(48.9,7.4,48.5));
#89778=CARTESIAN_POINT('',(48.9,7.4,48.5));
#89779=CARTESIAN_POINT('',(24.45,7.4,48.5));
#89780=CARTESIAN_POINT('',(48.9,7.4,48.35));
#89781=CARTESIAN_POINT('',(48.9,7.4,48.5));
#89782=CARTESIAN_POINT('',(49.1,7.4,48.35));
#89783=CARTESIAN_POINT('Origin',(48.9,6.,48.5));
#89784=CARTESIAN_POINT('',(48.9,7.,48.5));
#89785=CARTESIAN_POINT('',(48.9,7.4,48.35));
#89786=CARTESIAN_POINT('Origin',(49.,6.7,48.35));
#89787=CARTESIAN_POINT('Origin',(51.1,6.,48.5));
#89788=CARTESIAN_POINT('',(51.1,6.,48.5));
#89789=CARTESIAN_POINT('',(50.9,6.,48.5));
#89790=CARTESIAN_POINT('',(25.55,6.,48.5));
#89791=CARTESIAN_POINT('',(51.1,6.,48.35));
#89792=CARTESIAN_POINT('',(51.1,6.,48.5));
#89793=CARTESIAN_POINT('',(50.9,6.,48.35));
#89794=CARTESIAN_POINT('',(50.9,6.,48.35));
#89795=CARTESIAN_POINT('',(50.9,6.,48.5));
#89796=CARTESIAN_POINT('Origin',(51.1,7.4,48.5));
#89797=CARTESIAN_POINT('',(51.1,7.4,48.5));
#89798=CARTESIAN_POINT('',(51.1,7.7,48.5));
#89799=CARTESIAN_POINT('',(51.1,7.4,48.35));
#89800=CARTESIAN_POINT('',(51.1,7.4,48.5));
#89801=CARTESIAN_POINT('',(51.1,6.,48.35));
#89802=CARTESIAN_POINT('Origin',(50.9,7.4,48.5));
#89803=CARTESIAN_POINT('',(50.9,7.4,48.5));
#89804=CARTESIAN_POINT('',(25.45,7.4,48.5));
#89805=CARTESIAN_POINT('',(50.9,7.4,48.35));
#89806=CARTESIAN_POINT('',(50.9,7.4,48.5));
#89807=CARTESIAN_POINT('',(51.1,7.4,48.35));
#89808=CARTESIAN_POINT('Origin',(50.9,6.,48.5));
#89809=CARTESIAN_POINT('',(50.9,7.,48.5));
#89810=CARTESIAN_POINT('',(50.9,7.4,48.35));
#89811=CARTESIAN_POINT('Origin',(51.,6.7,48.35));
#89812=CARTESIAN_POINT('Origin',(53.1,6.,48.5));
#89813=CARTESIAN_POINT('',(53.1,6.,48.5));
#89814=CARTESIAN_POINT('',(52.9,6.,48.5));
#89815=CARTESIAN_POINT('',(26.55,6.,48.5));
#89816=CARTESIAN_POINT('',(53.1,6.,48.35));
#89817=CARTESIAN_POINT('',(53.1,6.,48.5));
#89818=CARTESIAN_POINT('',(52.9,6.,48.35));
#89819=CARTESIAN_POINT('',(52.9,6.,48.35));
#89820=CARTESIAN_POINT('',(52.9,6.,48.5));
#89821=CARTESIAN_POINT('Origin',(53.1,7.4,48.5));
#89822=CARTESIAN_POINT('',(53.1,7.4,48.5));
#89823=CARTESIAN_POINT('',(53.1,7.7,48.5));
#89824=CARTESIAN_POINT('',(53.1,7.4,48.35));
#89825=CARTESIAN_POINT('',(53.1,7.4,48.5));
#89826=CARTESIAN_POINT('',(53.1,6.,48.35));
#89827=CARTESIAN_POINT('Origin',(52.9,7.4,48.5));
#89828=CARTESIAN_POINT('',(52.9,7.4,48.5));
#89829=CARTESIAN_POINT('',(26.45,7.4,48.5));
#89830=CARTESIAN_POINT('',(52.9,7.4,48.35));
#89831=CARTESIAN_POINT('',(52.9,7.4,48.5));
#89832=CARTESIAN_POINT('',(53.1,7.4,48.35));
#89833=CARTESIAN_POINT('Origin',(52.9,6.,48.5));
#89834=CARTESIAN_POINT('',(52.9,7.,48.5));
#89835=CARTESIAN_POINT('',(52.9,7.4,48.35));
#89836=CARTESIAN_POINT('Origin',(53.,6.7,48.35));
#89837=CARTESIAN_POINT('Origin',(55.1,5.2,48.5));
#89838=CARTESIAN_POINT('',(55.1,5.2,48.5));
#89839=CARTESIAN_POINT('',(54.9,5.2,48.5));
#89840=CARTESIAN_POINT('',(27.55,5.2,48.5));
#89841=CARTESIAN_POINT('',(55.1,5.2,48.35));
#89842=CARTESIAN_POINT('',(55.1,5.2,48.5));
#89843=CARTESIAN_POINT('',(54.9,5.2,48.35));
#89844=CARTESIAN_POINT('',(54.9,5.2,48.35));
#89845=CARTESIAN_POINT('',(54.9,5.2,48.5));
#89846=CARTESIAN_POINT('Origin',(55.1,7.4,48.5));
#89847=CARTESIAN_POINT('',(55.1,7.4,48.5));
#89848=CARTESIAN_POINT('',(55.1,7.7,48.5));
#89849=CARTESIAN_POINT('',(55.1,7.4,48.35));
#89850=CARTESIAN_POINT('',(55.1,7.4,48.5));
#89851=CARTESIAN_POINT('',(55.1,5.2,48.35));
#89852=CARTESIAN_POINT('Origin',(54.9,7.4,48.5));
#89853=CARTESIAN_POINT('',(54.9,7.4,48.5));
#89854=CARTESIAN_POINT('',(27.45,7.4,48.5));
#89855=CARTESIAN_POINT('',(54.9,7.4,48.35));
#89856=CARTESIAN_POINT('',(54.9,7.4,48.5));
#89857=CARTESIAN_POINT('',(55.1,7.4,48.35));
#89858=CARTESIAN_POINT('Origin',(54.9,5.2,48.5));
#89859=CARTESIAN_POINT('',(54.9,6.6,48.5));
#89860=CARTESIAN_POINT('',(54.9,7.4,48.35));
#89861=CARTESIAN_POINT('Origin',(55.,6.3,48.35));
#89862=CARTESIAN_POINT('Origin',(57.1,6.,48.5));
#89863=CARTESIAN_POINT('',(57.1,6.,48.5));
#89864=CARTESIAN_POINT('',(56.9,6.,48.5));
#89865=CARTESIAN_POINT('',(28.55,6.,48.5));
#89866=CARTESIAN_POINT('',(57.1,6.,48.35));
#89867=CARTESIAN_POINT('',(57.1,6.,48.5));
#89868=CARTESIAN_POINT('',(56.9,6.,48.35));
#89869=CARTESIAN_POINT('',(56.9,6.,48.35));
#89870=CARTESIAN_POINT('',(56.9,6.,48.5));
#89871=CARTESIAN_POINT('Origin',(57.1,7.4,48.5));
#89872=CARTESIAN_POINT('',(57.1,7.4,48.5));
#89873=CARTESIAN_POINT('',(57.1,7.7,48.5));
#89874=CARTESIAN_POINT('',(57.1,7.4,48.35));
#89875=CARTESIAN_POINT('',(57.1,7.4,48.5));
#89876=CARTESIAN_POINT('',(57.1,6.,48.35));
#89877=CARTESIAN_POINT('Origin',(56.9,7.4,48.5));
#89878=CARTESIAN_POINT('',(56.9,7.4,48.5));
#89879=CARTESIAN_POINT('',(28.45,7.4,48.5));
#89880=CARTESIAN_POINT('',(56.9,7.4,48.35));
#89881=CARTESIAN_POINT('',(56.9,7.4,48.5));
#89882=CARTESIAN_POINT('',(57.1,7.4,48.35));
#89883=CARTESIAN_POINT('Origin',(56.9,6.,48.5));
#89884=CARTESIAN_POINT('',(56.9,7.,48.5));
#89885=CARTESIAN_POINT('',(56.9,7.4,48.35));
#89886=CARTESIAN_POINT('Origin',(57.,6.7,48.35));
#89887=CARTESIAN_POINT('Origin',(59.1,6.,48.5));
#89888=CARTESIAN_POINT('',(59.1,6.,48.5));
#89889=CARTESIAN_POINT('',(58.9,6.,48.5));
#89890=CARTESIAN_POINT('',(29.55,6.,48.5));
#89891=CARTESIAN_POINT('',(59.1,6.,48.35));
#89892=CARTESIAN_POINT('',(59.1,6.,48.5));
#89893=CARTESIAN_POINT('',(58.9,6.,48.35));
#89894=CARTESIAN_POINT('',(58.9,6.,48.35));
#89895=CARTESIAN_POINT('',(58.9,6.,48.5));
#89896=CARTESIAN_POINT('Origin',(59.1,7.4,48.5));
#89897=CARTESIAN_POINT('',(59.1,7.4,48.5));
#89898=CARTESIAN_POINT('',(59.1,7.7,48.5));
#89899=CARTESIAN_POINT('',(59.1,7.4,48.35));
#89900=CARTESIAN_POINT('',(59.1,7.4,48.5));
#89901=CARTESIAN_POINT('',(59.1,6.,48.35));
#89902=CARTESIAN_POINT('Origin',(58.9,7.4,48.5));
#89903=CARTESIAN_POINT('',(58.9,7.4,48.5));
#89904=CARTESIAN_POINT('',(29.45,7.4,48.5));
#89905=CARTESIAN_POINT('',(58.9,7.4,48.35));
#89906=CARTESIAN_POINT('',(58.9,7.4,48.5));
#89907=CARTESIAN_POINT('',(59.1,7.4,48.35));
#89908=CARTESIAN_POINT('Origin',(58.9,6.,48.5));
#89909=CARTESIAN_POINT('',(58.9,7.,48.5));
#89910=CARTESIAN_POINT('',(58.9,7.4,48.35));
#89911=CARTESIAN_POINT('Origin',(59.,6.7,48.35));
#89912=CARTESIAN_POINT('Origin',(61.1,6.,48.5));
#89913=CARTESIAN_POINT('',(61.1,6.,48.5));
#89914=CARTESIAN_POINT('',(60.9,6.,48.5));
#89915=CARTESIAN_POINT('',(30.55,6.,48.5));
#89916=CARTESIAN_POINT('',(61.1,6.,48.35));
#89917=CARTESIAN_POINT('',(61.1,6.,48.5));
#89918=CARTESIAN_POINT('',(60.9,6.,48.35));
#89919=CARTESIAN_POINT('',(60.9,6.,48.35));
#89920=CARTESIAN_POINT('',(60.9,6.,48.5));
#89921=CARTESIAN_POINT('Origin',(61.1,7.4,48.5));
#89922=CARTESIAN_POINT('',(61.1,7.4,48.5));
#89923=CARTESIAN_POINT('',(61.1,7.7,48.5));
#89924=CARTESIAN_POINT('',(61.1,7.4,48.35));
#89925=CARTESIAN_POINT('',(61.1,7.4,48.5));
#89926=CARTESIAN_POINT('',(61.1,6.,48.35));
#89927=CARTESIAN_POINT('Origin',(60.9,7.4,48.5));
#89928=CARTESIAN_POINT('',(60.9,7.4,48.5));
#89929=CARTESIAN_POINT('',(30.45,7.4,48.5));
#89930=CARTESIAN_POINT('',(60.9,7.4,48.35));
#89931=CARTESIAN_POINT('',(60.9,7.4,48.5));
#89932=CARTESIAN_POINT('',(61.1,7.4,48.35));
#89933=CARTESIAN_POINT('Origin',(60.9,6.,48.5));
#89934=CARTESIAN_POINT('',(60.9,7.,48.5));
#89935=CARTESIAN_POINT('',(60.9,7.4,48.35));
#89936=CARTESIAN_POINT('Origin',(61.,6.7,48.35));
#89937=CARTESIAN_POINT('Origin',(63.1,6.,48.5));
#89938=CARTESIAN_POINT('',(63.1,6.,48.5));
#89939=CARTESIAN_POINT('',(62.9,6.,48.5));
#89940=CARTESIAN_POINT('',(31.55,6.,48.5));
#89941=CARTESIAN_POINT('',(63.1,6.,48.35));
#89942=CARTESIAN_POINT('',(63.1,6.,48.5));
#89943=CARTESIAN_POINT('',(62.9,6.,48.35));
#89944=CARTESIAN_POINT('',(62.9,6.,48.35));
#89945=CARTESIAN_POINT('',(62.9,6.,48.5));
#89946=CARTESIAN_POINT('Origin',(63.1,7.4,48.5));
#89947=CARTESIAN_POINT('',(63.1,7.4,48.5));
#89948=CARTESIAN_POINT('',(63.1,7.7,48.5));
#89949=CARTESIAN_POINT('',(63.1,7.4,48.35));
#89950=CARTESIAN_POINT('',(63.1,7.4,48.5));
#89951=CARTESIAN_POINT('',(63.1,6.,48.35));
#89952=CARTESIAN_POINT('Origin',(62.9,7.4,48.5));
#89953=CARTESIAN_POINT('',(62.9,7.4,48.5));
#89954=CARTESIAN_POINT('',(31.45,7.4,48.5));
#89955=CARTESIAN_POINT('',(62.9,7.4,48.35));
#89956=CARTESIAN_POINT('',(62.9,7.4,48.5));
#89957=CARTESIAN_POINT('',(63.1,7.4,48.35));
#89958=CARTESIAN_POINT('Origin',(62.9,6.,48.5));
#89959=CARTESIAN_POINT('',(62.9,7.,48.5));
#89960=CARTESIAN_POINT('',(62.9,7.4,48.35));
#89961=CARTESIAN_POINT('Origin',(63.,6.7,48.35));
#89962=CARTESIAN_POINT('Origin',(65.1,5.2,48.5));
#89963=CARTESIAN_POINT('',(65.1,5.2,48.5));
#89964=CARTESIAN_POINT('',(64.9,5.2,48.5));
#89965=CARTESIAN_POINT('',(32.55,5.2,48.5));
#89966=CARTESIAN_POINT('',(65.1,5.2,48.35));
#89967=CARTESIAN_POINT('',(65.1,5.2,48.5));
#89968=CARTESIAN_POINT('',(64.9,5.2,48.35));
#89969=CARTESIAN_POINT('',(64.9,5.2,48.35));
#89970=CARTESIAN_POINT('',(64.9,5.2,48.5));
#89971=CARTESIAN_POINT('Origin',(65.1,7.4,48.5));
#89972=CARTESIAN_POINT('',(65.1,7.4,48.5));
#89973=CARTESIAN_POINT('',(65.1,7.7,48.5));
#89974=CARTESIAN_POINT('',(65.1,7.4,48.35));
#89975=CARTESIAN_POINT('',(65.1,7.4,48.5));
#89976=CARTESIAN_POINT('',(65.1,5.2,48.35));
#89977=CARTESIAN_POINT('Origin',(64.9,7.4,48.5));
#89978=CARTESIAN_POINT('',(64.9,7.4,48.5));
#89979=CARTESIAN_POINT('',(32.45,7.4,48.5));
#89980=CARTESIAN_POINT('',(64.9,7.4,48.35));
#89981=CARTESIAN_POINT('',(64.9,7.4,48.5));
#89982=CARTESIAN_POINT('',(65.1,7.4,48.35));
#89983=CARTESIAN_POINT('Origin',(64.9,5.2,48.5));
#89984=CARTESIAN_POINT('',(64.9,6.6,48.5));
#89985=CARTESIAN_POINT('',(64.9,7.4,48.35));
#89986=CARTESIAN_POINT('Origin',(65.,6.3,48.35));
#89987=CARTESIAN_POINT('Origin',(67.1,6.,48.5));
#89988=CARTESIAN_POINT('',(67.1,6.,48.5));
#89989=CARTESIAN_POINT('',(66.9,6.,48.5));
#89990=CARTESIAN_POINT('',(33.55,6.,48.5));
#89991=CARTESIAN_POINT('',(67.1,6.,48.35));
#89992=CARTESIAN_POINT('',(67.1,6.,48.5));
#89993=CARTESIAN_POINT('',(66.9,6.,48.35));
#89994=CARTESIAN_POINT('',(66.9,6.,48.35));
#89995=CARTESIAN_POINT('',(66.9,6.,48.5));
#89996=CARTESIAN_POINT('Origin',(67.1,7.4,48.5));
#89997=CARTESIAN_POINT('',(67.1,7.4,48.5));
#89998=CARTESIAN_POINT('',(67.1,7.7,48.5));
#89999=CARTESIAN_POINT('',(67.1,7.4,48.35));
#90000=CARTESIAN_POINT('',(67.1,7.4,48.5));
#90001=CARTESIAN_POINT('',(67.1,6.,48.35));
#90002=CARTESIAN_POINT('Origin',(66.9,7.4,48.5));
#90003=CARTESIAN_POINT('',(66.9,7.4,48.5));
#90004=CARTESIAN_POINT('',(33.45,7.4,48.5));
#90005=CARTESIAN_POINT('',(66.9,7.4,48.35));
#90006=CARTESIAN_POINT('',(66.9,7.4,48.5));
#90007=CARTESIAN_POINT('',(67.1,7.4,48.35));
#90008=CARTESIAN_POINT('Origin',(66.9,6.,48.5));
#90009=CARTESIAN_POINT('',(66.9,7.,48.5));
#90010=CARTESIAN_POINT('',(66.9,7.4,48.35));
#90011=CARTESIAN_POINT('Origin',(67.,6.7,48.35));
#90012=CARTESIAN_POINT('Origin',(69.1,6.,48.5));
#90013=CARTESIAN_POINT('',(69.1,6.,48.5));
#90014=CARTESIAN_POINT('',(68.9,6.,48.5));
#90015=CARTESIAN_POINT('',(34.55,6.,48.5));
#90016=CARTESIAN_POINT('',(69.1,6.,48.35));
#90017=CARTESIAN_POINT('',(69.1,6.,48.5));
#90018=CARTESIAN_POINT('',(68.9,6.,48.35));
#90019=CARTESIAN_POINT('',(68.9,6.,48.35));
#90020=CARTESIAN_POINT('',(68.9,6.,48.5));
#90021=CARTESIAN_POINT('Origin',(69.1,7.4,48.5));
#90022=CARTESIAN_POINT('',(69.1,7.4,48.5));
#90023=CARTESIAN_POINT('',(69.1,7.7,48.5));
#90024=CARTESIAN_POINT('',(69.1,7.4,48.35));
#90025=CARTESIAN_POINT('',(69.1,7.4,48.5));
#90026=CARTESIAN_POINT('',(69.1,6.,48.35));
#90027=CARTESIAN_POINT('Origin',(68.9,7.4,48.5));
#90028=CARTESIAN_POINT('',(68.9,7.4,48.5));
#90029=CARTESIAN_POINT('',(34.45,7.4,48.5));
#90030=CARTESIAN_POINT('',(68.9,7.4,48.35));
#90031=CARTESIAN_POINT('',(68.9,7.4,48.5));
#90032=CARTESIAN_POINT('',(69.1,7.4,48.35));
#90033=CARTESIAN_POINT('Origin',(68.9,6.,48.5));
#90034=CARTESIAN_POINT('',(68.9,7.,48.5));
#90035=CARTESIAN_POINT('',(68.9,7.4,48.35));
#90036=CARTESIAN_POINT('Origin',(69.,6.7,48.35));
#90037=CARTESIAN_POINT('Origin',(71.1,6.,48.5));
#90038=CARTESIAN_POINT('',(71.1,6.,48.5));
#90039=CARTESIAN_POINT('',(70.9,6.,48.5));
#90040=CARTESIAN_POINT('',(35.55,6.,48.5));
#90041=CARTESIAN_POINT('',(71.1,6.,48.35));
#90042=CARTESIAN_POINT('',(71.1,6.,48.5));
#90043=CARTESIAN_POINT('',(70.9,6.,48.35));
#90044=CARTESIAN_POINT('',(70.9,6.,48.35));
#90045=CARTESIAN_POINT('',(70.9,6.,48.5));
#90046=CARTESIAN_POINT('Origin',(71.1,7.4,48.5));
#90047=CARTESIAN_POINT('',(71.1,7.4,48.5));
#90048=CARTESIAN_POINT('',(71.1,7.7,48.5));
#90049=CARTESIAN_POINT('',(71.1,7.4,48.35));
#90050=CARTESIAN_POINT('',(71.1,7.4,48.5));
#90051=CARTESIAN_POINT('',(71.1,6.,48.35));
#90052=CARTESIAN_POINT('Origin',(70.9,7.4,48.5));
#90053=CARTESIAN_POINT('',(70.9,7.4,48.5));
#90054=CARTESIAN_POINT('',(35.45,7.4,48.5));
#90055=CARTESIAN_POINT('',(70.9,7.4,48.35));
#90056=CARTESIAN_POINT('',(70.9,7.4,48.5));
#90057=CARTESIAN_POINT('',(71.1,7.4,48.35));
#90058=CARTESIAN_POINT('Origin',(70.9,6.,48.5));
#90059=CARTESIAN_POINT('',(70.9,7.,48.5));
#90060=CARTESIAN_POINT('',(70.9,7.4,48.35));
#90061=CARTESIAN_POINT('Origin',(71.,6.7,48.35));
#90062=CARTESIAN_POINT('Origin',(73.1,6.,48.5));
#90063=CARTESIAN_POINT('',(73.1,6.,48.5));
#90064=CARTESIAN_POINT('',(72.9,6.,48.5));
#90065=CARTESIAN_POINT('',(36.55,6.,48.5));
#90066=CARTESIAN_POINT('',(73.1,6.,48.35));
#90067=CARTESIAN_POINT('',(73.1,6.,48.5));
#90068=CARTESIAN_POINT('',(72.9,6.,48.35));
#90069=CARTESIAN_POINT('',(72.9,6.,48.35));
#90070=CARTESIAN_POINT('',(72.9,6.,48.5));
#90071=CARTESIAN_POINT('Origin',(73.1,7.4,48.5));
#90072=CARTESIAN_POINT('',(73.1,7.4,48.5));
#90073=CARTESIAN_POINT('',(73.1,7.7,48.5));
#90074=CARTESIAN_POINT('',(73.1,7.4,48.35));
#90075=CARTESIAN_POINT('',(73.1,7.4,48.5));
#90076=CARTESIAN_POINT('',(73.1,6.,48.35));
#90077=CARTESIAN_POINT('Origin',(72.9,7.4,48.5));
#90078=CARTESIAN_POINT('',(72.9,7.4,48.5));
#90079=CARTESIAN_POINT('',(36.45,7.4,48.5));
#90080=CARTESIAN_POINT('',(72.9,7.4,48.35));
#90081=CARTESIAN_POINT('',(72.9,7.4,48.5));
#90082=CARTESIAN_POINT('',(73.1,7.4,48.35));
#90083=CARTESIAN_POINT('Origin',(72.9,6.,48.5));
#90084=CARTESIAN_POINT('',(72.9,7.,48.5));
#90085=CARTESIAN_POINT('',(72.9,7.4,48.35));
#90086=CARTESIAN_POINT('Origin',(73.,6.7,48.35));
#90087=CARTESIAN_POINT('Origin',(75.1,5.2,48.5));
#90088=CARTESIAN_POINT('',(75.1,5.2,48.5));
#90089=CARTESIAN_POINT('',(74.9,5.2,48.5));
#90090=CARTESIAN_POINT('',(37.55,5.2,48.5));
#90091=CARTESIAN_POINT('',(75.1,5.2,48.35));
#90092=CARTESIAN_POINT('',(75.1,5.2,48.5));
#90093=CARTESIAN_POINT('',(74.9,5.2,48.35));
#90094=CARTESIAN_POINT('',(74.9,5.2,48.35));
#90095=CARTESIAN_POINT('',(74.9,5.2,48.5));
#90096=CARTESIAN_POINT('Origin',(75.1,7.4,48.5));
#90097=CARTESIAN_POINT('',(75.1,7.4,48.5));
#90098=CARTESIAN_POINT('',(75.1,7.7,48.5));
#90099=CARTESIAN_POINT('',(75.1,7.4,48.35));
#90100=CARTESIAN_POINT('',(75.1,7.4,48.5));
#90101=CARTESIAN_POINT('',(75.1,5.2,48.35));
#90102=CARTESIAN_POINT('Origin',(74.9,7.4,48.5));
#90103=CARTESIAN_POINT('',(74.9,7.4,48.5));
#90104=CARTESIAN_POINT('',(37.45,7.4,48.5));
#90105=CARTESIAN_POINT('',(74.9,7.4,48.35));
#90106=CARTESIAN_POINT('',(74.9,7.4,48.5));
#90107=CARTESIAN_POINT('',(75.1,7.4,48.35));
#90108=CARTESIAN_POINT('Origin',(74.9,5.2,48.5));
#90109=CARTESIAN_POINT('',(74.9,6.6,48.5));
#90110=CARTESIAN_POINT('',(74.9,7.4,48.35));
#90111=CARTESIAN_POINT('Origin',(75.,6.3,48.35));
#90112=CARTESIAN_POINT('Origin',(77.1,6.,48.5));
#90113=CARTESIAN_POINT('',(77.1,6.,48.5));
#90114=CARTESIAN_POINT('',(76.9,6.,48.5));
#90115=CARTESIAN_POINT('',(38.55,6.,48.5));
#90116=CARTESIAN_POINT('',(77.1,6.,48.35));
#90117=CARTESIAN_POINT('',(77.1,6.,48.5));
#90118=CARTESIAN_POINT('',(76.9,6.,48.35));
#90119=CARTESIAN_POINT('',(76.9,6.,48.35));
#90120=CARTESIAN_POINT('',(76.9,6.,48.5));
#90121=CARTESIAN_POINT('Origin',(77.1,7.4,48.5));
#90122=CARTESIAN_POINT('',(77.1,7.4,48.5));
#90123=CARTESIAN_POINT('',(77.1,7.7,48.5));
#90124=CARTESIAN_POINT('',(77.1,7.4,48.35));
#90125=CARTESIAN_POINT('',(77.1,7.4,48.5));
#90126=CARTESIAN_POINT('',(77.1,6.,48.35));
#90127=CARTESIAN_POINT('Origin',(76.9,7.4,48.5));
#90128=CARTESIAN_POINT('',(76.9,7.4,48.5));
#90129=CARTESIAN_POINT('',(38.45,7.4,48.5));
#90130=CARTESIAN_POINT('',(76.9,7.4,48.35));
#90131=CARTESIAN_POINT('',(76.9,7.4,48.5));
#90132=CARTESIAN_POINT('',(77.1,7.4,48.35));
#90133=CARTESIAN_POINT('Origin',(76.9,6.,48.5));
#90134=CARTESIAN_POINT('',(76.9,7.,48.5));
#90135=CARTESIAN_POINT('',(76.9,7.4,48.35));
#90136=CARTESIAN_POINT('Origin',(77.,6.7,48.35));
#90137=CARTESIAN_POINT('Origin',(79.1,6.,48.5));
#90138=CARTESIAN_POINT('',(79.1,6.,48.5));
#90139=CARTESIAN_POINT('',(78.9,6.,48.5));
#90140=CARTESIAN_POINT('',(39.55,6.,48.5));
#90141=CARTESIAN_POINT('',(79.1,6.,48.35));
#90142=CARTESIAN_POINT('',(79.1,6.,48.5));
#90143=CARTESIAN_POINT('',(78.9,6.,48.35));
#90144=CARTESIAN_POINT('',(78.9,6.,48.35));
#90145=CARTESIAN_POINT('',(78.9,6.,48.5));
#90146=CARTESIAN_POINT('Origin',(79.1,7.4,48.5));
#90147=CARTESIAN_POINT('',(79.1,7.4,48.5));
#90148=CARTESIAN_POINT('',(79.1,7.7,48.5));
#90149=CARTESIAN_POINT('',(79.1,7.4,48.35));
#90150=CARTESIAN_POINT('',(79.1,7.4,48.5));
#90151=CARTESIAN_POINT('',(79.1,6.,48.35));
#90152=CARTESIAN_POINT('Origin',(78.9,7.4,48.5));
#90153=CARTESIAN_POINT('',(78.9,7.4,48.5));
#90154=CARTESIAN_POINT('',(39.45,7.4,48.5));
#90155=CARTESIAN_POINT('',(78.9,7.4,48.35));
#90156=CARTESIAN_POINT('',(78.9,7.4,48.5));
#90157=CARTESIAN_POINT('',(79.1,7.4,48.35));
#90158=CARTESIAN_POINT('Origin',(78.9,6.,48.5));
#90159=CARTESIAN_POINT('',(78.9,7.,48.5));
#90160=CARTESIAN_POINT('',(78.9,7.4,48.35));
#90161=CARTESIAN_POINT('Origin',(79.,6.7,48.35));
#90162=CARTESIAN_POINT('Origin',(81.1,6.,48.5));
#90163=CARTESIAN_POINT('',(81.1,6.,48.5));
#90164=CARTESIAN_POINT('',(80.9,6.,48.5));
#90165=CARTESIAN_POINT('',(40.55,6.,48.5));
#90166=CARTESIAN_POINT('',(81.1,6.,48.35));
#90167=CARTESIAN_POINT('',(81.1,6.,48.5));
#90168=CARTESIAN_POINT('',(80.9,6.,48.35));
#90169=CARTESIAN_POINT('',(80.9,6.,48.35));
#90170=CARTESIAN_POINT('',(80.9,6.,48.5));
#90171=CARTESIAN_POINT('Origin',(81.1,7.4,48.5));
#90172=CARTESIAN_POINT('',(81.1,7.4,48.5));
#90173=CARTESIAN_POINT('',(81.1,7.7,48.5));
#90174=CARTESIAN_POINT('',(81.1,7.4,48.35));
#90175=CARTESIAN_POINT('',(81.1,7.4,48.5));
#90176=CARTESIAN_POINT('',(81.1,6.,48.35));
#90177=CARTESIAN_POINT('Origin',(80.9,7.4,48.5));
#90178=CARTESIAN_POINT('',(80.9,7.4,48.5));
#90179=CARTESIAN_POINT('',(40.45,7.4,48.5));
#90180=CARTESIAN_POINT('',(80.9,7.4,48.35));
#90181=CARTESIAN_POINT('',(80.9,7.4,48.5));
#90182=CARTESIAN_POINT('',(81.1,7.4,48.35));
#90183=CARTESIAN_POINT('Origin',(80.9,6.,48.5));
#90184=CARTESIAN_POINT('',(80.9,7.,48.5));
#90185=CARTESIAN_POINT('',(80.9,7.4,48.35));
#90186=CARTESIAN_POINT('Origin',(81.,6.7,48.35));
#90187=CARTESIAN_POINT('Origin',(83.1,6.,48.5));
#90188=CARTESIAN_POINT('',(83.1,6.,48.5));
#90189=CARTESIAN_POINT('',(82.9,6.,48.5));
#90190=CARTESIAN_POINT('',(41.55,6.,48.5));
#90191=CARTESIAN_POINT('',(83.1,6.,48.35));
#90192=CARTESIAN_POINT('',(83.1,6.,48.5));
#90193=CARTESIAN_POINT('',(82.9,6.,48.35));
#90194=CARTESIAN_POINT('',(82.9,6.,48.35));
#90195=CARTESIAN_POINT('',(82.9,6.,48.5));
#90196=CARTESIAN_POINT('Origin',(83.1,7.4,48.5));
#90197=CARTESIAN_POINT('',(83.1,7.4,48.5));
#90198=CARTESIAN_POINT('',(83.1,7.7,48.5));
#90199=CARTESIAN_POINT('',(83.1,7.4,48.35));
#90200=CARTESIAN_POINT('',(83.1,7.4,48.5));
#90201=CARTESIAN_POINT('',(83.1,6.,48.35));
#90202=CARTESIAN_POINT('Origin',(82.9,7.4,48.5));
#90203=CARTESIAN_POINT('',(82.9,7.4,48.5));
#90204=CARTESIAN_POINT('',(41.45,7.4,48.5));
#90205=CARTESIAN_POINT('',(82.9,7.4,48.35));
#90206=CARTESIAN_POINT('',(82.9,7.4,48.5));
#90207=CARTESIAN_POINT('',(83.1,7.4,48.35));
#90208=CARTESIAN_POINT('Origin',(82.9,6.,48.5));
#90209=CARTESIAN_POINT('',(82.9,7.,48.5));
#90210=CARTESIAN_POINT('',(82.9,7.4,48.35));
#90211=CARTESIAN_POINT('Origin',(83.,6.7,48.35));
#90212=CARTESIAN_POINT('Origin',(85.1,5.2,48.5));
#90213=CARTESIAN_POINT('',(85.1,5.2,48.5));
#90214=CARTESIAN_POINT('',(84.9,5.2,48.5));
#90215=CARTESIAN_POINT('',(42.55,5.2,48.5));
#90216=CARTESIAN_POINT('',(85.1,5.2,48.35));
#90217=CARTESIAN_POINT('',(85.1,5.2,48.5));
#90218=CARTESIAN_POINT('',(84.9,5.2,48.35));
#90219=CARTESIAN_POINT('',(84.9,5.2,48.35));
#90220=CARTESIAN_POINT('',(84.9,5.2,48.5));
#90221=CARTESIAN_POINT('Origin',(85.1,7.4,48.5));
#90222=CARTESIAN_POINT('',(85.1,7.4,48.5));
#90223=CARTESIAN_POINT('',(85.1,7.7,48.5));
#90224=CARTESIAN_POINT('',(85.1,7.4,48.35));
#90225=CARTESIAN_POINT('',(85.1,7.4,48.5));
#90226=CARTESIAN_POINT('',(85.1,5.2,48.35));
#90227=CARTESIAN_POINT('Origin',(84.9,7.4,48.5));
#90228=CARTESIAN_POINT('',(84.9,7.4,48.5));
#90229=CARTESIAN_POINT('',(42.45,7.4,48.5));
#90230=CARTESIAN_POINT('',(84.9,7.4,48.35));
#90231=CARTESIAN_POINT('',(84.9,7.4,48.5));
#90232=CARTESIAN_POINT('',(85.1,7.4,48.35));
#90233=CARTESIAN_POINT('Origin',(84.9,5.2,48.5));
#90234=CARTESIAN_POINT('',(84.9,6.6,48.5));
#90235=CARTESIAN_POINT('',(84.9,7.4,48.35));
#90236=CARTESIAN_POINT('Origin',(85.,6.3,48.35));
#90237=CARTESIAN_POINT('Origin',(87.1,6.,48.5));
#90238=CARTESIAN_POINT('',(87.1,6.,48.5));
#90239=CARTESIAN_POINT('',(86.9,6.,48.5));
#90240=CARTESIAN_POINT('',(43.55,6.,48.5));
#90241=CARTESIAN_POINT('',(87.1,6.,48.35));
#90242=CARTESIAN_POINT('',(87.1,6.,48.5));
#90243=CARTESIAN_POINT('',(86.9,6.,48.35));
#90244=CARTESIAN_POINT('',(86.9,6.,48.35));
#90245=CARTESIAN_POINT('',(86.9,6.,48.5));
#90246=CARTESIAN_POINT('Origin',(87.1,7.4,48.5));
#90247=CARTESIAN_POINT('',(87.1,7.4,48.5));
#90248=CARTESIAN_POINT('',(87.1,7.7,48.5));
#90249=CARTESIAN_POINT('',(87.1,7.4,48.35));
#90250=CARTESIAN_POINT('',(87.1,7.4,48.5));
#90251=CARTESIAN_POINT('',(87.1,6.,48.35));
#90252=CARTESIAN_POINT('Origin',(86.9,7.4,48.5));
#90253=CARTESIAN_POINT('',(86.9,7.4,48.5));
#90254=CARTESIAN_POINT('',(43.45,7.4,48.5));
#90255=CARTESIAN_POINT('',(86.9,7.4,48.35));
#90256=CARTESIAN_POINT('',(86.9,7.4,48.5));
#90257=CARTESIAN_POINT('',(87.1,7.4,48.35));
#90258=CARTESIAN_POINT('Origin',(86.9,6.,48.5));
#90259=CARTESIAN_POINT('',(86.9,7.,48.5));
#90260=CARTESIAN_POINT('',(86.9,7.4,48.35));
#90261=CARTESIAN_POINT('Origin',(87.,6.7,48.35));
#90262=CARTESIAN_POINT('Origin',(89.1,6.,48.5));
#90263=CARTESIAN_POINT('',(89.1,6.,48.5));
#90264=CARTESIAN_POINT('',(88.9,6.,48.5));
#90265=CARTESIAN_POINT('',(44.55,6.,48.5));
#90266=CARTESIAN_POINT('',(89.1,6.,48.35));
#90267=CARTESIAN_POINT('',(89.1,6.,48.5));
#90268=CARTESIAN_POINT('',(88.9,6.,48.35));
#90269=CARTESIAN_POINT('',(88.9,6.,48.35));
#90270=CARTESIAN_POINT('',(88.9,6.,48.5));
#90271=CARTESIAN_POINT('Origin',(89.1,7.4,48.5));
#90272=CARTESIAN_POINT('',(89.1,7.4,48.5));
#90273=CARTESIAN_POINT('',(89.1,7.7,48.5));
#90274=CARTESIAN_POINT('',(89.1,7.4,48.35));
#90275=CARTESIAN_POINT('',(89.1,7.4,48.5));
#90276=CARTESIAN_POINT('',(89.1,6.,48.35));
#90277=CARTESIAN_POINT('Origin',(88.9,7.4,48.5));
#90278=CARTESIAN_POINT('',(88.9,7.4,48.5));
#90279=CARTESIAN_POINT('',(44.45,7.4,48.5));
#90280=CARTESIAN_POINT('',(88.9,7.4,48.35));
#90281=CARTESIAN_POINT('',(88.9,7.4,48.5));
#90282=CARTESIAN_POINT('',(89.1,7.4,48.35));
#90283=CARTESIAN_POINT('Origin',(88.9,6.,48.5));
#90284=CARTESIAN_POINT('',(88.9,7.,48.5));
#90285=CARTESIAN_POINT('',(88.9,7.4,48.35));
#90286=CARTESIAN_POINT('Origin',(89.,6.7,48.35));
#90287=CARTESIAN_POINT('Origin',(91.1,6.,48.5));
#90288=CARTESIAN_POINT('',(91.1,6.,48.5));
#90289=CARTESIAN_POINT('',(90.9,6.,48.5));
#90290=CARTESIAN_POINT('',(45.55,6.,48.5));
#90291=CARTESIAN_POINT('',(91.1,6.,48.35));
#90292=CARTESIAN_POINT('',(91.1,6.,48.5));
#90293=CARTESIAN_POINT('',(90.9,6.,48.35));
#90294=CARTESIAN_POINT('',(90.9,6.,48.35));
#90295=CARTESIAN_POINT('',(90.9,6.,48.5));
#90296=CARTESIAN_POINT('Origin',(91.1,7.4,48.5));
#90297=CARTESIAN_POINT('',(91.1,7.4,48.5));
#90298=CARTESIAN_POINT('',(91.1,7.7,48.5));
#90299=CARTESIAN_POINT('',(91.1,7.4,48.35));
#90300=CARTESIAN_POINT('',(91.1,7.4,48.5));
#90301=CARTESIAN_POINT('',(91.1,6.,48.35));
#90302=CARTESIAN_POINT('Origin',(90.9,7.4,48.5));
#90303=CARTESIAN_POINT('',(90.9,7.4,48.5));
#90304=CARTESIAN_POINT('',(45.45,7.4,48.5));
#90305=CARTESIAN_POINT('',(90.9,7.4,48.35));
#90306=CARTESIAN_POINT('',(90.9,7.4,48.5));
#90307=CARTESIAN_POINT('',(91.1,7.4,48.35));
#90308=CARTESIAN_POINT('Origin',(90.9,6.,48.5));
#90309=CARTESIAN_POINT('',(90.9,7.,48.5));
#90310=CARTESIAN_POINT('',(90.9,7.4,48.35));
#90311=CARTESIAN_POINT('Origin',(91.,6.7,48.35));
#90312=CARTESIAN_POINT('Origin',(93.1,6.,48.5));
#90313=CARTESIAN_POINT('',(93.1,6.,48.5));
#90314=CARTESIAN_POINT('',(92.9,6.,48.5));
#90315=CARTESIAN_POINT('',(46.55,6.,48.5));
#90316=CARTESIAN_POINT('',(93.1,6.,48.35));
#90317=CARTESIAN_POINT('',(93.1,6.,48.5));
#90318=CARTESIAN_POINT('',(92.9,6.,48.35));
#90319=CARTESIAN_POINT('',(92.9,6.,48.35));
#90320=CARTESIAN_POINT('',(92.9,6.,48.5));
#90321=CARTESIAN_POINT('Origin',(93.1,7.4,48.5));
#90322=CARTESIAN_POINT('',(93.1,7.4,48.5));
#90323=CARTESIAN_POINT('',(93.1,7.7,48.5));
#90324=CARTESIAN_POINT('',(93.1,7.4,48.35));
#90325=CARTESIAN_POINT('',(93.1,7.4,48.5));
#90326=CARTESIAN_POINT('',(93.1,6.,48.35));
#90327=CARTESIAN_POINT('Origin',(92.9,7.4,48.5));
#90328=CARTESIAN_POINT('',(92.9,7.4,48.5));
#90329=CARTESIAN_POINT('',(46.45,7.4,48.5));
#90330=CARTESIAN_POINT('',(92.9,7.4,48.35));
#90331=CARTESIAN_POINT('',(92.9,7.4,48.5));
#90332=CARTESIAN_POINT('',(93.1,7.4,48.35));
#90333=CARTESIAN_POINT('Origin',(92.9,6.,48.5));
#90334=CARTESIAN_POINT('',(92.9,7.,48.5));
#90335=CARTESIAN_POINT('',(92.9,7.4,48.35));
#90336=CARTESIAN_POINT('Origin',(93.,6.7,48.35));
#90337=CARTESIAN_POINT('Origin',(95.1,5.2,48.5));
#90338=CARTESIAN_POINT('',(95.1,5.2,48.5));
#90339=CARTESIAN_POINT('',(94.9,5.2,48.5));
#90340=CARTESIAN_POINT('',(47.55,5.2,48.5));
#90341=CARTESIAN_POINT('',(95.1,5.2,48.35));
#90342=CARTESIAN_POINT('',(95.1,5.2,48.5));
#90343=CARTESIAN_POINT('',(94.9,5.2,48.35));
#90344=CARTESIAN_POINT('',(94.9,5.2,48.35));
#90345=CARTESIAN_POINT('',(94.9,5.2,48.5));
#90346=CARTESIAN_POINT('Origin',(95.1,7.4,48.5));
#90347=CARTESIAN_POINT('',(95.1,7.4,48.5));
#90348=CARTESIAN_POINT('',(95.1,7.7,48.5));
#90349=CARTESIAN_POINT('',(95.1,7.4,48.35));
#90350=CARTESIAN_POINT('',(95.1,7.4,48.5));
#90351=CARTESIAN_POINT('',(95.1,5.2,48.35));
#90352=CARTESIAN_POINT('Origin',(94.9,7.4,48.5));
#90353=CARTESIAN_POINT('',(94.9,7.4,48.5));
#90354=CARTESIAN_POINT('',(47.45,7.4,48.5));
#90355=CARTESIAN_POINT('',(94.9,7.4,48.35));
#90356=CARTESIAN_POINT('',(94.9,7.4,48.5));
#90357=CARTESIAN_POINT('',(95.1,7.4,48.35));
#90358=CARTESIAN_POINT('Origin',(94.9,5.2,48.5));
#90359=CARTESIAN_POINT('',(94.9,6.6,48.5));
#90360=CARTESIAN_POINT('',(94.9,7.4,48.35));
#90361=CARTESIAN_POINT('Origin',(95.,6.3,48.35));
#90362=CARTESIAN_POINT('Origin',(97.1,6.,48.5));
#90363=CARTESIAN_POINT('',(97.1,6.,48.5));
#90364=CARTESIAN_POINT('',(96.9,6.,48.5));
#90365=CARTESIAN_POINT('',(48.55,6.,48.5));
#90366=CARTESIAN_POINT('',(97.1,6.,48.35));
#90367=CARTESIAN_POINT('',(97.1,6.,48.5));
#90368=CARTESIAN_POINT('',(96.9,6.,48.35));
#90369=CARTESIAN_POINT('',(96.9,6.,48.35));
#90370=CARTESIAN_POINT('',(96.9,6.,48.5));
#90371=CARTESIAN_POINT('Origin',(97.1,7.4,48.5));
#90372=CARTESIAN_POINT('',(97.1,7.4,48.5));
#90373=CARTESIAN_POINT('',(97.1,7.7,48.5));
#90374=CARTESIAN_POINT('',(97.1,7.4,48.35));
#90375=CARTESIAN_POINT('',(97.1,7.4,48.5));
#90376=CARTESIAN_POINT('',(97.1,6.,48.35));
#90377=CARTESIAN_POINT('Origin',(96.9,7.4,48.5));
#90378=CARTESIAN_POINT('',(96.9,7.4,48.5));
#90379=CARTESIAN_POINT('',(48.45,7.4,48.5));
#90380=CARTESIAN_POINT('',(96.9,7.4,48.35));
#90381=CARTESIAN_POINT('',(96.9,7.4,48.5));
#90382=CARTESIAN_POINT('',(97.1,7.4,48.35));
#90383=CARTESIAN_POINT('Origin',(96.9,6.,48.5));
#90384=CARTESIAN_POINT('',(96.9,7.,48.5));
#90385=CARTESIAN_POINT('',(96.9,7.4,48.35));
#90386=CARTESIAN_POINT('Origin',(97.,6.7,48.35));
#90387=CARTESIAN_POINT('Origin',(99.1,6.,48.5));
#90388=CARTESIAN_POINT('',(99.1,6.,48.5));
#90389=CARTESIAN_POINT('',(98.9,6.,48.5));
#90390=CARTESIAN_POINT('',(49.55,6.,48.5));
#90391=CARTESIAN_POINT('',(99.1,6.,48.35));
#90392=CARTESIAN_POINT('',(99.1,6.,48.5));
#90393=CARTESIAN_POINT('',(98.9,6.,48.35));
#90394=CARTESIAN_POINT('',(98.9,6.,48.35));
#90395=CARTESIAN_POINT('',(98.9,6.,48.5));
#90396=CARTESIAN_POINT('Origin',(99.1,7.4,48.5));
#90397=CARTESIAN_POINT('',(99.1,7.4,48.5));
#90398=CARTESIAN_POINT('',(99.1,7.7,48.5));
#90399=CARTESIAN_POINT('',(99.1,7.4,48.35));
#90400=CARTESIAN_POINT('',(99.1,7.4,48.5));
#90401=CARTESIAN_POINT('',(99.1,6.,48.35));
#90402=CARTESIAN_POINT('Origin',(98.9,7.4,48.5));
#90403=CARTESIAN_POINT('',(98.9,7.4,48.5));
#90404=CARTESIAN_POINT('',(49.45,7.4,48.5));
#90405=CARTESIAN_POINT('',(98.9,7.4,48.35));
#90406=CARTESIAN_POINT('',(98.9,7.4,48.5));
#90407=CARTESIAN_POINT('',(99.1,7.4,48.35));
#90408=CARTESIAN_POINT('Origin',(98.9,6.,48.5));
#90409=CARTESIAN_POINT('',(98.9,7.,48.5));
#90410=CARTESIAN_POINT('',(98.9,7.4,48.35));
#90411=CARTESIAN_POINT('Origin',(99.,6.7,48.35));
#90412=CARTESIAN_POINT('Origin',(101.1,6.,48.5));
#90413=CARTESIAN_POINT('',(101.1,6.,48.5));
#90414=CARTESIAN_POINT('',(100.9,6.,48.5));
#90415=CARTESIAN_POINT('',(50.55,6.,48.5));
#90416=CARTESIAN_POINT('',(101.1,6.,48.35));
#90417=CARTESIAN_POINT('',(101.1,6.,48.5));
#90418=CARTESIAN_POINT('',(100.9,6.,48.35));
#90419=CARTESIAN_POINT('',(100.9,6.,48.35));
#90420=CARTESIAN_POINT('',(100.9,6.,48.5));
#90421=CARTESIAN_POINT('Origin',(101.1,7.4,48.5));
#90422=CARTESIAN_POINT('',(101.1,7.4,48.5));
#90423=CARTESIAN_POINT('',(101.1,7.7,48.5));
#90424=CARTESIAN_POINT('',(101.1,7.4,48.35));
#90425=CARTESIAN_POINT('',(101.1,7.4,48.5));
#90426=CARTESIAN_POINT('',(101.1,6.,48.35));
#90427=CARTESIAN_POINT('Origin',(100.9,7.4,48.5));
#90428=CARTESIAN_POINT('',(100.9,7.4,48.5));
#90429=CARTESIAN_POINT('',(50.45,7.4,48.5));
#90430=CARTESIAN_POINT('',(100.9,7.4,48.35));
#90431=CARTESIAN_POINT('',(100.9,7.4,48.5));
#90432=CARTESIAN_POINT('',(101.1,7.4,48.35));
#90433=CARTESIAN_POINT('Origin',(100.9,6.,48.5));
#90434=CARTESIAN_POINT('',(100.9,7.,48.5));
#90435=CARTESIAN_POINT('',(100.9,7.4,48.35));
#90436=CARTESIAN_POINT('Origin',(101.,6.7,48.35));
#90437=CARTESIAN_POINT('Origin',(103.1,6.,48.5));
#90438=CARTESIAN_POINT('',(103.1,6.,48.5));
#90439=CARTESIAN_POINT('',(102.9,6.,48.5));
#90440=CARTESIAN_POINT('',(51.55,6.,48.5));
#90441=CARTESIAN_POINT('',(103.1,6.,48.35));
#90442=CARTESIAN_POINT('',(103.1,6.,48.5));
#90443=CARTESIAN_POINT('',(102.9,6.,48.35));
#90444=CARTESIAN_POINT('',(102.9,6.,48.35));
#90445=CARTESIAN_POINT('',(102.9,6.,48.5));
#90446=CARTESIAN_POINT('Origin',(103.1,7.4,48.5));
#90447=CARTESIAN_POINT('',(103.1,7.4,48.5));
#90448=CARTESIAN_POINT('',(103.1,7.7,48.5));
#90449=CARTESIAN_POINT('',(103.1,7.4,48.35));
#90450=CARTESIAN_POINT('',(103.1,7.4,48.5));
#90451=CARTESIAN_POINT('',(103.1,6.,48.35));
#90452=CARTESIAN_POINT('Origin',(102.9,7.4,48.5));
#90453=CARTESIAN_POINT('',(102.9,7.4,48.5));
#90454=CARTESIAN_POINT('',(51.45,7.4,48.5));
#90455=CARTESIAN_POINT('',(102.9,7.4,48.35));
#90456=CARTESIAN_POINT('',(102.9,7.4,48.5));
#90457=CARTESIAN_POINT('',(103.1,7.4,48.35));
#90458=CARTESIAN_POINT('Origin',(102.9,6.,48.5));
#90459=CARTESIAN_POINT('',(102.9,7.,48.5));
#90460=CARTESIAN_POINT('',(102.9,7.4,48.35));
#90461=CARTESIAN_POINT('Origin',(103.,6.7,48.35));
#90462=CARTESIAN_POINT('Origin',(105.1,5.2,48.5));
#90463=CARTESIAN_POINT('',(105.1,5.2,48.5));
#90464=CARTESIAN_POINT('',(104.9,5.2,48.5));
#90465=CARTESIAN_POINT('',(52.55,5.2,48.5));
#90466=CARTESIAN_POINT('',(105.1,5.2,48.35));
#90467=CARTESIAN_POINT('',(105.1,5.2,48.5));
#90468=CARTESIAN_POINT('',(104.9,5.2,48.35));
#90469=CARTESIAN_POINT('',(104.9,5.2,48.35));
#90470=CARTESIAN_POINT('',(104.9,5.2,48.5));
#90471=CARTESIAN_POINT('Origin',(105.1,7.4,48.5));
#90472=CARTESIAN_POINT('',(105.1,7.4,48.5));
#90473=CARTESIAN_POINT('',(105.1,7.7,48.5));
#90474=CARTESIAN_POINT('',(105.1,7.4,48.35));
#90475=CARTESIAN_POINT('',(105.1,7.4,48.5));
#90476=CARTESIAN_POINT('',(105.1,5.2,48.35));
#90477=CARTESIAN_POINT('Origin',(104.9,7.4,48.5));
#90478=CARTESIAN_POINT('',(104.9,7.4,48.5));
#90479=CARTESIAN_POINT('',(52.45,7.4,48.5));
#90480=CARTESIAN_POINT('',(104.9,7.4,48.35));
#90481=CARTESIAN_POINT('',(104.9,7.4,48.5));
#90482=CARTESIAN_POINT('',(105.1,7.4,48.35));
#90483=CARTESIAN_POINT('Origin',(104.9,5.2,48.5));
#90484=CARTESIAN_POINT('',(104.9,6.6,48.5));
#90485=CARTESIAN_POINT('',(104.9,7.4,48.35));
#90486=CARTESIAN_POINT('Origin',(105.,6.3,48.35));
#90487=CARTESIAN_POINT('Origin',(107.1,6.,48.5));
#90488=CARTESIAN_POINT('',(107.1,6.,48.5));
#90489=CARTESIAN_POINT('',(106.9,6.,48.5));
#90490=CARTESIAN_POINT('',(53.55,6.,48.5));
#90491=CARTESIAN_POINT('',(107.1,6.,48.35));
#90492=CARTESIAN_POINT('',(107.1,6.,48.5));
#90493=CARTESIAN_POINT('',(106.9,6.,48.35));
#90494=CARTESIAN_POINT('',(106.9,6.,48.35));
#90495=CARTESIAN_POINT('',(106.9,6.,48.5));
#90496=CARTESIAN_POINT('Origin',(107.1,7.4,48.5));
#90497=CARTESIAN_POINT('',(107.1,7.4,48.5));
#90498=CARTESIAN_POINT('',(107.1,7.7,48.5));
#90499=CARTESIAN_POINT('',(107.1,7.4,48.35));
#90500=CARTESIAN_POINT('',(107.1,7.4,48.5));
#90501=CARTESIAN_POINT('',(107.1,6.,48.35));
#90502=CARTESIAN_POINT('Origin',(106.9,7.4,48.5));
#90503=CARTESIAN_POINT('',(106.9,7.4,48.5));
#90504=CARTESIAN_POINT('',(53.45,7.4,48.5));
#90505=CARTESIAN_POINT('',(106.9,7.4,48.35));
#90506=CARTESIAN_POINT('',(106.9,7.4,48.5));
#90507=CARTESIAN_POINT('',(107.1,7.4,48.35));
#90508=CARTESIAN_POINT('Origin',(106.9,6.,48.5));
#90509=CARTESIAN_POINT('',(106.9,7.,48.5));
#90510=CARTESIAN_POINT('',(106.9,7.4,48.35));
#90511=CARTESIAN_POINT('Origin',(107.,6.7,48.35));
#90512=CARTESIAN_POINT('Origin',(109.1,6.,48.5));
#90513=CARTESIAN_POINT('',(109.1,6.,48.5));
#90514=CARTESIAN_POINT('',(108.9,6.,48.5));
#90515=CARTESIAN_POINT('',(54.55,6.,48.5));
#90516=CARTESIAN_POINT('',(109.1,6.,48.35));
#90517=CARTESIAN_POINT('',(109.1,6.,48.5));
#90518=CARTESIAN_POINT('',(108.9,6.,48.35));
#90519=CARTESIAN_POINT('',(108.9,6.,48.35));
#90520=CARTESIAN_POINT('',(108.9,6.,48.5));
#90521=CARTESIAN_POINT('Origin',(109.1,7.4,48.5));
#90522=CARTESIAN_POINT('',(109.1,7.4,48.5));
#90523=CARTESIAN_POINT('',(109.1,7.7,48.5));
#90524=CARTESIAN_POINT('',(109.1,7.4,48.35));
#90525=CARTESIAN_POINT('',(109.1,7.4,48.5));
#90526=CARTESIAN_POINT('',(109.1,6.,48.35));
#90527=CARTESIAN_POINT('Origin',(108.9,7.4,48.5));
#90528=CARTESIAN_POINT('',(108.9,7.4,48.5));
#90529=CARTESIAN_POINT('',(54.45,7.4,48.5));
#90530=CARTESIAN_POINT('',(108.9,7.4,48.35));
#90531=CARTESIAN_POINT('',(108.9,7.4,48.5));
#90532=CARTESIAN_POINT('',(109.1,7.4,48.35));
#90533=CARTESIAN_POINT('Origin',(108.9,6.,48.5));
#90534=CARTESIAN_POINT('',(108.9,7.,48.5));
#90535=CARTESIAN_POINT('',(108.9,7.4,48.35));
#90536=CARTESIAN_POINT('Origin',(109.,6.7,48.35));
#90537=CARTESIAN_POINT('Origin',(20.1,4.4,48.5));
#90538=CARTESIAN_POINT('',(20.1,4.4,48.5));
#90539=CARTESIAN_POINT('',(19.9,4.4,48.5));
#90540=CARTESIAN_POINT('',(10.05,4.4,48.5));
#90541=CARTESIAN_POINT('',(20.1,4.4,48.35));
#90542=CARTESIAN_POINT('',(20.1,4.4,48.5));
#90543=CARTESIAN_POINT('',(19.9,4.4,48.35));
#90544=CARTESIAN_POINT('',(19.9,4.4,48.35));
#90545=CARTESIAN_POINT('',(19.9,4.4,48.5));
#90546=CARTESIAN_POINT('Origin',(20.1,7.4,48.5));
#90547=CARTESIAN_POINT('',(20.1,7.4,48.5));
#90548=CARTESIAN_POINT('',(20.1,7.7,48.5));
#90549=CARTESIAN_POINT('',(20.1,7.4,48.35));
#90550=CARTESIAN_POINT('',(20.1,7.4,48.5));
#90551=CARTESIAN_POINT('',(20.1,4.4,48.35));
#90552=CARTESIAN_POINT('Origin',(19.9,7.4,48.5));
#90553=CARTESIAN_POINT('',(19.9,7.4,48.5));
#90554=CARTESIAN_POINT('',(9.95,7.4,48.5));
#90555=CARTESIAN_POINT('',(19.9,7.4,48.35));
#90556=CARTESIAN_POINT('',(19.9,7.4,48.5));
#90557=CARTESIAN_POINT('',(20.1,7.4,48.35));
#90558=CARTESIAN_POINT('Origin',(19.9,4.4,48.5));
#90559=CARTESIAN_POINT('',(19.9,6.2,48.5));
#90560=CARTESIAN_POINT('',(19.9,7.4,48.35));
#90561=CARTESIAN_POINT('Origin',(20.,5.9,48.35));
#90562=CARTESIAN_POINT('Origin',(112.1,6.,48.5));
#90563=CARTESIAN_POINT('',(112.1,6.,48.5));
#90564=CARTESIAN_POINT('',(111.9,6.,48.5));
#90565=CARTESIAN_POINT('',(56.05,6.,48.5));
#90566=CARTESIAN_POINT('',(112.1,6.,48.35));
#90567=CARTESIAN_POINT('',(112.1,6.,48.5));
#90568=CARTESIAN_POINT('',(111.9,6.,48.35));
#90569=CARTESIAN_POINT('',(111.9,6.,48.35));
#90570=CARTESIAN_POINT('',(111.9,6.,48.5));
#90571=CARTESIAN_POINT('Origin',(112.1,7.4,48.5));
#90572=CARTESIAN_POINT('',(112.1,7.4,48.5));
#90573=CARTESIAN_POINT('',(112.1,7.7,48.5));
#90574=CARTESIAN_POINT('',(112.1,7.4,48.35));
#90575=CARTESIAN_POINT('',(112.1,7.4,48.5));
#90576=CARTESIAN_POINT('',(112.1,6.,48.35));
#90577=CARTESIAN_POINT('Origin',(111.9,7.4,48.5));
#90578=CARTESIAN_POINT('',(111.9,7.4,48.5));
#90579=CARTESIAN_POINT('',(55.95,7.4,48.5));
#90580=CARTESIAN_POINT('',(111.9,7.4,48.35));
#90581=CARTESIAN_POINT('',(111.9,7.4,48.5));
#90582=CARTESIAN_POINT('',(112.1,7.4,48.35));
#90583=CARTESIAN_POINT('Origin',(111.9,6.,48.5));
#90584=CARTESIAN_POINT('',(111.9,7.,48.5));
#90585=CARTESIAN_POINT('',(111.9,7.4,48.35));
#90586=CARTESIAN_POINT('Origin',(112.,6.7,48.35));
#90587=CARTESIAN_POINT('Origin',(114.1,6.,48.5));
#90588=CARTESIAN_POINT('',(114.1,6.,48.5));
#90589=CARTESIAN_POINT('',(113.9,6.,48.5));
#90590=CARTESIAN_POINT('',(57.05,6.,48.5));
#90591=CARTESIAN_POINT('',(114.1,6.,48.35));
#90592=CARTESIAN_POINT('',(114.1,6.,48.5));
#90593=CARTESIAN_POINT('',(113.9,6.,48.35));
#90594=CARTESIAN_POINT('',(113.9,6.,48.35));
#90595=CARTESIAN_POINT('',(113.9,6.,48.5));
#90596=CARTESIAN_POINT('Origin',(114.1,7.4,48.5));
#90597=CARTESIAN_POINT('',(114.1,7.4,48.5));
#90598=CARTESIAN_POINT('',(114.1,7.7,48.5));
#90599=CARTESIAN_POINT('',(114.1,7.4,48.35));
#90600=CARTESIAN_POINT('',(114.1,7.4,48.5));
#90601=CARTESIAN_POINT('',(114.1,6.,48.35));
#90602=CARTESIAN_POINT('Origin',(113.9,7.4,48.5));
#90603=CARTESIAN_POINT('',(113.9,7.4,48.5));
#90604=CARTESIAN_POINT('',(56.95,7.4,48.5));
#90605=CARTESIAN_POINT('',(113.9,7.4,48.35));
#90606=CARTESIAN_POINT('',(113.9,7.4,48.5));
#90607=CARTESIAN_POINT('',(114.1,7.4,48.35));
#90608=CARTESIAN_POINT('Origin',(113.9,6.,48.5));
#90609=CARTESIAN_POINT('',(113.9,7.,48.5));
#90610=CARTESIAN_POINT('',(113.9,7.4,48.35));
#90611=CARTESIAN_POINT('Origin',(114.,6.7,48.35));
#90612=CARTESIAN_POINT('Origin',(116.1,6.,48.5));
#90613=CARTESIAN_POINT('',(116.1,6.,48.5));
#90614=CARTESIAN_POINT('',(115.9,6.,48.5));
#90615=CARTESIAN_POINT('',(58.05,6.,48.5));
#90616=CARTESIAN_POINT('',(116.1,6.,48.35));
#90617=CARTESIAN_POINT('',(116.1,6.,48.5));
#90618=CARTESIAN_POINT('',(115.9,6.,48.35));
#90619=CARTESIAN_POINT('',(115.9,6.,48.35));
#90620=CARTESIAN_POINT('',(115.9,6.,48.5));
#90621=CARTESIAN_POINT('Origin',(116.1,7.4,48.5));
#90622=CARTESIAN_POINT('',(116.1,7.4,48.5));
#90623=CARTESIAN_POINT('',(116.1,7.7,48.5));
#90624=CARTESIAN_POINT('',(116.1,7.4,48.35));
#90625=CARTESIAN_POINT('',(116.1,7.4,48.5));
#90626=CARTESIAN_POINT('',(116.1,6.,48.35));
#90627=CARTESIAN_POINT('Origin',(115.9,7.4,48.5));
#90628=CARTESIAN_POINT('',(115.9,7.4,48.5));
#90629=CARTESIAN_POINT('',(57.95,7.4,48.5));
#90630=CARTESIAN_POINT('',(115.9,7.4,48.35));
#90631=CARTESIAN_POINT('',(115.9,7.4,48.5));
#90632=CARTESIAN_POINT('',(116.1,7.4,48.35));
#90633=CARTESIAN_POINT('Origin',(115.9,6.,48.5));
#90634=CARTESIAN_POINT('',(115.9,7.,48.5));
#90635=CARTESIAN_POINT('',(115.9,7.4,48.35));
#90636=CARTESIAN_POINT('Origin',(116.,6.7,48.35));
#90637=CARTESIAN_POINT('Origin',(118.1,6.,48.5));
#90638=CARTESIAN_POINT('',(118.1,6.,48.5));
#90639=CARTESIAN_POINT('',(117.9,6.,48.5));
#90640=CARTESIAN_POINT('',(59.05,6.,48.5));
#90641=CARTESIAN_POINT('',(118.1,6.,48.35));
#90642=CARTESIAN_POINT('',(118.1,6.,48.5));
#90643=CARTESIAN_POINT('',(117.9,6.,48.35));
#90644=CARTESIAN_POINT('',(117.9,6.,48.35));
#90645=CARTESIAN_POINT('',(117.9,6.,48.5));
#90646=CARTESIAN_POINT('Origin',(118.1,7.4,48.5));
#90647=CARTESIAN_POINT('',(118.1,7.4,48.5));
#90648=CARTESIAN_POINT('',(118.1,7.7,48.5));
#90649=CARTESIAN_POINT('',(118.1,7.4,48.35));
#90650=CARTESIAN_POINT('',(118.1,7.4,48.5));
#90651=CARTESIAN_POINT('',(118.1,6.,48.35));
#90652=CARTESIAN_POINT('Origin',(117.9,7.4,48.5));
#90653=CARTESIAN_POINT('',(117.9,7.4,48.5));
#90654=CARTESIAN_POINT('',(58.95,7.4,48.5));
#90655=CARTESIAN_POINT('',(117.9,7.4,48.35));
#90656=CARTESIAN_POINT('',(117.9,7.4,48.5));
#90657=CARTESIAN_POINT('',(118.1,7.4,48.35));
#90658=CARTESIAN_POINT('Origin',(117.9,6.,48.5));
#90659=CARTESIAN_POINT('',(117.9,7.,48.5));
#90660=CARTESIAN_POINT('',(117.9,7.4,48.35));
#90661=CARTESIAN_POINT('Origin',(118.,6.7,48.35));
#90662=CARTESIAN_POINT('Origin',(120.1,4.4,48.5));
#90663=CARTESIAN_POINT('',(120.1,4.4,48.5));
#90664=CARTESIAN_POINT('',(119.9,4.4,48.5));
#90665=CARTESIAN_POINT('',(60.05,4.4,48.5));
#90666=CARTESIAN_POINT('',(120.1,4.4,48.35));
#90667=CARTESIAN_POINT('',(120.1,4.4,48.5));
#90668=CARTESIAN_POINT('',(119.9,4.4,48.35));
#90669=CARTESIAN_POINT('',(119.9,4.4,48.35));
#90670=CARTESIAN_POINT('',(119.9,4.4,48.5));
#90671=CARTESIAN_POINT('Origin',(120.1,7.4,48.5));
#90672=CARTESIAN_POINT('',(120.1,7.4,48.5));
#90673=CARTESIAN_POINT('',(120.1,7.7,48.5));
#90674=CARTESIAN_POINT('',(120.1,7.4,48.35));
#90675=CARTESIAN_POINT('',(120.1,7.4,48.5));
#90676=CARTESIAN_POINT('',(120.1,4.4,48.35));
#90677=CARTESIAN_POINT('Origin',(119.9,7.4,48.5));
#90678=CARTESIAN_POINT('',(119.9,7.4,48.5));
#90679=CARTESIAN_POINT('',(59.95,7.4,48.5));
#90680=CARTESIAN_POINT('',(119.9,7.4,48.35));
#90681=CARTESIAN_POINT('',(119.9,7.4,48.5));
#90682=CARTESIAN_POINT('',(120.1,7.4,48.35));
#90683=CARTESIAN_POINT('Origin',(119.9,4.4,48.5));
#90684=CARTESIAN_POINT('',(119.9,6.2,48.5));
#90685=CARTESIAN_POINT('',(119.9,7.4,48.35));
#90686=CARTESIAN_POINT('Origin',(120.,5.9,48.35));
#90687=CARTESIAN_POINT('Origin',(122.1,6.,48.5));
#90688=CARTESIAN_POINT('',(122.1,6.,48.5));
#90689=CARTESIAN_POINT('',(121.9,6.,48.5));
#90690=CARTESIAN_POINT('',(61.05,6.,48.5));
#90691=CARTESIAN_POINT('',(122.1,6.,48.35));
#90692=CARTESIAN_POINT('',(122.1,6.,48.5));
#90693=CARTESIAN_POINT('',(121.9,6.,48.35));
#90694=CARTESIAN_POINT('',(121.9,6.,48.35));
#90695=CARTESIAN_POINT('',(121.9,6.,48.5));
#90696=CARTESIAN_POINT('Origin',(122.1,7.4,48.5));
#90697=CARTESIAN_POINT('',(122.1,7.4,48.5));
#90698=CARTESIAN_POINT('',(122.1,7.7,48.5));
#90699=CARTESIAN_POINT('',(122.1,7.4,48.35));
#90700=CARTESIAN_POINT('',(122.1,7.4,48.5));
#90701=CARTESIAN_POINT('',(122.1,6.,48.35));
#90702=CARTESIAN_POINT('Origin',(121.9,7.4,48.5));
#90703=CARTESIAN_POINT('',(121.9,7.4,48.5));
#90704=CARTESIAN_POINT('',(60.95,7.4,48.5));
#90705=CARTESIAN_POINT('',(121.9,7.4,48.35));
#90706=CARTESIAN_POINT('',(121.9,7.4,48.5));
#90707=CARTESIAN_POINT('',(122.1,7.4,48.35));
#90708=CARTESIAN_POINT('Origin',(121.9,6.,48.5));
#90709=CARTESIAN_POINT('',(121.9,7.,48.5));
#90710=CARTESIAN_POINT('',(121.9,7.4,48.35));
#90711=CARTESIAN_POINT('Origin',(122.,6.7,48.35));
#90712=CARTESIAN_POINT('Origin',(124.1,6.,48.5));
#90713=CARTESIAN_POINT('',(124.1,6.,48.5));
#90714=CARTESIAN_POINT('',(123.9,6.,48.5));
#90715=CARTESIAN_POINT('',(62.05,6.,48.5));
#90716=CARTESIAN_POINT('',(124.1,6.,48.35));
#90717=CARTESIAN_POINT('',(124.1,6.,48.5));
#90718=CARTESIAN_POINT('',(123.9,6.,48.35));
#90719=CARTESIAN_POINT('',(123.9,6.,48.35));
#90720=CARTESIAN_POINT('',(123.9,6.,48.5));
#90721=CARTESIAN_POINT('Origin',(124.1,7.4,48.5));
#90722=CARTESIAN_POINT('',(124.1,7.4,48.5));
#90723=CARTESIAN_POINT('',(124.1,7.7,48.5));
#90724=CARTESIAN_POINT('',(124.1,7.4,48.35));
#90725=CARTESIAN_POINT('',(124.1,7.4,48.5));
#90726=CARTESIAN_POINT('',(124.1,6.,48.35));
#90727=CARTESIAN_POINT('Origin',(123.9,7.4,48.5));
#90728=CARTESIAN_POINT('',(123.9,7.4,48.5));
#90729=CARTESIAN_POINT('',(61.95,7.4,48.5));
#90730=CARTESIAN_POINT('',(123.9,7.4,48.35));
#90731=CARTESIAN_POINT('',(123.9,7.4,48.5));
#90732=CARTESIAN_POINT('',(124.1,7.4,48.35));
#90733=CARTESIAN_POINT('Origin',(123.9,6.,48.5));
#90734=CARTESIAN_POINT('',(123.9,7.,48.5));
#90735=CARTESIAN_POINT('',(123.9,7.4,48.35));
#90736=CARTESIAN_POINT('Origin',(124.,6.7,48.35));
#90737=CARTESIAN_POINT('Origin',(126.1,6.,48.5));
#90738=CARTESIAN_POINT('',(126.1,6.,48.5));
#90739=CARTESIAN_POINT('',(125.9,6.,48.5));
#90740=CARTESIAN_POINT('',(63.05,6.,48.5));
#90741=CARTESIAN_POINT('',(126.1,6.,48.35));
#90742=CARTESIAN_POINT('',(126.1,6.,48.5));
#90743=CARTESIAN_POINT('',(125.9,6.,48.35));
#90744=CARTESIAN_POINT('',(125.9,6.,48.35));
#90745=CARTESIAN_POINT('',(125.9,6.,48.5));
#90746=CARTESIAN_POINT('Origin',(126.1,7.4,48.5));
#90747=CARTESIAN_POINT('',(126.1,7.4,48.5));
#90748=CARTESIAN_POINT('',(126.1,7.7,48.5));
#90749=CARTESIAN_POINT('',(126.1,7.4,48.35));
#90750=CARTESIAN_POINT('',(126.1,7.4,48.5));
#90751=CARTESIAN_POINT('',(126.1,6.,48.35));
#90752=CARTESIAN_POINT('Origin',(125.9,7.4,48.5));
#90753=CARTESIAN_POINT('',(125.9,7.4,48.5));
#90754=CARTESIAN_POINT('',(62.95,7.4,48.5));
#90755=CARTESIAN_POINT('',(125.9,7.4,48.35));
#90756=CARTESIAN_POINT('',(125.9,7.4,48.5));
#90757=CARTESIAN_POINT('',(126.1,7.4,48.35));
#90758=CARTESIAN_POINT('Origin',(125.9,6.,48.5));
#90759=CARTESIAN_POINT('',(125.9,7.,48.5));
#90760=CARTESIAN_POINT('',(125.9,7.4,48.35));
#90761=CARTESIAN_POINT('Origin',(126.,6.7,48.35));
#90762=CARTESIAN_POINT('Origin',(128.1,6.,48.5));
#90763=CARTESIAN_POINT('',(128.1,6.,48.5));
#90764=CARTESIAN_POINT('',(127.9,6.,48.5));
#90765=CARTESIAN_POINT('',(64.05,6.,48.5));
#90766=CARTESIAN_POINT('',(128.1,6.,48.35));
#90767=CARTESIAN_POINT('',(128.1,6.,48.5));
#90768=CARTESIAN_POINT('',(127.9,6.,48.35));
#90769=CARTESIAN_POINT('',(127.9,6.,48.35));
#90770=CARTESIAN_POINT('',(127.9,6.,48.5));
#90771=CARTESIAN_POINT('Origin',(128.1,7.4,48.5));
#90772=CARTESIAN_POINT('',(128.1,7.4,48.5));
#90773=CARTESIAN_POINT('',(128.1,7.7,48.5));
#90774=CARTESIAN_POINT('',(128.1,7.4,48.35));
#90775=CARTESIAN_POINT('',(128.1,7.4,48.5));
#90776=CARTESIAN_POINT('',(128.1,6.,48.35));
#90777=CARTESIAN_POINT('Origin',(127.9,7.4,48.5));
#90778=CARTESIAN_POINT('',(127.9,7.4,48.5));
#90779=CARTESIAN_POINT('',(63.95,7.4,48.5));
#90780=CARTESIAN_POINT('',(127.9,7.4,48.35));
#90781=CARTESIAN_POINT('',(127.9,7.4,48.5));
#90782=CARTESIAN_POINT('',(128.1,7.4,48.35));
#90783=CARTESIAN_POINT('Origin',(127.9,6.,48.5));
#90784=CARTESIAN_POINT('',(127.9,7.,48.5));
#90785=CARTESIAN_POINT('',(127.9,7.4,48.35));
#90786=CARTESIAN_POINT('Origin',(128.,6.7,48.35));
#90787=CARTESIAN_POINT('Origin',(130.1,4.4,48.5));
#90788=CARTESIAN_POINT('',(130.1,4.4,48.5));
#90789=CARTESIAN_POINT('',(129.9,4.4,48.5));
#90790=CARTESIAN_POINT('',(65.05,4.4,48.5));
#90791=CARTESIAN_POINT('',(130.1,4.4,48.35));
#90792=CARTESIAN_POINT('',(130.1,4.4,48.5));
#90793=CARTESIAN_POINT('',(129.9,4.4,48.35));
#90794=CARTESIAN_POINT('',(129.9,4.4,48.35));
#90795=CARTESIAN_POINT('',(129.9,4.4,48.5));
#90796=CARTESIAN_POINT('Origin',(130.1,7.4,48.5));
#90797=CARTESIAN_POINT('',(130.1,7.4,48.5));
#90798=CARTESIAN_POINT('',(130.1,7.7,48.5));
#90799=CARTESIAN_POINT('',(130.1,7.4,48.35));
#90800=CARTESIAN_POINT('',(130.1,7.4,48.5));
#90801=CARTESIAN_POINT('',(130.1,4.4,48.35));
#90802=CARTESIAN_POINT('Origin',(129.9,7.4,48.5));
#90803=CARTESIAN_POINT('',(129.9,7.4,48.5));
#90804=CARTESIAN_POINT('',(64.95,7.4,48.5));
#90805=CARTESIAN_POINT('',(129.9,7.4,48.35));
#90806=CARTESIAN_POINT('',(129.9,7.4,48.5));
#90807=CARTESIAN_POINT('',(130.1,7.4,48.35));
#90808=CARTESIAN_POINT('Origin',(129.9,4.4,48.5));
#90809=CARTESIAN_POINT('',(129.9,6.2,48.5));
#90810=CARTESIAN_POINT('',(129.9,7.4,48.35));
#90811=CARTESIAN_POINT('Origin',(130.,5.9,48.35));
#90812=CARTESIAN_POINT('Origin',(132.1,6.,48.5));
#90813=CARTESIAN_POINT('',(132.1,6.,48.5));
#90814=CARTESIAN_POINT('',(131.9,6.,48.5));
#90815=CARTESIAN_POINT('',(66.05,6.,48.5));
#90816=CARTESIAN_POINT('',(132.1,6.,48.35));
#90817=CARTESIAN_POINT('',(132.1,6.,48.5));
#90818=CARTESIAN_POINT('',(131.9,6.,48.35));
#90819=CARTESIAN_POINT('',(131.9,6.,48.35));
#90820=CARTESIAN_POINT('',(131.9,6.,48.5));
#90821=CARTESIAN_POINT('Origin',(132.1,7.4,48.5));
#90822=CARTESIAN_POINT('',(132.1,7.4,48.5));
#90823=CARTESIAN_POINT('',(132.1,7.7,48.5));
#90824=CARTESIAN_POINT('',(132.1,7.4,48.35));
#90825=CARTESIAN_POINT('',(132.1,7.4,48.5));
#90826=CARTESIAN_POINT('',(132.1,6.,48.35));
#90827=CARTESIAN_POINT('Origin',(131.9,7.4,48.5));
#90828=CARTESIAN_POINT('',(131.9,7.4,48.5));
#90829=CARTESIAN_POINT('',(65.95,7.4,48.5));
#90830=CARTESIAN_POINT('',(131.9,7.4,48.35));
#90831=CARTESIAN_POINT('',(131.9,7.4,48.5));
#90832=CARTESIAN_POINT('',(132.1,7.4,48.35));
#90833=CARTESIAN_POINT('Origin',(131.9,6.,48.5));
#90834=CARTESIAN_POINT('',(131.9,7.,48.5));
#90835=CARTESIAN_POINT('',(131.9,7.4,48.35));
#90836=CARTESIAN_POINT('Origin',(132.,6.7,48.35));
#90837=CARTESIAN_POINT('Origin',(134.1,6.,48.5));
#90838=CARTESIAN_POINT('',(134.1,6.,48.5));
#90839=CARTESIAN_POINT('',(133.9,6.,48.5));
#90840=CARTESIAN_POINT('',(67.05,6.,48.5));
#90841=CARTESIAN_POINT('',(134.1,6.,48.35));
#90842=CARTESIAN_POINT('',(134.1,6.,48.5));
#90843=CARTESIAN_POINT('',(133.9,6.,48.35));
#90844=CARTESIAN_POINT('',(133.9,6.,48.35));
#90845=CARTESIAN_POINT('',(133.9,6.,48.5));
#90846=CARTESIAN_POINT('Origin',(134.1,7.4,48.5));
#90847=CARTESIAN_POINT('',(134.1,7.4,48.5));
#90848=CARTESIAN_POINT('',(134.1,7.7,48.5));
#90849=CARTESIAN_POINT('',(134.1,7.4,48.35));
#90850=CARTESIAN_POINT('',(134.1,7.4,48.5));
#90851=CARTESIAN_POINT('',(134.1,6.,48.35));
#90852=CARTESIAN_POINT('Origin',(133.9,7.4,48.5));
#90853=CARTESIAN_POINT('',(133.9,7.4,48.5));
#90854=CARTESIAN_POINT('',(66.95,7.4,48.5));
#90855=CARTESIAN_POINT('',(133.9,7.4,48.35));
#90856=CARTESIAN_POINT('',(133.9,7.4,48.5));
#90857=CARTESIAN_POINT('',(134.1,7.4,48.35));
#90858=CARTESIAN_POINT('Origin',(133.9,6.,48.5));
#90859=CARTESIAN_POINT('',(133.9,7.,48.5));
#90860=CARTESIAN_POINT('',(133.9,7.4,48.35));
#90861=CARTESIAN_POINT('Origin',(134.,6.7,48.35));
#90862=CARTESIAN_POINT('Origin',(136.1,6.,48.5));
#90863=CARTESIAN_POINT('',(136.1,6.,48.5));
#90864=CARTESIAN_POINT('',(135.9,6.,48.5));
#90865=CARTESIAN_POINT('',(68.05,6.,48.5));
#90866=CARTESIAN_POINT('',(136.1,6.,48.35));
#90867=CARTESIAN_POINT('',(136.1,6.,48.5));
#90868=CARTESIAN_POINT('',(135.9,6.,48.35));
#90869=CARTESIAN_POINT('',(135.9,6.,48.35));
#90870=CARTESIAN_POINT('',(135.9,6.,48.5));
#90871=CARTESIAN_POINT('Origin',(136.1,7.4,48.5));
#90872=CARTESIAN_POINT('',(136.1,7.4,48.5));
#90873=CARTESIAN_POINT('',(136.1,7.7,48.5));
#90874=CARTESIAN_POINT('',(136.1,7.4,48.35));
#90875=CARTESIAN_POINT('',(136.1,7.4,48.5));
#90876=CARTESIAN_POINT('',(136.1,6.,48.35));
#90877=CARTESIAN_POINT('Origin',(135.9,7.4,48.5));
#90878=CARTESIAN_POINT('',(135.9,7.4,48.5));
#90879=CARTESIAN_POINT('',(67.95,7.4,48.5));
#90880=CARTESIAN_POINT('',(135.9,7.4,48.35));
#90881=CARTESIAN_POINT('',(135.9,7.4,48.5));
#90882=CARTESIAN_POINT('',(136.1,7.4,48.35));
#90883=CARTESIAN_POINT('Origin',(135.9,6.,48.5));
#90884=CARTESIAN_POINT('',(135.9,7.,48.5));
#90885=CARTESIAN_POINT('',(135.9,7.4,48.35));
#90886=CARTESIAN_POINT('Origin',(136.,6.7,48.35));
#90887=CARTESIAN_POINT('Origin',(138.1,6.,48.5));
#90888=CARTESIAN_POINT('',(138.1,6.,48.5));
#90889=CARTESIAN_POINT('',(137.9,6.,48.5));
#90890=CARTESIAN_POINT('',(69.05,6.,48.5));
#90891=CARTESIAN_POINT('',(138.1,6.,48.35));
#90892=CARTESIAN_POINT('',(138.1,6.,48.5));
#90893=CARTESIAN_POINT('',(137.9,6.,48.35));
#90894=CARTESIAN_POINT('',(137.9,6.,48.35));
#90895=CARTESIAN_POINT('',(137.9,6.,48.5));
#90896=CARTESIAN_POINT('Origin',(138.1,7.4,48.5));
#90897=CARTESIAN_POINT('',(138.1,7.4,48.5));
#90898=CARTESIAN_POINT('',(138.1,7.7,48.5));
#90899=CARTESIAN_POINT('',(138.1,7.4,48.35));
#90900=CARTESIAN_POINT('',(138.1,7.4,48.5));
#90901=CARTESIAN_POINT('',(138.1,6.,48.35));
#90902=CARTESIAN_POINT('Origin',(137.9,7.4,48.5));
#90903=CARTESIAN_POINT('',(137.9,7.4,48.5));
#90904=CARTESIAN_POINT('',(68.95,7.4,48.5));
#90905=CARTESIAN_POINT('',(137.9,7.4,48.35));
#90906=CARTESIAN_POINT('',(137.9,7.4,48.5));
#90907=CARTESIAN_POINT('',(138.1,7.4,48.35));
#90908=CARTESIAN_POINT('Origin',(137.9,6.,48.5));
#90909=CARTESIAN_POINT('',(137.9,7.,48.5));
#90910=CARTESIAN_POINT('',(137.9,7.4,48.35));
#90911=CARTESIAN_POINT('Origin',(138.,6.7,48.35));
#90912=CARTESIAN_POINT('Origin',(140.1,4.4,48.5));
#90913=CARTESIAN_POINT('',(140.1,4.4,48.5));
#90914=CARTESIAN_POINT('',(139.9,4.4,48.5));
#90915=CARTESIAN_POINT('',(70.05,4.4,48.5));
#90916=CARTESIAN_POINT('',(140.1,4.4,48.35));
#90917=CARTESIAN_POINT('',(140.1,4.4,48.5));
#90918=CARTESIAN_POINT('',(139.9,4.4,48.35));
#90919=CARTESIAN_POINT('',(139.9,4.4,48.35));
#90920=CARTESIAN_POINT('',(139.9,4.4,48.5));
#90921=CARTESIAN_POINT('Origin',(140.1,7.4,48.5));
#90922=CARTESIAN_POINT('',(140.1,7.4,48.5));
#90923=CARTESIAN_POINT('',(140.1,7.7,48.5));
#90924=CARTESIAN_POINT('',(140.1,7.4,48.35));
#90925=CARTESIAN_POINT('',(140.1,7.4,48.5));
#90926=CARTESIAN_POINT('',(140.1,4.4,48.35));
#90927=CARTESIAN_POINT('Origin',(139.9,7.4,48.5));
#90928=CARTESIAN_POINT('',(139.9,7.4,48.5));
#90929=CARTESIAN_POINT('',(69.95,7.4,48.5));
#90930=CARTESIAN_POINT('',(139.9,7.4,48.35));
#90931=CARTESIAN_POINT('',(139.9,7.4,48.5));
#90932=CARTESIAN_POINT('',(140.1,7.4,48.35));
#90933=CARTESIAN_POINT('Origin',(139.9,4.4,48.5));
#90934=CARTESIAN_POINT('',(139.9,6.2,48.5));
#90935=CARTESIAN_POINT('',(139.9,7.4,48.35));
#90936=CARTESIAN_POINT('Origin',(140.,5.9,48.35));
#90937=CARTESIAN_POINT('Origin',(142.1,6.,48.5));
#90938=CARTESIAN_POINT('',(142.1,6.,48.5));
#90939=CARTESIAN_POINT('',(141.9,6.,48.5));
#90940=CARTESIAN_POINT('',(71.05,6.,48.5));
#90941=CARTESIAN_POINT('',(142.1,6.,48.35));
#90942=CARTESIAN_POINT('',(142.1,6.,48.5));
#90943=CARTESIAN_POINT('',(141.9,6.,48.35));
#90944=CARTESIAN_POINT('',(141.9,6.,48.35));
#90945=CARTESIAN_POINT('',(141.9,6.,48.5));
#90946=CARTESIAN_POINT('Origin',(142.1,7.4,48.5));
#90947=CARTESIAN_POINT('',(142.1,7.4,48.5));
#90948=CARTESIAN_POINT('',(142.1,7.7,48.5));
#90949=CARTESIAN_POINT('',(142.1,7.4,48.35));
#90950=CARTESIAN_POINT('',(142.1,7.4,48.5));
#90951=CARTESIAN_POINT('',(142.1,6.,48.35));
#90952=CARTESIAN_POINT('Origin',(141.9,7.4,48.5));
#90953=CARTESIAN_POINT('',(141.9,7.4,48.5));
#90954=CARTESIAN_POINT('',(70.95,7.4,48.5));
#90955=CARTESIAN_POINT('',(141.9,7.4,48.35));
#90956=CARTESIAN_POINT('',(141.9,7.4,48.5));
#90957=CARTESIAN_POINT('',(142.1,7.4,48.35));
#90958=CARTESIAN_POINT('Origin',(141.9,6.,48.5));
#90959=CARTESIAN_POINT('',(141.9,7.,48.5));
#90960=CARTESIAN_POINT('',(141.9,7.4,48.35));
#90961=CARTESIAN_POINT('Origin',(142.,6.7,48.35));
#90962=CARTESIAN_POINT('Origin',(144.1,6.,48.5));
#90963=CARTESIAN_POINT('',(144.1,6.,48.5));
#90964=CARTESIAN_POINT('',(143.9,6.,48.5));
#90965=CARTESIAN_POINT('',(72.05,6.,48.5));
#90966=CARTESIAN_POINT('',(144.1,6.,48.35));
#90967=CARTESIAN_POINT('',(144.1,6.,48.5));
#90968=CARTESIAN_POINT('',(143.9,6.,48.35));
#90969=CARTESIAN_POINT('',(143.9,6.,48.35));
#90970=CARTESIAN_POINT('',(143.9,6.,48.5));
#90971=CARTESIAN_POINT('Origin',(144.1,7.4,48.5));
#90972=CARTESIAN_POINT('',(144.1,7.4,48.5));
#90973=CARTESIAN_POINT('',(144.1,7.7,48.5));
#90974=CARTESIAN_POINT('',(144.1,7.4,48.35));
#90975=CARTESIAN_POINT('',(144.1,7.4,48.5));
#90976=CARTESIAN_POINT('',(144.1,6.,48.35));
#90977=CARTESIAN_POINT('Origin',(143.9,7.4,48.5));
#90978=CARTESIAN_POINT('',(143.9,7.4,48.5));
#90979=CARTESIAN_POINT('',(71.95,7.4,48.5));
#90980=CARTESIAN_POINT('',(143.9,7.4,48.35));
#90981=CARTESIAN_POINT('',(143.9,7.4,48.5));
#90982=CARTESIAN_POINT('',(144.1,7.4,48.35));
#90983=CARTESIAN_POINT('Origin',(143.9,6.,48.5));
#90984=CARTESIAN_POINT('',(143.9,7.,48.5));
#90985=CARTESIAN_POINT('',(143.9,7.4,48.35));
#90986=CARTESIAN_POINT('Origin',(144.,6.7,48.35));
#90987=CARTESIAN_POINT('Origin',(146.1,6.,48.5));
#90988=CARTESIAN_POINT('',(146.1,6.,48.5));
#90989=CARTESIAN_POINT('',(145.9,6.,48.5));
#90990=CARTESIAN_POINT('',(73.05,6.,48.5));
#90991=CARTESIAN_POINT('',(146.1,6.,48.35));
#90992=CARTESIAN_POINT('',(146.1,6.,48.5));
#90993=CARTESIAN_POINT('',(145.9,6.,48.35));
#90994=CARTESIAN_POINT('',(145.9,6.,48.35));
#90995=CARTESIAN_POINT('',(145.9,6.,48.5));
#90996=CARTESIAN_POINT('Origin',(146.1,7.4,48.5));
#90997=CARTESIAN_POINT('',(146.1,7.4,48.5));
#90998=CARTESIAN_POINT('',(146.1,7.7,48.5));
#90999=CARTESIAN_POINT('',(146.1,7.4,48.35));
#91000=CARTESIAN_POINT('',(146.1,7.4,48.5));
#91001=CARTESIAN_POINT('',(146.1,6.,48.35));
#91002=CARTESIAN_POINT('Origin',(145.9,7.4,48.5));
#91003=CARTESIAN_POINT('',(145.9,7.4,48.5));
#91004=CARTESIAN_POINT('',(72.95,7.4,48.5));
#91005=CARTESIAN_POINT('',(145.9,7.4,48.35));
#91006=CARTESIAN_POINT('',(145.9,7.4,48.5));
#91007=CARTESIAN_POINT('',(146.1,7.4,48.35));
#91008=CARTESIAN_POINT('Origin',(145.9,6.,48.5));
#91009=CARTESIAN_POINT('',(145.9,7.,48.5));
#91010=CARTESIAN_POINT('',(145.9,7.4,48.35));
#91011=CARTESIAN_POINT('Origin',(146.,6.7,48.35));
#91012=CARTESIAN_POINT('Origin',(148.1,6.,48.5));
#91013=CARTESIAN_POINT('',(148.1,6.,48.5));
#91014=CARTESIAN_POINT('',(147.9,6.,48.5));
#91015=CARTESIAN_POINT('',(74.05,6.,48.5));
#91016=CARTESIAN_POINT('',(148.1,6.,48.35));
#91017=CARTESIAN_POINT('',(148.1,6.,48.5));
#91018=CARTESIAN_POINT('',(147.9,6.,48.35));
#91019=CARTESIAN_POINT('',(147.9,6.,48.35));
#91020=CARTESIAN_POINT('',(147.9,6.,48.5));
#91021=CARTESIAN_POINT('Origin',(148.1,7.4,48.5));
#91022=CARTESIAN_POINT('',(148.1,7.4,48.5));
#91023=CARTESIAN_POINT('',(148.1,7.7,48.5));
#91024=CARTESIAN_POINT('',(148.1,7.4,48.35));
#91025=CARTESIAN_POINT('',(148.1,7.4,48.5));
#91026=CARTESIAN_POINT('',(148.1,6.,48.35));
#91027=CARTESIAN_POINT('Origin',(147.9,7.4,48.5));
#91028=CARTESIAN_POINT('',(147.9,7.4,48.5));
#91029=CARTESIAN_POINT('',(73.95,7.4,48.5));
#91030=CARTESIAN_POINT('',(147.9,7.4,48.35));
#91031=CARTESIAN_POINT('',(147.9,7.4,48.5));
#91032=CARTESIAN_POINT('',(148.1,7.4,48.35));
#91033=CARTESIAN_POINT('Origin',(147.9,6.,48.5));
#91034=CARTESIAN_POINT('',(147.9,7.,48.5));
#91035=CARTESIAN_POINT('',(147.9,7.4,48.35));
#91036=CARTESIAN_POINT('Origin',(148.,6.7,48.35));
#91037=CARTESIAN_POINT('Origin',(150.1,4.4,48.5));
#91038=CARTESIAN_POINT('',(150.1,4.4,48.5));
#91039=CARTESIAN_POINT('',(149.9,4.4,48.5));
#91040=CARTESIAN_POINT('',(75.05,4.4,48.5));
#91041=CARTESIAN_POINT('',(150.1,4.4,48.35));
#91042=CARTESIAN_POINT('',(150.1,4.4,48.5));
#91043=CARTESIAN_POINT('',(149.9,4.4,48.35));
#91044=CARTESIAN_POINT('',(149.9,4.4,48.35));
#91045=CARTESIAN_POINT('',(149.9,4.4,48.5));
#91046=CARTESIAN_POINT('Origin',(150.1,7.4,48.5));
#91047=CARTESIAN_POINT('',(150.1,7.4,48.5));
#91048=CARTESIAN_POINT('',(150.1,7.7,48.5));
#91049=CARTESIAN_POINT('',(150.1,7.4,48.35));
#91050=CARTESIAN_POINT('',(150.1,7.4,48.5));
#91051=CARTESIAN_POINT('',(150.1,4.4,48.35));
#91052=CARTESIAN_POINT('Origin',(149.9,7.4,48.5));
#91053=CARTESIAN_POINT('',(149.9,7.4,48.5));
#91054=CARTESIAN_POINT('',(74.95,7.4,48.5));
#91055=CARTESIAN_POINT('',(149.9,7.4,48.35));
#91056=CARTESIAN_POINT('',(149.9,7.4,48.5));
#91057=CARTESIAN_POINT('',(150.1,7.4,48.35));
#91058=CARTESIAN_POINT('Origin',(149.9,4.4,48.5));
#91059=CARTESIAN_POINT('',(149.9,6.2,48.5));
#91060=CARTESIAN_POINT('',(149.9,7.4,48.35));
#91061=CARTESIAN_POINT('Origin',(150.,5.9,48.35));
#91062=CARTESIAN_POINT('Origin',(152.1,6.,48.5));
#91063=CARTESIAN_POINT('',(152.1,6.,48.5));
#91064=CARTESIAN_POINT('',(151.9,6.,48.5));
#91065=CARTESIAN_POINT('',(76.05,6.,48.5));
#91066=CARTESIAN_POINT('',(152.1,6.,48.35));
#91067=CARTESIAN_POINT('',(152.1,6.,48.5));
#91068=CARTESIAN_POINT('',(151.9,6.,48.35));
#91069=CARTESIAN_POINT('',(151.9,6.,48.35));
#91070=CARTESIAN_POINT('',(151.9,6.,48.5));
#91071=CARTESIAN_POINT('Origin',(152.1,7.4,48.5));
#91072=CARTESIAN_POINT('',(152.1,7.4,48.5));
#91073=CARTESIAN_POINT('',(152.1,7.7,48.5));
#91074=CARTESIAN_POINT('',(152.1,7.4,48.35));
#91075=CARTESIAN_POINT('',(152.1,7.4,48.5));
#91076=CARTESIAN_POINT('',(152.1,6.,48.35));
#91077=CARTESIAN_POINT('Origin',(151.9,7.4,48.5));
#91078=CARTESIAN_POINT('',(151.9,7.4,48.5));
#91079=CARTESIAN_POINT('',(75.95,7.4,48.5));
#91080=CARTESIAN_POINT('',(151.9,7.4,48.35));
#91081=CARTESIAN_POINT('',(151.9,7.4,48.5));
#91082=CARTESIAN_POINT('',(152.1,7.4,48.35));
#91083=CARTESIAN_POINT('Origin',(151.9,6.,48.5));
#91084=CARTESIAN_POINT('',(151.9,7.,48.5));
#91085=CARTESIAN_POINT('',(151.9,7.4,48.35));
#91086=CARTESIAN_POINT('Origin',(152.,6.7,48.35));
#91087=CARTESIAN_POINT('Origin',(154.1,6.,48.5));
#91088=CARTESIAN_POINT('',(154.1,6.,48.5));
#91089=CARTESIAN_POINT('',(153.9,6.,48.5));
#91090=CARTESIAN_POINT('',(77.05,6.,48.5));
#91091=CARTESIAN_POINT('',(154.1,6.,48.35));
#91092=CARTESIAN_POINT('',(154.1,6.,48.5));
#91093=CARTESIAN_POINT('',(153.9,6.,48.35));
#91094=CARTESIAN_POINT('',(153.9,6.,48.35));
#91095=CARTESIAN_POINT('',(153.9,6.,48.5));
#91096=CARTESIAN_POINT('Origin',(154.1,7.4,48.5));
#91097=CARTESIAN_POINT('',(154.1,7.4,48.5));
#91098=CARTESIAN_POINT('',(154.1,7.7,48.5));
#91099=CARTESIAN_POINT('',(154.1,7.4,48.35));
#91100=CARTESIAN_POINT('',(154.1,7.4,48.5));
#91101=CARTESIAN_POINT('',(154.1,6.,48.35));
#91102=CARTESIAN_POINT('Origin',(153.9,7.4,48.5));
#91103=CARTESIAN_POINT('',(153.9,7.4,48.5));
#91104=CARTESIAN_POINT('',(76.95,7.4,48.5));
#91105=CARTESIAN_POINT('',(153.9,7.4,48.35));
#91106=CARTESIAN_POINT('',(153.9,7.4,48.5));
#91107=CARTESIAN_POINT('',(154.1,7.4,48.35));
#91108=CARTESIAN_POINT('Origin',(153.9,6.,48.5));
#91109=CARTESIAN_POINT('',(153.9,7.,48.5));
#91110=CARTESIAN_POINT('',(153.9,7.4,48.35));
#91111=CARTESIAN_POINT('Origin',(154.,6.7,48.35));
#91112=CARTESIAN_POINT('Origin',(156.1,6.,48.5));
#91113=CARTESIAN_POINT('',(156.1,6.,48.5));
#91114=CARTESIAN_POINT('',(155.9,6.,48.5));
#91115=CARTESIAN_POINT('',(78.05,6.,48.5));
#91116=CARTESIAN_POINT('',(156.1,6.,48.35));
#91117=CARTESIAN_POINT('',(156.1,6.,48.5));
#91118=CARTESIAN_POINT('',(155.9,6.,48.35));
#91119=CARTESIAN_POINT('',(155.9,6.,48.35));
#91120=CARTESIAN_POINT('',(155.9,6.,48.5));
#91121=CARTESIAN_POINT('Origin',(156.1,7.4,48.5));
#91122=CARTESIAN_POINT('',(156.1,7.4,48.5));
#91123=CARTESIAN_POINT('',(156.1,7.7,48.5));
#91124=CARTESIAN_POINT('',(156.1,7.4,48.35));
#91125=CARTESIAN_POINT('',(156.1,7.4,48.5));
#91126=CARTESIAN_POINT('',(156.1,6.,48.35));
#91127=CARTESIAN_POINT('Origin',(155.9,7.4,48.5));
#91128=CARTESIAN_POINT('',(155.9,7.4,48.5));
#91129=CARTESIAN_POINT('',(77.95,7.4,48.5));
#91130=CARTESIAN_POINT('',(155.9,7.4,48.35));
#91131=CARTESIAN_POINT('',(155.9,7.4,48.5));
#91132=CARTESIAN_POINT('',(156.1,7.4,48.35));
#91133=CARTESIAN_POINT('Origin',(155.9,6.,48.5));
#91134=CARTESIAN_POINT('',(155.9,7.,48.5));
#91135=CARTESIAN_POINT('',(155.9,7.4,48.35));
#91136=CARTESIAN_POINT('Origin',(156.,6.7,48.35));
#91137=CARTESIAN_POINT('Origin',(158.1,6.,48.5));
#91138=CARTESIAN_POINT('',(158.1,6.,48.5));
#91139=CARTESIAN_POINT('',(157.9,6.,48.5));
#91140=CARTESIAN_POINT('',(79.05,6.,48.5));
#91141=CARTESIAN_POINT('',(158.1,6.,48.35));
#91142=CARTESIAN_POINT('',(158.1,6.,48.5));
#91143=CARTESIAN_POINT('',(157.9,6.,48.35));
#91144=CARTESIAN_POINT('',(157.9,6.,48.35));
#91145=CARTESIAN_POINT('',(157.9,6.,48.5));
#91146=CARTESIAN_POINT('Origin',(158.1,7.4,48.5));
#91147=CARTESIAN_POINT('',(158.1,7.4,48.5));
#91148=CARTESIAN_POINT('',(158.1,7.7,48.5));
#91149=CARTESIAN_POINT('',(158.1,7.4,48.35));
#91150=CARTESIAN_POINT('',(158.1,7.4,48.5));
#91151=CARTESIAN_POINT('',(158.1,6.,48.35));
#91152=CARTESIAN_POINT('Origin',(157.9,7.4,48.5));
#91153=CARTESIAN_POINT('',(157.9,7.4,48.5));
#91154=CARTESIAN_POINT('',(78.95,7.4,48.5));
#91155=CARTESIAN_POINT('',(157.9,7.4,48.35));
#91156=CARTESIAN_POINT('',(157.9,7.4,48.5));
#91157=CARTESIAN_POINT('',(158.1,7.4,48.35));
#91158=CARTESIAN_POINT('Origin',(157.9,6.,48.5));
#91159=CARTESIAN_POINT('',(157.9,7.,48.5));
#91160=CARTESIAN_POINT('',(157.9,7.4,48.35));
#91161=CARTESIAN_POINT('Origin',(158.,6.7,48.35));
#91162=CARTESIAN_POINT('Origin',(160.1,4.4,48.5));
#91163=CARTESIAN_POINT('',(160.1,4.4,48.5));
#91164=CARTESIAN_POINT('',(159.9,4.4,48.5));
#91165=CARTESIAN_POINT('',(80.05,4.4,48.5));
#91166=CARTESIAN_POINT('',(160.1,4.4,48.35));
#91167=CARTESIAN_POINT('',(160.1,4.4,48.5));
#91168=CARTESIAN_POINT('',(159.9,4.4,48.35));
#91169=CARTESIAN_POINT('',(159.9,4.4,48.35));
#91170=CARTESIAN_POINT('',(159.9,4.4,48.5));
#91171=CARTESIAN_POINT('Origin',(160.1,7.4,48.5));
#91172=CARTESIAN_POINT('',(160.1,7.4,48.5));
#91173=CARTESIAN_POINT('',(160.1,7.7,48.5));
#91174=CARTESIAN_POINT('',(160.1,7.4,48.35));
#91175=CARTESIAN_POINT('',(160.1,7.4,48.5));
#91176=CARTESIAN_POINT('',(160.1,4.4,48.35));
#91177=CARTESIAN_POINT('Origin',(159.9,7.4,48.5));
#91178=CARTESIAN_POINT('',(159.9,7.4,48.5));
#91179=CARTESIAN_POINT('',(79.95,7.4,48.5));
#91180=CARTESIAN_POINT('',(159.9,7.4,48.35));
#91181=CARTESIAN_POINT('',(159.9,7.4,48.5));
#91182=CARTESIAN_POINT('',(160.1,7.4,48.35));
#91183=CARTESIAN_POINT('Origin',(159.9,4.4,48.5));
#91184=CARTESIAN_POINT('',(159.9,6.2,48.5));
#91185=CARTESIAN_POINT('',(159.9,7.4,48.35));
#91186=CARTESIAN_POINT('Origin',(160.,5.9,48.35));
#91187=CARTESIAN_POINT('Origin',(162.1,6.,48.5));
#91188=CARTESIAN_POINT('',(162.1,6.,48.5));
#91189=CARTESIAN_POINT('',(161.9,6.,48.5));
#91190=CARTESIAN_POINT('',(81.05,6.,48.5));
#91191=CARTESIAN_POINT('',(162.1,6.,48.35));
#91192=CARTESIAN_POINT('',(162.1,6.,48.5));
#91193=CARTESIAN_POINT('',(161.9,6.,48.35));
#91194=CARTESIAN_POINT('',(161.9,6.,48.35));
#91195=CARTESIAN_POINT('',(161.9,6.,48.5));
#91196=CARTESIAN_POINT('Origin',(162.1,7.4,48.5));
#91197=CARTESIAN_POINT('',(162.1,7.4,48.5));
#91198=CARTESIAN_POINT('',(162.1,7.7,48.5));
#91199=CARTESIAN_POINT('',(162.1,7.4,48.35));
#91200=CARTESIAN_POINT('',(162.1,7.4,48.5));
#91201=CARTESIAN_POINT('',(162.1,6.,48.35));
#91202=CARTESIAN_POINT('Origin',(161.9,7.4,48.5));
#91203=CARTESIAN_POINT('',(161.9,7.4,48.5));
#91204=CARTESIAN_POINT('',(80.95,7.4,48.5));
#91205=CARTESIAN_POINT('',(161.9,7.4,48.35));
#91206=CARTESIAN_POINT('',(161.9,7.4,48.5));
#91207=CARTESIAN_POINT('',(162.1,7.4,48.35));
#91208=CARTESIAN_POINT('Origin',(161.9,6.,48.5));
#91209=CARTESIAN_POINT('',(161.9,7.,48.5));
#91210=CARTESIAN_POINT('',(161.9,7.4,48.35));
#91211=CARTESIAN_POINT('Origin',(162.,6.7,48.35));
#91212=CARTESIAN_POINT('Origin',(164.1,6.,48.5));
#91213=CARTESIAN_POINT('',(164.1,6.,48.5));
#91214=CARTESIAN_POINT('',(163.9,6.,48.5));
#91215=CARTESIAN_POINT('',(82.05,6.,48.5));
#91216=CARTESIAN_POINT('',(164.1,6.,48.35));
#91217=CARTESIAN_POINT('',(164.1,6.,48.5));
#91218=CARTESIAN_POINT('',(163.9,6.,48.35));
#91219=CARTESIAN_POINT('',(163.9,6.,48.35));
#91220=CARTESIAN_POINT('',(163.9,6.,48.5));
#91221=CARTESIAN_POINT('Origin',(164.1,7.4,48.5));
#91222=CARTESIAN_POINT('',(164.1,7.4,48.5));
#91223=CARTESIAN_POINT('',(164.1,7.7,48.5));
#91224=CARTESIAN_POINT('',(164.1,7.4,48.35));
#91225=CARTESIAN_POINT('',(164.1,7.4,48.5));
#91226=CARTESIAN_POINT('',(164.1,6.,48.35));
#91227=CARTESIAN_POINT('Origin',(163.9,7.4,48.5));
#91228=CARTESIAN_POINT('',(163.9,7.4,48.5));
#91229=CARTESIAN_POINT('',(81.95,7.4,48.5));
#91230=CARTESIAN_POINT('',(163.9,7.4,48.35));
#91231=CARTESIAN_POINT('',(163.9,7.4,48.5));
#91232=CARTESIAN_POINT('',(164.1,7.4,48.35));
#91233=CARTESIAN_POINT('Origin',(163.9,6.,48.5));
#91234=CARTESIAN_POINT('',(163.9,7.,48.5));
#91235=CARTESIAN_POINT('',(163.9,7.4,48.35));
#91236=CARTESIAN_POINT('Origin',(164.,6.7,48.35));
#91237=CARTESIAN_POINT('Origin',(166.1,6.,48.5));
#91238=CARTESIAN_POINT('',(166.1,6.,48.5));
#91239=CARTESIAN_POINT('',(165.9,6.,48.5));
#91240=CARTESIAN_POINT('',(83.05,6.,48.5));
#91241=CARTESIAN_POINT('',(166.1,6.,48.35));
#91242=CARTESIAN_POINT('',(166.1,6.,48.5));
#91243=CARTESIAN_POINT('',(165.9,6.,48.35));
#91244=CARTESIAN_POINT('',(165.9,6.,48.35));
#91245=CARTESIAN_POINT('',(165.9,6.,48.5));
#91246=CARTESIAN_POINT('Origin',(166.1,7.4,48.5));
#91247=CARTESIAN_POINT('',(166.1,7.4,48.5));
#91248=CARTESIAN_POINT('',(166.1,7.7,48.5));
#91249=CARTESIAN_POINT('',(166.1,7.4,48.35));
#91250=CARTESIAN_POINT('',(166.1,7.4,48.5));
#91251=CARTESIAN_POINT('',(166.1,6.,48.35));
#91252=CARTESIAN_POINT('Origin',(165.9,7.4,48.5));
#91253=CARTESIAN_POINT('',(165.9,7.4,48.5));
#91254=CARTESIAN_POINT('',(82.95,7.4,48.5));
#91255=CARTESIAN_POINT('',(165.9,7.4,48.35));
#91256=CARTESIAN_POINT('',(165.9,7.4,48.5));
#91257=CARTESIAN_POINT('',(166.1,7.4,48.35));
#91258=CARTESIAN_POINT('Origin',(165.9,6.,48.5));
#91259=CARTESIAN_POINT('',(165.9,7.,48.5));
#91260=CARTESIAN_POINT('',(165.9,7.4,48.35));
#91261=CARTESIAN_POINT('Origin',(166.,6.7,48.35));
#91262=CARTESIAN_POINT('Origin',(168.1,6.,48.5));
#91263=CARTESIAN_POINT('',(168.1,6.,48.5));
#91264=CARTESIAN_POINT('',(167.9,6.,48.5));
#91265=CARTESIAN_POINT('',(84.05,6.,48.5));
#91266=CARTESIAN_POINT('',(168.1,6.,48.35));
#91267=CARTESIAN_POINT('',(168.1,6.,48.5));
#91268=CARTESIAN_POINT('',(167.9,6.,48.35));
#91269=CARTESIAN_POINT('',(167.9,6.,48.35));
#91270=CARTESIAN_POINT('',(167.9,6.,48.5));
#91271=CARTESIAN_POINT('Origin',(168.1,7.4,48.5));
#91272=CARTESIAN_POINT('',(168.1,7.4,48.5));
#91273=CARTESIAN_POINT('',(168.1,7.7,48.5));
#91274=CARTESIAN_POINT('',(168.1,7.4,48.35));
#91275=CARTESIAN_POINT('',(168.1,7.4,48.5));
#91276=CARTESIAN_POINT('',(168.1,6.,48.35));
#91277=CARTESIAN_POINT('Origin',(167.9,7.4,48.5));
#91278=CARTESIAN_POINT('',(167.9,7.4,48.5));
#91279=CARTESIAN_POINT('',(83.95,7.4,48.5));
#91280=CARTESIAN_POINT('',(167.9,7.4,48.35));
#91281=CARTESIAN_POINT('',(167.9,7.4,48.5));
#91282=CARTESIAN_POINT('',(168.1,7.4,48.35));
#91283=CARTESIAN_POINT('Origin',(167.9,6.,48.5));
#91284=CARTESIAN_POINT('',(167.9,7.,48.5));
#91285=CARTESIAN_POINT('',(167.9,7.4,48.35));
#91286=CARTESIAN_POINT('Origin',(168.,6.7,48.35));
#91287=CARTESIAN_POINT('Origin',(170.1,4.4,48.5));
#91288=CARTESIAN_POINT('',(170.1,4.4,48.5));
#91289=CARTESIAN_POINT('',(169.9,4.4,48.5));
#91290=CARTESIAN_POINT('',(85.05,4.4,48.5));
#91291=CARTESIAN_POINT('',(170.1,4.4,48.35));
#91292=CARTESIAN_POINT('',(170.1,4.4,48.5));
#91293=CARTESIAN_POINT('',(169.9,4.4,48.35));
#91294=CARTESIAN_POINT('',(169.9,4.4,48.35));
#91295=CARTESIAN_POINT('',(169.9,4.4,48.5));
#91296=CARTESIAN_POINT('Origin',(170.1,7.4,48.5));
#91297=CARTESIAN_POINT('',(170.1,7.4,48.5));
#91298=CARTESIAN_POINT('',(170.1,7.7,48.5));
#91299=CARTESIAN_POINT('',(170.1,7.4,48.35));
#91300=CARTESIAN_POINT('',(170.1,7.4,48.5));
#91301=CARTESIAN_POINT('',(170.1,4.4,48.35));
#91302=CARTESIAN_POINT('Origin',(169.9,7.4,48.5));
#91303=CARTESIAN_POINT('',(169.9,7.4,48.5));
#91304=CARTESIAN_POINT('',(84.95,7.4,48.5));
#91305=CARTESIAN_POINT('',(169.9,7.4,48.35));
#91306=CARTESIAN_POINT('',(169.9,7.4,48.5));
#91307=CARTESIAN_POINT('',(170.1,7.4,48.35));
#91308=CARTESIAN_POINT('Origin',(169.9,4.4,48.5));
#91309=CARTESIAN_POINT('',(169.9,6.2,48.5));
#91310=CARTESIAN_POINT('',(169.9,7.4,48.35));
#91311=CARTESIAN_POINT('Origin',(170.,5.9,48.35));
#91312=CARTESIAN_POINT('Origin',(172.1,6.,48.5));
#91313=CARTESIAN_POINT('',(172.1,6.,48.5));
#91314=CARTESIAN_POINT('',(171.9,6.,48.5));
#91315=CARTESIAN_POINT('',(86.05,6.,48.5));
#91316=CARTESIAN_POINT('',(172.1,6.,48.35));
#91317=CARTESIAN_POINT('',(172.1,6.,48.5));
#91318=CARTESIAN_POINT('',(171.9,6.,48.35));
#91319=CARTESIAN_POINT('',(171.9,6.,48.35));
#91320=CARTESIAN_POINT('',(171.9,6.,48.5));
#91321=CARTESIAN_POINT('Origin',(172.1,7.4,48.5));
#91322=CARTESIAN_POINT('',(172.1,7.4,48.5));
#91323=CARTESIAN_POINT('',(172.1,7.7,48.5));
#91324=CARTESIAN_POINT('',(172.1,7.4,48.35));
#91325=CARTESIAN_POINT('',(172.1,7.4,48.5));
#91326=CARTESIAN_POINT('',(172.1,6.,48.35));
#91327=CARTESIAN_POINT('Origin',(171.9,7.4,48.5));
#91328=CARTESIAN_POINT('',(171.9,7.4,48.5));
#91329=CARTESIAN_POINT('',(85.95,7.4,48.5));
#91330=CARTESIAN_POINT('',(171.9,7.4,48.35));
#91331=CARTESIAN_POINT('',(171.9,7.4,48.5));
#91332=CARTESIAN_POINT('',(172.1,7.4,48.35));
#91333=CARTESIAN_POINT('Origin',(171.9,6.,48.5));
#91334=CARTESIAN_POINT('',(171.9,7.,48.5));
#91335=CARTESIAN_POINT('',(171.9,7.4,48.35));
#91336=CARTESIAN_POINT('Origin',(172.,6.7,48.35));
#91337=CARTESIAN_POINT('Origin',(174.1,6.,48.5));
#91338=CARTESIAN_POINT('',(174.1,6.,48.5));
#91339=CARTESIAN_POINT('',(173.9,6.,48.5));
#91340=CARTESIAN_POINT('',(87.05,6.,48.5));
#91341=CARTESIAN_POINT('',(174.1,6.,48.35));
#91342=CARTESIAN_POINT('',(174.1,6.,48.5));
#91343=CARTESIAN_POINT('',(173.9,6.,48.35));
#91344=CARTESIAN_POINT('',(173.9,6.,48.35));
#91345=CARTESIAN_POINT('',(173.9,6.,48.5));
#91346=CARTESIAN_POINT('Origin',(174.1,7.4,48.5));
#91347=CARTESIAN_POINT('',(174.1,7.4,48.5));
#91348=CARTESIAN_POINT('',(174.1,7.7,48.5));
#91349=CARTESIAN_POINT('',(174.1,7.4,48.35));
#91350=CARTESIAN_POINT('',(174.1,7.4,48.5));
#91351=CARTESIAN_POINT('',(174.1,6.,48.35));
#91352=CARTESIAN_POINT('Origin',(173.9,7.4,48.5));
#91353=CARTESIAN_POINT('',(173.9,7.4,48.5));
#91354=CARTESIAN_POINT('',(86.95,7.4,48.5));
#91355=CARTESIAN_POINT('',(173.9,7.4,48.35));
#91356=CARTESIAN_POINT('',(173.9,7.4,48.5));
#91357=CARTESIAN_POINT('',(174.1,7.4,48.35));
#91358=CARTESIAN_POINT('Origin',(173.9,6.,48.5));
#91359=CARTESIAN_POINT('',(173.9,7.,48.5));
#91360=CARTESIAN_POINT('',(173.9,7.4,48.35));
#91361=CARTESIAN_POINT('Origin',(174.,6.7,48.35));
#91362=CARTESIAN_POINT('Origin',(176.1,6.,48.5));
#91363=CARTESIAN_POINT('',(176.1,6.,48.5));
#91364=CARTESIAN_POINT('',(175.9,6.,48.5));
#91365=CARTESIAN_POINT('',(88.05,6.,48.5));
#91366=CARTESIAN_POINT('',(176.1,6.,48.35));
#91367=CARTESIAN_POINT('',(176.1,6.,48.5));
#91368=CARTESIAN_POINT('',(175.9,6.,48.35));
#91369=CARTESIAN_POINT('',(175.9,6.,48.35));
#91370=CARTESIAN_POINT('',(175.9,6.,48.5));
#91371=CARTESIAN_POINT('Origin',(176.1,7.4,48.5));
#91372=CARTESIAN_POINT('',(176.1,7.4,48.5));
#91373=CARTESIAN_POINT('',(176.1,7.7,48.5));
#91374=CARTESIAN_POINT('',(176.1,7.4,48.35));
#91375=CARTESIAN_POINT('',(176.1,7.4,48.5));
#91376=CARTESIAN_POINT('',(176.1,6.,48.35));
#91377=CARTESIAN_POINT('Origin',(175.9,7.4,48.5));
#91378=CARTESIAN_POINT('',(175.9,7.4,48.5));
#91379=CARTESIAN_POINT('',(87.95,7.4,48.5));
#91380=CARTESIAN_POINT('',(175.9,7.4,48.35));
#91381=CARTESIAN_POINT('',(175.9,7.4,48.5));
#91382=CARTESIAN_POINT('',(176.1,7.4,48.35));
#91383=CARTESIAN_POINT('Origin',(175.9,6.,48.5));
#91384=CARTESIAN_POINT('',(175.9,7.,48.5));
#91385=CARTESIAN_POINT('',(175.9,7.4,48.35));
#91386=CARTESIAN_POINT('Origin',(176.,6.7,48.35));
#91387=CARTESIAN_POINT('Origin',(178.1,6.,48.5));
#91388=CARTESIAN_POINT('',(178.1,6.,48.5));
#91389=CARTESIAN_POINT('',(177.9,6.,48.5));
#91390=CARTESIAN_POINT('',(89.05,6.,48.5));
#91391=CARTESIAN_POINT('',(178.1,6.,48.35));
#91392=CARTESIAN_POINT('',(178.1,6.,48.5));
#91393=CARTESIAN_POINT('',(177.9,6.,48.35));
#91394=CARTESIAN_POINT('',(177.9,6.,48.35));
#91395=CARTESIAN_POINT('',(177.9,6.,48.5));
#91396=CARTESIAN_POINT('Origin',(178.1,7.4,48.5));
#91397=CARTESIAN_POINT('',(178.1,7.4,48.5));
#91398=CARTESIAN_POINT('',(178.1,7.7,48.5));
#91399=CARTESIAN_POINT('',(178.1,7.4,48.35));
#91400=CARTESIAN_POINT('',(178.1,7.4,48.5));
#91401=CARTESIAN_POINT('',(178.1,6.,48.35));
#91402=CARTESIAN_POINT('Origin',(177.9,7.4,48.5));
#91403=CARTESIAN_POINT('',(177.9,7.4,48.5));
#91404=CARTESIAN_POINT('',(88.95,7.4,48.5));
#91405=CARTESIAN_POINT('',(177.9,7.4,48.35));
#91406=CARTESIAN_POINT('',(177.9,7.4,48.5));
#91407=CARTESIAN_POINT('',(178.1,7.4,48.35));
#91408=CARTESIAN_POINT('Origin',(177.9,6.,48.5));
#91409=CARTESIAN_POINT('',(177.9,7.,48.5));
#91410=CARTESIAN_POINT('',(177.9,7.4,48.35));
#91411=CARTESIAN_POINT('Origin',(178.,6.7,48.35));
#91412=CARTESIAN_POINT('Origin',(180.1,4.4,48.5));
#91413=CARTESIAN_POINT('',(180.1,4.4,48.5));
#91414=CARTESIAN_POINT('',(179.9,4.4,48.5));
#91415=CARTESIAN_POINT('',(90.05,4.4,48.5));
#91416=CARTESIAN_POINT('',(180.1,4.4,48.35));
#91417=CARTESIAN_POINT('',(180.1,4.4,48.5));
#91418=CARTESIAN_POINT('',(179.9,4.4,48.35));
#91419=CARTESIAN_POINT('',(179.9,4.4,48.35));
#91420=CARTESIAN_POINT('',(179.9,4.4,48.5));
#91421=CARTESIAN_POINT('Origin',(180.1,7.4,48.5));
#91422=CARTESIAN_POINT('',(180.1,7.4,48.5));
#91423=CARTESIAN_POINT('',(180.1,7.7,48.5));
#91424=CARTESIAN_POINT('',(180.1,7.4,48.35));
#91425=CARTESIAN_POINT('',(180.1,7.4,48.5));
#91426=CARTESIAN_POINT('',(180.1,4.4,48.35));
#91427=CARTESIAN_POINT('Origin',(179.9,7.4,48.5));
#91428=CARTESIAN_POINT('',(179.9,7.4,48.5));
#91429=CARTESIAN_POINT('',(89.95,7.4,48.5));
#91430=CARTESIAN_POINT('',(179.9,7.4,48.35));
#91431=CARTESIAN_POINT('',(179.9,7.4,48.5));
#91432=CARTESIAN_POINT('',(180.1,7.4,48.35));
#91433=CARTESIAN_POINT('Origin',(179.9,4.4,48.5));
#91434=CARTESIAN_POINT('',(179.9,6.2,48.5));
#91435=CARTESIAN_POINT('',(179.9,7.4,48.35));
#91436=CARTESIAN_POINT('Origin',(180.,5.9,48.35));
#91437=CARTESIAN_POINT('Origin',(182.1,6.,48.5));
#91438=CARTESIAN_POINT('',(182.1,6.,48.5));
#91439=CARTESIAN_POINT('',(181.9,6.,48.5));
#91440=CARTESIAN_POINT('',(91.05,6.,48.5));
#91441=CARTESIAN_POINT('',(182.1,6.,48.35));
#91442=CARTESIAN_POINT('',(182.1,6.,48.5));
#91443=CARTESIAN_POINT('',(181.9,6.,48.35));
#91444=CARTESIAN_POINT('',(181.9,6.,48.35));
#91445=CARTESIAN_POINT('',(181.9,6.,48.5));
#91446=CARTESIAN_POINT('Origin',(182.1,7.4,48.5));
#91447=CARTESIAN_POINT('',(182.1,7.4,48.5));
#91448=CARTESIAN_POINT('',(182.1,7.7,48.5));
#91449=CARTESIAN_POINT('',(182.1,7.4,48.35));
#91450=CARTESIAN_POINT('',(182.1,7.4,48.5));
#91451=CARTESIAN_POINT('',(182.1,6.,48.35));
#91452=CARTESIAN_POINT('Origin',(181.9,7.4,48.5));
#91453=CARTESIAN_POINT('',(181.9,7.4,48.5));
#91454=CARTESIAN_POINT('',(90.95,7.4,48.5));
#91455=CARTESIAN_POINT('',(181.9,7.4,48.35));
#91456=CARTESIAN_POINT('',(181.9,7.4,48.5));
#91457=CARTESIAN_POINT('',(182.1,7.4,48.35));
#91458=CARTESIAN_POINT('Origin',(181.9,6.,48.5));
#91459=CARTESIAN_POINT('',(181.9,7.,48.5));
#91460=CARTESIAN_POINT('',(181.9,7.4,48.35));
#91461=CARTESIAN_POINT('Origin',(182.,6.7,48.35));
#91462=CARTESIAN_POINT('Origin',(184.1,6.,48.5));
#91463=CARTESIAN_POINT('',(184.1,6.,48.5));
#91464=CARTESIAN_POINT('',(183.9,6.,48.5));
#91465=CARTESIAN_POINT('',(92.05,6.,48.5));
#91466=CARTESIAN_POINT('',(184.1,6.,48.35));
#91467=CARTESIAN_POINT('',(184.1,6.,48.5));
#91468=CARTESIAN_POINT('',(183.9,6.,48.35));
#91469=CARTESIAN_POINT('',(183.9,6.,48.35));
#91470=CARTESIAN_POINT('',(183.9,6.,48.5));
#91471=CARTESIAN_POINT('Origin',(184.1,7.4,48.5));
#91472=CARTESIAN_POINT('',(184.1,7.4,48.5));
#91473=CARTESIAN_POINT('',(184.1,7.7,48.5));
#91474=CARTESIAN_POINT('',(184.1,7.4,48.35));
#91475=CARTESIAN_POINT('',(184.1,7.4,48.5));
#91476=CARTESIAN_POINT('',(184.1,6.,48.35));
#91477=CARTESIAN_POINT('Origin',(183.9,7.4,48.5));
#91478=CARTESIAN_POINT('',(183.9,7.4,48.5));
#91479=CARTESIAN_POINT('',(91.95,7.4,48.5));
#91480=CARTESIAN_POINT('',(183.9,7.4,48.35));
#91481=CARTESIAN_POINT('',(183.9,7.4,48.5));
#91482=CARTESIAN_POINT('',(184.1,7.4,48.35));
#91483=CARTESIAN_POINT('Origin',(183.9,6.,48.5));
#91484=CARTESIAN_POINT('',(183.9,7.,48.5));
#91485=CARTESIAN_POINT('',(183.9,7.4,48.35));
#91486=CARTESIAN_POINT('Origin',(184.,6.7,48.35));
#91487=CARTESIAN_POINT('Origin',(186.1,6.,48.5));
#91488=CARTESIAN_POINT('',(186.1,6.,48.5));
#91489=CARTESIAN_POINT('',(185.9,6.,48.5));
#91490=CARTESIAN_POINT('',(93.05,6.,48.5));
#91491=CARTESIAN_POINT('',(186.1,6.,48.35));
#91492=CARTESIAN_POINT('',(186.1,6.,48.5));
#91493=CARTESIAN_POINT('',(185.9,6.,48.35));
#91494=CARTESIAN_POINT('',(185.9,6.,48.35));
#91495=CARTESIAN_POINT('',(185.9,6.,48.5));
#91496=CARTESIAN_POINT('Origin',(186.1,7.4,48.5));
#91497=CARTESIAN_POINT('',(186.1,7.4,48.5));
#91498=CARTESIAN_POINT('',(186.1,7.7,48.5));
#91499=CARTESIAN_POINT('',(186.1,7.4,48.35));
#91500=CARTESIAN_POINT('',(186.1,7.4,48.5));
#91501=CARTESIAN_POINT('',(186.1,6.,48.35));
#91502=CARTESIAN_POINT('Origin',(185.9,7.4,48.5));
#91503=CARTESIAN_POINT('',(185.9,7.4,48.5));
#91504=CARTESIAN_POINT('',(92.95,7.4,48.5));
#91505=CARTESIAN_POINT('',(185.9,7.4,48.35));
#91506=CARTESIAN_POINT('',(185.9,7.4,48.5));
#91507=CARTESIAN_POINT('',(186.1,7.4,48.35));
#91508=CARTESIAN_POINT('Origin',(185.9,6.,48.5));
#91509=CARTESIAN_POINT('',(185.9,7.,48.5));
#91510=CARTESIAN_POINT('',(185.9,7.4,48.35));
#91511=CARTESIAN_POINT('Origin',(186.,6.7,48.35));
#91512=CARTESIAN_POINT('Origin',(188.1,6.,48.5));
#91513=CARTESIAN_POINT('',(188.1,6.,48.5));
#91514=CARTESIAN_POINT('',(187.9,6.,48.5));
#91515=CARTESIAN_POINT('',(94.05,6.,48.5));
#91516=CARTESIAN_POINT('',(188.1,6.,48.35));
#91517=CARTESIAN_POINT('',(188.1,6.,48.5));
#91518=CARTESIAN_POINT('',(187.9,6.,48.35));
#91519=CARTESIAN_POINT('',(187.9,6.,48.35));
#91520=CARTESIAN_POINT('',(187.9,6.,48.5));
#91521=CARTESIAN_POINT('Origin',(188.1,7.4,48.5));
#91522=CARTESIAN_POINT('',(188.1,7.4,48.5));
#91523=CARTESIAN_POINT('',(188.1,7.7,48.5));
#91524=CARTESIAN_POINT('',(188.1,7.4,48.35));
#91525=CARTESIAN_POINT('',(188.1,7.4,48.5));
#91526=CARTESIAN_POINT('',(188.1,6.,48.35));
#91527=CARTESIAN_POINT('Origin',(187.9,7.4,48.5));
#91528=CARTESIAN_POINT('',(187.9,7.4,48.5));
#91529=CARTESIAN_POINT('',(93.95,7.4,48.5));
#91530=CARTESIAN_POINT('',(187.9,7.4,48.35));
#91531=CARTESIAN_POINT('',(187.9,7.4,48.5));
#91532=CARTESIAN_POINT('',(188.1,7.4,48.35));
#91533=CARTESIAN_POINT('Origin',(187.9,6.,48.5));
#91534=CARTESIAN_POINT('',(187.9,7.,48.5));
#91535=CARTESIAN_POINT('',(187.9,7.4,48.35));
#91536=CARTESIAN_POINT('Origin',(188.,6.7,48.35));
#91537=CARTESIAN_POINT('Origin',(190.1,4.4,48.5));
#91538=CARTESIAN_POINT('',(190.1,4.4,48.5));
#91539=CARTESIAN_POINT('',(189.9,4.4,48.5));
#91540=CARTESIAN_POINT('',(95.05,4.4,48.5));
#91541=CARTESIAN_POINT('',(190.1,4.4,48.35));
#91542=CARTESIAN_POINT('',(190.1,4.4,48.5));
#91543=CARTESIAN_POINT('',(189.9,4.4,48.35));
#91544=CARTESIAN_POINT('',(189.9,4.4,48.35));
#91545=CARTESIAN_POINT('',(189.9,4.4,48.5));
#91546=CARTESIAN_POINT('Origin',(190.1,7.4,48.5));
#91547=CARTESIAN_POINT('',(190.1,7.4,48.5));
#91548=CARTESIAN_POINT('',(190.1,7.7,48.5));
#91549=CARTESIAN_POINT('',(190.1,7.4,48.35));
#91550=CARTESIAN_POINT('',(190.1,7.4,48.5));
#91551=CARTESIAN_POINT('',(190.1,4.4,48.35));
#91552=CARTESIAN_POINT('Origin',(189.9,7.4,48.5));
#91553=CARTESIAN_POINT('',(189.9,7.4,48.5));
#91554=CARTESIAN_POINT('',(94.95,7.4,48.5));
#91555=CARTESIAN_POINT('',(189.9,7.4,48.35));
#91556=CARTESIAN_POINT('',(189.9,7.4,48.5));
#91557=CARTESIAN_POINT('',(190.1,7.4,48.35));
#91558=CARTESIAN_POINT('Origin',(189.9,4.4,48.5));
#91559=CARTESIAN_POINT('',(189.9,6.2,48.5));
#91560=CARTESIAN_POINT('',(189.9,7.4,48.35));
#91561=CARTESIAN_POINT('Origin',(190.,5.9,48.35));
#91562=CARTESIAN_POINT('Origin',(192.1,6.,48.5));
#91563=CARTESIAN_POINT('',(192.1,6.,48.5));
#91564=CARTESIAN_POINT('',(191.9,6.,48.5));
#91565=CARTESIAN_POINT('',(96.05,6.,48.5));
#91566=CARTESIAN_POINT('',(192.1,6.,48.35));
#91567=CARTESIAN_POINT('',(192.1,6.,48.5));
#91568=CARTESIAN_POINT('',(191.9,6.,48.35));
#91569=CARTESIAN_POINT('',(191.9,6.,48.35));
#91570=CARTESIAN_POINT('',(191.9,6.,48.5));
#91571=CARTESIAN_POINT('Origin',(192.1,7.4,48.5));
#91572=CARTESIAN_POINT('',(192.1,7.4,48.5));
#91573=CARTESIAN_POINT('',(192.1,7.7,48.5));
#91574=CARTESIAN_POINT('',(192.1,7.4,48.35));
#91575=CARTESIAN_POINT('',(192.1,7.4,48.5));
#91576=CARTESIAN_POINT('',(192.1,6.,48.35));
#91577=CARTESIAN_POINT('Origin',(191.9,7.4,48.5));
#91578=CARTESIAN_POINT('',(191.9,7.4,48.5));
#91579=CARTESIAN_POINT('',(95.95,7.4,48.5));
#91580=CARTESIAN_POINT('',(191.9,7.4,48.35));
#91581=CARTESIAN_POINT('',(191.9,7.4,48.5));
#91582=CARTESIAN_POINT('',(192.1,7.4,48.35));
#91583=CARTESIAN_POINT('Origin',(191.9,6.,48.5));
#91584=CARTESIAN_POINT('',(191.9,7.,48.5));
#91585=CARTESIAN_POINT('',(191.9,7.4,48.35));
#91586=CARTESIAN_POINT('Origin',(192.,6.7,48.35));
#91587=CARTESIAN_POINT('Origin',(194.1,6.,48.5));
#91588=CARTESIAN_POINT('',(194.1,6.,48.5));
#91589=CARTESIAN_POINT('',(193.9,6.,48.5));
#91590=CARTESIAN_POINT('',(97.05,6.,48.5));
#91591=CARTESIAN_POINT('',(194.1,6.,48.35));
#91592=CARTESIAN_POINT('',(194.1,6.,48.5));
#91593=CARTESIAN_POINT('',(193.9,6.,48.35));
#91594=CARTESIAN_POINT('',(193.9,6.,48.35));
#91595=CARTESIAN_POINT('',(193.9,6.,48.5));
#91596=CARTESIAN_POINT('Origin',(194.1,7.4,48.5));
#91597=CARTESIAN_POINT('',(194.1,7.4,48.5));
#91598=CARTESIAN_POINT('',(194.1,7.7,48.5));
#91599=CARTESIAN_POINT('',(194.1,7.4,48.35));
#91600=CARTESIAN_POINT('',(194.1,7.4,48.5));
#91601=CARTESIAN_POINT('',(194.1,6.,48.35));
#91602=CARTESIAN_POINT('Origin',(193.9,7.4,48.5));
#91603=CARTESIAN_POINT('',(193.9,7.4,48.5));
#91604=CARTESIAN_POINT('',(96.95,7.4,48.5));
#91605=CARTESIAN_POINT('',(193.9,7.4,48.35));
#91606=CARTESIAN_POINT('',(193.9,7.4,48.5));
#91607=CARTESIAN_POINT('',(194.1,7.4,48.35));
#91608=CARTESIAN_POINT('Origin',(193.9,6.,48.5));
#91609=CARTESIAN_POINT('',(193.9,7.,48.5));
#91610=CARTESIAN_POINT('',(193.9,7.4,48.35));
#91611=CARTESIAN_POINT('Origin',(194.,6.7,48.35));
#91612=CARTESIAN_POINT('Origin',(196.1,6.,48.5));
#91613=CARTESIAN_POINT('',(196.1,6.,48.5));
#91614=CARTESIAN_POINT('',(195.9,6.,48.5));
#91615=CARTESIAN_POINT('',(98.05,6.,48.5));
#91616=CARTESIAN_POINT('',(196.1,6.,48.35));
#91617=CARTESIAN_POINT('',(196.1,6.,48.5));
#91618=CARTESIAN_POINT('',(195.9,6.,48.35));
#91619=CARTESIAN_POINT('',(195.9,6.,48.35));
#91620=CARTESIAN_POINT('',(195.9,6.,48.5));
#91621=CARTESIAN_POINT('Origin',(196.1,7.4,48.5));
#91622=CARTESIAN_POINT('',(196.1,7.4,48.5));
#91623=CARTESIAN_POINT('',(196.1,7.7,48.5));
#91624=CARTESIAN_POINT('',(196.1,7.4,48.35));
#91625=CARTESIAN_POINT('',(196.1,7.4,48.5));
#91626=CARTESIAN_POINT('',(196.1,6.,48.35));
#91627=CARTESIAN_POINT('Origin',(195.9,7.4,48.5));
#91628=CARTESIAN_POINT('',(195.9,7.4,48.5));
#91629=CARTESIAN_POINT('',(97.95,7.4,48.5));
#91630=CARTESIAN_POINT('',(195.9,7.4,48.35));
#91631=CARTESIAN_POINT('',(195.9,7.4,48.5));
#91632=CARTESIAN_POINT('',(196.1,7.4,48.35));
#91633=CARTESIAN_POINT('Origin',(195.9,6.,48.5));
#91634=CARTESIAN_POINT('',(195.9,7.,48.5));
#91635=CARTESIAN_POINT('',(195.9,7.4,48.35));
#91636=CARTESIAN_POINT('Origin',(196.,6.7,48.35));
#91637=CARTESIAN_POINT('Origin',(198.1,6.,48.5));
#91638=CARTESIAN_POINT('',(198.1,6.,48.5));
#91639=CARTESIAN_POINT('',(197.9,6.,48.5));
#91640=CARTESIAN_POINT('',(99.05,6.,48.5));
#91641=CARTESIAN_POINT('',(198.1,6.,48.35));
#91642=CARTESIAN_POINT('',(198.1,6.,48.5));
#91643=CARTESIAN_POINT('',(197.9,6.,48.35));
#91644=CARTESIAN_POINT('',(197.9,6.,48.35));
#91645=CARTESIAN_POINT('',(197.9,6.,48.5));
#91646=CARTESIAN_POINT('Origin',(198.1,7.4,48.5));
#91647=CARTESIAN_POINT('',(198.1,7.4,48.5));
#91648=CARTESIAN_POINT('',(198.1,7.7,48.5));
#91649=CARTESIAN_POINT('',(198.1,7.4,48.35));
#91650=CARTESIAN_POINT('',(198.1,7.4,48.5));
#91651=CARTESIAN_POINT('',(198.1,6.,48.35));
#91652=CARTESIAN_POINT('Origin',(197.9,7.4,48.5));
#91653=CARTESIAN_POINT('',(197.9,7.4,48.5));
#91654=CARTESIAN_POINT('',(98.95,7.4,48.5));
#91655=CARTESIAN_POINT('',(197.9,7.4,48.35));
#91656=CARTESIAN_POINT('',(197.9,7.4,48.5));
#91657=CARTESIAN_POINT('',(198.1,7.4,48.35));
#91658=CARTESIAN_POINT('Origin',(197.9,6.,48.5));
#91659=CARTESIAN_POINT('',(197.9,7.,48.5));
#91660=CARTESIAN_POINT('',(197.9,7.4,48.35));
#91661=CARTESIAN_POINT('Origin',(198.,6.7,48.35));
#91662=CARTESIAN_POINT('Origin',(200.1,4.4,48.5));
#91663=CARTESIAN_POINT('',(200.1,4.4,48.5));
#91664=CARTESIAN_POINT('',(199.9,4.4,48.5));
#91665=CARTESIAN_POINT('',(100.05,4.4,48.5));
#91666=CARTESIAN_POINT('',(200.1,4.4,48.35));
#91667=CARTESIAN_POINT('',(200.1,4.4,48.5));
#91668=CARTESIAN_POINT('',(199.9,4.4,48.35));
#91669=CARTESIAN_POINT('',(199.9,4.4,48.35));
#91670=CARTESIAN_POINT('',(199.9,4.4,48.5));
#91671=CARTESIAN_POINT('Origin',(200.1,7.4,48.5));
#91672=CARTESIAN_POINT('',(200.1,7.4,48.5));
#91673=CARTESIAN_POINT('',(200.1,7.7,48.5));
#91674=CARTESIAN_POINT('',(200.1,7.4,48.35));
#91675=CARTESIAN_POINT('',(200.1,7.4,48.5));
#91676=CARTESIAN_POINT('',(200.1,4.4,48.35));
#91677=CARTESIAN_POINT('Origin',(199.9,7.4,48.5));
#91678=CARTESIAN_POINT('',(199.9,7.4,48.5));
#91679=CARTESIAN_POINT('',(99.95,7.4,48.5));
#91680=CARTESIAN_POINT('',(199.9,7.4,48.35));
#91681=CARTESIAN_POINT('',(199.9,7.4,48.5));
#91682=CARTESIAN_POINT('',(200.1,7.4,48.35));
#91683=CARTESIAN_POINT('Origin',(199.9,4.4,48.5));
#91684=CARTESIAN_POINT('',(199.9,6.2,48.5));
#91685=CARTESIAN_POINT('',(199.9,7.4,48.35));
#91686=CARTESIAN_POINT('Origin',(200.,5.9,48.35));
#91687=CARTESIAN_POINT('Origin',(220.,0.,20.5));
#91688=CARTESIAN_POINT('',(220.,0.3,20.5));
#91689=CARTESIAN_POINT('',(219.7,0.,20.5));
#91690=CARTESIAN_POINT('',(219.85,0.150000000000003,20.5));
#91691=CARTESIAN_POINT('',(220.,0.5,20.5));
#91692=CARTESIAN_POINT('',(220.,2.,20.5));
#91693=CARTESIAN_POINT('',(0.,0.5,20.5));
#91694=CARTESIAN_POINT('',(0.,0.5,20.5));
#91695=CARTESIAN_POINT('',(0.,0.3,20.5));
#91696=CARTESIAN_POINT('',(0.,2.,20.5));
#91697=CARTESIAN_POINT('',(0.3,0.,20.5));
#91698=CARTESIAN_POINT('',(55.15,-54.85,20.5));
#91699=CARTESIAN_POINT('',(110.,0.,20.5));
#91700=CARTESIAN_POINT('Origin',(0.,0.,36.5));
#91701=CARTESIAN_POINT('',(219.7,0.,36.5));
#91702=CARTESIAN_POINT('',(220.,0.3,36.5));
#91703=CARTESIAN_POINT('',(164.849999999998,-54.85,36.5));
#91704=CARTESIAN_POINT('',(0.3,0.,36.5));
#91705=CARTESIAN_POINT('',(0.,0.,36.5));
#91706=CARTESIAN_POINT('',(0.,0.3,36.5));
#91707=CARTESIAN_POINT('',(0.15,0.15,36.5));
#91708=CARTESIAN_POINT('',(0.,0.5,36.5));
#91709=CARTESIAN_POINT('',(0.,2.,36.5));
#91710=CARTESIAN_POINT('',(220.,0.5,36.5));
#91711=CARTESIAN_POINT('',(220.,0.5,36.5));
#91712=CARTESIAN_POINT('',(220.,2.,36.5));
#91713=CARTESIAN_POINT('Origin',(110.,0.5,28.5));
#91714=CARTESIAN_POINT('',(0.,0.5,28.5));
#91715=CARTESIAN_POINT('',(220.,0.5,28.5));
#91716=CARTESIAN_POINT('Origin',(0.,4.,28.5));
#91717=CARTESIAN_POINT('',(0.,0.3,47.8757359312881));
#91718=CARTESIAN_POINT('',(0.,0.3,38.5));
#91719=CARTESIAN_POINT('',(0.,0.624264068711927,48.2));
#91720=CARTESIAN_POINT('',(0.,-3.53786796564405,44.037867965644));
#91721=CARTESIAN_POINT('',(0.,7.37573593128807,48.2));
#91722=CARTESIAN_POINT('',(0.,6.,48.2));
#91723=CARTESIAN_POINT('',(0.,7.7,47.8757359312881));
#91724=CARTESIAN_POINT('',(0.,11.537867965644,44.037867965644));
#91725=CARTESIAN_POINT('',(0.,7.7,38.5132486540519));
#91726=CARTESIAN_POINT('',(0.,7.7,18.5));
#91727=CARTESIAN_POINT('',(0.,8.49641016151377,38.0534410329165));
#91728=CARTESIAN_POINT('Origin',(0.,8.,38.1132486540519));
#91729=CARTESIAN_POINT('',(0.,12.6535898384862,40.4535898384862));
#91730=CARTESIAN_POINT('',(0.,7.06867061317363,37.2291352203497));
#91731=CARTESIAN_POINT('',(0.,12.7,40.4267949192431));
#91732=CARTESIAN_POINT('',(0.,12.0081243060696,40.8262495373796));
#91733=CARTESIAN_POINT('',(0.,12.7,31.83));
#91734=CARTESIAN_POINT('',(0.,12.7,22.25));
#91735=CARTESIAN_POINT('',(0.,9.2,31.83));
#91736=CARTESIAN_POINT('',(0.,9.,31.83));
#91737=CARTESIAN_POINT('',(0.,9.2,25.17));
#91738=CARTESIAN_POINT('',(0.,9.2,30.015));
#91739=CARTESIAN_POINT('',(0.,12.7,25.17));
#91740=CARTESIAN_POINT('',(0.,6.75,25.17));
#91741=CARTESIAN_POINT('',(0.,12.7,16.5732050807569));
#91742=CARTESIAN_POINT('',(0.,12.7,22.25));
#91743=CARTESIAN_POINT('',(0.,12.6535898384862,16.5464101615138));
#91744=CARTESIAN_POINT('',(0.,12.0081243060695,16.1737504626203));
#91745=CARTESIAN_POINT('',(0.,8.49641016151378,18.9465589670835));
#91746=CARTESIAN_POINT('',(0.,4.56867061317363,21.2142404526244));
#91747=CARTESIAN_POINT('',(0.,7.7,18.4867513459481));
#91748=CARTESIAN_POINT('Origin',(0.,8.,18.8867513459481));
#91749=CARTESIAN_POINT('',(0.,7.7,9.12426406871192));
#91750=CARTESIAN_POINT('',(0.,7.7,18.5));
#91751=CARTESIAN_POINT('',(0.,7.37573593128808,8.8));
#91752=CARTESIAN_POINT('',(0.,11.537867965644,12.9621320343559));
#91753=CARTESIAN_POINT('',(0.,0.624264068711924,8.8));
#91754=CARTESIAN_POINT('',(0.,2.,8.8));
#91755=CARTESIAN_POINT('',(0.,0.300000000000004,9.12426406871192));
#91756=CARTESIAN_POINT('',(0.,-3.53786796564403,12.962132034356));
#91757=CARTESIAN_POINT('',(0.,0.3,38.5));
#91758=CARTESIAN_POINT('Origin',(219.85,0.15,38.5));
#91759=CARTESIAN_POINT('',(220.,0.300000000000002,47.8757359312881));
#91760=CARTESIAN_POINT('',(220.,0.3,38.5));
#91761=CARTESIAN_POINT('',(219.7,0.,48.));
#91762=CARTESIAN_POINT('',(220.,0.300000000000001,47.8757359312881));
#91763=CARTESIAN_POINT('',(219.7,0.,38.5));
#91764=CARTESIAN_POINT('Origin',(219.85,0.15,38.5));
#91765=CARTESIAN_POINT('',(219.7,0.,9.));
#91766=CARTESIAN_POINT('',(219.7,0.,38.5));
#91767=CARTESIAN_POINT('',(220.,0.3,9.12426406871192));
#91768=CARTESIAN_POINT('',(220.,0.3,9.12426406871192));
#91769=CARTESIAN_POINT('',(220.,0.3,38.5));
#91770=CARTESIAN_POINT('Origin',(0.15,0.15,38.5));
#91771=CARTESIAN_POINT('',(0.3,0.,48.));
#91772=CARTESIAN_POINT('',(0.3,0.,38.5));
#91773=CARTESIAN_POINT('',(0.,0.3,47.8757359312881));
#91774=CARTESIAN_POINT('Origin',(0.,0.,48.5));
#91775=CARTESIAN_POINT('',(0.,0.,48.));
#91776=CARTESIAN_POINT('',(107.65,0.,44.5));
#91777=CARTESIAN_POINT('Origin',(110.,0.,44.5));
#91778=CARTESIAN_POINT('',(32.65,0.,44.5));
#91779=CARTESIAN_POINT('Origin',(35.,0.,44.5));
#91780=CARTESIAN_POINT('',(182.65,0.,44.5));
#91781=CARTESIAN_POINT('Origin',(185.,0.,44.5));
#91782=CARTESIAN_POINT('Origin',(216.,4.5,46.));
#91783=CARTESIAN_POINT('',(215.,4.50000000000002,46.));
#91784=CARTESIAN_POINT('Origin',(216.,4.5,46.));
#91785=CARTESIAN_POINT('',(216.,3.89913938097244,46.));
#91786=CARTESIAN_POINT('',(215.,4.5,46.));
#91787=CARTESIAN_POINT('Origin',(4.,4.5,11.));
#91788=CARTESIAN_POINT('',(3.,4.5,11.));
#91789=CARTESIAN_POINT('Origin',(4.,4.5,11.));
#91790=CARTESIAN_POINT('',(4.,3.89913938097244,11.));
#91791=CARTESIAN_POINT('',(3.,4.5,11.));
#91792=CARTESIAN_POINT('Origin',(4.,8.,11.));
#91793=CARTESIAN_POINT('',(3.,8.,11.));
#91794=CARTESIAN_POINT('Origin',(4.,8.,11.));
#91795=CARTESIAN_POINT('',(3.,8.,11.));
#91796=CARTESIAN_POINT('Origin',(216.,8.,46.));
#91797=CARTESIAN_POINT('',(215.,8.,46.));
#91798=CARTESIAN_POINT('Origin',(216.,8.,46.));
#91799=CARTESIAN_POINT('',(215.,8.,46.));
#91800=CARTESIAN_POINT('Origin',(214.,9.4,28.5));
#91801=CARTESIAN_POINT('',(212.5,9.5,28.5));
#91802=CARTESIAN_POINT('Origin',(214.,9.5,28.5));
#91803=CARTESIAN_POINT('',(212.7,9.3,28.5));
#91804=CARTESIAN_POINT('',(212.6,9.4,28.5));
#91805=CARTESIAN_POINT('Origin',(214.,9.3,28.5));
#91806=CARTESIAN_POINT('Origin',(214.,9.5,28.5));
#91807=CARTESIAN_POINT('',(212.7,4.5,28.5));
#91808=CARTESIAN_POINT('',(212.7,9.5,28.5));
#91809=CARTESIAN_POINT('Origin',(214.,4.5,28.5));
#91810=CARTESIAN_POINT('Origin',(0.,9.5,31.53));
#91811=CARTESIAN_POINT('',(219.7,9.5,25.47));
#91812=CARTESIAN_POINT('',(219.7,9.5,31.53));
#91813=CARTESIAN_POINT('',(219.7,9.5,30.015));
#91814=CARTESIAN_POINT('',(0.3,9.5,25.47));
#91815=CARTESIAN_POINT('',(0.,9.5,25.47));
#91816=CARTESIAN_POINT('',(0.3,9.5,31.53));
#91817=CARTESIAN_POINT('',(0.3,9.5,30.015));
#91818=CARTESIAN_POINT('',(0.,9.5,31.53));
#91819=CARTESIAN_POINT('',(4.5,9.5,28.5));
#91820=CARTESIAN_POINT('Origin',(6.,9.5,28.5));
#91821=CARTESIAN_POINT('Origin',(214.,4.5,28.5));
#91822=CARTESIAN_POINT('',(214.,3.71888119526417,28.5));
#91823=CARTESIAN_POINT('',(212.7,4.5,28.5));
#91824=CARTESIAN_POINT('Origin',(6.,9.4,28.5));
#91825=CARTESIAN_POINT('',(4.7,9.3,28.5));
#91826=CARTESIAN_POINT('',(4.6,9.4,28.5));
#91827=CARTESIAN_POINT('Origin',(6.,9.3,28.5));
#91828=CARTESIAN_POINT('Origin',(6.,9.5,28.5));
#91829=CARTESIAN_POINT('',(4.7,4.5,28.5));
#91830=CARTESIAN_POINT('',(4.7,9.5,28.5));
#91831=CARTESIAN_POINT('Origin',(6.,4.5,28.5));
#91832=CARTESIAN_POINT('Origin',(6.,4.5,28.5));
#91833=CARTESIAN_POINT('',(6.,3.71888119526417,28.5));
#91834=CARTESIAN_POINT('',(4.7,4.5,28.5));
#91835=CARTESIAN_POINT('Origin',(185.,8.,12.5));
#91836=CARTESIAN_POINT('',(182.,8.,12.5));
#91837=CARTESIAN_POINT('Origin',(185.,8.,12.5));
#91838=CARTESIAN_POINT('',(182.,4.8,12.5));
#91839=CARTESIAN_POINT('',(182.,8.,12.5));
#91840=CARTESIAN_POINT('Origin',(185.,4.8,12.5));
#91841=CARTESIAN_POINT('Origin',(185.,4.8,12.5));
#91842=CARTESIAN_POINT('',(182.95,4.8,12.5));
#91843=CARTESIAN_POINT('Origin',(185.,4.8,12.5));
#91844=CARTESIAN_POINT('Origin',(35.,8.,12.5));
#91845=CARTESIAN_POINT('',(32.,8.,12.5));
#91846=CARTESIAN_POINT('Origin',(35.,8.,12.5));
#91847=CARTESIAN_POINT('',(32.,4.8,12.5));
#91848=CARTESIAN_POINT('',(32.,8.,12.5));
#91849=CARTESIAN_POINT('Origin',(35.,4.8,12.5));
#91850=CARTESIAN_POINT('Origin',(35.,4.8,12.5));
#91851=CARTESIAN_POINT('',(32.95,4.8,12.5));
#91852=CARTESIAN_POINT('Origin',(35.,4.8,12.5));
#91853=CARTESIAN_POINT('Origin',(35.,8.,44.5));
#91854=CARTESIAN_POINT('',(32.,8.,44.5));
#91855=CARTESIAN_POINT('Origin',(35.,8.,44.5));
#91856=CARTESIAN_POINT('',(32.,4.8,44.5));
#91857=CARTESIAN_POINT('',(32.,8.,44.5));
#91858=CARTESIAN_POINT('Origin',(35.,4.8,44.5));
#91859=CARTESIAN_POINT('Origin',(35.,4.8,44.5));
#91860=CARTESIAN_POINT('',(32.95,4.8,44.5));
#91861=CARTESIAN_POINT('Origin',(35.,4.8,44.5));
#91862=CARTESIAN_POINT('Origin',(110.,8.,12.5));
#91863=CARTESIAN_POINT('',(107.,8.,12.5));
#91864=CARTESIAN_POINT('Origin',(110.,8.,12.5));
#91865=CARTESIAN_POINT('',(107.,4.8,12.5));
#91866=CARTESIAN_POINT('',(107.,8.,12.5));
#91867=CARTESIAN_POINT('Origin',(110.,4.8,12.5));
#91868=CARTESIAN_POINT('Origin',(110.,4.8,12.5));
#91869=CARTESIAN_POINT('',(107.95,4.8,12.5));
#91870=CARTESIAN_POINT('Origin',(110.,4.8,12.5));
#91871=CARTESIAN_POINT('Origin',(110.,8.,44.5));
#91872=CARTESIAN_POINT('',(107.,8.,44.5));
#91873=CARTESIAN_POINT('Origin',(110.,8.,44.5));
#91874=CARTESIAN_POINT('',(107.,4.8,44.5));
#91875=CARTESIAN_POINT('',(107.,8.,44.5));
#91876=CARTESIAN_POINT('Origin',(110.,4.8,44.5));
#91877=CARTESIAN_POINT('Origin',(110.,4.8,44.5));
#91878=CARTESIAN_POINT('',(107.95,4.8,44.5));
#91879=CARTESIAN_POINT('Origin',(110.,4.8,44.5));
#91880=CARTESIAN_POINT('Origin',(185.,8.,44.5));
#91881=CARTESIAN_POINT('',(182.,8.,44.5));
#91882=CARTESIAN_POINT('Origin',(185.,8.,44.5));
#91883=CARTESIAN_POINT('',(182.,4.8,44.5));
#91884=CARTESIAN_POINT('',(182.,8.,44.5));
#91885=CARTESIAN_POINT('Origin',(185.,4.8,44.5));
#91886=CARTESIAN_POINT('Origin',(185.,4.8,44.5));
#91887=CARTESIAN_POINT('',(182.95,4.8,44.5));
#91888=CARTESIAN_POINT('Origin',(185.,4.8,44.5));
#91889=CARTESIAN_POINT('Origin',(185.,0.15,44.5));
#91890=CARTESIAN_POINT('',(182.95,0.3,44.5));
#91891=CARTESIAN_POINT('',(182.8,0.15,44.5));
#91892=CARTESIAN_POINT('Origin',(185.,0.3,44.5));
#91893=CARTESIAN_POINT('Origin',(0.,0.,48.5));
#91894=CARTESIAN_POINT('',(0.3,0.,9.));
#91895=CARTESIAN_POINT('',(0.3,0.,38.5));
#91896=CARTESIAN_POINT('',(0.,0.,9.));
#91897=CARTESIAN_POINT('',(182.65,0.,12.5));
#91898=CARTESIAN_POINT('Origin',(185.,0.,12.5));
#91899=CARTESIAN_POINT('',(32.65,0.,12.5));
#91900=CARTESIAN_POINT('Origin',(35.,0.,12.5));
#91901=CARTESIAN_POINT('',(107.65,0.,12.5));
#91902=CARTESIAN_POINT('Origin',(110.,0.,12.5));
#91903=CARTESIAN_POINT('Origin',(185.,0.,44.5));
#91904=CARTESIAN_POINT('',(182.95,0.,44.5));
#91905=CARTESIAN_POINT('Origin',(110.,0.15,44.5));
#91906=CARTESIAN_POINT('',(107.95,0.3,44.5));
#91907=CARTESIAN_POINT('',(107.8,0.15,44.5));
#91908=CARTESIAN_POINT('Origin',(110.,0.3,44.5));
#91909=CARTESIAN_POINT('Origin',(110.,0.,44.5));
#91910=CARTESIAN_POINT('',(107.95,0.,44.5));
#91911=CARTESIAN_POINT('Origin',(110.,0.15,12.5));
#91912=CARTESIAN_POINT('',(107.95,0.3,12.5));
#91913=CARTESIAN_POINT('',(107.8,0.15,12.5));
#91914=CARTESIAN_POINT('Origin',(110.,0.3,12.5));
#91915=CARTESIAN_POINT('Origin',(110.,0.,12.5));
#91916=CARTESIAN_POINT('',(107.95,0.,12.5));
#91917=CARTESIAN_POINT('Origin',(35.,0.15,44.5));
#91918=CARTESIAN_POINT('',(32.95,0.3,44.5));
#91919=CARTESIAN_POINT('',(32.8,0.15,44.5));
#91920=CARTESIAN_POINT('Origin',(35.,0.3,44.5));
#91921=CARTESIAN_POINT('Origin',(35.,0.,44.5));
#91922=CARTESIAN_POINT('',(32.95,0.,44.5));
#91923=CARTESIAN_POINT('Origin',(35.,0.15,12.5));
#91924=CARTESIAN_POINT('',(32.95,0.3,12.5));
#91925=CARTESIAN_POINT('',(32.8,0.15,12.5));
#91926=CARTESIAN_POINT('Origin',(35.,0.3,12.5));
#91927=CARTESIAN_POINT('Origin',(35.,0.,12.5));
#91928=CARTESIAN_POINT('',(32.95,0.,12.5));
#91929=CARTESIAN_POINT('Origin',(185.,0.15,12.5));
#91930=CARTESIAN_POINT('',(182.95,0.3,12.5));
#91931=CARTESIAN_POINT('',(182.8,0.15,12.5));
#91932=CARTESIAN_POINT('Origin',(185.,0.3,12.5));
#91933=CARTESIAN_POINT('Origin',(185.,0.,12.5));
#91934=CARTESIAN_POINT('',(182.95,0.,12.5));
#91935=CARTESIAN_POINT('Origin',(219.85,6.99367061317363,37.3590390309174));
#91936=CARTESIAN_POINT('',(219.7,12.6535898384862,40.8));
#91937=CARTESIAN_POINT('',(219.7,8.43301270189222,38.3632486540519));
#91938=CARTESIAN_POINT('',(219.7,6.91867061317363,37.488942841485));
#91939=CARTESIAN_POINT('',(220.,8.49641016151377,38.0534410329165));
#91940=CARTESIAN_POINT('Origin',(219.7,8.,38.1132486540519));
#91941=CARTESIAN_POINT('',(220.,12.6535898384862,40.4535898384862));
#91942=CARTESIAN_POINT('',(220.,7.06867061317363,37.2291352203497));
#91943=CARTESIAN_POINT('',(220.,12.6535898384862,40.4535898384862));
#91944=CARTESIAN_POINT('Origin',(219.85,12.0831243060696,40.9561533479473));
#91945=CARTESIAN_POINT('',(220.,12.7,40.4267949192431));
#91946=CARTESIAN_POINT('',(220.,12.0081243060696,40.8262495373796));
#91947=CARTESIAN_POINT('',(219.7,13.,40.6));
#91948=CARTESIAN_POINT('',(220.,12.7,40.4267949192431));
#91949=CARTESIAN_POINT('',(219.7,12.1581243060696,41.086057158515));
#91950=CARTESIAN_POINT('Origin',(219.85,12.85,22.25));
#91951=CARTESIAN_POINT('',(220.,12.7,31.83));
#91952=CARTESIAN_POINT('',(220.,12.7,22.25));
#91953=CARTESIAN_POINT('',(219.7,13.,31.53));
#91954=CARTESIAN_POINT('',(220.,12.7,31.83));
#91955=CARTESIAN_POINT('',(219.7,13.,22.25));
#91956=CARTESIAN_POINT('Origin',(219.85,6.75,25.32));
#91957=CARTESIAN_POINT('',(220.,9.2,25.17));
#91958=CARTESIAN_POINT('',(220.,12.7,25.17));
#91959=CARTESIAN_POINT('',(220.,6.75,25.17));
#91960=CARTESIAN_POINT('',(219.7,13.,25.47));
#91961=CARTESIAN_POINT('',(220.,12.7,25.17));
#91962=CARTESIAN_POINT('',(219.7,6.75,25.47));
#91963=CARTESIAN_POINT('',(219.7,9.5,25.47));
#91964=CARTESIAN_POINT('Origin',(219.85,12.85,22.25));
#91965=CARTESIAN_POINT('',(220.,12.7,16.5732050807569));
#91966=CARTESIAN_POINT('',(220.,12.7,22.25));
#91967=CARTESIAN_POINT('',(219.7,13.,16.4));
#91968=CARTESIAN_POINT('',(220.,12.7,16.5732050807569));
#91969=CARTESIAN_POINT('',(219.7,13.,22.25));
#91970=CARTESIAN_POINT('Origin',(219.85,12.0831243060695,16.0438466520527));
#91971=CARTESIAN_POINT('',(220.,12.6535898384862,16.5464101615138));
#91972=CARTESIAN_POINT('',(220.,12.0081243060695,16.1737504626203));
#91973=CARTESIAN_POINT('',(219.7,12.6535898384862,16.2));
#91974=CARTESIAN_POINT('',(220.,12.6535898384862,16.5464101615138));
#91975=CARTESIAN_POINT('',(219.7,12.1581243060695,15.913942841485));
#91976=CARTESIAN_POINT('Origin',(219.85,4.49367061317363,21.0843366420567));
#91977=CARTESIAN_POINT('',(220.,8.49641016151378,18.9465589670835));
#91978=CARTESIAN_POINT('',(220.,4.56867061317363,21.2142404526244));
#91979=CARTESIAN_POINT('',(219.7,8.43301270189222,18.6367513459481));
#91980=CARTESIAN_POINT('Origin',(219.7,8.,18.8867513459481));
#91981=CARTESIAN_POINT('',(219.7,4.41867061317363,20.954432831489));
#91982=CARTESIAN_POINT('Origin',(219.85,9.35,30.015));
#91983=CARTESIAN_POINT('',(220.,9.2,31.83));
#91984=CARTESIAN_POINT('',(220.,9.2,30.015));
#91985=CARTESIAN_POINT('',(219.7,9.5,31.53));
#91986=CARTESIAN_POINT('Origin',(219.85,9.,31.68));
#91987=CARTESIAN_POINT('',(220.,9.,31.83));
#91988=CARTESIAN_POINT('',(219.7,9.,31.53));
#91989=CARTESIAN_POINT('Origin',(0.,8.,38.1132486540519));
#91990=CARTESIAN_POINT('',(0.3,8.43301270189222,38.3632486540519));
#91991=CARTESIAN_POINT('',(0.,8.43301270189222,38.3632486540519));
#91992=CARTESIAN_POINT('Origin',(0.300000000000001,8.,38.1132486540519));
#91993=CARTESIAN_POINT('',(0.3,8.,38.6132486540519));
#91994=CARTESIAN_POINT('Origin',(0.3,8.,38.1132486540519));
#91995=CARTESIAN_POINT('',(219.7,8.,38.6132486540519));
#91996=CARTESIAN_POINT('',(0.,8.,38.6132486540519));
#91997=CARTESIAN_POINT('',(220.,7.7,38.5132486540519));
#91998=CARTESIAN_POINT('Origin',(219.7,8.,38.1132486540519));
#91999=CARTESIAN_POINT('Origin',(220.,8.,38.1132486540519));
#92000=CARTESIAN_POINT('Origin',(0.,13.,41.));
#92001=CARTESIAN_POINT('',(0.3,12.6535898384862,40.8));
#92002=CARTESIAN_POINT('',(0.,12.6535898384862,40.8));
#92003=CARTESIAN_POINT('',(0.3,6.91867061317363,37.488942841485));
#92004=CARTESIAN_POINT('Origin',(0.,12.8267949192431,40.7));
#92005=CARTESIAN_POINT('',(0.3,13.,40.6));
#92006=CARTESIAN_POINT('',(0.,13.,40.6));
#92007=CARTESIAN_POINT('',(0.3,12.1581243060696,41.086057158515));
#92008=CARTESIAN_POINT('Origin',(0.,13.,16.));
#92009=CARTESIAN_POINT('',(0.3,13.,31.53));
#92010=CARTESIAN_POINT('',(0.,13.,31.53));
#92011=CARTESIAN_POINT('',(0.3,13.,22.25));
#92012=CARTESIAN_POINT('Origin',(0.,14.,31.53));
#92013=CARTESIAN_POINT('',(0.3,9.,31.53));
#92014=CARTESIAN_POINT('Origin',(0.,9.5,25.47));
#92015=CARTESIAN_POINT('',(0.3,13.,25.47));
#92016=CARTESIAN_POINT('',(0.,13.,25.47));
#92017=CARTESIAN_POINT('',(0.3,6.75,25.47));
#92018=CARTESIAN_POINT('Origin',(219.85,7.85,18.5));
#92019=CARTESIAN_POINT('',(219.7,8.,9.));
#92020=CARTESIAN_POINT('',(219.7,8.,18.3867513459481));
#92021=CARTESIAN_POINT('',(219.7,8.,18.5));
#92022=CARTESIAN_POINT('',(220.,7.7,18.4867513459481));
#92023=CARTESIAN_POINT('Origin',(219.7,8.,18.8867513459481));
#92024=CARTESIAN_POINT('',(220.,7.7,9.12426406871192));
#92025=CARTESIAN_POINT('',(220.,7.7,18.5));
#92026=CARTESIAN_POINT('',(220.,7.7,9.12426406871192));
#92027=CARTESIAN_POINT('Origin',(219.85,11.643933982822,12.856066017178));
#92028=CARTESIAN_POINT('',(220.,7.37573593128808,8.8));
#92029=CARTESIAN_POINT('',(220.,11.537867965644,12.9621320343559));
#92030=CARTESIAN_POINT('',(219.7,7.5,8.5));
#92031=CARTESIAN_POINT('',(220.,7.37573593128808,8.8));
#92032=CARTESIAN_POINT('',(219.7,11.75,12.75));
#92033=CARTESIAN_POINT('Origin',(219.85,2.,8.65));
#92034=CARTESIAN_POINT('',(220.,0.624264068711924,8.8));
#92035=CARTESIAN_POINT('',(220.,2.,8.8));
#92036=CARTESIAN_POINT('',(219.7,0.5,8.5));
#92037=CARTESIAN_POINT('',(220.,0.624264068711924,8.8));
#92038=CARTESIAN_POINT('',(219.7,2.,8.5));
#92039=CARTESIAN_POINT('Origin',(219.85,-3.64393398282202,12.856066017178));
#92040=CARTESIAN_POINT('',(220.,-3.53786796564403,12.962132034356));
#92041=CARTESIAN_POINT('',(219.7,-3.75,12.75));
#92042=CARTESIAN_POINT('Origin',(219.85,-3.64393398282203,44.1439339828219));
#92043=CARTESIAN_POINT('',(220.,0.624264068711926,48.2));
#92044=CARTESIAN_POINT('',(220.,-3.53786796564405,44.037867965644));
#92045=CARTESIAN_POINT('',(219.7,0.5,48.5));
#92046=CARTESIAN_POINT('',(220.,0.624264068711926,48.2));
#92047=CARTESIAN_POINT('',(219.7,-3.75000000000001,44.2499999999999));
#92048=CARTESIAN_POINT('Origin',(219.85,6.,48.35));
#92049=CARTESIAN_POINT('',(220.,7.37573593128807,48.2));
#92050=CARTESIAN_POINT('',(220.,6.,48.2));
#92051=CARTESIAN_POINT('',(219.7,7.5,48.5));
#92052=CARTESIAN_POINT('',(220.,7.37573593128807,48.2));
#92053=CARTESIAN_POINT('',(219.7,6.,48.5));
#92054=CARTESIAN_POINT('Origin',(219.85,11.643933982822,44.143933982822));
#92055=CARTESIAN_POINT('',(220.,7.7,47.8757359312881));
#92056=CARTESIAN_POINT('',(220.,11.537867965644,44.037867965644));
#92057=CARTESIAN_POINT('',(219.7,8.,48.));
#92058=CARTESIAN_POINT('',(220.,7.7,47.8757359312881));
#92059=CARTESIAN_POINT('',(219.7,11.75,44.25));
#92060=CARTESIAN_POINT('Origin',(219.85,7.85,18.5));
#92061=CARTESIAN_POINT('',(220.,7.7,18.5));
#92062=CARTESIAN_POINT('',(219.7,8.,18.5));
#92063=CARTESIAN_POINT('Origin',(0.,8.,8.5));
#92064=CARTESIAN_POINT('',(0.3,8.,9.));
#92065=CARTESIAN_POINT('',(0.,8.,9.));
#92066=CARTESIAN_POINT('',(0.3,8.,18.3867513459481));
#92067=CARTESIAN_POINT('',(0.3,8.,18.5));
#92068=CARTESIAN_POINT('',(0.,8.,18.3867513459481));
#92069=CARTESIAN_POINT('Origin',(0.,7.75,8.75));
#92070=CARTESIAN_POINT('',(0.3,7.5,8.5));
#92071=CARTESIAN_POINT('',(0.,7.5,8.5));
#92072=CARTESIAN_POINT('',(0.3,11.75,12.75));
#92073=CARTESIAN_POINT('Origin',(0.,0.,8.5));
#92074=CARTESIAN_POINT('',(0.3,0.5,8.5));
#92075=CARTESIAN_POINT('',(0.,0.5,8.5));
#92076=CARTESIAN_POINT('',(0.3,2.,8.5));
#92077=CARTESIAN_POINT('Origin',(0.,0.25,8.75));
#92078=CARTESIAN_POINT('',(0.3,-3.75,12.75));
#92079=CARTESIAN_POINT('Origin',(0.,0.25,48.25));
#92080=CARTESIAN_POINT('',(0.3,0.5,48.5));
#92081=CARTESIAN_POINT('',(0.,0.5,48.5));
#92082=CARTESIAN_POINT('',(0.3,-3.75000000000001,44.2499999999999));
#92083=CARTESIAN_POINT('Origin',(0.,8.,48.5));
#92084=CARTESIAN_POINT('',(0.3,7.5,48.5));
#92085=CARTESIAN_POINT('',(0.,7.5,48.5));
#92086=CARTESIAN_POINT('',(0.3,6.,48.5));
#92087=CARTESIAN_POINT('Origin',(0.,7.75,48.25));
#92088=CARTESIAN_POINT('',(0.3,8.,48.));
#92089=CARTESIAN_POINT('',(0.,8.,48.));
#92090=CARTESIAN_POINT('',(0.3,11.75,44.25));
#92091=CARTESIAN_POINT('Origin',(0.,8.,8.5));
#92092=CARTESIAN_POINT('',(0.3,8.,18.5));
#92093=CARTESIAN_POINT('Origin',(0.15,4.49367061317363,21.0843366420567));
#92094=CARTESIAN_POINT('',(0.3,12.6535898384862,16.2));
#92095=CARTESIAN_POINT('',(0.3,8.43301270189222,18.6367513459481));
#92096=CARTESIAN_POINT('',(0.3,4.41867061317363,20.954432831489));
#92097=CARTESIAN_POINT('Origin',(0.300000000000001,8.,18.8867513459481));
#92098=CARTESIAN_POINT('',(0.,12.6535898384862,16.5464101615138));
#92099=CARTESIAN_POINT('Origin',(0.15,12.0831243060695,16.0438466520527));
#92100=CARTESIAN_POINT('',(0.3,13.,16.4));
#92101=CARTESIAN_POINT('',(0.,12.7,16.5732050807569));
#92102=CARTESIAN_POINT('',(0.3,12.1581243060695,15.913942841485));
#92103=CARTESIAN_POINT('Origin',(0.15,12.85,22.25));
#92104=CARTESIAN_POINT('',(0.,12.7,25.17));
#92105=CARTESIAN_POINT('',(0.3,13.,22.25));
#92106=CARTESIAN_POINT('Origin',(0.15,6.75,25.32));
#92107=CARTESIAN_POINT('',(0.,9.2,25.17));
#92108=CARTESIAN_POINT('Origin',(0.15,9.35,30.015));
#92109=CARTESIAN_POINT('',(0.,9.2,31.83));
#92110=CARTESIAN_POINT('Origin',(0.15,9.,31.68));
#92111=CARTESIAN_POINT('',(0.,12.7,31.83));
#92112=CARTESIAN_POINT('Origin',(0.15,12.85,22.25));
#92113=CARTESIAN_POINT('',(0.,12.7,40.4267949192431));
#92114=CARTESIAN_POINT('Origin',(0.15,12.0831243060696,40.9561533479473));
#92115=CARTESIAN_POINT('',(0.,12.6535898384862,40.4535898384862));
#92116=CARTESIAN_POINT('Origin',(0.15,6.99367061317363,37.3590390309174));
#92117=CARTESIAN_POINT('Origin',(0.15,7.85,18.5));
#92118=CARTESIAN_POINT('',(0.,7.7,47.8757359312881));
#92119=CARTESIAN_POINT('Origin',(0.15,11.643933982822,44.143933982822));
#92120=CARTESIAN_POINT('',(0.,7.37573593128807,48.2));
#92121=CARTESIAN_POINT('Origin',(0.15,6.,48.35));
#92122=CARTESIAN_POINT('',(0.,0.624264068711926,48.2));
#92123=CARTESIAN_POINT('Origin',(0.15,-3.64393398282203,44.1439339828219));
#92124=CARTESIAN_POINT('Origin',(0.15,0.15,38.5));
#92125=CARTESIAN_POINT('',(0.,0.300000000000004,9.12426406871192));
#92126=CARTESIAN_POINT('Origin',(0.15,-3.64393398282202,12.856066017178));
#92127=CARTESIAN_POINT('',(0.,0.624264068711924,8.8));
#92128=CARTESIAN_POINT('Origin',(0.15,2.,8.65));
#92129=CARTESIAN_POINT('',(0.,7.37573593128808,8.8));
#92130=CARTESIAN_POINT('Origin',(0.15,11.643933982822,12.856066017178));
#92131=CARTESIAN_POINT('',(0.,7.7,9.12426406871192));
#92132=CARTESIAN_POINT('Origin',(0.15,7.85,18.5));
#92133=CARTESIAN_POINT('Origin',(0.3,8.,18.8867513459481));
#92134=CARTESIAN_POINT('Origin',(220.,4.,28.5));
#92135=CARTESIAN_POINT('Origin',(220.,8.,18.8867513459481));
#92136=CARTESIAN_POINT('Origin',(0.,13.,16.));
#92137=CARTESIAN_POINT('',(0.,13.,16.4));
#92138=CARTESIAN_POINT('Origin',(0.,8.,18.8867513459481));
#92139=CARTESIAN_POINT('',(0.,8.43301270189222,18.6367513459481));
#92140=CARTESIAN_POINT('Origin',(0.,12.8267949192431,16.3));
#92141=CARTESIAN_POINT('',(0.,12.6535898384862,16.2));
#92142=CARTESIAN_POINT('Origin',(0.,8.,18.8867513459481));
#92143=CARTESIAN_POINT('',(0.,0.,0.));
#92144=CARTESIAN_POINT('Origin',(110.,10.75,8.65));
#92145=CARTESIAN_POINT('',(107.65,10.75,8.5));
#92146=CARTESIAN_POINT('',(107.95,10.75,8.8));
#92147=CARTESIAN_POINT('',(107.8,10.75,8.65));
#92148=CARTESIAN_POINT('',(111.568438714136,9.,8.5));
#92149=CARTESIAN_POINT('Origin',(110.,10.75,8.5));
#92150=CARTESIAN_POINT('',(110.,8.7,8.8));
#92151=CARTESIAN_POINT('Ctrl Pts',(111.568438714136,9.,8.5));
#92152=CARTESIAN_POINT('Ctrl Pts',(110.784219357068,8.7,8.8));
#92153=CARTESIAN_POINT('Ctrl Pts',(110.,8.7,8.8));
#92154=CARTESIAN_POINT('Origin',(110.,10.75,8.8));
#92155=CARTESIAN_POINT('Origin',(118.5,10.2,48.425));
#92156=CARTESIAN_POINT('',(118.5,9.,48.5));
#92157=CARTESIAN_POINT('',(117.3,10.2,48.5));
#92158=CARTESIAN_POINT('Origin',(118.5,10.2,48.5));
#92159=CARTESIAN_POINT('',(117.45,10.2,48.35));
#92160=CARTESIAN_POINT('',(117.375,10.2,48.425));
#92161=CARTESIAN_POINT('Origin',(118.5,10.2,48.35));
#92162=CARTESIAN_POINT('Origin',(118.5,10.2,48.5));
#92163=CARTESIAN_POINT('Origin',(90.,28.,48.5));
#92164=CARTESIAN_POINT('',(90.5,9.,48.5));
#92165=CARTESIAN_POINT('',(90.5,27.5,48.5));
#92166=CARTESIAN_POINT('',(90.5,23.125,48.5));
#92167=CARTESIAN_POINT('',(101.5,9.,48.5));
#92168=CARTESIAN_POINT('',(90.,9.,48.5));
#92169=CARTESIAN_POINT('',(100.3,10.2,48.5));
#92170=CARTESIAN_POINT('Origin',(101.5,10.2,48.5));
#92171=CARTESIAN_POINT('Origin',(101.5,10.2,48.5));
#92172=CARTESIAN_POINT('',(90.,9.,48.5));
#92173=CARTESIAN_POINT('',(129.5,9.,48.5));
#92174=CARTESIAN_POINT('',(90.,9.,48.5));
#92175=CARTESIAN_POINT('',(129.5,27.5,48.5));
#92176=CARTESIAN_POINT('',(129.5,23.125,48.5));
#92177=CARTESIAN_POINT('',(90.,27.5,48.5));
#92178=CARTESIAN_POINT('',(104.9,18.,48.5));
#92179=CARTESIAN_POINT('Origin',(110.,18.,48.5));
#92180=CARTESIAN_POINT('Origin',(118.5,10.2,48.5));
#92181=CARTESIAN_POINT('',(117.45,10.2,44.5));
#92182=CARTESIAN_POINT('',(117.45,10.2,48.5));
#92183=CARTESIAN_POINT('Origin',(118.5,10.2,44.5));
#92184=CARTESIAN_POINT('Origin',(101.5,10.2,48.425));
#92185=CARTESIAN_POINT('',(100.45,10.2,48.35));
#92186=CARTESIAN_POINT('',(100.375,10.2,48.425));
#92187=CARTESIAN_POINT('Origin',(101.5,10.2,48.35));
#92188=CARTESIAN_POINT('Origin',(101.5,10.2,48.5));
#92189=CARTESIAN_POINT('',(100.45,10.2,44.5));
#92190=CARTESIAN_POINT('',(100.45,10.2,48.5));
#92191=CARTESIAN_POINT('Origin',(101.5,10.2,44.5));
#92192=CARTESIAN_POINT('Origin',(118.5,10.2,44.1845481750105));
#92193=CARTESIAN_POINT('',(118.5,10.2,43.8690963500211));
#92194=CARTESIAN_POINT('',(117.975,10.2,44.1845481750105));
#92195=CARTESIAN_POINT('Origin',(101.5,10.2,44.1845481750105));
#92196=CARTESIAN_POINT('',(101.5,10.2,43.8690963500211));
#92197=CARTESIAN_POINT('',(100.975,10.2,44.1845481750105));
#92198=CARTESIAN_POINT('Origin',(122.,10.75,8.625));
#92199=CARTESIAN_POINT('',(122.421307488659,9.,8.5));
#92200=CARTESIAN_POINT('',(121.578692511341,9.,8.5));
#92201=CARTESIAN_POINT('Ctrl Pts',(122.421307488659,9.,8.5));
#92202=CARTESIAN_POINT('Ctrl Pts',(122.,8.95,8.55));
#92203=CARTESIAN_POINT('Ctrl Pts',(121.578692511341,9.,8.5));
#92204=CARTESIAN_POINT('',(120.2,10.75,8.5));
#92205=CARTESIAN_POINT('Origin',(122.,10.75,8.5));
#92206=CARTESIAN_POINT('',(120.45,10.75,8.75));
#92207=CARTESIAN_POINT('',(120.325,10.75,8.625));
#92208=CARTESIAN_POINT('Origin',(122.,10.75,8.75));
#92209=CARTESIAN_POINT('Origin',(122.,10.75,8.5));
#92210=CARTESIAN_POINT('Origin',(90.,8.75,8.75));
#92211=CARTESIAN_POINT('',(129.5,9.,8.5));
#92212=CARTESIAN_POINT('',(90.,9.,8.5));
#92213=CARTESIAN_POINT('',(129.5,8.5,9.));
#92214=CARTESIAN_POINT('',(129.5,9.,8.5));
#92215=CARTESIAN_POINT('',(90.5,8.5,9.));
#92216=CARTESIAN_POINT('',(90.,8.5,9.));
#92217=CARTESIAN_POINT('',(90.5,9.,8.5));
#92218=CARTESIAN_POINT('',(90.5,8.5,9.));
#92219=CARTESIAN_POINT('',(97.5786925113412,9.,8.5));
#92220=CARTESIAN_POINT('',(90.,9.,8.5));
#92221=CARTESIAN_POINT('',(98.4213074886588,9.,8.5));
#92222=CARTESIAN_POINT('Ctrl Pts',(98.4213074886588,9.,8.5));
#92223=CARTESIAN_POINT('Ctrl Pts',(98.,8.95,8.55));
#92224=CARTESIAN_POINT('Ctrl Pts',(97.5786925113412,9.,8.5));
#92225=CARTESIAN_POINT('',(108.431561285864,9.,8.5));
#92226=CARTESIAN_POINT('',(90.,9.,8.5));
#92227=CARTESIAN_POINT('Ctrl Pts',(110.,8.7,8.8));
#92228=CARTESIAN_POINT('Ctrl Pts',(109.215780642932,8.7,8.8));
#92229=CARTESIAN_POINT('Ctrl Pts',(108.431561285864,9.,8.5));
#92230=CARTESIAN_POINT('',(90.,9.,8.5));
#92231=CARTESIAN_POINT('Origin',(122.,10.75,8.5));
#92232=CARTESIAN_POINT('',(120.45,10.75,15.497705265805));
#92233=CARTESIAN_POINT('',(120.45,10.75,8.5));
#92234=CARTESIAN_POINT('Origin',(122.,10.75,15.497705265805));
#92235=CARTESIAN_POINT('Origin',(98.,10.75,8.625));
#92236=CARTESIAN_POINT('',(96.2,10.75,8.5));
#92237=CARTESIAN_POINT('Origin',(98.,10.75,8.5));
#92238=CARTESIAN_POINT('',(96.45,10.75,8.75));
#92239=CARTESIAN_POINT('',(96.325,10.75,8.625));
#92240=CARTESIAN_POINT('Origin',(98.,10.75,8.75));
#92241=CARTESIAN_POINT('Origin',(98.,10.75,8.5));
#92242=CARTESIAN_POINT('Origin',(98.,10.75,8.5));
#92243=CARTESIAN_POINT('',(96.45,10.75,15.497705265805));
#92244=CARTESIAN_POINT('',(96.45,10.75,8.5));
#92245=CARTESIAN_POINT('Origin',(98.,10.75,15.497705265805));
#92246=CARTESIAN_POINT('Origin',(110.,10.75,8.65));
#92247=CARTESIAN_POINT('Origin',(110.,10.75,8.8));
#92248=CARTESIAN_POINT('Origin',(110.,10.75,8.5));
#92249=CARTESIAN_POINT('Origin',(110.,10.75,8.5));
#92250=CARTESIAN_POINT('',(107.95,10.75,15.497705265805));
#92251=CARTESIAN_POINT('',(107.95,10.75,8.5));
#92252=CARTESIAN_POINT('Origin',(110.,10.75,15.497705265805));
#92253=CARTESIAN_POINT('Origin',(90.,8.5,8.5));
#92254=CARTESIAN_POINT('',(90.5,27.5,8.5));
#92255=CARTESIAN_POINT('',(90.5,13.375,8.5));
#92256=CARTESIAN_POINT('',(129.5,27.5,8.5));
#92257=CARTESIAN_POINT('',(90.,27.5,8.5));
#92258=CARTESIAN_POINT('',(129.5,13.375,8.5));
#92259=CARTESIAN_POINT('Origin',(110.,27.925,47.));
#92260=CARTESIAN_POINT('',(109.336675041929,28.,48.));
#92261=CARTESIAN_POINT('',(110.663324958071,28.,48.));
#92262=CARTESIAN_POINT('Ctrl Pts',(109.336675041929,28.,48.));
#92263=CARTESIAN_POINT('Ctrl Pts',(110.,27.8,48.2));
#92264=CARTESIAN_POINT('Ctrl Pts',(110.663324958071,28.,48.));
#92265=CARTESIAN_POINT('',(108.8,28.,47.));
#92266=CARTESIAN_POINT('Origin',(110.,28.,47.));
#92267=CARTESIAN_POINT('',(108.95,27.85,47.));
#92268=CARTESIAN_POINT('',(108.875,27.925,47.));
#92269=CARTESIAN_POINT('Origin',(110.,27.85,47.));
#92270=CARTESIAN_POINT('Origin',(110.,28.,47.));
#92271=CARTESIAN_POINT('Origin',(90.,27.75,48.25));
#92272=CARTESIAN_POINT('',(90.5,28.,48.));
#92273=CARTESIAN_POINT('',(90.,28.,48.));
#92274=CARTESIAN_POINT('',(90.5,28.,48.));
#92275=CARTESIAN_POINT('',(129.5,28.,48.));
#92276=CARTESIAN_POINT('',(129.5,27.5,48.5));
#92277=CARTESIAN_POINT('',(90.,28.,48.));
#92278=CARTESIAN_POINT('Origin',(110.,28.,47.));
#92279=CARTESIAN_POINT('',(108.95,22.8,47.));
#92280=CARTESIAN_POINT('',(108.95,28.,47.));
#92281=CARTESIAN_POINT('',(110.,22.8,45.95));
#92282=CARTESIAN_POINT('Origin',(110.,22.8,47.));
#92283=CARTESIAN_POINT('',(110.,22.8,48.05));
#92284=CARTESIAN_POINT('Origin',(110.,22.8,47.));
#92285=CARTESIAN_POINT('Origin',(110.,22.8,47.));
#92286=CARTESIAN_POINT('Origin',(110.,27.925,44.5));
#92287=CARTESIAN_POINT('',(108.8,28.,44.5));
#92288=CARTESIAN_POINT('Origin',(110.,28.,44.5));
#92289=CARTESIAN_POINT('',(108.95,27.85,44.5));
#92290=CARTESIAN_POINT('',(108.875,27.925,44.5));
#92291=CARTESIAN_POINT('Origin',(110.,27.85,44.5));
#92292=CARTESIAN_POINT('Origin',(90.,28.,8.5));
#92293=CARTESIAN_POINT('',(129.5,28.,9.));
#92294=CARTESIAN_POINT('',(129.5,28.,18.5));
#92295=CARTESIAN_POINT('',(90.5,28.,9.));
#92296=CARTESIAN_POINT('',(90.,28.,9.));
#92297=CARTESIAN_POINT('',(90.5,28.,18.5));
#92298=CARTESIAN_POINT('',(108.8,28.,42.));
#92299=CARTESIAN_POINT('Origin',(110.,28.,42.));
#92300=CARTESIAN_POINT('',(124.2,28.,44.5));
#92301=CARTESIAN_POINT('Origin',(126.,28.,44.5));
#92302=CARTESIAN_POINT('',(92.2,28.,44.5));
#92303=CARTESIAN_POINT('Origin',(94.,28.,44.5));
#92304=CARTESIAN_POINT('',(124.2,28.,12.5));
#92305=CARTESIAN_POINT('Origin',(126.,28.,12.5));
#92306=CARTESIAN_POINT('',(92.2,28.,12.5));
#92307=CARTESIAN_POINT('Origin',(94.,28.,12.5));
#92308=CARTESIAN_POINT('Origin',(110.,28.,44.5));
#92309=CARTESIAN_POINT('',(108.95,22.8,44.5));
#92310=CARTESIAN_POINT('',(108.95,28.,44.5));
#92311=CARTESIAN_POINT('',(110.,22.8,43.45));
#92312=CARTESIAN_POINT('Origin',(110.,22.8,44.5));
#92313=CARTESIAN_POINT('',(110.,22.8,45.55));
#92314=CARTESIAN_POINT('Origin',(110.,22.8,44.5));
#92315=CARTESIAN_POINT('Origin',(110.,22.8,44.5));
#92316=CARTESIAN_POINT('Origin',(110.,27.925,42.));
#92317=CARTESIAN_POINT('',(108.95,27.85,42.));
#92318=CARTESIAN_POINT('',(108.875,27.925,42.));
#92319=CARTESIAN_POINT('Origin',(110.,27.85,42.));
#92320=CARTESIAN_POINT('Origin',(110.,28.,42.));
#92321=CARTESIAN_POINT('',(108.95,22.8,42.));
#92322=CARTESIAN_POINT('',(108.95,28.,42.));
#92323=CARTESIAN_POINT('',(110.,22.8,40.95));
#92324=CARTESIAN_POINT('Origin',(110.,22.8,42.));
#92325=CARTESIAN_POINT('',(110.,22.8,43.05));
#92326=CARTESIAN_POINT('Origin',(110.,22.8,42.));
#92327=CARTESIAN_POINT('Origin',(110.,22.8,42.));
#92328=CARTESIAN_POINT('Origin',(110.,22.8,42.));
#92329=CARTESIAN_POINT('',(110.,22.8,48.5));
#92330=CARTESIAN_POINT('Origin',(110.,22.8,42.));
#92331=CARTESIAN_POINT('',(110.,22.8,48.5));
#92332=CARTESIAN_POINT('Origin',(110.,22.8,44.5));
#92333=CARTESIAN_POINT('',(110.,22.8,48.5));
#92334=CARTESIAN_POINT('Origin',(110.,22.8,44.5));
#92335=CARTESIAN_POINT('',(110.,22.8,48.5));
#92336=CARTESIAN_POINT('Origin',(110.,22.8,47.));
#92337=CARTESIAN_POINT('',(110.,22.8,48.5));
#92338=CARTESIAN_POINT('Origin',(110.,22.8,47.));
#92339=CARTESIAN_POINT('',(110.,22.8,48.5));
#92340=CARTESIAN_POINT('Origin',(126.,27.875,44.5));
#92341=CARTESIAN_POINT('',(124.45,27.75,44.5));
#92342=CARTESIAN_POINT('',(124.325,27.875,44.5));
#92343=CARTESIAN_POINT('Origin',(126.,27.75,44.5));
#92344=CARTESIAN_POINT('Origin',(126.,28.,44.5));
#92345=CARTESIAN_POINT('',(124.45,22.,44.5));
#92346=CARTESIAN_POINT('',(124.45,28.,44.5));
#92347=CARTESIAN_POINT('Origin',(126.,22.,44.5));
#92348=CARTESIAN_POINT('Origin',(94.,27.875,12.5));
#92349=CARTESIAN_POINT('',(92.45,27.75,12.5));
#92350=CARTESIAN_POINT('',(92.325,27.875,12.5));
#92351=CARTESIAN_POINT('Origin',(94.,27.75,12.5));
#92352=CARTESIAN_POINT('Origin',(94.,28.,12.5));
#92353=CARTESIAN_POINT('',(92.45,22.,12.5));
#92354=CARTESIAN_POINT('',(92.45,28.,12.5));
#92355=CARTESIAN_POINT('Origin',(94.,22.,12.5));
#92356=CARTESIAN_POINT('Origin',(94.,27.875,44.5));
#92357=CARTESIAN_POINT('',(92.45,27.75,44.5));
#92358=CARTESIAN_POINT('',(92.325,27.875,44.5));
#92359=CARTESIAN_POINT('Origin',(94.,27.75,44.5));
#92360=CARTESIAN_POINT('Origin',(94.,28.,44.5));
#92361=CARTESIAN_POINT('',(92.45,22.,44.5));
#92362=CARTESIAN_POINT('',(92.45,28.,44.5));
#92363=CARTESIAN_POINT('Origin',(94.,22.,44.5));
#92364=CARTESIAN_POINT('Origin',(126.,27.875,12.5));
#92365=CARTESIAN_POINT('',(124.45,27.75,12.5));
#92366=CARTESIAN_POINT('',(124.325,27.875,12.5));
#92367=CARTESIAN_POINT('Origin',(126.,27.75,12.5));
#92368=CARTESIAN_POINT('Origin',(126.,28.,12.5));
#92369=CARTESIAN_POINT('',(124.45,22.,12.5));
#92370=CARTESIAN_POINT('',(124.45,28.,12.5));
#92371=CARTESIAN_POINT('Origin',(126.,22.,12.5));
#92372=CARTESIAN_POINT('Origin',(126.,22.,44.5));
#92373=CARTESIAN_POINT('',(126.,21.0686660405073,44.5));
#92374=CARTESIAN_POINT('',(124.45,22.,44.5));
#92375=CARTESIAN_POINT('Origin',(126.,22.,12.5));
#92376=CARTESIAN_POINT('',(126.,21.0686660405073,12.5));
#92377=CARTESIAN_POINT('',(124.45,22.,12.5));
#92378=CARTESIAN_POINT('Origin',(94.,22.,44.5));
#92379=CARTESIAN_POINT('',(94.,21.0686660405073,44.5));
#92380=CARTESIAN_POINT('',(92.45,22.,44.5));
#92381=CARTESIAN_POINT('Origin',(94.,22.,12.5));
#92382=CARTESIAN_POINT('',(94.,21.0686660405073,12.5));
#92383=CARTESIAN_POINT('',(92.45,22.,12.5));
#92384=CARTESIAN_POINT('Origin',(110.,18.,48.35));
#92385=CARTESIAN_POINT('',(105.2,18.,48.2));
#92386=CARTESIAN_POINT('',(105.05,18.,48.35));
#92387=CARTESIAN_POINT('',(110.,22.8,48.2));
#92388=CARTESIAN_POINT('Origin',(110.,18.,48.2));
#92389=CARTESIAN_POINT('Origin',(110.,18.,48.2));
#92390=CARTESIAN_POINT('Origin',(110.,18.,48.5));
#92391=CARTESIAN_POINT('',(110.,22.8,48.5));
#92392=CARTESIAN_POINT('',(110.,22.8,48.5));
#92393=CARTESIAN_POINT('',(110.,22.8,48.5));
#92394=CARTESIAN_POINT('',(110.,22.8,25.8));
#92395=CARTESIAN_POINT('',(110.,22.8,48.5));
#92396=CARTESIAN_POINT('',(113.746998799039,15.,25.8));
#92397=CARTESIAN_POINT('Origin',(110.,18.,25.8));
#92398=CARTESIAN_POINT('',(113.746998799039,15.,32.));
#92399=CARTESIAN_POINT('',(113.746998799039,15.,48.5));
#92400=CARTESIAN_POINT('',(106.253001200961,15.,32.));
#92401=CARTESIAN_POINT('Origin',(110.,18.,32.));
#92402=CARTESIAN_POINT('',(106.253001200961,15.,25.8));
#92403=CARTESIAN_POINT('',(106.253001200961,15.,48.5));
#92404=CARTESIAN_POINT('Origin',(110.,18.,25.8));
#92405=CARTESIAN_POINT('Origin',(110.,18.,10.7414134684777));
#92406=CARTESIAN_POINT('',(110.,18.,9.98282693695541));
#92407=CARTESIAN_POINT('',(107.475,18.,11.5));
#92408=CARTESIAN_POINT('',(108.7375,18.,10.7414134684777));
#92409=CARTESIAN_POINT('Origin',(110.,18.,11.5));
#92410=CARTESIAN_POINT('Origin',(110.,18.,25.8));
#92411=CARTESIAN_POINT('',(107.475,18.,25.8));
#92412=CARTESIAN_POINT('Origin',(110.,18.,25.8));
#92413=CARTESIAN_POINT('',(107.475,18.,25.8));
#92414=CARTESIAN_POINT('Origin',(110.,18.,25.8));
#92415=CARTESIAN_POINT('',(100.,15.,25.8));
#92416=CARTESIAN_POINT('Origin',(90.,15.,25.));
#92417=CARTESIAN_POINT('',(90.,15.,32.));
#92418=CARTESIAN_POINT('',(90.,15.,32.));
#92419=CARTESIAN_POINT('',(90.,15.,25.));
#92420=CARTESIAN_POINT('',(90.,15.,26.75));
#92421=CARTESIAN_POINT('',(130.,15.,25.));
#92422=CARTESIAN_POINT('',(90.,15.,25.));
#92423=CARTESIAN_POINT('',(130.,15.,32.));
#92424=CARTESIAN_POINT('',(130.,15.,26.75));
#92425=CARTESIAN_POINT('',(90.,15.,32.));
#92426=CARTESIAN_POINT('Origin',(90.,7.5,25.));
#92427=CARTESIAN_POINT('',(130.,13.03,25.));
#92428=CARTESIAN_POINT('',(90.,13.03,25.));
#92429=CARTESIAN_POINT('',(90.,13.03,25.));
#92430=CARTESIAN_POINT('',(130.,12.875,25.));
#92431=CARTESIAN_POINT('',(90.,12.875,25.));
#92432=CARTESIAN_POINT('Origin',(90.,15.,32.));
#92433=CARTESIAN_POINT('',(130.,13.03,32.));
#92434=CARTESIAN_POINT('',(130.,16.625,32.));
#92435=CARTESIAN_POINT('',(90.,13.03,32.));
#92436=CARTESIAN_POINT('',(90.,13.03,32.));
#92437=CARTESIAN_POINT('',(90.,16.625,32.));
#92438=CARTESIAN_POINT('Origin',(90.,18.25,28.5));
#92439=CARTESIAN_POINT('',(90.,13.03,41.0519615242271));
#92440=CARTESIAN_POINT('',(90.,13.03,21.3406733260263));
#92441=CARTESIAN_POINT('',(90.,9.,38.7252399393929));
#92442=CARTESIAN_POINT('',(90.,12.2699206131736,40.6131294856374));
#92443=CARTESIAN_POINT('',(90.,9.,48.));
#92444=CARTESIAN_POINT('',(90.,9.,38.5));
#92445=CARTESIAN_POINT('',(90.,27.5,48.));
#92446=CARTESIAN_POINT('',(90.,23.125,48.));
#92447=CARTESIAN_POINT('',(90.,27.5,9.));
#92448=CARTESIAN_POINT('',(90.,27.5,18.5));
#92449=CARTESIAN_POINT('',(90.,9.,9.));
#92450=CARTESIAN_POINT('',(90.,13.375,9.));
#92451=CARTESIAN_POINT('',(90.,9.,16.5080682368869));
#92452=CARTESIAN_POINT('',(90.,9.,38.5));
#92453=CARTESIAN_POINT('',(90.,13.03,14.1813466520527));
#92454=CARTESIAN_POINT('',(90.,9.12242061317363,16.4373886629167));
#92455=CARTESIAN_POINT('',(90.,13.03,21.3406733260263));
#92456=CARTESIAN_POINT('Origin',(90.,13.03,14.1813466520527));
#92457=CARTESIAN_POINT('',(130.,13.03,41.0519615242271));
#92458=CARTESIAN_POINT('',(130.,13.03,21.3406733260263));
#92459=CARTESIAN_POINT('',(90.,13.03,41.0519615242271));
#92460=CARTESIAN_POINT('Origin',(90.,13.03,41.0519615242271));
#92461=CARTESIAN_POINT('',(90.5,8.5,38.4365648047981));
#92462=CARTESIAN_POINT('',(88.9835805013516,10.0164194986484,39.3120700105471));
#92463=CARTESIAN_POINT('',(130.,9.,38.7252399393929));
#92464=CARTESIAN_POINT('',(130.,12.2699206131736,40.6131294856374));
#92465=CARTESIAN_POINT('',(129.5,8.5,38.4365648047981));
#92466=CARTESIAN_POINT('',(122.44499092722,1.44499092721981,34.3633534174932));
#92467=CARTESIAN_POINT('',(90.,8.5,38.4365648047981));
#92468=CARTESIAN_POINT('Origin',(90.,7.5,17.3740936406713));
#92469=CARTESIAN_POINT('',(90.5,8.5,16.7967433714817));
#92470=CARTESIAN_POINT('',(93.25651022645,5.74348977355006,18.3882152927465));
#92471=CARTESIAN_POINT('',(129.5,8.5,16.7967433714817));
#92472=CARTESIAN_POINT('',(90.,8.5,16.7967433714817));
#92473=CARTESIAN_POINT('',(130.,9.,16.5080682368869));
#92474=CARTESIAN_POINT('',(118.172061202121,-2.82793879787853,23.3369318858005));
#92475=CARTESIAN_POINT('',(130.,13.03,14.1813466520527));
#92476=CARTESIAN_POINT('',(130.,9.12242061317363,16.4373886629167));
#92477=CARTESIAN_POINT('',(90.,13.03,14.1813466520527));
#92478=CARTESIAN_POINT('Origin',(90.,13.03,14.1813466520527));
#92479=CARTESIAN_POINT('',(130.,13.03,21.3406733260263));
#92480=CARTESIAN_POINT('Origin',(90.25,8.75,38.5));
#92481=CARTESIAN_POINT('',(90.5,8.5,48.));
#92482=CARTESIAN_POINT('',(90.5,8.5,38.5));
#92483=CARTESIAN_POINT('',(90.5,8.5,48.));
#92484=CARTESIAN_POINT('Origin',(90.25,8.75,38.5));
#92485=CARTESIAN_POINT('',(90.,9.,9.));
#92486=CARTESIAN_POINT('',(90.5,8.5,38.5));
#92487=CARTESIAN_POINT('Origin',(90.,8.5,48.5));
#92488=CARTESIAN_POINT('',(129.5,8.5,48.));
#92489=CARTESIAN_POINT('',(129.5,8.5,38.5));
#92490=CARTESIAN_POINT('',(90.,8.5,48.));
#92491=CARTESIAN_POINT('Origin',(129.75,8.75,38.5));
#92492=CARTESIAN_POINT('',(130.,9.,48.));
#92493=CARTESIAN_POINT('',(130.,9.,38.5));
#92494=CARTESIAN_POINT('',(130.,9.,48.));
#92495=CARTESIAN_POINT('Origin',(129.5,8.5,48.));
#92496=CARTESIAN_POINT('',(129.5,9.,48.5));
#92497=CARTESIAN_POINT('',(129.5,8.5,48.));
#92498=CARTESIAN_POINT('Origin',(129.5,27.5,48.5));
#92499=CARTESIAN_POINT('',(130.,27.5,48.));
#92500=CARTESIAN_POINT('',(129.5,28.,48.));
#92501=CARTESIAN_POINT('',(130.,27.5,48.));
#92502=CARTESIAN_POINT('Origin',(90.,9.,48.));
#92503=CARTESIAN_POINT('',(90.5,9.,48.5));
#92504=CARTESIAN_POINT('',(90.,9.,48.));
#92505=CARTESIAN_POINT('Origin',(129.5,9.,8.5));
#92506=CARTESIAN_POINT('',(130.,9.,9.));
#92507=CARTESIAN_POINT('',(129.5,8.5,9.));
#92508=CARTESIAN_POINT('',(130.,9.,9.));
#92509=CARTESIAN_POINT('Origin',(90.,27.5,48.));
#92510=CARTESIAN_POINT('',(90.,27.5,48.));
#92511=CARTESIAN_POINT('',(90.5,27.5,48.5));
#92512=CARTESIAN_POINT('Origin',(129.5,28.,9.));
#92513=CARTESIAN_POINT('',(130.,27.5,9.));
#92514=CARTESIAN_POINT('',(129.5,27.5,8.5));
#92515=CARTESIAN_POINT('',(129.5,28.,9.));
#92516=CARTESIAN_POINT('',(130.,27.5,9.));
#92517=CARTESIAN_POINT('Origin',(90.,9.,9.));
#92518=CARTESIAN_POINT('',(90.5,9.,8.5));
#92519=CARTESIAN_POINT('Origin',(90.5,28.,9.));
#92520=CARTESIAN_POINT('',(90.,27.5,9.));
#92521=CARTESIAN_POINT('',(90.5,28.,9.));
#92522=CARTESIAN_POINT('',(90.5,27.5,8.5));
#92523=CARTESIAN_POINT('Origin',(90.25,27.75,18.5));
#92524=CARTESIAN_POINT('Origin',(90.,27.75,8.75));
#92525=CARTESIAN_POINT('Origin',(90.25,13.375,8.75));
#92526=CARTESIAN_POINT('Origin',(129.75,27.75,18.5));
#92527=CARTESIAN_POINT('',(130.,27.5,18.5));
#92528=CARTESIAN_POINT('Origin',(129.75,13.375,8.75));
#92529=CARTESIAN_POINT('',(130.,13.375,9.));
#92530=CARTESIAN_POINT('Origin',(90.25,23.125,48.25));
#92531=CARTESIAN_POINT('Origin',(129.75,8.75,38.5));
#92532=CARTESIAN_POINT('',(129.5,8.5,38.5));
#92533=CARTESIAN_POINT('',(130.,9.,38.5));
#92534=CARTESIAN_POINT('Origin',(90.,8.75,48.25));
#92535=CARTESIAN_POINT('Origin',(129.75,23.125,48.25));
#92536=CARTESIAN_POINT('',(130.,23.125,48.));
#92537=CARTESIAN_POINT('Origin',(90.,8.5,48.5));
#92538=CARTESIAN_POINT('Origin',(130.,18.25,28.5));
#92539=CARTESIAN_POINT('',(0.,0.,0.));
#92540=CARTESIAN_POINT('Origin',(110.,10.75,14.5323462819564));
#92541=CARTESIAN_POINT('',(109.6,10.75,15.5323462819564));
#92542=CARTESIAN_POINT('Origin',(110.,11.0964101615138,15.3323462819564));
#92543=CARTESIAN_POINT('',(110.,10.75,15.9323462819564));
#92544=CARTESIAN_POINT('',(108.6,10.75,14.5323462819564));
#92545=CARTESIAN_POINT('Origin',(122.,10.75,14.5323462819564));
#92546=CARTESIAN_POINT('',(121.6,10.75,15.5323462819564));
#92547=CARTESIAN_POINT('Origin',(122.,11.0964101615138,15.3323462819564));
#92548=CARTESIAN_POINT('',(122.,10.75,15.9323462819564));
#92549=CARTESIAN_POINT('',(120.6,10.75,14.5323462819564));
#92550=CARTESIAN_POINT('Origin',(98.,10.75,14.5323462819564));
#92551=CARTESIAN_POINT('',(97.6,10.75,15.5323462819564));
#92552=CARTESIAN_POINT('Origin',(98.,11.0964101615138,15.3323462819564));
#92553=CARTESIAN_POINT('',(98.,10.75,15.9323462819564));
#92554=CARTESIAN_POINT('',(96.6,10.75,14.5323462819564));
#92555=CARTESIAN_POINT('Origin',(129.6,12.7,15.3735749579293));
#92556=CARTESIAN_POINT('',(129.7,12.6,15.9653589838486));
#92557=CARTESIAN_POINT('',(129.7,12.6,14.6951883916314));
#92558=CARTESIAN_POINT('',(129.7,12.6,15.3735749579293));
#92559=CARTESIAN_POINT('',(129.5,12.8,14.3487782301177));
#92560=CARTESIAN_POINT('',(129.7,12.6,14.6951883916314));
#92561=CARTESIAN_POINT('',(129.5,12.8,16.0808290376865));
#92562=CARTESIAN_POINT('',(129.5,12.8,15.3735749579293));
#92563=CARTESIAN_POINT('',(129.7,12.6,15.9653589838486));
#92564=CARTESIAN_POINT('Origin',(129.6,9.5875,16.3189860237273));
#92565=CARTESIAN_POINT('',(129.7,8.9,16.8313843876331));
#92566=CARTESIAN_POINT('',(129.7,9.6375,16.4055885641057));
#92567=CARTESIAN_POINT('',(129.5,8.7,16.7159143337951));
#92568=CARTESIAN_POINT('',(129.7,8.9,16.8313843876331));
#92569=CARTESIAN_POINT('',(129.5,9.5375,16.2323834833488));
#92570=CARTESIAN_POINT('Origin',(129.6,8.8,17.4231684135524));
#92571=CARTESIAN_POINT('',(129.7,8.9,18.1015549798502));
#92572=CARTESIAN_POINT('',(129.7,8.9,17.4231684135524));
#92573=CARTESIAN_POINT('',(129.5,8.7,18.447965141364));
#92574=CARTESIAN_POINT('',(129.7,8.9,18.1015549798502));
#92575=CARTESIAN_POINT('',(129.5,8.7,17.4231684135524));
#92576=CARTESIAN_POINT('Origin',(129.6,11.9125,16.4777573477544));
#92577=CARTESIAN_POINT('',(129.5,11.9625,16.5643598881329));
#92578=CARTESIAN_POINT('',(129.7,11.8625,16.391154807376));
#92579=CARTESIAN_POINT('Origin',(90.3,12.8,16.0808290376865));
#92580=CARTESIAN_POINT('',(90.5,12.8,16.0808290376865));
#92581=CARTESIAN_POINT('',(90.3,12.8,16.0808290376865));
#92582=CARTESIAN_POINT('',(90.5,8.7,18.447965141364));
#92583=CARTESIAN_POINT('',(90.5,11.9625,16.5643598881329));
#92584=CARTESIAN_POINT('',(90.3,8.7,18.447965141364));
#92585=CARTESIAN_POINT('Origin',(90.3,12.8,14.3487782301177));
#92586=CARTESIAN_POINT('',(90.5,12.8,14.3487782301177));
#92587=CARTESIAN_POINT('',(90.3,12.8,14.3487782301177));
#92588=CARTESIAN_POINT('',(90.5,12.8,15.3735749579293));
#92589=CARTESIAN_POINT('Origin',(129.7,10.75,16.3983716857408));
#92590=CARTESIAN_POINT('Origin',(90.4,12.7,15.3735749579293));
#92591=CARTESIAN_POINT('',(90.3,12.6,14.6951883916314));
#92592=CARTESIAN_POINT('',(90.3,12.6,15.9653589838486));
#92593=CARTESIAN_POINT('',(90.3,12.6,15.3735749579293));
#92594=CARTESIAN_POINT('',(90.3,12.6,15.9653589838486));
#92595=CARTESIAN_POINT('',(90.3,12.6,14.6951883916314));
#92596=CARTESIAN_POINT('Origin',(90.4,11.9125,16.4777573477544));
#92597=CARTESIAN_POINT('',(90.3,8.9,18.1015549798502));
#92598=CARTESIAN_POINT('',(90.3,11.8625,16.391154807376));
#92599=CARTESIAN_POINT('',(90.3,8.9,18.1015549798502));
#92600=CARTESIAN_POINT('Origin',(90.4,9.5875,16.3189860237273));
#92601=CARTESIAN_POINT('',(90.5,8.7,16.7159143337951));
#92602=CARTESIAN_POINT('',(90.5,9.5375,16.2323834833488));
#92603=CARTESIAN_POINT('',(90.3,8.9,16.8313843876331));
#92604=CARTESIAN_POINT('',(90.5,8.7,16.7159143337951));
#92605=CARTESIAN_POINT('',(90.3,9.6375,16.4055885641057));
#92606=CARTESIAN_POINT('Origin',(90.4,8.8,17.4231684135524));
#92607=CARTESIAN_POINT('',(90.3,8.9,17.4231684135524));
#92608=CARTESIAN_POINT('',(90.5,8.7,17.4231684135524));
#92609=CARTESIAN_POINT('Origin',(90.3,8.7,16.7159143337951));
#92610=CARTESIAN_POINT('',(90.3,8.7,16.7159143337951));
#92611=CARTESIAN_POINT('Origin',(90.3,10.75,16.3983716857408));
#92612=CARTESIAN_POINT('Origin',(90.3,8.7,18.447965141364));
#92613=CARTESIAN_POINT('',(0.,0.,0.));
#92614=CARTESIAN_POINT('Origin',(113.,20.1,61.));
#92615=CARTESIAN_POINT('',(108.643534003375,20.1,61.));
#92616=CARTESIAN_POINT('',(111.356465996625,20.1,61.));
#92617=CARTESIAN_POINT('Origin',(110.,18.,61.));
#92618=CARTESIAN_POINT('',(107.,20.1,61.));
#92619=CARTESIAN_POINT('Origin',(107.,20.1,65.));
#92620=CARTESIAN_POINT('',(111.356465996625,20.1,65.));
#92621=CARTESIAN_POINT('',(108.643534003375,20.1,65.));
#92622=CARTESIAN_POINT('Origin',(110.,18.,65.));
#92623=CARTESIAN_POINT('',(113.,20.1,65.));
#92624=CARTESIAN_POINT('Origin',(110.,20.1,63.));
#92625=CARTESIAN_POINT('',(108.643534003375,20.1,44.75));
#92626=CARTESIAN_POINT('',(111.356465996625,20.1,44.75));
#92627=CARTESIAN_POINT('Origin',(113.,20.1,32.3));
#92628=CARTESIAN_POINT('',(108.643534003375,20.1,32.3));
#92629=CARTESIAN_POINT('',(111.356465996625,20.1,32.3));
#92630=CARTESIAN_POINT('Origin',(110.,18.,32.3));
#92631=CARTESIAN_POINT('',(107.,20.1,32.3));
#92632=CARTESIAN_POINT('Origin',(107.,20.1,34.3));
#92633=CARTESIAN_POINT('',(111.356465996625,20.1,34.3));
#92634=CARTESIAN_POINT('',(108.643534003375,20.1,34.3));
#92635=CARTESIAN_POINT('Origin',(110.,18.,34.3));
#92636=CARTESIAN_POINT('',(113.,20.1,34.3));
#92637=CARTESIAN_POINT('Origin',(110.,20.1,33.3));
#92638=CARTESIAN_POINT('',(108.643534003375,20.1,44.75));
#92639=CARTESIAN_POINT('',(111.356465996625,20.1,44.75));
#92640=CARTESIAN_POINT('Origin',(112.2,18.,11.7));
#92641=CARTESIAN_POINT('',(107.8,18.,11.7));
#92642=CARTESIAN_POINT('Origin',(110.,18.,11.7));
#92643=CARTESIAN_POINT('Origin',(110.,18.,11.85));
#92644=CARTESIAN_POINT('',(107.5,18.,12.));
#92645=CARTESIAN_POINT('Origin',(110.,18.,12.));
#92646=CARTESIAN_POINT('',(107.65,18.,11.85));
#92647=CARTESIAN_POINT('Origin',(110.,18.,44.75));
#92648=CARTESIAN_POINT('',(107.5,18.,77.5));
#92649=CARTESIAN_POINT('Origin',(110.,18.,77.5));
#92650=CARTESIAN_POINT('',(107.5,18.,44.75));
#92651=CARTESIAN_POINT('Origin',(110.,18.,77.65));
#92652=CARTESIAN_POINT('',(107.8,18.,77.8));
#92653=CARTESIAN_POINT('Origin',(110.,18.,77.8));
#92654=CARTESIAN_POINT('',(107.65,18.,77.65));
#92655=CARTESIAN_POINT('Origin',(110.,18.,77.8));
#92656=CARTESIAN_POINT('',(0.,0.,0.));
#92657=CARTESIAN_POINT('Origin',(110.,20.4,33.3));
#92658=CARTESIAN_POINT('',(110.7,20.4,34.0826237921249));
#92659=CARTESIAN_POINT('',(110.7,20.4,32.5173762078751));
#92660=CARTESIAN_POINT('',(110.7,20.4,30.4));
#92661=CARTESIAN_POINT('Origin',(110.,20.4,33.3));
#92662=CARTESIAN_POINT('Origin',(110.,22.5,33.3));
#92663=CARTESIAN_POINT('',(110.,22.5,34.35));
#92664=CARTESIAN_POINT('',(108.95,22.3757856437444,33.3));
#92665=CARTESIAN_POINT('Ctrl Pts',(110.,22.5,34.35));
#92666=CARTESIAN_POINT('Ctrl Pts',(109.867639766981,22.5,34.35));
#92667=CARTESIAN_POINT('Ctrl Pts',(109.72678604534,22.4935734225297,34.3234481778509));
#92668=CARTESIAN_POINT('Ctrl Pts',(109.46822707977,22.470354072227,34.2161384098672));
#92669=CARTESIAN_POINT('Ctrl Pts',(109.350482714578,22.4538755915385,34.1354069550695));
#92670=CARTESIAN_POINT('Ctrl Pts',(109.164583259651,22.4227775468468,33.9495075001425));
#92671=CARTESIAN_POINT('Ctrl Pts',(109.083859447964,22.4060986376458,33.8317672389861));
#92672=CARTESIAN_POINT('Ctrl Pts',(108.97655524524,22.382417098112,33.5732227222323));
#92673=CARTESIAN_POINT('Ctrl Pts',(108.95,22.3757856437444,33.4323741679718));
#92674=CARTESIAN_POINT('Ctrl Pts',(108.95,22.3757856437444,33.3));
#92675=CARTESIAN_POINT('',(110.,22.5,32.25));
#92676=CARTESIAN_POINT('Ctrl Pts',(110.,22.5,32.25));
#92677=CARTESIAN_POINT('Ctrl Pts',(110.132360233019,22.5,32.25));
#92678=CARTESIAN_POINT('Ctrl Pts',(110.27321395466,22.4935734225297,32.2765518221491));
#92679=CARTESIAN_POINT('Ctrl Pts',(110.53177292023,22.470354072227,32.3838615901328));
#92680=CARTESIAN_POINT('Ctrl Pts',(110.649517285422,22.4538755915385,32.4645930449305));
#92681=CARTESIAN_POINT('Ctrl Pts',(110.835416740349,22.4227775468468,32.6504924998574));
#92682=CARTESIAN_POINT('Ctrl Pts',(110.916140552036,22.4060986376458,32.7682327610139));
#92683=CARTESIAN_POINT('Ctrl Pts',(111.02344475476,22.382417098112,33.0267772777677));
#92684=CARTESIAN_POINT('Ctrl Pts',(111.05,22.3757856437444,33.1676258320282));
#92685=CARTESIAN_POINT('Ctrl Pts',(111.05,22.3757856437444,33.3));
#92686=CARTESIAN_POINT('Ctrl Pts',(111.05,22.3757856437444,33.4323741679718));
#92687=CARTESIAN_POINT('Ctrl Pts',(111.02344475476,22.382417098112,33.5732227222323));
#92688=CARTESIAN_POINT('Ctrl Pts',(110.916140552036,22.4060986376458,33.8317672389861));
#92689=CARTESIAN_POINT('Ctrl Pts',(110.835416740349,22.4227775468468,33.9495075001425));
#92690=CARTESIAN_POINT('Ctrl Pts',(110.649517285422,22.4538755915385,34.1354069550695));
#92691=CARTESIAN_POINT('Ctrl Pts',(110.53177292023,22.470354072227,34.2161384098672));
#92692=CARTESIAN_POINT('Ctrl Pts',(110.27321395466,22.4935734225297,34.3234481778509));
#92693=CARTESIAN_POINT('Ctrl Pts',(110.132360233019,22.5,34.35));
#92694=CARTESIAN_POINT('Ctrl Pts',(110.,22.5,34.35));
#92695=CARTESIAN_POINT('Ctrl Pts',(108.95,22.3757856437444,33.3));
#92696=CARTESIAN_POINT('Ctrl Pts',(108.95,22.3757856437444,33.1676258320282));
#92697=CARTESIAN_POINT('Ctrl Pts',(108.97655524524,22.382417098112,33.0267772777677));
#92698=CARTESIAN_POINT('Ctrl Pts',(109.083859447964,22.4060986376458,32.7682327610139));
#92699=CARTESIAN_POINT('Ctrl Pts',(109.164583259651,22.4227775468468,32.6504924998574));
#92700=CARTESIAN_POINT('Ctrl Pts',(109.350482714578,22.4538755915385,32.4645930449305));
#92701=CARTESIAN_POINT('Ctrl Pts',(109.46822707977,22.470354072227,32.3838615901328));
#92702=CARTESIAN_POINT('Ctrl Pts',(109.72678604534,22.4935734225297,32.2765518221491));
#92703=CARTESIAN_POINT('Ctrl Pts',(109.867639766981,22.5,32.25));
#92704=CARTESIAN_POINT('Ctrl Pts',(110.,22.5,32.25));
#92705=CARTESIAN_POINT('',(108.95,20.4,33.3));
#92706=CARTESIAN_POINT('',(108.95,22.5,33.3));
#92707=CARTESIAN_POINT('',(109.3,20.4,32.5173762078751));
#92708=CARTESIAN_POINT('Origin',(110.,20.4,33.3));
#92709=CARTESIAN_POINT('Ctrl Pts',(110.7,20.4,32.5173762078751));
#92710=CARTESIAN_POINT('Ctrl Pts',(110.615542349369,20.424633481434,32.4418349886629));
#92711=CARTESIAN_POINT('Ctrl Pts',(110.514132074769,20.4491019379392,32.376755439497));
#92712=CARTESIAN_POINT('Ctrl Pts',(110.274969793834,20.4882751681165,32.2770312340585));
#92713=CARTESIAN_POINT('Ctrl Pts',(110.133578485591,20.5,32.25));
#92714=CARTESIAN_POINT('Ctrl Pts',(109.866421514409,20.5,32.25));
#92715=CARTESIAN_POINT('Ctrl Pts',(109.725030206166,20.4882751681165,32.2770312340585));
#92716=CARTESIAN_POINT('Ctrl Pts',(109.485867925231,20.4491019379392,32.376755439497));
#92717=CARTESIAN_POINT('Ctrl Pts',(109.384457650631,20.424633481434,32.4418349886629));
#92718=CARTESIAN_POINT('Ctrl Pts',(109.3,20.4,32.5173762078751));
#92719=CARTESIAN_POINT('',(109.3,20.4,34.0826237921249));
#92720=CARTESIAN_POINT('Ctrl Pts',(109.3,20.4,34.0826237921249));
#92721=CARTESIAN_POINT('Ctrl Pts',(109.384457650631,20.424633481434,34.1581650113371));
#92722=CARTESIAN_POINT('Ctrl Pts',(109.485867925231,20.4491019379392,34.223244560503));
#92723=CARTESIAN_POINT('Ctrl Pts',(109.725030206166,20.4882751681165,34.3229687659415));
#92724=CARTESIAN_POINT('Ctrl Pts',(109.866421514409,20.5,34.35));
#92725=CARTESIAN_POINT('Ctrl Pts',(110.133578485591,20.5,34.35));
#92726=CARTESIAN_POINT('Ctrl Pts',(110.274969793834,20.4882751681165,34.3229687659415));
#92727=CARTESIAN_POINT('Ctrl Pts',(110.514132074769,20.4491019379392,34.223244560503));
#92728=CARTESIAN_POINT('Ctrl Pts',(110.615542349369,20.424633481434,34.1581650113371));
#92729=CARTESIAN_POINT('Ctrl Pts',(110.7,20.4,34.0826237921249));
#92730=CARTESIAN_POINT('Origin',(110.,20.4,33.3));
#92731=CARTESIAN_POINT('Origin',(110.,20.4,33.3));
#92732=CARTESIAN_POINT('',(109.3,20.4,30.4));
#92733=CARTESIAN_POINT('Origin',(109.09444357506,14.9047467694467,31.));
#92734=CARTESIAN_POINT('',(109.052324671575,14.7607815029093,31.));
#92735=CARTESIAN_POINT('',(109.052324671575,14.7607815029093,26.));
#92736=CARTESIAN_POINT('',(109.052324671575,14.7607815029093,28.9));
#92737=CARTESIAN_POINT('',(108.944564725307,14.3924507036097,31.));
#92738=CARTESIAN_POINT('',(108.944564725307,14.3924507036097,31.));
#92739=CARTESIAN_POINT('',(108.944564725307,14.3924507036097,26.));
#92740=CARTESIAN_POINT('',(108.944564725307,14.3924507036097,31.));
#92741=CARTESIAN_POINT('',(108.944564725307,14.3924507036097,26.));
#92742=CARTESIAN_POINT('Origin',(108.195382868896,14.702771989219,31.));
#92743=CARTESIAN_POINT('',(108.379634286055,15.0394189838697,26.));
#92744=CARTESIAN_POINT('',(108.379634286055,15.0394189838697,31.));
#92745=CARTESIAN_POINT('',(108.379634286055,15.0394189838697,28.9));
#92746=CARTESIAN_POINT('',(108.195382868896,14.702771989219,26.));
#92747=CARTESIAN_POINT('',(108.451650540008,15.1710003623644,26.));
#92748=CARTESIAN_POINT('',(108.195382868896,14.702771989219,31.));
#92749=CARTESIAN_POINT('',(108.195382868896,14.702771989219,31.));
#92750=CARTESIAN_POINT('',(108.451650540008,15.1710003623644,31.));
#92751=CARTESIAN_POINT('Ctrl Pts',(108.145858377777,13.8997367347037,31.));
#92752=CARTESIAN_POINT('Ctrl Pts',(108.145858377777,13.8997367347037,26.));
#92753=CARTESIAN_POINT('Ctrl Pts',(108.14473177199,13.9069480980004,31.));
#92754=CARTESIAN_POINT('Ctrl Pts',(108.14473177199,13.9069480980004,26.));
#92755=CARTESIAN_POINT('Ctrl Pts',(108.14253438479,13.9213259759795,31.));
#92756=CARTESIAN_POINT('Ctrl Pts',(108.14253438479,13.9213259759795,26.));
#92757=CARTESIAN_POINT('Ctrl Pts',(108.139405776934,13.9427582473116,31.));
#92758=CARTESIAN_POINT('Ctrl Pts',(108.139405776934,13.9427582473116,26.));
#92759=CARTESIAN_POINT('Ctrl Pts',(108.135569853724,13.9710650288043,31.));
#92760=CARTESIAN_POINT('Ctrl Pts',(108.135569853724,13.9710650288043,26.));
#92761=CARTESIAN_POINT('Ctrl Pts',(108.131337578061,14.005995880259,31.));
#92762=CARTESIAN_POINT('Ctrl Pts',(108.131337578061,14.005995880259,26.));
#92763=CARTESIAN_POINT('Ctrl Pts',(108.127671920245,14.0404690398857,31.));
#92764=CARTESIAN_POINT('Ctrl Pts',(108.127671920245,14.0404690398857,26.));
#92765=CARTESIAN_POINT('Ctrl Pts',(108.124576114257,14.0744781941125,31.));
#92766=CARTESIAN_POINT('Ctrl Pts',(108.124576114257,14.0744781941125,26.));
#92767=CARTESIAN_POINT('Ctrl Pts',(108.122051296587,14.1080161789411,31.));
#92768=CARTESIAN_POINT('Ctrl Pts',(108.122051296587,14.1080161789411,26.));
#92769=CARTESIAN_POINT('Ctrl Pts',(108.120094755478,14.141075848522,31.));
#92770=CARTESIAN_POINT('Ctrl Pts',(108.120094755478,14.141075848522,26.));
#92771=CARTESIAN_POINT('Ctrl Pts',(108.118699969367,14.1736486380529,31.));
#92772=CARTESIAN_POINT('Ctrl Pts',(108.118699969367,14.1736486380529,26.));
#92773=CARTESIAN_POINT('Ctrl Pts',(108.117857140196,14.2057226050197,31.));
#92774=CARTESIAN_POINT('Ctrl Pts',(108.117857140196,14.2057226050197,26.));
#92775=CARTESIAN_POINT('Ctrl Pts',(108.11755334977,14.2372805163279,31.));
#92776=CARTESIAN_POINT('Ctrl Pts',(108.11755334977,14.2372805163279,26.));
#92777=CARTESIAN_POINT('Ctrl Pts',(108.117772886125,14.2682984546298,31.));
#92778=CARTESIAN_POINT('Ctrl Pts',(108.117772886125,14.2682984546298,26.));
#92779=CARTESIAN_POINT('Ctrl Pts',(108.118496961781,14.2987431062216,31.));
#92780=CARTESIAN_POINT('Ctrl Pts',(108.118496961781,14.2987431062216,26.));
#92781=CARTESIAN_POINT('Ctrl Pts',(108.119705321862,14.3285749073991,31.));
#92782=CARTESIAN_POINT('Ctrl Pts',(108.119705321862,14.3285749073991,26.));
#92783=CARTESIAN_POINT('Ctrl Pts',(108.121378863878,14.3577546057035,31.));
#92784=CARTESIAN_POINT('Ctrl Pts',(108.121378863878,14.3577546057035,26.));
#92785=CARTESIAN_POINT('Ctrl Pts',(108.123502124645,14.3862495604353,31.));
#92786=CARTESIAN_POINT('Ctrl Pts',(108.123502124645,14.3862495604353,26.));
#92787=CARTESIAN_POINT('Ctrl Pts',(108.126065158394,14.4140388871472,31.));
#92788=CARTESIAN_POINT('Ctrl Pts',(108.126065158394,14.4140388871472,26.));
#92789=CARTESIAN_POINT('Ctrl Pts',(108.129067047035,14.4411228648582,31.));
#92790=CARTESIAN_POINT('Ctrl Pts',(108.129067047035,14.4411228648582,26.));
#92791=CARTESIAN_POINT('Ctrl Pts',(108.132512853032,14.4675164161688,31.));
#92792=CARTESIAN_POINT('Ctrl Pts',(108.132512853032,14.4675164161688,26.));
#92793=CARTESIAN_POINT('Ctrl Pts',(108.136405082654,14.4932291911838,31.));
#92794=CARTESIAN_POINT('Ctrl Pts',(108.136405082654,14.4932291911838,26.));
#92795=CARTESIAN_POINT('Ctrl Pts',(108.140736063189,14.5182483587362,31.));
#92796=CARTESIAN_POINT('Ctrl Pts',(108.140736063189,14.5182483587362,26.));
#92797=CARTESIAN_POINT('Ctrl Pts',(108.145480953033,14.5425228839262,31.));
#92798=CARTESIAN_POINT('Ctrl Pts',(108.145480953033,14.5425228839262,26.));
#92799=CARTESIAN_POINT('Ctrl Pts',(108.150587396025,14.5659407047248,31.));
#92800=CARTESIAN_POINT('Ctrl Pts',(108.150587396025,14.5659407047248,26.));
#92801=CARTESIAN_POINT('Ctrl Pts',(108.155978401035,14.5883354024226,31.));
#92802=CARTESIAN_POINT('Ctrl Pts',(108.155978401035,14.5883354024226,26.));
#92803=CARTESIAN_POINT('Ctrl Pts',(108.161565843363,14.6095165692449,31.));
#92804=CARTESIAN_POINT('Ctrl Pts',(108.161565843363,14.6095165692449,26.));
#92805=CARTESIAN_POINT('Ctrl Pts',(108.167261205399,14.6292944653163,31.));
#92806=CARTESIAN_POINT('Ctrl Pts',(108.167261205399,14.6292944653163,26.));
#92807=CARTESIAN_POINT('Ctrl Pts',(108.172986416044,14.6475048278073,31.));
#92808=CARTESIAN_POINT('Ctrl Pts',(108.172986416044,14.6475048278073,26.));
#92809=CARTESIAN_POINT('Ctrl Pts',(108.178687097234,14.6640400995864,31.));
#92810=CARTESIAN_POINT('Ctrl Pts',(108.178687097234,14.6640400995864,26.));
#92811=CARTESIAN_POINT('Ctrl Pts',(108.184331851892,14.6788459938496,31.));
#92812=CARTESIAN_POINT('Ctrl Pts',(108.184331851892,14.6788459938496,26.));
#92813=CARTESIAN_POINT('Ctrl Pts',(108.188790420063,14.6892908937643,31.));
#92814=CARTESIAN_POINT('Ctrl Pts',(108.188790420063,14.6892908937643,26.));
#92815=CARTESIAN_POINT('Ctrl Pts',(108.192099987045,14.6963371269515,31.));
#92816=CARTESIAN_POINT('Ctrl Pts',(108.192099987045,14.6963371269515,26.));
#92817=CARTESIAN_POINT('Ctrl Pts',(108.194291116197,14.7006852604777,31.));
#92818=CARTESIAN_POINT('Ctrl Pts',(108.194291116197,14.7006852604777,26.));
#92819=CARTESIAN_POINT('Ctrl Pts',(108.195382868896,14.702771989219,31.));
#92820=CARTESIAN_POINT('Ctrl Pts',(108.195382868896,14.702771989219,26.));
#92821=CARTESIAN_POINT('',(108.145858377777,13.8997367347037,31.));
#92822=CARTESIAN_POINT('Ctrl Pts',(108.195382868896,14.702771989219,31.));
#92823=CARTESIAN_POINT('Ctrl Pts',(108.194291116197,14.7006852604777,31.));
#92824=CARTESIAN_POINT('Ctrl Pts',(108.192099987045,14.6963371269515,31.));
#92825=CARTESIAN_POINT('Ctrl Pts',(108.188790420063,14.6892908937643,31.));
#92826=CARTESIAN_POINT('Ctrl Pts',(108.184331851892,14.6788459938496,31.));
#92827=CARTESIAN_POINT('Ctrl Pts',(108.178687097234,14.6640400995864,31.));
#92828=CARTESIAN_POINT('Ctrl Pts',(108.172986416044,14.6475048278073,31.));
#92829=CARTESIAN_POINT('Ctrl Pts',(108.167261205399,14.6292944653163,31.));
#92830=CARTESIAN_POINT('Ctrl Pts',(108.161565843363,14.6095165692449,31.));
#92831=CARTESIAN_POINT('Ctrl Pts',(108.155978401035,14.5883354024226,31.));
#92832=CARTESIAN_POINT('Ctrl Pts',(108.150587396025,14.5659407047248,31.));
#92833=CARTESIAN_POINT('Ctrl Pts',(108.145480953033,14.5425228839262,31.));
#92834=CARTESIAN_POINT('Ctrl Pts',(108.140736063189,14.5182483587362,31.));
#92835=CARTESIAN_POINT('Ctrl Pts',(108.136405082654,14.4932291911838,31.));
#92836=CARTESIAN_POINT('Ctrl Pts',(108.132512853032,14.4675164161688,31.));
#92837=CARTESIAN_POINT('Ctrl Pts',(108.129067047035,14.4411228648582,31.));
#92838=CARTESIAN_POINT('Ctrl Pts',(108.126065158394,14.4140388871472,31.));
#92839=CARTESIAN_POINT('Ctrl Pts',(108.123502124645,14.3862495604353,31.));
#92840=CARTESIAN_POINT('Ctrl Pts',(108.121378863878,14.3577546057035,31.));
#92841=CARTESIAN_POINT('Ctrl Pts',(108.119705321862,14.3285749073991,31.));
#92842=CARTESIAN_POINT('Ctrl Pts',(108.118496961781,14.2987431062216,31.));
#92843=CARTESIAN_POINT('Ctrl Pts',(108.117772886125,14.2682984546298,31.));
#92844=CARTESIAN_POINT('Ctrl Pts',(108.11755334977,14.2372805163279,31.));
#92845=CARTESIAN_POINT('Ctrl Pts',(108.117857140196,14.2057226050197,31.));
#92846=CARTESIAN_POINT('Ctrl Pts',(108.118699969367,14.1736486380529,31.));
#92847=CARTESIAN_POINT('Ctrl Pts',(108.120094755478,14.141075848522,31.));
#92848=CARTESIAN_POINT('Ctrl Pts',(108.122051296587,14.1080161789411,31.));
#92849=CARTESIAN_POINT('Ctrl Pts',(108.124576114257,14.0744781941125,31.));
#92850=CARTESIAN_POINT('Ctrl Pts',(108.127671920245,14.0404690398857,31.));
#92851=CARTESIAN_POINT('Ctrl Pts',(108.131337578061,14.005995880259,31.));
#92852=CARTESIAN_POINT('Ctrl Pts',(108.135569853724,13.9710650288043,31.));
#92853=CARTESIAN_POINT('Ctrl Pts',(108.139405776934,13.9427582473116,31.));
#92854=CARTESIAN_POINT('Ctrl Pts',(108.14253438479,13.9213259759795,31.));
#92855=CARTESIAN_POINT('Ctrl Pts',(108.14473177199,13.9069480980004,31.));
#92856=CARTESIAN_POINT('Ctrl Pts',(108.145858377777,13.8997367347037,31.));
#92857=CARTESIAN_POINT('',(108.145858377777,13.8997367347037,26.));
#92858=CARTESIAN_POINT('Ctrl Pts',(108.145858377777,13.8997367347037,26.));
#92859=CARTESIAN_POINT('Ctrl Pts',(108.14473177199,13.9069480980004,26.));
#92860=CARTESIAN_POINT('Ctrl Pts',(108.14253438479,13.9213259759795,26.));
#92861=CARTESIAN_POINT('Ctrl Pts',(108.139405776934,13.9427582473116,26.));
#92862=CARTESIAN_POINT('Ctrl Pts',(108.135569853724,13.9710650288043,26.));
#92863=CARTESIAN_POINT('Ctrl Pts',(108.131337578061,14.005995880259,26.));
#92864=CARTESIAN_POINT('Ctrl Pts',(108.127671920245,14.0404690398857,26.));
#92865=CARTESIAN_POINT('Ctrl Pts',(108.124576114257,14.0744781941125,26.));
#92866=CARTESIAN_POINT('Ctrl Pts',(108.122051296587,14.1080161789411,26.));
#92867=CARTESIAN_POINT('Ctrl Pts',(108.120094755478,14.141075848522,26.));
#92868=CARTESIAN_POINT('Ctrl Pts',(108.118699969367,14.1736486380529,26.));
#92869=CARTESIAN_POINT('Ctrl Pts',(108.117857140196,14.2057226050197,26.));
#92870=CARTESIAN_POINT('Ctrl Pts',(108.11755334977,14.2372805163279,26.));
#92871=CARTESIAN_POINT('Ctrl Pts',(108.117772886125,14.2682984546298,26.));
#92872=CARTESIAN_POINT('Ctrl Pts',(108.118496961781,14.2987431062216,26.));
#92873=CARTESIAN_POINT('Ctrl Pts',(108.119705321862,14.3285749073991,26.));
#92874=CARTESIAN_POINT('Ctrl Pts',(108.121378863878,14.3577546057035,26.));
#92875=CARTESIAN_POINT('Ctrl Pts',(108.123502124645,14.3862495604353,26.));
#92876=CARTESIAN_POINT('Ctrl Pts',(108.126065158394,14.4140388871472,26.));
#92877=CARTESIAN_POINT('Ctrl Pts',(108.129067047035,14.4411228648582,26.));
#92878=CARTESIAN_POINT('Ctrl Pts',(108.132512853032,14.4675164161688,26.));
#92879=CARTESIAN_POINT('Ctrl Pts',(108.136405082654,14.4932291911838,26.));
#92880=CARTESIAN_POINT('Ctrl Pts',(108.140736063189,14.5182483587362,26.));
#92881=CARTESIAN_POINT('Ctrl Pts',(108.145480953033,14.5425228839262,26.));
#92882=CARTESIAN_POINT('Ctrl Pts',(108.150587396025,14.5659407047248,26.));
#92883=CARTESIAN_POINT('Ctrl Pts',(108.155978401035,14.5883354024226,26.));
#92884=CARTESIAN_POINT('Ctrl Pts',(108.161565843363,14.6095165692449,26.));
#92885=CARTESIAN_POINT('Ctrl Pts',(108.167261205399,14.6292944653163,26.));
#92886=CARTESIAN_POINT('Ctrl Pts',(108.172986416044,14.6475048278073,26.));
#92887=CARTESIAN_POINT('Ctrl Pts',(108.178687097234,14.6640400995864,26.));
#92888=CARTESIAN_POINT('Ctrl Pts',(108.184331851892,14.6788459938496,26.));
#92889=CARTESIAN_POINT('Ctrl Pts',(108.188790420063,14.6892908937643,26.));
#92890=CARTESIAN_POINT('Ctrl Pts',(108.192099987045,14.6963371269515,26.));
#92891=CARTESIAN_POINT('Ctrl Pts',(108.194291116197,14.7006852604777,26.));
#92892=CARTESIAN_POINT('Ctrl Pts',(108.195382868896,14.702771989219,26.));
#92893=CARTESIAN_POINT('',(108.145858377777,13.8997367347037,31.));
#92894=CARTESIAN_POINT('Origin',(110.000000000001,18.0000000000028,31.));
#92895=CARTESIAN_POINT('',(108.411752154813,13.7895999261044,31.));
#92896=CARTESIAN_POINT('Origin',(110.000000000001,18.0000000000028,31.));
#92897=CARTESIAN_POINT('',(108.411752154813,13.7895999261044,26.));
#92898=CARTESIAN_POINT('Origin',(110.000000000001,18.0000000000028,26.));
#92899=CARTESIAN_POINT('',(108.411752154813,13.7895999261044,31.));
#92900=CARTESIAN_POINT('Ctrl Pts',(108.944564725307,14.3924507036097,31.));
#92901=CARTESIAN_POINT('Ctrl Pts',(108.944564725307,14.3924507036097,26.));
#92902=CARTESIAN_POINT('Ctrl Pts',(108.943861171006,14.3902031778268,31.));
#92903=CARTESIAN_POINT('Ctrl Pts',(108.943861171006,14.3902031778268,26.));
#92904=CARTESIAN_POINT('Ctrl Pts',(108.942335938597,14.3855792208381,31.));
#92905=CARTESIAN_POINT('Ctrl Pts',(108.942335938597,14.3855792208381,26.));
#92906=CARTESIAN_POINT('Ctrl Pts',(108.939693716593,14.3782565643098,31.));
#92907=CARTESIAN_POINT('Ctrl Pts',(108.939693716593,14.3782565643098,26.));
#92908=CARTESIAN_POINT('Ctrl Pts',(108.935460740827,14.3677182209614,31.));
#92909=CARTESIAN_POINT('Ctrl Pts',(108.935460740827,14.3677182209614,26.));
#92910=CARTESIAN_POINT('Ctrl Pts',(108.928982836883,14.3532574284319,31.));
#92911=CARTESIAN_POINT('Ctrl Pts',(108.928982836883,14.3532574284319,26.));
#92912=CARTESIAN_POINT('Ctrl Pts',(108.921321624393,14.3375342353073,31.));
#92913=CARTESIAN_POINT('Ctrl Pts',(108.921321624393,14.3375342353073,26.));
#92914=CARTESIAN_POINT('Ctrl Pts',(108.912493288843,14.3206092292388,31.));
#92915=CARTESIAN_POINT('Ctrl Pts',(108.912493288843,14.3206092292388,26.));
#92916=CARTESIAN_POINT('Ctrl Pts',(108.902535433517,14.3025969156976,31.));
#92917=CARTESIAN_POINT('Ctrl Pts',(108.902535433517,14.3025969156976,26.));
#92918=CARTESIAN_POINT('Ctrl Pts',(108.891509005179,14.2836686506462,31.));
#92919=CARTESIAN_POINT('Ctrl Pts',(108.891509005179,14.2836686506462,26.));
#92920=CARTESIAN_POINT('Ctrl Pts',(108.879485578779,14.2640211918396,31.));
#92921=CARTESIAN_POINT('Ctrl Pts',(108.879485578779,14.2640211918396,26.));
#92922=CARTESIAN_POINT('Ctrl Pts',(108.86653747937,14.2438514914799,31.));
#92923=CARTESIAN_POINT('Ctrl Pts',(108.86653747937,14.2438514914799,26.));
#92924=CARTESIAN_POINT('Ctrl Pts',(108.852727941796,14.2233316663176,31.));
#92925=CARTESIAN_POINT('Ctrl Pts',(108.852727941796,14.2233316663176,26.));
#92926=CARTESIAN_POINT('Ctrl Pts',(108.838099184477,14.2025779775712,31.));
#92927=CARTESIAN_POINT('Ctrl Pts',(108.838099184477,14.2025779775712,26.));
#92928=CARTESIAN_POINT('Ctrl Pts',(108.822669728866,14.1816440780331,31.));
#92929=CARTESIAN_POINT('Ctrl Pts',(108.822669728866,14.1816440780331,26.));
#92930=CARTESIAN_POINT('Ctrl Pts',(108.80644322254,14.1605444661352,31.));
#92931=CARTESIAN_POINT('Ctrl Pts',(108.80644322254,14.1605444661352,26.));
#92932=CARTESIAN_POINT('Ctrl Pts',(108.789414614043,14.1392705460246,31.));
#92933=CARTESIAN_POINT('Ctrl Pts',(108.789414614043,14.1392705460246,26.));
#92934=CARTESIAN_POINT('Ctrl Pts',(108.771576931205,14.117808186126,31.));
#92935=CARTESIAN_POINT('Ctrl Pts',(108.771576931205,14.117808186126,26.));
#92936=CARTESIAN_POINT('Ctrl Pts',(108.752929327551,14.0961578383272,31.));
#92937=CARTESIAN_POINT('Ctrl Pts',(108.752929327551,14.0961578383272,26.));
#92938=CARTESIAN_POINT('Ctrl Pts',(108.733479537902,14.0743413028801,31.));
#92939=CARTESIAN_POINT('Ctrl Pts',(108.733479537902,14.0743413028801,26.));
#92940=CARTESIAN_POINT('Ctrl Pts',(108.713239708603,14.052392594365,31.));
#92941=CARTESIAN_POINT('Ctrl Pts',(108.713239708603,14.052392594365,26.));
#92942=CARTESIAN_POINT('Ctrl Pts',(108.692224087836,14.0303529759594,31.));
#92943=CARTESIAN_POINT('Ctrl Pts',(108.692224087836,14.0303529759594,26.));
#92944=CARTESIAN_POINT('Ctrl Pts',(108.670446329005,14.008264745788,31.));
#92945=CARTESIAN_POINT('Ctrl Pts',(108.670446329005,14.008264745788,26.));
#92946=CARTESIAN_POINT('Ctrl Pts',(108.647916703691,13.9861647449546,31.));
#92947=CARTESIAN_POINT('Ctrl Pts',(108.647916703691,13.9861647449546,26.));
#92948=CARTESIAN_POINT('Ctrl Pts',(108.624641013961,13.9640809956211,31.));
#92949=CARTESIAN_POINT('Ctrl Pts',(108.624641013961,13.9640809956211,26.));
#92950=CARTESIAN_POINT('Ctrl Pts',(108.60062231089,13.9420348179765,31.));
#92951=CARTESIAN_POINT('Ctrl Pts',(108.60062231089,13.9420348179765,26.));
#92952=CARTESIAN_POINT('Ctrl Pts',(108.575862110827,13.9200415849314,31.));
#92953=CARTESIAN_POINT('Ctrl Pts',(108.575862110827,13.9200415849314,26.));
#92954=CARTESIAN_POINT('Ctrl Pts',(108.550361858556,13.8981119641586,31.));
#92955=CARTESIAN_POINT('Ctrl Pts',(108.550361858556,13.8981119641586,26.));
#92956=CARTESIAN_POINT('Ctrl Pts',(108.524124689469,13.8762529260328,31.));
#92957=CARTESIAN_POINT('Ctrl Pts',(108.524124689469,13.8762529260328,26.));
#92958=CARTESIAN_POINT('Ctrl Pts',(108.497156472931,13.8544687326315,31.));
#92959=CARTESIAN_POINT('Ctrl Pts',(108.497156472931,13.8544687326315,26.));
#92960=CARTESIAN_POINT('Ctrl Pts',(108.469463960127,13.8327615615353,31.));
#92961=CARTESIAN_POINT('Ctrl Pts',(108.469463960127,13.8327615615353,26.));
#92962=CARTESIAN_POINT('Ctrl Pts',(108.446735635703,13.8154580516872,31.));
#92963=CARTESIAN_POINT('Ctrl Pts',(108.446735635703,13.8154580516872,26.));
#92964=CARTESIAN_POINT('Ctrl Pts',(108.429368471565,13.8025154070864,31.));
#92965=CARTESIAN_POINT('Ctrl Pts',(108.429368471565,13.8025154070864,26.));
#92966=CARTESIAN_POINT('Ctrl Pts',(108.417647989244,13.7939024994221,31.));
#92967=CARTESIAN_POINT('Ctrl Pts',(108.417647989244,13.7939024994221,26.));
#92968=CARTESIAN_POINT('Ctrl Pts',(108.411752154813,13.7895999261044,31.));
#92969=CARTESIAN_POINT('Ctrl Pts',(108.411752154813,13.7895999261044,26.));
#92970=CARTESIAN_POINT('Ctrl Pts',(108.944564725307,14.3924507036097,31.));
#92971=CARTESIAN_POINT('Ctrl Pts',(108.943861171006,14.3902031778268,31.));
#92972=CARTESIAN_POINT('Ctrl Pts',(108.942335938597,14.3855792208381,31.));
#92973=CARTESIAN_POINT('Ctrl Pts',(108.939693716593,14.3782565643098,31.));
#92974=CARTESIAN_POINT('Ctrl Pts',(108.935460740827,14.3677182209614,31.));
#92975=CARTESIAN_POINT('Ctrl Pts',(108.928982836883,14.3532574284319,31.));
#92976=CARTESIAN_POINT('Ctrl Pts',(108.921321624393,14.3375342353073,31.));
#92977=CARTESIAN_POINT('Ctrl Pts',(108.912493288843,14.3206092292388,31.));
#92978=CARTESIAN_POINT('Ctrl Pts',(108.902535433517,14.3025969156976,31.));
#92979=CARTESIAN_POINT('Ctrl Pts',(108.891509005179,14.2836686506462,31.));
#92980=CARTESIAN_POINT('Ctrl Pts',(108.879485578779,14.2640211918396,31.));
#92981=CARTESIAN_POINT('Ctrl Pts',(108.86653747937,14.2438514914799,31.));
#92982=CARTESIAN_POINT('Ctrl Pts',(108.852727941796,14.2233316663176,31.));
#92983=CARTESIAN_POINT('Ctrl Pts',(108.838099184477,14.2025779775712,31.));
#92984=CARTESIAN_POINT('Ctrl Pts',(108.822669728866,14.1816440780331,31.));
#92985=CARTESIAN_POINT('Ctrl Pts',(108.80644322254,14.1605444661352,31.));
#92986=CARTESIAN_POINT('Ctrl Pts',(108.789414614043,14.1392705460246,31.));
#92987=CARTESIAN_POINT('Ctrl Pts',(108.771576931205,14.117808186126,31.));
#92988=CARTESIAN_POINT('Ctrl Pts',(108.752929327551,14.0961578383272,31.));
#92989=CARTESIAN_POINT('Ctrl Pts',(108.733479537902,14.0743413028801,31.));
#92990=CARTESIAN_POINT('Ctrl Pts',(108.713239708603,14.052392594365,31.));
#92991=CARTESIAN_POINT('Ctrl Pts',(108.692224087836,14.0303529759594,31.));
#92992=CARTESIAN_POINT('Ctrl Pts',(108.670446329005,14.008264745788,31.));
#92993=CARTESIAN_POINT('Ctrl Pts',(108.647916703691,13.9861647449546,31.));
#92994=CARTESIAN_POINT('Ctrl Pts',(108.624641013961,13.9640809956211,31.));
#92995=CARTESIAN_POINT('Ctrl Pts',(108.60062231089,13.9420348179765,31.));
#92996=CARTESIAN_POINT('Ctrl Pts',(108.575862110827,13.9200415849314,31.));
#92997=CARTESIAN_POINT('Ctrl Pts',(108.550361858556,13.8981119641586,31.));
#92998=CARTESIAN_POINT('Ctrl Pts',(108.524124689469,13.8762529260328,31.));
#92999=CARTESIAN_POINT('Ctrl Pts',(108.497156472931,13.8544687326315,31.));
#93000=CARTESIAN_POINT('Ctrl Pts',(108.469463960127,13.8327615615353,31.));
#93001=CARTESIAN_POINT('Ctrl Pts',(108.446735635703,13.8154580516872,31.));
#93002=CARTESIAN_POINT('Ctrl Pts',(108.429368471565,13.8025154070864,31.));
#93003=CARTESIAN_POINT('Ctrl Pts',(108.417647989244,13.7939024994221,31.));
#93004=CARTESIAN_POINT('Ctrl Pts',(108.411752154813,13.7895999261044,31.));
#93005=CARTESIAN_POINT('Ctrl Pts',(108.944564725307,14.3924507036097,26.));
#93006=CARTESIAN_POINT('Ctrl Pts',(108.943861171006,14.3902031778268,26.));
#93007=CARTESIAN_POINT('Ctrl Pts',(108.942335938597,14.3855792208381,26.));
#93008=CARTESIAN_POINT('Ctrl Pts',(108.939693716593,14.3782565643098,26.));
#93009=CARTESIAN_POINT('Ctrl Pts',(108.935460740827,14.3677182209614,26.));
#93010=CARTESIAN_POINT('Ctrl Pts',(108.928982836883,14.3532574284319,26.));
#93011=CARTESIAN_POINT('Ctrl Pts',(108.921321624393,14.3375342353073,26.));
#93012=CARTESIAN_POINT('Ctrl Pts',(108.912493288843,14.3206092292388,26.));
#93013=CARTESIAN_POINT('Ctrl Pts',(108.902535433517,14.3025969156976,26.));
#93014=CARTESIAN_POINT('Ctrl Pts',(108.891509005179,14.2836686506462,26.));
#93015=CARTESIAN_POINT('Ctrl Pts',(108.879485578779,14.2640211918396,26.));
#93016=CARTESIAN_POINT('Ctrl Pts',(108.86653747937,14.2438514914799,26.));
#93017=CARTESIAN_POINT('Ctrl Pts',(108.852727941796,14.2233316663176,26.));
#93018=CARTESIAN_POINT('Ctrl Pts',(108.838099184477,14.2025779775712,26.));
#93019=CARTESIAN_POINT('Ctrl Pts',(108.822669728866,14.1816440780331,26.));
#93020=CARTESIAN_POINT('Ctrl Pts',(108.80644322254,14.1605444661352,26.));
#93021=CARTESIAN_POINT('Ctrl Pts',(108.789414614043,14.1392705460246,26.));
#93022=CARTESIAN_POINT('Ctrl Pts',(108.771576931205,14.117808186126,26.));
#93023=CARTESIAN_POINT('Ctrl Pts',(108.752929327551,14.0961578383272,26.));
#93024=CARTESIAN_POINT('Ctrl Pts',(108.733479537902,14.0743413028801,26.));
#93025=CARTESIAN_POINT('Ctrl Pts',(108.713239708603,14.052392594365,26.));
#93026=CARTESIAN_POINT('Ctrl Pts',(108.692224087836,14.0303529759594,26.));
#93027=CARTESIAN_POINT('Ctrl Pts',(108.670446329005,14.008264745788,26.));
#93028=CARTESIAN_POINT('Ctrl Pts',(108.647916703691,13.9861647449546,26.));
#93029=CARTESIAN_POINT('Ctrl Pts',(108.624641013961,13.9640809956211,26.));
#93030=CARTESIAN_POINT('Ctrl Pts',(108.60062231089,13.9420348179765,26.));
#93031=CARTESIAN_POINT('Ctrl Pts',(108.575862110827,13.9200415849314,26.));
#93032=CARTESIAN_POINT('Ctrl Pts',(108.550361858556,13.8981119641586,26.));
#93033=CARTESIAN_POINT('Ctrl Pts',(108.524124689469,13.8762529260328,26.));
#93034=CARTESIAN_POINT('Ctrl Pts',(108.497156472931,13.8544687326315,26.));
#93035=CARTESIAN_POINT('Ctrl Pts',(108.469463960127,13.8327615615353,26.));
#93036=CARTESIAN_POINT('Ctrl Pts',(108.446735635703,13.8154580516872,26.));
#93037=CARTESIAN_POINT('Ctrl Pts',(108.429368471565,13.8025154070864,26.));
#93038=CARTESIAN_POINT('Ctrl Pts',(108.417647989244,13.7939024994221,26.));
#93039=CARTESIAN_POINT('Ctrl Pts',(108.411752154813,13.7895999261044,26.));
#93040=CARTESIAN_POINT('Origin',(108.52548580596,14.4402078347963,31.));
#93041=CARTESIAN_POINT('Origin',(110.,18.,31.));
#93042=CARTESIAN_POINT('Origin',(110.,18.,28.9));
#93043=CARTESIAN_POINT('',(106.625,18.,31.8));
#93044=CARTESIAN_POINT('Origin',(110.,18.,31.8));
#93045=CARTESIAN_POINT('',(106.625,18.,31.));
#93046=CARTESIAN_POINT('',(106.625,18.,28.9));
#93047=CARTESIAN_POINT('',(106.644692681757,17.6359425867508,31.));
#93048=CARTESIAN_POINT('Origin',(110.,18.,31.));
#93049=CARTESIAN_POINT('',(106.644692681757,17.6359425867508,26.));
#93050=CARTESIAN_POINT('',(106.644692681757,17.6359425867508,28.9));
#93051=CARTESIAN_POINT('',(106.760781502909,17.0523246715749,26.));
#93052=CARTESIAN_POINT('Origin',(110.,18.,26.));
#93053=CARTESIAN_POINT('',(106.760781502909,17.0523246715749,31.));
#93054=CARTESIAN_POINT('',(106.760781502909,17.0523246715749,28.9));
#93055=CARTESIAN_POINT('',(107.03941898387,16.3796342860549,31.));
#93056=CARTESIAN_POINT('Origin',(110.,18.,31.));
#93057=CARTESIAN_POINT('',(107.03941898387,16.3796342860549,26.));
#93058=CARTESIAN_POINT('',(107.03941898387,16.3796342860549,28.9));
#93059=CARTESIAN_POINT('',(107.370011976655,15.884866907955,26.));
#93060=CARTESIAN_POINT('Origin',(110.,18.,26.));
#93061=CARTESIAN_POINT('',(107.370011976655,15.884866907955,31.));
#93062=CARTESIAN_POINT('',(107.370011976655,15.884866907955,28.9));
#93063=CARTESIAN_POINT('',(107.884866907955,15.3700119766554,31.));
#93064=CARTESIAN_POINT('Origin',(110.,18.,31.));
#93065=CARTESIAN_POINT('',(107.884866907955,15.3700119766554,26.));
#93066=CARTESIAN_POINT('',(107.884866907955,15.3700119766554,28.9));
#93067=CARTESIAN_POINT('Origin',(110.,18.,26.));
#93068=CARTESIAN_POINT('',(109.635942586751,14.6446926817565,26.));
#93069=CARTESIAN_POINT('Origin',(110.,18.,26.));
#93070=CARTESIAN_POINT('',(109.635942586751,14.6446926817565,31.));
#93071=CARTESIAN_POINT('',(109.635942586751,14.6446926817565,28.9));
#93072=CARTESIAN_POINT('',(110.364057413249,14.6446926817565,31.));
#93073=CARTESIAN_POINT('Origin',(110.,18.,31.));
#93074=CARTESIAN_POINT('',(110.364057413249,14.6446926817565,26.));
#93075=CARTESIAN_POINT('',(110.364057413249,14.6446926817565,28.9));
#93076=CARTESIAN_POINT('',(110.947675328425,14.7607815029093,26.));
#93077=CARTESIAN_POINT('Origin',(110.,18.,26.));
#93078=CARTESIAN_POINT('',(110.947675328425,14.7607815029093,31.));
#93079=CARTESIAN_POINT('',(110.947675328425,14.7607815029093,28.9));
#93080=CARTESIAN_POINT('',(111.620365713945,15.0394189838697,31.));
#93081=CARTESIAN_POINT('Origin',(110.,18.,31.));
#93082=CARTESIAN_POINT('',(111.620365713945,15.0394189838697,26.));
#93083=CARTESIAN_POINT('',(111.620365713945,15.0394189838697,28.9));
#93084=CARTESIAN_POINT('',(112.115133092045,15.3700119766554,26.));
#93085=CARTESIAN_POINT('Origin',(110.,18.,26.));
#93086=CARTESIAN_POINT('',(112.115133092045,15.3700119766554,31.));
#93087=CARTESIAN_POINT('',(112.115133092045,15.3700119766554,28.9));
#93088=CARTESIAN_POINT('',(112.629988023345,15.884866907955,31.));
#93089=CARTESIAN_POINT('Origin',(110.,18.,31.));
#93090=CARTESIAN_POINT('',(112.629988023345,15.884866907955,26.));
#93091=CARTESIAN_POINT('',(112.629988023345,15.884866907955,28.9));
#93092=CARTESIAN_POINT('',(112.96058101613,16.3796342860549,26.));
#93093=CARTESIAN_POINT('Origin',(110.,18.,26.));
#93094=CARTESIAN_POINT('',(112.96058101613,16.3796342860549,31.));
#93095=CARTESIAN_POINT('',(112.96058101613,16.3796342860549,28.9));
#93096=CARTESIAN_POINT('',(113.239218497091,17.0523246715749,31.));
#93097=CARTESIAN_POINT('Origin',(110.,18.,31.));
#93098=CARTESIAN_POINT('',(113.239218497091,17.0523246715749,26.));
#93099=CARTESIAN_POINT('',(113.239218497091,17.0523246715749,28.9));
#93100=CARTESIAN_POINT('',(113.355307318243,17.6359425867508,26.));
#93101=CARTESIAN_POINT('Origin',(110.,18.,26.));
#93102=CARTESIAN_POINT('',(113.355307318243,17.6359425867508,31.));
#93103=CARTESIAN_POINT('',(113.355307318243,17.6359425867508,28.9));
#93104=CARTESIAN_POINT('',(113.355307318243,18.3640574132493,31.));
#93105=CARTESIAN_POINT('Origin',(110.,18.,31.));
#93106=CARTESIAN_POINT('',(113.355307318243,18.3640574132493,26.));
#93107=CARTESIAN_POINT('',(113.355307318243,18.3640574132493,28.9));
#93108=CARTESIAN_POINT('',(113.239218497091,18.9476753284251,26.));
#93109=CARTESIAN_POINT('Origin',(110.,18.,26.));
#93110=CARTESIAN_POINT('',(113.239218497091,18.9476753284251,31.));
#93111=CARTESIAN_POINT('',(113.239218497091,18.9476753284251,28.9));
#93112=CARTESIAN_POINT('',(112.96058101613,19.6203657139451,31.));
#93113=CARTESIAN_POINT('Origin',(110.,18.,31.));
#93114=CARTESIAN_POINT('',(112.96058101613,19.6203657139451,26.));
#93115=CARTESIAN_POINT('',(112.96058101613,19.6203657139451,28.9));
#93116=CARTESIAN_POINT('',(112.629988023345,20.115133092045,26.));
#93117=CARTESIAN_POINT('Origin',(110.,18.,26.));
#93118=CARTESIAN_POINT('',(112.629988023345,20.115133092045,31.));
#93119=CARTESIAN_POINT('',(112.629988023345,20.115133092045,28.9));
#93120=CARTESIAN_POINT('',(112.115133092045,20.6299880233446,31.));
#93121=CARTESIAN_POINT('Origin',(110.,18.,31.));
#93122=CARTESIAN_POINT('',(112.115133092045,20.6299880233446,26.));
#93123=CARTESIAN_POINT('',(112.115133092045,20.6299880233446,28.9));
#93124=CARTESIAN_POINT('',(111.620365713945,20.9605810161303,26.));
#93125=CARTESIAN_POINT('Origin',(110.,18.,26.));
#93126=CARTESIAN_POINT('',(111.620365713945,20.9605810161303,31.));
#93127=CARTESIAN_POINT('',(111.620365713945,20.9605810161303,28.9));
#93128=CARTESIAN_POINT('',(110.947675328425,21.2392184970907,31.));
#93129=CARTESIAN_POINT('Origin',(110.,18.,31.));
#93130=CARTESIAN_POINT('',(110.947675328425,21.2392184970907,26.));
#93131=CARTESIAN_POINT('',(110.947675328425,21.2392184970907,28.9));
#93132=CARTESIAN_POINT('',(110.364057413249,21.3553073182435,26.));
#93133=CARTESIAN_POINT('Origin',(110.,18.,26.));
#93134=CARTESIAN_POINT('',(110.364057413249,21.3553073182435,31.));
#93135=CARTESIAN_POINT('',(110.364057413249,21.3553073182435,28.9));
#93136=CARTESIAN_POINT('',(109.635942586751,21.3553073182435,31.));
#93137=CARTESIAN_POINT('Origin',(110.,18.,31.));
#93138=CARTESIAN_POINT('',(109.635942586751,21.3553073182435,26.));
#93139=CARTESIAN_POINT('',(109.635942586751,21.3553073182435,28.9));
#93140=CARTESIAN_POINT('',(109.052324671575,21.2392184970907,26.));
#93141=CARTESIAN_POINT('Origin',(110.,18.,26.));
#93142=CARTESIAN_POINT('',(109.052324671575,21.2392184970907,31.));
#93143=CARTESIAN_POINT('',(109.052324671575,21.2392184970907,28.9));
#93144=CARTESIAN_POINT('',(108.379634286055,20.9605810161303,31.));
#93145=CARTESIAN_POINT('Origin',(110.,18.,31.));
#93146=CARTESIAN_POINT('',(108.379634286055,20.9605810161303,26.));
#93147=CARTESIAN_POINT('',(108.379634286055,20.9605810161303,28.9));
#93148=CARTESIAN_POINT('',(107.884866907955,20.6299880233446,26.));
#93149=CARTESIAN_POINT('Origin',(110.,18.,26.));
#93150=CARTESIAN_POINT('',(107.884866907955,20.6299880233446,31.));
#93151=CARTESIAN_POINT('',(107.884866907955,20.6299880233446,28.9));
#93152=CARTESIAN_POINT('',(107.370011976655,20.115133092045,31.));
#93153=CARTESIAN_POINT('Origin',(110.,18.,31.));
#93154=CARTESIAN_POINT('',(107.370011976655,20.115133092045,26.));
#93155=CARTESIAN_POINT('',(107.370011976655,20.115133092045,28.9));
#93156=CARTESIAN_POINT('',(107.03941898387,19.6203657139451,26.));
#93157=CARTESIAN_POINT('Origin',(110.,18.,26.));
#93158=CARTESIAN_POINT('',(107.03941898387,19.6203657139451,31.));
#93159=CARTESIAN_POINT('',(107.03941898387,19.6203657139451,28.9));
#93160=CARTESIAN_POINT('',(106.760781502909,18.9476753284252,31.));
#93161=CARTESIAN_POINT('Origin',(110.,18.,31.));
#93162=CARTESIAN_POINT('',(106.760781502909,18.9476753284252,26.));
#93163=CARTESIAN_POINT('',(106.760781502909,18.9476753284252,28.9));
#93164=CARTESIAN_POINT('',(106.644692681757,18.3640574132493,26.));
#93165=CARTESIAN_POINT('Origin',(110.,18.,26.));
#93166=CARTESIAN_POINT('',(106.644692681757,18.3640574132493,31.));
#93167=CARTESIAN_POINT('',(106.644692681757,18.3640574132493,28.9));
#93168=CARTESIAN_POINT('Origin',(110.,18.,31.));
#93169=CARTESIAN_POINT('Origin',(107.978872823157,15.4869003332485,31.));
#93170=CARTESIAN_POINT('',(107.644355604652,15.0709566360981,31.));
#93171=CARTESIAN_POINT('',(107.644355604652,15.0709566360981,31.));
#93172=CARTESIAN_POINT('',(107.644355604652,15.0709566360981,26.));
#93173=CARTESIAN_POINT('',(107.644355604652,15.0709566360981,31.));
#93174=CARTESIAN_POINT('',(107.644355604652,15.0709566360981,26.));
#93175=CARTESIAN_POINT('Origin',(107.070956636098,15.6443556046521,31.));
#93176=CARTESIAN_POINT('',(107.070956636098,15.6443556046521,26.));
#93177=CARTESIAN_POINT('',(107.486900333248,15.978872823157,26.));
#93178=CARTESIAN_POINT('',(107.070956636098,15.6443556046521,31.));
#93179=CARTESIAN_POINT('',(107.070956636098,15.6443556046521,31.));
#93180=CARTESIAN_POINT('',(107.486900333248,15.978872823157,31.));
#93181=CARTESIAN_POINT('Ctrl Pts',(106.717893684886,14.9213999713683,31.));
#93182=CARTESIAN_POINT('Ctrl Pts',(106.717893684886,14.9213999713683,26.));
#93183=CARTESIAN_POINT('Ctrl Pts',(106.719612506117,14.9284935356891,31.));
#93184=CARTESIAN_POINT('Ctrl Pts',(106.719612506117,14.9284935356891,26.));
#93185=CARTESIAN_POINT('Ctrl Pts',(106.723084560754,14.9426178665506,31.));
#93186=CARTESIAN_POINT('Ctrl Pts',(106.723084560754,14.9426178665506,26.));
#93187=CARTESIAN_POINT('Ctrl Pts',(106.728395879147,14.9636159697624,31.));
#93188=CARTESIAN_POINT('Ctrl Pts',(106.728395879147,14.9636159697624,26.));
#93189=CARTESIAN_POINT('Ctrl Pts',(106.735684484505,14.9912359700753,31.));
#93190=CARTESIAN_POINT('Ctrl Pts',(106.735684484505,14.9912359700753,26.));
#93191=CARTESIAN_POINT('Ctrl Pts',(106.745141829775,15.0251274905646,31.));
#93192=CARTESIAN_POINT('Ctrl Pts',(106.745141829775,15.0251274905646,26.));
#93193=CARTESIAN_POINT('Ctrl Pts',(106.754947510596,15.0583793236798,31.));
#93194=CARTESIAN_POINT('Ctrl Pts',(106.754947510596,15.0583793236798,26.));
#93195=CARTESIAN_POINT('Ctrl Pts',(106.765102098678,15.0909843988495,31.));
#93196=CARTESIAN_POINT('Ctrl Pts',(106.765102098678,15.0909843988495,26.));
#93197=CARTESIAN_POINT('Ctrl Pts',(106.775603902459,15.1229356624862,31.));
#93198=CARTESIAN_POINT('Ctrl Pts',(106.775603902459,15.1229356624862,26.));
#93199=CARTESIAN_POINT('Ctrl Pts',(106.786447682002,15.1542275504307,31.));
#93200=CARTESIAN_POINT('Ctrl Pts',(106.786447682002,15.1542275504307,26.));
#93201=CARTESIAN_POINT('Ctrl Pts',(106.79762413456,15.1848546455316,31.));
#93202=CARTESIAN_POINT('Ctrl Pts',(106.79762413456,15.1848546455316,26.));
#93203=CARTESIAN_POINT('Ctrl Pts',(106.809119637709,15.2148096638986,31.));
#93204=CARTESIAN_POINT('Ctrl Pts',(106.809119637709,15.2148096638986,26.));
#93205=CARTESIAN_POINT('Ctrl Pts',(106.82091566177,15.244081627808,31.));
#93206=CARTESIAN_POINT('Ctrl Pts',(106.82091566177,15.244081627808,26.));
#93207=CARTESIAN_POINT('Ctrl Pts',(106.832988538009,15.2726544532201,31.));
#93208=CARTESIAN_POINT('Ctrl Pts',(106.832988538009,15.2726544532201,26.));
#93209=CARTESIAN_POINT('Ctrl Pts',(106.845308160455,15.3005045519429,31.));
#93210=CARTESIAN_POINT('Ctrl Pts',(106.845308160455,15.3005045519429,26.));
#93211=CARTESIAN_POINT('Ctrl Pts',(106.85784067567,15.3276031230855,31.));
#93212=CARTESIAN_POINT('Ctrl Pts',(106.85784067567,15.3276031230855,26.));
#93213=CARTESIAN_POINT('Ctrl Pts',(106.870553413989,15.3539212123107,31.));
#93214=CARTESIAN_POINT('Ctrl Pts',(106.870553413989,15.3539212123107,26.));
#93215=CARTESIAN_POINT('Ctrl Pts',(106.883419598235,15.379434581049,31.));
#93216=CARTESIAN_POINT('Ctrl Pts',(106.883419598235,15.379434581049,26.));
#93217=CARTESIAN_POINT('Ctrl Pts',(106.896422047586,15.4041277406684,31.));
#93218=CARTESIAN_POINT('Ctrl Pts',(106.896422047586,15.4041277406684,26.));
#93219=CARTESIAN_POINT('Ctrl Pts',(106.909560020613,15.4280013002857,31.));
#93220=CARTESIAN_POINT('Ctrl Pts',(106.909560020613,15.4280013002857,26.));
#93221=CARTESIAN_POINT('Ctrl Pts',(106.922843905055,15.4510671092656,31.));
#93222=CARTESIAN_POINT('Ctrl Pts',(106.922843905055,15.4510671092656,26.));
#93223=CARTESIAN_POINT('Ctrl Pts',(106.936279709336,15.4733331240349,31.));
#93224=CARTESIAN_POINT('Ctrl Pts',(106.936279709336,15.4733331240349,26.));
#93225=CARTESIAN_POINT('Ctrl Pts',(106.949855434522,15.4947904263603,31.));
#93226=CARTESIAN_POINT('Ctrl Pts',(106.949855434522,15.4947904263603,26.));
#93227=CARTESIAN_POINT('Ctrl Pts',(106.963528599752,15.5154013726131,31.));
#93228=CARTESIAN_POINT('Ctrl Pts',(106.963528599752,15.5154013726131,26.));
#93229=CARTESIAN_POINT('Ctrl Pts',(106.977207949958,15.5350824668136,31.));
#93230=CARTESIAN_POINT('Ctrl Pts',(106.977207949958,15.5350824668136,26.));
#93231=CARTESIAN_POINT('Ctrl Pts',(106.990758668928,15.5537094213523,31.));
#93232=CARTESIAN_POINT('Ctrl Pts',(106.990758668928,15.5537094213523,26.));
#93233=CARTESIAN_POINT('Ctrl Pts',(107.004026474155,15.5711400462457,31.));
#93234=CARTESIAN_POINT('Ctrl Pts',(107.004026474155,15.5711400462457,26.));
#93235=CARTESIAN_POINT('Ctrl Pts',(107.016856975724,15.5872329189297,31.));
#93236=CARTESIAN_POINT('Ctrl Pts',(107.016856975724,15.5872329189297,26.));
#93237=CARTESIAN_POINT('Ctrl Pts',(107.029115184681,15.6018661568543,31.));
#93238=CARTESIAN_POINT('Ctrl Pts',(107.029115184681,15.6018661568543,26.));
#93239=CARTESIAN_POINT('Ctrl Pts',(107.040709701913,15.6149611997708,31.));
#93240=CARTESIAN_POINT('Ctrl Pts',(107.040709701913,15.6149611997708,26.));
#93241=CARTESIAN_POINT('Ctrl Pts',(107.051590745644,15.6264799083536,31.));
#93242=CARTESIAN_POINT('Ctrl Pts',(107.051590745644,15.6264799083536,26.));
#93243=CARTESIAN_POINT('Ctrl Pts',(107.059707015671,15.6344235174329,31.));
#93244=CARTESIAN_POINT('Ctrl Pts',(107.059707015671,15.6344235174329,26.));
#93245=CARTESIAN_POINT('Ctrl Pts',(107.065461133568,15.6396668716037,31.));
#93246=CARTESIAN_POINT('Ctrl Pts',(107.065461133568,15.6396668716037,26.));
#93247=CARTESIAN_POINT('Ctrl Pts',(107.069149431608,15.6428455143482,31.));
#93248=CARTESIAN_POINT('Ctrl Pts',(107.069149431608,15.6428455143482,26.));
#93249=CARTESIAN_POINT('Ctrl Pts',(107.070956636098,15.6443556046521,31.));
#93250=CARTESIAN_POINT('Ctrl Pts',(107.070956636098,15.6443556046521,26.));
#93251=CARTESIAN_POINT('',(106.717893684886,14.9213999713683,31.));
#93252=CARTESIAN_POINT('Ctrl Pts',(107.070956636098,15.6443556046521,31.));
#93253=CARTESIAN_POINT('Ctrl Pts',(107.069149431608,15.6428455143482,31.));
#93254=CARTESIAN_POINT('Ctrl Pts',(107.065461133568,15.6396668716037,31.));
#93255=CARTESIAN_POINT('Ctrl Pts',(107.059707015671,15.6344235174329,31.));
#93256=CARTESIAN_POINT('Ctrl Pts',(107.051590745644,15.6264799083536,31.));
#93257=CARTESIAN_POINT('Ctrl Pts',(107.040709701913,15.6149611997708,31.));
#93258=CARTESIAN_POINT('Ctrl Pts',(107.029115184681,15.6018661568543,31.));
#93259=CARTESIAN_POINT('Ctrl Pts',(107.016856975724,15.5872329189297,31.));
#93260=CARTESIAN_POINT('Ctrl Pts',(107.004026474155,15.5711400462457,31.));
#93261=CARTESIAN_POINT('Ctrl Pts',(106.990758668928,15.5537094213523,31.));
#93262=CARTESIAN_POINT('Ctrl Pts',(106.977207949958,15.5350824668136,31.));
#93263=CARTESIAN_POINT('Ctrl Pts',(106.963528599752,15.5154013726131,31.));
#93264=CARTESIAN_POINT('Ctrl Pts',(106.949855434522,15.4947904263603,31.));
#93265=CARTESIAN_POINT('Ctrl Pts',(106.936279709336,15.4733331240349,31.));
#93266=CARTESIAN_POINT('Ctrl Pts',(106.922843905055,15.4510671092656,31.));
#93267=CARTESIAN_POINT('Ctrl Pts',(106.909560020613,15.4280013002857,31.));
#93268=CARTESIAN_POINT('Ctrl Pts',(106.896422047586,15.4041277406684,31.));
#93269=CARTESIAN_POINT('Ctrl Pts',(106.883419598235,15.379434581049,31.));
#93270=CARTESIAN_POINT('Ctrl Pts',(106.870553413989,15.3539212123107,31.));
#93271=CARTESIAN_POINT('Ctrl Pts',(106.85784067567,15.3276031230855,31.));
#93272=CARTESIAN_POINT('Ctrl Pts',(106.845308160455,15.3005045519429,31.));
#93273=CARTESIAN_POINT('Ctrl Pts',(106.832988538009,15.2726544532201,31.));
#93274=CARTESIAN_POINT('Ctrl Pts',(106.82091566177,15.244081627808,31.));
#93275=CARTESIAN_POINT('Ctrl Pts',(106.809119637709,15.2148096638986,31.));
#93276=CARTESIAN_POINT('Ctrl Pts',(106.79762413456,15.1848546455316,31.));
#93277=CARTESIAN_POINT('Ctrl Pts',(106.786447682002,15.1542275504307,31.));
#93278=CARTESIAN_POINT('Ctrl Pts',(106.775603902459,15.1229356624862,31.));
#93279=CARTESIAN_POINT('Ctrl Pts',(106.765102098678,15.0909843988495,31.));
#93280=CARTESIAN_POINT('Ctrl Pts',(106.754947510596,15.0583793236798,31.));
#93281=CARTESIAN_POINT('Ctrl Pts',(106.745141829775,15.0251274905646,31.));
#93282=CARTESIAN_POINT('Ctrl Pts',(106.735684484505,14.9912359700753,31.));
#93283=CARTESIAN_POINT('Ctrl Pts',(106.728395879147,14.9636159697624,31.));
#93284=CARTESIAN_POINT('Ctrl Pts',(106.723084560754,14.9426178665506,31.));
#93285=CARTESIAN_POINT('Ctrl Pts',(106.719612506117,14.9284935356891,31.));
#93286=CARTESIAN_POINT('Ctrl Pts',(106.717893684886,14.9213999713683,31.));
#93287=CARTESIAN_POINT('',(106.717893684886,14.9213999713683,26.));
#93288=CARTESIAN_POINT('Ctrl Pts',(106.717893684886,14.9213999713683,26.));
#93289=CARTESIAN_POINT('Ctrl Pts',(106.719612506117,14.9284935356891,26.));
#93290=CARTESIAN_POINT('Ctrl Pts',(106.723084560754,14.9426178665506,26.));
#93291=CARTESIAN_POINT('Ctrl Pts',(106.728395879147,14.9636159697624,26.));
#93292=CARTESIAN_POINT('Ctrl Pts',(106.735684484505,14.9912359700753,26.));
#93293=CARTESIAN_POINT('Ctrl Pts',(106.745141829775,15.0251274905646,26.));
#93294=CARTESIAN_POINT('Ctrl Pts',(106.754947510596,15.0583793236798,26.));
#93295=CARTESIAN_POINT('Ctrl Pts',(106.765102098678,15.0909843988495,26.));
#93296=CARTESIAN_POINT('Ctrl Pts',(106.775603902459,15.1229356624862,26.));
#93297=CARTESIAN_POINT('Ctrl Pts',(106.786447682002,15.1542275504307,26.));
#93298=CARTESIAN_POINT('Ctrl Pts',(106.79762413456,15.1848546455316,26.));
#93299=CARTESIAN_POINT('Ctrl Pts',(106.809119637709,15.2148096638986,26.));
#93300=CARTESIAN_POINT('Ctrl Pts',(106.82091566177,15.244081627808,26.));
#93301=CARTESIAN_POINT('Ctrl Pts',(106.832988538009,15.2726544532201,26.));
#93302=CARTESIAN_POINT('Ctrl Pts',(106.845308160455,15.3005045519429,26.));
#93303=CARTESIAN_POINT('Ctrl Pts',(106.85784067567,15.3276031230855,26.));
#93304=CARTESIAN_POINT('Ctrl Pts',(106.870553413989,15.3539212123107,26.));
#93305=CARTESIAN_POINT('Ctrl Pts',(106.883419598235,15.379434581049,26.));
#93306=CARTESIAN_POINT('Ctrl Pts',(106.896422047586,15.4041277406684,26.));
#93307=CARTESIAN_POINT('Ctrl Pts',(106.909560020613,15.4280013002857,26.));
#93308=CARTESIAN_POINT('Ctrl Pts',(106.922843905055,15.4510671092656,26.));
#93309=CARTESIAN_POINT('Ctrl Pts',(106.936279709336,15.4733331240349,26.));
#93310=CARTESIAN_POINT('Ctrl Pts',(106.949855434522,15.4947904263603,26.));
#93311=CARTESIAN_POINT('Ctrl Pts',(106.963528599752,15.5154013726131,26.));
#93312=CARTESIAN_POINT('Ctrl Pts',(106.977207949958,15.5350824668136,26.));
#93313=CARTESIAN_POINT('Ctrl Pts',(106.990758668928,15.5537094213523,26.));
#93314=CARTESIAN_POINT('Ctrl Pts',(107.004026474155,15.5711400462457,26.));
#93315=CARTESIAN_POINT('Ctrl Pts',(107.016856975724,15.5872329189297,26.));
#93316=CARTESIAN_POINT('Ctrl Pts',(107.029115184681,15.6018661568543,26.));
#93317=CARTESIAN_POINT('Ctrl Pts',(107.040709701913,15.6149611997708,26.));
#93318=CARTESIAN_POINT('Ctrl Pts',(107.051590745644,15.6264799083536,26.));
#93319=CARTESIAN_POINT('Ctrl Pts',(107.059707015671,15.6344235174329,26.));
#93320=CARTESIAN_POINT('Ctrl Pts',(107.065461133568,15.6396668716037,26.));
#93321=CARTESIAN_POINT('Ctrl Pts',(107.069149431608,15.6428455143482,26.));
#93322=CARTESIAN_POINT('Ctrl Pts',(107.070956636098,15.6443556046521,26.));
#93323=CARTESIAN_POINT('',(106.717893684886,14.9213999713683,31.));
#93324=CARTESIAN_POINT('Origin',(110.000000000002,18.0000000000022,31.));
#93325=CARTESIAN_POINT('',(106.921399971368,14.7178936848864,31.));
#93326=CARTESIAN_POINT('Origin',(110.000000000002,18.0000000000022,31.));
#93327=CARTESIAN_POINT('',(106.921399971368,14.7178936848864,26.));
#93328=CARTESIAN_POINT('Origin',(110.000000000002,18.0000000000022,26.));
#93329=CARTESIAN_POINT('',(106.921399971368,14.7178936848864,31.));
#93330=CARTESIAN_POINT('Ctrl Pts',(107.644355604652,15.0709566360981,31.));
#93331=CARTESIAN_POINT('Ctrl Pts',(107.644355604652,15.0709566360981,26.));
#93332=CARTESIAN_POINT('Ctrl Pts',(107.642845514352,15.0691494316033,31.));
#93333=CARTESIAN_POINT('Ctrl Pts',(107.642845514352,15.0691494316033,26.));
#93334=CARTESIAN_POINT('Ctrl Pts',(107.639666871615,15.0654611335559,31.));
#93335=CARTESIAN_POINT('Ctrl Pts',(107.639666871615,15.0654611335559,26.));
#93336=CARTESIAN_POINT('Ctrl Pts',(107.634423517451,15.0597070156512,31.));
#93337=CARTESIAN_POINT('Ctrl Pts',(107.634423517451,15.0597070156512,26.));
#93338=CARTESIAN_POINT('Ctrl Pts',(107.626479908375,15.0515907456204,31.));
#93339=CARTESIAN_POINT('Ctrl Pts',(107.626479908375,15.0515907456204,26.));
#93340=CARTESIAN_POINT('Ctrl Pts',(107.614961199788,15.0407097018941,31.));
#93341=CARTESIAN_POINT('Ctrl Pts',(107.614961199788,15.0407097018941,26.));
#93342=CARTESIAN_POINT('Ctrl Pts',(107.601866156862,15.0291151846723,31.));
#93343=CARTESIAN_POINT('Ctrl Pts',(107.601866156862,15.0291151846723,26.));
#93344=CARTESIAN_POINT('Ctrl Pts',(107.587232918926,15.0168569757285,31.));
#93345=CARTESIAN_POINT('Ctrl Pts',(107.587232918926,15.0168569757285,26.));
#93346=CARTESIAN_POINT('Ctrl Pts',(107.571140046232,15.0040264741695,31.));
#93347=CARTESIAN_POINT('Ctrl Pts',(107.571140046232,15.0040264741695,26.));
#93348=CARTESIAN_POINT('Ctrl Pts',(107.553709421335,14.9907586689459,31.));
#93349=CARTESIAN_POINT('Ctrl Pts',(107.553709421335,14.9907586689459,26.));
#93350=CARTESIAN_POINT('Ctrl Pts',(107.5350824668,14.9772079499723,31.));
#93351=CARTESIAN_POINT('Ctrl Pts',(107.5350824668,14.9772079499723,26.));
#93352=CARTESIAN_POINT('Ctrl Pts',(107.515401372608,14.9635285997574,31.));
#93353=CARTESIAN_POINT('Ctrl Pts',(107.515401372608,14.9635285997574,26.));
#93354=CARTESIAN_POINT('Ctrl Pts',(107.494790426365,14.9498554345175,31.));
#93355=CARTESIAN_POINT('Ctrl Pts',(107.494790426365,14.9498554345175,26.));
#93356=CARTESIAN_POINT('Ctrl Pts',(107.473333124048,14.9362797093226,31.));
#93357=CARTESIAN_POINT('Ctrl Pts',(107.473333124048,14.9362797093226,26.));
#93358=CARTESIAN_POINT('Ctrl Pts',(107.451067109284,14.9228439050363,31.));
#93359=CARTESIAN_POINT('Ctrl Pts',(107.451067109284,14.9228439050363,26.));
#93360=CARTESIAN_POINT('Ctrl Pts',(107.428001300302,14.9095600205959,31.));
#93361=CARTESIAN_POINT('Ctrl Pts',(107.428001300302,14.9095600205959,26.));
#93362=CARTESIAN_POINT('Ctrl Pts',(107.404127740676,14.8964220475778,31.));
#93363=CARTESIAN_POINT('Ctrl Pts',(107.404127740676,14.8964220475778,26.));
#93364=CARTESIAN_POINT('Ctrl Pts',(107.379434581043,14.8834195982418,31.));
#93365=CARTESIAN_POINT('Ctrl Pts',(107.379434581043,14.8834195982418,26.));
#93366=CARTESIAN_POINT('Ctrl Pts',(107.353921212289,14.8705534140105,31.));
#93367=CARTESIAN_POINT('Ctrl Pts',(107.353921212289,14.8705534140105,26.));
#93368=CARTESIAN_POINT('Ctrl Pts',(107.327603123054,14.8578406757021,31.));
#93369=CARTESIAN_POINT('Ctrl Pts',(107.327603123054,14.8578406757021,26.));
#93370=CARTESIAN_POINT('Ctrl Pts',(107.300504551911,14.8453081604869,31.));
#93371=CARTESIAN_POINT('Ctrl Pts',(107.300504551911,14.8453081604869,26.));
#93372=CARTESIAN_POINT('Ctrl Pts',(107.272654453203,14.8329885380258,31.));
#93373=CARTESIAN_POINT('Ctrl Pts',(107.272654453203,14.8329885380258,26.));
#93374=CARTESIAN_POINT('Ctrl Pts',(107.244081627818,14.8209156617599,31.));
#93375=CARTESIAN_POINT('Ctrl Pts',(107.244081627818,14.8209156617599,26.));
#93376=CARTESIAN_POINT('Ctrl Pts',(107.214809663941,14.8091196376662,31.));
#93377=CARTESIAN_POINT('Ctrl Pts',(107.214809663941,14.8091196376662,26.));
#93378=CARTESIAN_POINT('Ctrl Pts',(107.1848546456,14.7976241344926,31.));
#93379=CARTESIAN_POINT('Ctrl Pts',(107.1848546456,14.7976241344926,26.));
#93380=CARTESIAN_POINT('Ctrl Pts',(107.154227550504,14.7864476819287,31.));
#93381=CARTESIAN_POINT('Ctrl Pts',(107.154227550504,14.7864476819287,26.));
#93382=CARTESIAN_POINT('Ctrl Pts',(107.122935662534,14.7756039024108,31.));
#93383=CARTESIAN_POINT('Ctrl Pts',(107.122935662534,14.7756039024108,26.));
#93384=CARTESIAN_POINT('Ctrl Pts',(107.090984398839,14.7651020986883,31.));
#93385=CARTESIAN_POINT('Ctrl Pts',(107.090984398839,14.7651020986883,26.));
#93386=CARTESIAN_POINT('Ctrl Pts',(107.05837932359,14.7549475106854,31.));
#93387=CARTESIAN_POINT('Ctrl Pts',(107.05837932359,14.7549475106854,26.));
#93388=CARTESIAN_POINT('Ctrl Pts',(107.0251274904,14.7451418299393,31.));
#93389=CARTESIAN_POINT('Ctrl Pts',(107.0251274904,14.7451418299393,26.));
#93390=CARTESIAN_POINT('Ctrl Pts',(106.991235969875,14.7356844847053,31.));
#93391=CARTESIAN_POINT('Ctrl Pts',(106.991235969875,14.7356844847053,26.));
#93392=CARTESIAN_POINT('Ctrl Pts',(106.963615969591,14.7283958793185,31.));
#93393=CARTESIAN_POINT('Ctrl Pts',(106.963615969591,14.7283958793185,26.));
#93394=CARTESIAN_POINT('Ctrl Pts',(106.942617866446,14.7230845608581,31.));
#93395=CARTESIAN_POINT('Ctrl Pts',(106.942617866446,14.7230845608581,26.));
#93396=CARTESIAN_POINT('Ctrl Pts',(106.928493535651,14.7196125061553,31.));
#93397=CARTESIAN_POINT('Ctrl Pts',(106.928493535651,14.7196125061553,26.));
#93398=CARTESIAN_POINT('Ctrl Pts',(106.921399971368,14.7178936848864,31.));
#93399=CARTESIAN_POINT('Ctrl Pts',(106.921399971368,14.7178936848864,26.));
#93400=CARTESIAN_POINT('Ctrl Pts',(107.644355604652,15.0709566360981,31.));
#93401=CARTESIAN_POINT('Ctrl Pts',(107.642845514352,15.0691494316033,31.));
#93402=CARTESIAN_POINT('Ctrl Pts',(107.639666871615,15.0654611335559,31.));
#93403=CARTESIAN_POINT('Ctrl Pts',(107.634423517451,15.0597070156512,31.));
#93404=CARTESIAN_POINT('Ctrl Pts',(107.626479908375,15.0515907456204,31.));
#93405=CARTESIAN_POINT('Ctrl Pts',(107.614961199788,15.0407097018941,31.));
#93406=CARTESIAN_POINT('Ctrl Pts',(107.601866156862,15.0291151846723,31.));
#93407=CARTESIAN_POINT('Ctrl Pts',(107.587232918926,15.0168569757285,31.));
#93408=CARTESIAN_POINT('Ctrl Pts',(107.571140046232,15.0040264741695,31.));
#93409=CARTESIAN_POINT('Ctrl Pts',(107.553709421335,14.9907586689459,31.));
#93410=CARTESIAN_POINT('Ctrl Pts',(107.5350824668,14.9772079499723,31.));
#93411=CARTESIAN_POINT('Ctrl Pts',(107.515401372608,14.9635285997574,31.));
#93412=CARTESIAN_POINT('Ctrl Pts',(107.494790426365,14.9498554345175,31.));
#93413=CARTESIAN_POINT('Ctrl Pts',(107.473333124048,14.9362797093226,31.));
#93414=CARTESIAN_POINT('Ctrl Pts',(107.451067109284,14.9228439050363,31.));
#93415=CARTESIAN_POINT('Ctrl Pts',(107.428001300302,14.9095600205959,31.));
#93416=CARTESIAN_POINT('Ctrl Pts',(107.404127740676,14.8964220475778,31.));
#93417=CARTESIAN_POINT('Ctrl Pts',(107.379434581043,14.8834195982418,31.));
#93418=CARTESIAN_POINT('Ctrl Pts',(107.353921212289,14.8705534140105,31.));
#93419=CARTESIAN_POINT('Ctrl Pts',(107.327603123054,14.8578406757021,31.));
#93420=CARTESIAN_POINT('Ctrl Pts',(107.300504551911,14.8453081604869,31.));
#93421=CARTESIAN_POINT('Ctrl Pts',(107.272654453203,14.8329885380258,31.));
#93422=CARTESIAN_POINT('Ctrl Pts',(107.244081627818,14.8209156617599,31.));
#93423=CARTESIAN_POINT('Ctrl Pts',(107.214809663941,14.8091196376662,31.));
#93424=CARTESIAN_POINT('Ctrl Pts',(107.1848546456,14.7976241344926,31.));
#93425=CARTESIAN_POINT('Ctrl Pts',(107.154227550504,14.7864476819287,31.));
#93426=CARTESIAN_POINT('Ctrl Pts',(107.122935662534,14.7756039024108,31.));
#93427=CARTESIAN_POINT('Ctrl Pts',(107.090984398839,14.7651020986883,31.));
#93428=CARTESIAN_POINT('Ctrl Pts',(107.05837932359,14.7549475106854,31.));
#93429=CARTESIAN_POINT('Ctrl Pts',(107.0251274904,14.7451418299393,31.));
#93430=CARTESIAN_POINT('Ctrl Pts',(106.991235969875,14.7356844847053,31.));
#93431=CARTESIAN_POINT('Ctrl Pts',(106.963615969591,14.7283958793185,31.));
#93432=CARTESIAN_POINT('Ctrl Pts',(106.942617866446,14.7230845608581,31.));
#93433=CARTESIAN_POINT('Ctrl Pts',(106.928493535651,14.7196125061553,31.));
#93434=CARTESIAN_POINT('Ctrl Pts',(106.921399971368,14.7178936848864,31.));
#93435=CARTESIAN_POINT('Ctrl Pts',(107.644355604652,15.0709566360981,26.));
#93436=CARTESIAN_POINT('Ctrl Pts',(107.642845514352,15.0691494316033,26.));
#93437=CARTESIAN_POINT('Ctrl Pts',(107.639666871615,15.0654611335559,26.));
#93438=CARTESIAN_POINT('Ctrl Pts',(107.634423517451,15.0597070156512,26.));
#93439=CARTESIAN_POINT('Ctrl Pts',(107.626479908375,15.0515907456204,26.));
#93440=CARTESIAN_POINT('Ctrl Pts',(107.614961199788,15.0407097018941,26.));
#93441=CARTESIAN_POINT('Ctrl Pts',(107.601866156862,15.0291151846723,26.));
#93442=CARTESIAN_POINT('Ctrl Pts',(107.587232918926,15.0168569757285,26.));
#93443=CARTESIAN_POINT('Ctrl Pts',(107.571140046232,15.0040264741695,26.));
#93444=CARTESIAN_POINT('Ctrl Pts',(107.553709421335,14.9907586689459,26.));
#93445=CARTESIAN_POINT('Ctrl Pts',(107.5350824668,14.9772079499723,26.));
#93446=CARTESIAN_POINT('Ctrl Pts',(107.515401372608,14.9635285997574,26.));
#93447=CARTESIAN_POINT('Ctrl Pts',(107.494790426365,14.9498554345175,26.));
#93448=CARTESIAN_POINT('Ctrl Pts',(107.473333124048,14.9362797093226,26.));
#93449=CARTESIAN_POINT('Ctrl Pts',(107.451067109284,14.9228439050363,26.));
#93450=CARTESIAN_POINT('Ctrl Pts',(107.428001300302,14.9095600205959,26.));
#93451=CARTESIAN_POINT('Ctrl Pts',(107.404127740676,14.8964220475778,26.));
#93452=CARTESIAN_POINT('Ctrl Pts',(107.379434581043,14.8834195982418,26.));
#93453=CARTESIAN_POINT('Ctrl Pts',(107.353921212289,14.8705534140105,26.));
#93454=CARTESIAN_POINT('Ctrl Pts',(107.327603123054,14.8578406757021,26.));
#93455=CARTESIAN_POINT('Ctrl Pts',(107.300504551911,14.8453081604869,26.));
#93456=CARTESIAN_POINT('Ctrl Pts',(107.272654453203,14.8329885380258,26.));
#93457=CARTESIAN_POINT('Ctrl Pts',(107.244081627818,14.8209156617599,26.));
#93458=CARTESIAN_POINT('Ctrl Pts',(107.214809663941,14.8091196376662,26.));
#93459=CARTESIAN_POINT('Ctrl Pts',(107.1848546456,14.7976241344926,26.));
#93460=CARTESIAN_POINT('Ctrl Pts',(107.154227550504,14.7864476819287,26.));
#93461=CARTESIAN_POINT('Ctrl Pts',(107.122935662534,14.7756039024108,26.));
#93462=CARTESIAN_POINT('Ctrl Pts',(107.090984398839,14.7651020986883,26.));
#93463=CARTESIAN_POINT('Ctrl Pts',(107.05837932359,14.7549475106854,26.));
#93464=CARTESIAN_POINT('Ctrl Pts',(107.0251274904,14.7451418299393,26.));
#93465=CARTESIAN_POINT('Ctrl Pts',(106.991235969875,14.7356844847053,26.));
#93466=CARTESIAN_POINT('Ctrl Pts',(106.963615969591,14.7283958793185,26.));
#93467=CARTESIAN_POINT('Ctrl Pts',(106.942617866446,14.7230845608581,26.));
#93468=CARTESIAN_POINT('Ctrl Pts',(106.928493535651,14.7196125061553,26.));
#93469=CARTESIAN_POINT('Ctrl Pts',(106.921399971368,14.7178936848864,26.));
#93470=CARTESIAN_POINT('Origin',(107.275453031443,15.2754530314203,31.));
#93471=CARTESIAN_POINT('Origin',(107.171000362364,16.451650540008,31.));
#93472=CARTESIAN_POINT('',(106.702771989219,16.1953828688963,31.));
#93473=CARTESIAN_POINT('',(106.702771989219,16.1953828688963,31.));
#93474=CARTESIAN_POINT('',(106.702771989219,16.1953828688963,26.));
#93475=CARTESIAN_POINT('',(106.702771989219,16.1953828688963,31.));
#93476=CARTESIAN_POINT('',(106.702771989219,16.1953828688963,26.));
#93477=CARTESIAN_POINT('Origin',(106.39245070361,16.9445647253073,31.));
#93478=CARTESIAN_POINT('',(106.39245070361,16.9445647253073,26.));
#93479=CARTESIAN_POINT('',(106.904746769447,17.0944435750604,26.));
#93480=CARTESIAN_POINT('',(106.39245070361,16.9445647253073,31.));
#93481=CARTESIAN_POINT('',(106.39245070361,16.9445647253073,31.));
#93482=CARTESIAN_POINT('',(106.904746769447,17.0944435750604,31.));
#93483=CARTESIAN_POINT('Ctrl Pts',(105.789599926104,16.4117521548133,31.));
#93484=CARTESIAN_POINT('Ctrl Pts',(105.789599926104,16.4117521548133,26.));
#93485=CARTESIAN_POINT('Ctrl Pts',(105.793902499401,16.4176479892937,31.));
#93486=CARTESIAN_POINT('Ctrl Pts',(105.793902499401,16.4176479892937,26.));
#93487=CARTESIAN_POINT('Ctrl Pts',(105.80251540703,16.4293684717013,31.));
#93488=CARTESIAN_POINT('Ctrl Pts',(105.80251540703,16.4293684717013,26.));
#93489=CARTESIAN_POINT('Ctrl Pts',(105.815458051595,16.4467356359271,31.));
#93490=CARTESIAN_POINT('Ctrl Pts',(105.815458051595,16.4467356359271,26.));
#93491=CARTESIAN_POINT('Ctrl Pts',(105.832761561427,16.4694639603885,31.));
#93492=CARTESIAN_POINT('Ctrl Pts',(105.832761561427,16.4694639603885,26.));
#93493=CARTESIAN_POINT('Ctrl Pts',(105.854468732543,16.4971564731453,31.));
#93494=CARTESIAN_POINT('Ctrl Pts',(105.854468732543,16.4971564731453,26.));
#93495=CARTESIAN_POINT('Ctrl Pts',(105.876252925984,16.5241246895858,31.));
#93496=CARTESIAN_POINT('Ctrl Pts',(105.876252925984,16.5241246895858,26.));
#93497=CARTESIAN_POINT('Ctrl Pts',(105.898111964153,16.5503618585695,31.));
#93498=CARTESIAN_POINT('Ctrl Pts',(105.898111964153,16.5503618585695,26.));
#93499=CARTESIAN_POINT('Ctrl Pts',(105.920041584957,16.5758621107647,31.));
#93500=CARTESIAN_POINT('Ctrl Pts',(105.920041584957,16.5758621107647,26.));
#93501=CARTESIAN_POINT('Ctrl Pts',(105.942034818016,16.6006223107948,31.));
#93502=CARTESIAN_POINT('Ctrl Pts',(105.942034818016,16.6006223107948,26.));
#93503=CARTESIAN_POINT('Ctrl Pts',(105.964080995658,16.6246410138719,31.));
#93504=CARTESIAN_POINT('Ctrl Pts',(105.964080995658,16.6246410138719,26.));
#93505=CARTESIAN_POINT('Ctrl Pts',(105.986164744977,16.6479167036358,31.));
#93506=CARTESIAN_POINT('Ctrl Pts',(105.986164744977,16.6479167036358,26.));
#93507=CARTESIAN_POINT('Ctrl Pts',(106.008264745793,16.6704463289922,31.));
#93508=CARTESIAN_POINT('Ctrl Pts',(106.008264745793,16.6704463289922,26.));
#93509=CARTESIAN_POINT('Ctrl Pts',(106.03035297595,16.6922240878588,31.));
#93510=CARTESIAN_POINT('Ctrl Pts',(106.03035297595,16.6922240878588,26.));
#93511=CARTESIAN_POINT('Ctrl Pts',(106.052392594348,16.7132397086437,31.));
#93512=CARTESIAN_POINT('Ctrl Pts',(106.052392594348,16.7132397086437,26.));
#93513=CARTESIAN_POINT('Ctrl Pts',(106.074341302863,16.733479537944,31.));
#93514=CARTESIAN_POINT('Ctrl Pts',(106.074341302863,16.733479537944,26.));
#93515=CARTESIAN_POINT('Ctrl Pts',(106.096157838315,16.7529293275796,31.));
#93516=CARTESIAN_POINT('Ctrl Pts',(106.096157838315,16.7529293275796,26.));
#93517=CARTESIAN_POINT('Ctrl Pts',(106.117808186123,16.7715769312133,31.));
#93518=CARTESIAN_POINT('Ctrl Pts',(106.117808186123,16.7715769312133,26.));
#93519=CARTESIAN_POINT('Ctrl Pts',(106.139270546029,16.7894146140322,31.));
#93520=CARTESIAN_POINT('Ctrl Pts',(106.139270546029,16.7894146140322,26.));
#93521=CARTESIAN_POINT('Ctrl Pts',(106.160544466144,16.8064432225185,31.));
#93522=CARTESIAN_POINT('Ctrl Pts',(106.160544466144,16.8064432225185,26.));
#93523=CARTESIAN_POINT('Ctrl Pts',(106.181644078043,16.8226697288425,31.));
#93524=CARTESIAN_POINT('Ctrl Pts',(106.181644078043,16.8226697288425,26.));
#93525=CARTESIAN_POINT('Ctrl Pts',(106.202577977579,16.8380991844595,31.));
#93526=CARTESIAN_POINT('Ctrl Pts',(106.202577977579,16.8380991844595,26.));
#93527=CARTESIAN_POINT('Ctrl Pts',(106.22333166632,16.8527279417898,31.));
#93528=CARTESIAN_POINT('Ctrl Pts',(106.22333166632,16.8527279417898,26.));
#93529=CARTESIAN_POINT('Ctrl Pts',(106.243851491477,16.866537479377,31.));
#93530=CARTESIAN_POINT('Ctrl Pts',(106.243851491477,16.866537479377,26.));
#93531=CARTESIAN_POINT('Ctrl Pts',(106.264021191832,16.8794855787969,31.));
#93532=CARTESIAN_POINT('Ctrl Pts',(106.264021191832,16.8794855787969,26.));
#93533=CARTESIAN_POINT('Ctrl Pts',(106.283668650636,16.8915090052018,31.));
#93534=CARTESIAN_POINT('Ctrl Pts',(106.283668650636,16.8915090052018,26.));
#93535=CARTESIAN_POINT('Ctrl Pts',(106.302596915689,16.9025354335354,31.));
#93536=CARTESIAN_POINT('Ctrl Pts',(106.302596915689,16.9025354335354,26.));
#93537=CARTESIAN_POINT('Ctrl Pts',(106.320609229236,16.912493288848,31.));
#93538=CARTESIAN_POINT('Ctrl Pts',(106.320609229236,16.912493288848,26.));
#93539=CARTESIAN_POINT('Ctrl Pts',(106.337534235312,16.9213216243828,31.));
#93540=CARTESIAN_POINT('Ctrl Pts',(106.337534235312,16.9213216243828,26.));
#93541=CARTESIAN_POINT('Ctrl Pts',(106.353257428443,16.9289828368596,31.));
#93542=CARTESIAN_POINT('Ctrl Pts',(106.353257428443,16.9289828368596,26.));
#93543=CARTESIAN_POINT('Ctrl Pts',(106.367718220975,16.9354607407975,31.));
#93544=CARTESIAN_POINT('Ctrl Pts',(106.367718220975,16.9354607407975,26.));
#93545=CARTESIAN_POINT('Ctrl Pts',(106.378256564321,16.9396937165682,31.));
#93546=CARTESIAN_POINT('Ctrl Pts',(106.378256564321,16.9396937165682,26.));
#93547=CARTESIAN_POINT('Ctrl Pts',(106.385579220845,16.9423359385813,31.));
#93548=CARTESIAN_POINT('Ctrl Pts',(106.385579220845,16.9423359385813,26.));
#93549=CARTESIAN_POINT('Ctrl Pts',(106.390203177829,16.9438611710006,31.));
#93550=CARTESIAN_POINT('Ctrl Pts',(106.390203177829,16.9438611710006,26.));
#93551=CARTESIAN_POINT('Ctrl Pts',(106.39245070361,16.9445647253073,31.));
#93552=CARTESIAN_POINT('Ctrl Pts',(106.39245070361,16.9445647253073,26.));
#93553=CARTESIAN_POINT('',(105.789599926104,16.4117521548133,31.));
#93554=CARTESIAN_POINT('Ctrl Pts',(106.39245070361,16.9445647253073,31.));
#93555=CARTESIAN_POINT('Ctrl Pts',(106.390203177829,16.9438611710006,31.));
#93556=CARTESIAN_POINT('Ctrl Pts',(106.385579220845,16.9423359385813,31.));
#93557=CARTESIAN_POINT('Ctrl Pts',(106.378256564321,16.9396937165682,31.));
#93558=CARTESIAN_POINT('Ctrl Pts',(106.367718220975,16.9354607407975,31.));
#93559=CARTESIAN_POINT('Ctrl Pts',(106.353257428443,16.9289828368596,31.));
#93560=CARTESIAN_POINT('Ctrl Pts',(106.337534235312,16.9213216243828,31.));
#93561=CARTESIAN_POINT('Ctrl Pts',(106.320609229236,16.912493288848,31.));
#93562=CARTESIAN_POINT('Ctrl Pts',(106.302596915689,16.9025354335354,31.));
#93563=CARTESIAN_POINT('Ctrl Pts',(106.283668650636,16.8915090052018,31.));
#93564=CARTESIAN_POINT('Ctrl Pts',(106.264021191832,16.8794855787969,31.));
#93565=CARTESIAN_POINT('Ctrl Pts',(106.243851491477,16.866537479377,31.));
#93566=CARTESIAN_POINT('Ctrl Pts',(106.22333166632,16.8527279417898,31.));
#93567=CARTESIAN_POINT('Ctrl Pts',(106.202577977579,16.8380991844595,31.));
#93568=CARTESIAN_POINT('Ctrl Pts',(106.181644078043,16.8226697288425,31.));
#93569=CARTESIAN_POINT('Ctrl Pts',(106.160544466144,16.8064432225185,31.));
#93570=CARTESIAN_POINT('Ctrl Pts',(106.139270546029,16.7894146140322,31.));
#93571=CARTESIAN_POINT('Ctrl Pts',(106.117808186123,16.7715769312133,31.));
#93572=CARTESIAN_POINT('Ctrl Pts',(106.096157838315,16.7529293275796,31.));
#93573=CARTESIAN_POINT('Ctrl Pts',(106.074341302863,16.733479537944,31.));
#93574=CARTESIAN_POINT('Ctrl Pts',(106.052392594348,16.7132397086437,31.));
#93575=CARTESIAN_POINT('Ctrl Pts',(106.03035297595,16.6922240878588,31.));
#93576=CARTESIAN_POINT('Ctrl Pts',(106.008264745793,16.6704463289922,31.));
#93577=CARTESIAN_POINT('Ctrl Pts',(105.986164744977,16.6479167036358,31.));
#93578=CARTESIAN_POINT('Ctrl Pts',(105.964080995658,16.6246410138719,31.));
#93579=CARTESIAN_POINT('Ctrl Pts',(105.942034818016,16.6006223107948,31.));
#93580=CARTESIAN_POINT('Ctrl Pts',(105.920041584957,16.5758621107647,31.));
#93581=CARTESIAN_POINT('Ctrl Pts',(105.898111964153,16.5503618585695,31.));
#93582=CARTESIAN_POINT('Ctrl Pts',(105.876252925984,16.5241246895858,31.));
#93583=CARTESIAN_POINT('Ctrl Pts',(105.854468732543,16.4971564731453,31.));
#93584=CARTESIAN_POINT('Ctrl Pts',(105.832761561427,16.4694639603885,31.));
#93585=CARTESIAN_POINT('Ctrl Pts',(105.815458051595,16.4467356359271,31.));
#93586=CARTESIAN_POINT('Ctrl Pts',(105.80251540703,16.4293684717013,31.));
#93587=CARTESIAN_POINT('Ctrl Pts',(105.793902499401,16.4176479892937,31.));
#93588=CARTESIAN_POINT('Ctrl Pts',(105.789599926104,16.4117521548133,31.));
#93589=CARTESIAN_POINT('',(105.789599926104,16.4117521548133,26.));
#93590=CARTESIAN_POINT('Ctrl Pts',(105.789599926104,16.4117521548133,26.));
#93591=CARTESIAN_POINT('Ctrl Pts',(105.793902499401,16.4176479892937,26.));
#93592=CARTESIAN_POINT('Ctrl Pts',(105.80251540703,16.4293684717013,26.));
#93593=CARTESIAN_POINT('Ctrl Pts',(105.815458051595,16.4467356359271,26.));
#93594=CARTESIAN_POINT('Ctrl Pts',(105.832761561427,16.4694639603885,26.));
#93595=CARTESIAN_POINT('Ctrl Pts',(105.854468732543,16.4971564731453,26.));
#93596=CARTESIAN_POINT('Ctrl Pts',(105.876252925984,16.5241246895858,26.));
#93597=CARTESIAN_POINT('Ctrl Pts',(105.898111964153,16.5503618585695,26.));
#93598=CARTESIAN_POINT('Ctrl Pts',(105.920041584957,16.5758621107647,26.));
#93599=CARTESIAN_POINT('Ctrl Pts',(105.942034818016,16.6006223107948,26.));
#93600=CARTESIAN_POINT('Ctrl Pts',(105.964080995658,16.6246410138719,26.));
#93601=CARTESIAN_POINT('Ctrl Pts',(105.986164744977,16.6479167036358,26.));
#93602=CARTESIAN_POINT('Ctrl Pts',(106.008264745793,16.6704463289922,26.));
#93603=CARTESIAN_POINT('Ctrl Pts',(106.03035297595,16.6922240878588,26.));
#93604=CARTESIAN_POINT('Ctrl Pts',(106.052392594348,16.7132397086437,26.));
#93605=CARTESIAN_POINT('Ctrl Pts',(106.074341302863,16.733479537944,26.));
#93606=CARTESIAN_POINT('Ctrl Pts',(106.096157838315,16.7529293275796,26.));
#93607=CARTESIAN_POINT('Ctrl Pts',(106.117808186123,16.7715769312133,26.));
#93608=CARTESIAN_POINT('Ctrl Pts',(106.139270546029,16.7894146140322,26.));
#93609=CARTESIAN_POINT('Ctrl Pts',(106.160544466144,16.8064432225185,26.));
#93610=CARTESIAN_POINT('Ctrl Pts',(106.181644078043,16.8226697288425,26.));
#93611=CARTESIAN_POINT('Ctrl Pts',(106.202577977579,16.8380991844595,26.));
#93612=CARTESIAN_POINT('Ctrl Pts',(106.22333166632,16.8527279417898,26.));
#93613=CARTESIAN_POINT('Ctrl Pts',(106.243851491477,16.866537479377,26.));
#93614=CARTESIAN_POINT('Ctrl Pts',(106.264021191832,16.8794855787969,26.));
#93615=CARTESIAN_POINT('Ctrl Pts',(106.283668650636,16.8915090052018,26.));
#93616=CARTESIAN_POINT('Ctrl Pts',(106.302596915689,16.9025354335354,26.));
#93617=CARTESIAN_POINT('Ctrl Pts',(106.320609229236,16.912493288848,26.));
#93618=CARTESIAN_POINT('Ctrl Pts',(106.337534235312,16.9213216243828,26.));
#93619=CARTESIAN_POINT('Ctrl Pts',(106.353257428443,16.9289828368596,26.));
#93620=CARTESIAN_POINT('Ctrl Pts',(106.367718220975,16.9354607407975,26.));
#93621=CARTESIAN_POINT('Ctrl Pts',(106.378256564321,16.9396937165682,26.));
#93622=CARTESIAN_POINT('Ctrl Pts',(106.385579220845,16.9423359385813,26.));
#93623=CARTESIAN_POINT('Ctrl Pts',(106.390203177829,16.9438611710006,26.));
#93624=CARTESIAN_POINT('Ctrl Pts',(106.39245070361,16.9445647253073,26.));
#93625=CARTESIAN_POINT('',(105.789599926104,16.4117521548133,31.));
#93626=CARTESIAN_POINT('Origin',(110.000000000003,18.0000000000012,31.));
#93627=CARTESIAN_POINT('',(105.899736734704,16.1458583777765,31.));
#93628=CARTESIAN_POINT('Origin',(110.000000000003,18.0000000000012,31.));
#93629=CARTESIAN_POINT('',(105.899736734704,16.1458583777765,26.));
#93630=CARTESIAN_POINT('Origin',(110.000000000003,18.0000000000012,26.));
#93631=CARTESIAN_POINT('',(105.899736734704,16.1458583777765,31.));
#93632=CARTESIAN_POINT('Ctrl Pts',(106.702771989219,16.1953828688963,31.));
#93633=CARTESIAN_POINT('Ctrl Pts',(106.702771989219,16.1953828688963,26.));
#93634=CARTESIAN_POINT('Ctrl Pts',(106.70068526048,16.1942911161916,31.));
#93635=CARTESIAN_POINT('Ctrl Pts',(106.70068526048,16.1942911161916,26.));
#93636=CARTESIAN_POINT('Ctrl Pts',(106.696337126957,16.1920999870287,31.));
#93637=CARTESIAN_POINT('Ctrl Pts',(106.696337126957,16.1920999870287,26.));
#93638=CARTESIAN_POINT('Ctrl Pts',(106.689290893774,16.1887904200375,31.));
#93639=CARTESIAN_POINT('Ctrl Pts',(106.689290893774,16.1887904200375,26.));
#93640=CARTESIAN_POINT('Ctrl Pts',(106.678845993861,16.1843318518623,31.));
#93641=CARTESIAN_POINT('Ctrl Pts',(106.678845993861,16.1843318518623,26.));
#93642=CARTESIAN_POINT('Ctrl Pts',(106.664040099595,16.1786870972096,31.));
#93643=CARTESIAN_POINT('Ctrl Pts',(106.664040099595,16.1786870972096,26.));
#93644=CARTESIAN_POINT('Ctrl Pts',(106.647504827811,16.1729864160331,31.));
#93645=CARTESIAN_POINT('Ctrl Pts',(106.647504827811,16.1729864160331,26.));
#93646=CARTESIAN_POINT('Ctrl Pts',(106.629294465314,16.1672612054047,31.));
#93647=CARTESIAN_POINT('Ctrl Pts',(106.629294465314,16.1672612054047,26.));
#93648=CARTESIAN_POINT('Ctrl Pts',(106.609516569238,16.1615658433815,31.));
#93649=CARTESIAN_POINT('Ctrl Pts',(106.609516569238,16.1615658433815,26.));
#93650=CARTESIAN_POINT('Ctrl Pts',(106.588335402414,16.1559784010579,31.));
#93651=CARTESIAN_POINT('Ctrl Pts',(106.588335402414,16.1559784010579,26.));
#93652=CARTESIAN_POINT('Ctrl Pts',(106.565940704718,16.1505873960435,31.));
#93653=CARTESIAN_POINT('Ctrl Pts',(106.565940704718,16.1505873960435,26.));
#93654=CARTESIAN_POINT('Ctrl Pts',(106.542522883923,16.1454809530401,31.));
#93655=CARTESIAN_POINT('Ctrl Pts',(106.542522883923,16.1454809530401,26.));
#93656=CARTESIAN_POINT('Ctrl Pts',(106.518248358739,16.1407360631828,31.));
#93657=CARTESIAN_POINT('Ctrl Pts',(106.518248358739,16.1407360631828,26.));
#93658=CARTESIAN_POINT('Ctrl Pts',(106.493229191191,16.136405082636,31.));
#93659=CARTESIAN_POINT('Ctrl Pts',(106.493229191191,16.136405082636,26.));
#93660=CARTESIAN_POINT('Ctrl Pts',(106.467516416179,16.1325128530083,31.));
#93661=CARTESIAN_POINT('Ctrl Pts',(106.467516416179,16.1325128530083,26.));
#93662=CARTESIAN_POINT('Ctrl Pts',(106.441122864867,16.1290670470128,31.));
#93663=CARTESIAN_POINT('Ctrl Pts',(106.441122864867,16.1290670470128,26.));
#93664=CARTESIAN_POINT('Ctrl Pts',(106.414038887152,16.1260651583832,31.));
#93665=CARTESIAN_POINT('Ctrl Pts',(106.414038887152,16.1260651583832,26.));
#93666=CARTESIAN_POINT('Ctrl Pts',(106.386249560432,16.1235021246537,31.));
#93667=CARTESIAN_POINT('Ctrl Pts',(106.386249560432,16.1235021246537,26.));
#93668=CARTESIAN_POINT('Ctrl Pts',(106.357754605692,16.1213788639067,31.));
#93669=CARTESIAN_POINT('Ctrl Pts',(106.357754605692,16.1213788639067,26.));
#93670=CARTESIAN_POINT('Ctrl Pts',(106.328574907382,16.1197053219033,31.));
#93671=CARTESIAN_POINT('Ctrl Pts',(106.328574907382,16.1197053219033,26.));
#93672=CARTESIAN_POINT('Ctrl Pts',(106.298743106205,16.1184969618219,31.));
#93673=CARTESIAN_POINT('Ctrl Pts',(106.298743106205,16.1184969618219,26.));
#93674=CARTESIAN_POINT('Ctrl Pts',(106.26829845462,16.1177728861474,31.));
#93675=CARTESIAN_POINT('Ctrl Pts',(106.26829845462,16.1177728861474,26.));
#93676=CARTESIAN_POINT('Ctrl Pts',(106.237280516333,16.1175533497575,31.));
#93677=CARTESIAN_POINT('Ctrl Pts',(106.237280516333,16.1175533497575,26.));
#93678=CARTESIAN_POINT('Ctrl Pts',(106.205722605043,16.1178571401407,31.));
#93679=CARTESIAN_POINT('Ctrl Pts',(106.205722605043,16.1178571401407,26.));
#93680=CARTESIAN_POINT('Ctrl Pts',(106.17364863809,16.1186999692782,31.));
#93681=CARTESIAN_POINT('Ctrl Pts',(106.17364863809,16.1186999692782,26.));
#93682=CARTESIAN_POINT('Ctrl Pts',(106.141075848562,16.1200947553829,31.));
#93683=CARTESIAN_POINT('Ctrl Pts',(106.141075848562,16.1200947553829,26.));
#93684=CARTESIAN_POINT('Ctrl Pts',(106.108016178967,16.1220512965248,31.));
#93685=CARTESIAN_POINT('Ctrl Pts',(106.108016178967,16.1220512965248,26.));
#93686=CARTESIAN_POINT('Ctrl Pts',(106.074478194107,16.1245761142702,31.));
#93687=CARTESIAN_POINT('Ctrl Pts',(106.074478194107,16.1245761142702,26.));
#93688=CARTESIAN_POINT('Ctrl Pts',(106.040469039837,16.1276719203621,31.));
#93689=CARTESIAN_POINT('Ctrl Pts',(106.040469039837,16.1276719203621,26.));
#93690=CARTESIAN_POINT('Ctrl Pts',(106.00599588017,16.131337578276,31.));
#93691=CARTESIAN_POINT('Ctrl Pts',(106.00599588017,16.131337578276,26.));
#93692=CARTESIAN_POINT('Ctrl Pts',(105.971065028696,16.1355698539851,31.));
#93693=CARTESIAN_POINT('Ctrl Pts',(105.971065028696,16.1355698539851,26.));
#93694=CARTESIAN_POINT('Ctrl Pts',(105.942758247219,16.1394057771583,31.));
#93695=CARTESIAN_POINT('Ctrl Pts',(105.942758247219,16.1394057771583,26.));
#93696=CARTESIAN_POINT('Ctrl Pts',(105.921325975923,16.1425343849267,31.));
#93697=CARTESIAN_POINT('Ctrl Pts',(105.921325975923,16.1425343849267,26.));
#93698=CARTESIAN_POINT('Ctrl Pts',(105.90694809798,16.1447317720396,31.));
#93699=CARTESIAN_POINT('Ctrl Pts',(105.90694809798,16.1447317720396,26.));
#93700=CARTESIAN_POINT('Ctrl Pts',(105.899736734704,16.1458583777765,31.));
#93701=CARTESIAN_POINT('Ctrl Pts',(105.899736734704,16.1458583777765,26.));
#93702=CARTESIAN_POINT('Ctrl Pts',(106.702771989219,16.1953828688963,31.));
#93703=CARTESIAN_POINT('Ctrl Pts',(106.70068526048,16.1942911161916,31.));
#93704=CARTESIAN_POINT('Ctrl Pts',(106.696337126957,16.1920999870287,31.));
#93705=CARTESIAN_POINT('Ctrl Pts',(106.689290893774,16.1887904200375,31.));
#93706=CARTESIAN_POINT('Ctrl Pts',(106.678845993861,16.1843318518623,31.));
#93707=CARTESIAN_POINT('Ctrl Pts',(106.664040099595,16.1786870972096,31.));
#93708=CARTESIAN_POINT('Ctrl Pts',(106.647504827811,16.1729864160331,31.));
#93709=CARTESIAN_POINT('Ctrl Pts',(106.629294465314,16.1672612054047,31.));
#93710=CARTESIAN_POINT('Ctrl Pts',(106.609516569238,16.1615658433815,31.));
#93711=CARTESIAN_POINT('Ctrl Pts',(106.588335402414,16.1559784010579,31.));
#93712=CARTESIAN_POINT('Ctrl Pts',(106.565940704718,16.1505873960435,31.));
#93713=CARTESIAN_POINT('Ctrl Pts',(106.542522883923,16.1454809530401,31.));
#93714=CARTESIAN_POINT('Ctrl Pts',(106.518248358739,16.1407360631828,31.));
#93715=CARTESIAN_POINT('Ctrl Pts',(106.493229191191,16.136405082636,31.));
#93716=CARTESIAN_POINT('Ctrl Pts',(106.467516416179,16.1325128530083,31.));
#93717=CARTESIAN_POINT('Ctrl Pts',(106.441122864867,16.1290670470128,31.));
#93718=CARTESIAN_POINT('Ctrl Pts',(106.414038887152,16.1260651583832,31.));
#93719=CARTESIAN_POINT('Ctrl Pts',(106.386249560432,16.1235021246537,31.));
#93720=CARTESIAN_POINT('Ctrl Pts',(106.357754605692,16.1213788639067,31.));
#93721=CARTESIAN_POINT('Ctrl Pts',(106.328574907382,16.1197053219033,31.));
#93722=CARTESIAN_POINT('Ctrl Pts',(106.298743106205,16.1184969618219,31.));
#93723=CARTESIAN_POINT('Ctrl Pts',(106.26829845462,16.1177728861474,31.));
#93724=CARTESIAN_POINT('Ctrl Pts',(106.237280516333,16.1175533497575,31.));
#93725=CARTESIAN_POINT('Ctrl Pts',(106.205722605043,16.1178571401407,31.));
#93726=CARTESIAN_POINT('Ctrl Pts',(106.17364863809,16.1186999692782,31.));
#93727=CARTESIAN_POINT('Ctrl Pts',(106.141075848562,16.1200947553829,31.));
#93728=CARTESIAN_POINT('Ctrl Pts',(106.108016178967,16.1220512965248,31.));
#93729=CARTESIAN_POINT('Ctrl Pts',(106.074478194107,16.1245761142702,31.));
#93730=CARTESIAN_POINT('Ctrl Pts',(106.040469039837,16.1276719203621,31.));
#93731=CARTESIAN_POINT('Ctrl Pts',(106.00599588017,16.131337578276,31.));
#93732=CARTESIAN_POINT('Ctrl Pts',(105.971065028696,16.1355698539851,31.));
#93733=CARTESIAN_POINT('Ctrl Pts',(105.942758247219,16.1394057771583,31.));
#93734=CARTESIAN_POINT('Ctrl Pts',(105.921325975923,16.1425343849267,31.));
#93735=CARTESIAN_POINT('Ctrl Pts',(105.90694809798,16.1447317720396,31.));
#93736=CARTESIAN_POINT('Ctrl Pts',(105.899736734704,16.1458583777765,31.));
#93737=CARTESIAN_POINT('Ctrl Pts',(106.702771989219,16.1953828688963,26.));
#93738=CARTESIAN_POINT('Ctrl Pts',(106.70068526048,16.1942911161916,26.));
#93739=CARTESIAN_POINT('Ctrl Pts',(106.696337126957,16.1920999870287,26.));
#93740=CARTESIAN_POINT('Ctrl Pts',(106.689290893774,16.1887904200375,26.));
#93741=CARTESIAN_POINT('Ctrl Pts',(106.678845993861,16.1843318518623,26.));
#93742=CARTESIAN_POINT('Ctrl Pts',(106.664040099595,16.1786870972096,26.));
#93743=CARTESIAN_POINT('Ctrl Pts',(106.647504827811,16.1729864160331,26.));
#93744=CARTESIAN_POINT('Ctrl Pts',(106.629294465314,16.1672612054047,26.));
#93745=CARTESIAN_POINT('Ctrl Pts',(106.609516569238,16.1615658433815,26.));
#93746=CARTESIAN_POINT('Ctrl Pts',(106.588335402414,16.1559784010579,26.));
#93747=CARTESIAN_POINT('Ctrl Pts',(106.565940704718,16.1505873960435,26.));
#93748=CARTESIAN_POINT('Ctrl Pts',(106.542522883923,16.1454809530401,26.));
#93749=CARTESIAN_POINT('Ctrl Pts',(106.518248358739,16.1407360631828,26.));
#93750=CARTESIAN_POINT('Ctrl Pts',(106.493229191191,16.136405082636,26.));
#93751=CARTESIAN_POINT('Ctrl Pts',(106.467516416179,16.1325128530083,26.));
#93752=CARTESIAN_POINT('Ctrl Pts',(106.441122864867,16.1290670470128,26.));
#93753=CARTESIAN_POINT('Ctrl Pts',(106.414038887152,16.1260651583832,26.));
#93754=CARTESIAN_POINT('Ctrl Pts',(106.386249560432,16.1235021246537,26.));
#93755=CARTESIAN_POINT('Ctrl Pts',(106.357754605692,16.1213788639067,26.));
#93756=CARTESIAN_POINT('Ctrl Pts',(106.328574907382,16.1197053219033,26.));
#93757=CARTESIAN_POINT('Ctrl Pts',(106.298743106205,16.1184969618219,26.));
#93758=CARTESIAN_POINT('Ctrl Pts',(106.26829845462,16.1177728861474,26.));
#93759=CARTESIAN_POINT('Ctrl Pts',(106.237280516333,16.1175533497575,26.));
#93760=CARTESIAN_POINT('Ctrl Pts',(106.205722605043,16.1178571401407,26.));
#93761=CARTESIAN_POINT('Ctrl Pts',(106.17364863809,16.1186999692782,26.));
#93762=CARTESIAN_POINT('Ctrl Pts',(106.141075848562,16.1200947553829,26.));
#93763=CARTESIAN_POINT('Ctrl Pts',(106.108016178967,16.1220512965248,26.));
#93764=CARTESIAN_POINT('Ctrl Pts',(106.074478194107,16.1245761142702,26.));
#93765=CARTESIAN_POINT('Ctrl Pts',(106.040469039837,16.1276719203621,26.));
#93766=CARTESIAN_POINT('Ctrl Pts',(106.00599588017,16.131337578276,26.));
#93767=CARTESIAN_POINT('Ctrl Pts',(105.971065028696,16.1355698539851,26.));
#93768=CARTESIAN_POINT('Ctrl Pts',(105.942758247219,16.1394057771583,26.));
#93769=CARTESIAN_POINT('Ctrl Pts',(105.921325975923,16.1425343849267,26.));
#93770=CARTESIAN_POINT('Ctrl Pts',(105.90694809798,16.1447317720396,26.));
#93771=CARTESIAN_POINT('Ctrl Pts',(105.899736734704,16.1458583777765,26.));
#93772=CARTESIAN_POINT('Origin',(106.440207834808,16.5254858059309,31.));
#93773=CARTESIAN_POINT('Origin',(106.793817451456,17.6521229162285,31.));
#93774=CARTESIAN_POINT('',(106.263161448981,17.5945457010101,31.));
#93775=CARTESIAN_POINT('',(106.263161448981,17.5945457010101,31.));
#93776=CARTESIAN_POINT('',(106.263161448981,17.5945457010101,26.));
#93777=CARTESIAN_POINT('',(106.263161448981,17.5945457010101,31.));
#93778=CARTESIAN_POINT('',(106.263161448981,17.5945457010101,26.));
#93779=CARTESIAN_POINT('Origin',(106.263161448981,18.4054542989899,31.));
#93780=CARTESIAN_POINT('',(106.263161448981,18.4054542989899,26.));
#93781=CARTESIAN_POINT('',(106.793817451456,18.3478770837715,26.));
#93782=CARTESIAN_POINT('',(106.263161448981,18.4054542989899,31.));
#93783=CARTESIAN_POINT('',(106.263161448981,18.4054542989899,31.));
#93784=CARTESIAN_POINT('',(106.793817451456,18.3478770837715,31.));
#93785=CARTESIAN_POINT('Ctrl Pts',(105.502301411201,18.1439006751855,31.));
#93786=CARTESIAN_POINT('Ctrl Pts',(105.502301411201,18.1439006751855,26.));
#93787=CARTESIAN_POINT('Ctrl Pts',(105.508532708783,18.1477011924717,31.));
#93788=CARTESIAN_POINT('Ctrl Pts',(105.508532708783,18.1477011924717,26.));
#93789=CARTESIAN_POINT('Ctrl Pts',(105.520975232293,18.1552334892252,31.));
#93790=CARTESIAN_POINT('Ctrl Pts',(105.520975232293,18.1552334892252,26.));
#93791=CARTESIAN_POINT('Ctrl Pts',(105.53957880272,18.1663257211454,31.));
#93792=CARTESIAN_POINT('Ctrl Pts',(105.53957880272,18.1663257211454,26.));
#93793=CARTESIAN_POINT('Ctrl Pts',(105.564262914511,18.1807021883888,31.));
#93794=CARTESIAN_POINT('Ctrl Pts',(105.564262914511,18.1807021883888,26.));
#93795=CARTESIAN_POINT('Ctrl Pts',(105.594915191446,18.1979797593792,31.));
#93796=CARTESIAN_POINT('Ctrl Pts',(105.594915191446,18.1979797593792,26.));
#93797=CARTESIAN_POINT('Ctrl Pts',(105.625361451532,18.2145586926593,31.));
#93798=CARTESIAN_POINT('Ctrl Pts',(105.625361451532,18.2145586926593,26.));
#93799=CARTESIAN_POINT('Ctrl Pts',(105.655597099378,18.2304335843199,31.));
#93800=CARTESIAN_POINT('Ctrl Pts',(105.655597099378,18.2304335843199,26.));
#93801=CARTESIAN_POINT('Ctrl Pts',(105.685615951231,18.2456006428371,31.));
#93802=CARTESIAN_POINT('Ctrl Pts',(105.685615951231,18.2456006428371,26.));
#93803=CARTESIAN_POINT('Ctrl Pts',(105.715410367441,18.26005963895,31.));
#93804=CARTESIAN_POINT('Ctrl Pts',(105.715410367441,18.26005963895,26.));
#93805=CARTESIAN_POINT('Ctrl Pts',(105.744969939469,18.27381332019,31.));
#93806=CARTESIAN_POINT('Ctrl Pts',(105.744969939469,18.27381332019,26.));
#93807=CARTESIAN_POINT('Ctrl Pts',(105.774279884316,18.2868661685787,31.));
#93808=CARTESIAN_POINT('Ctrl Pts',(105.774279884316,18.2868661685787,26.));
#93809=CARTESIAN_POINT('Ctrl Pts',(105.8033193371,18.2992235241532,31.));
#93810=CARTESIAN_POINT('Ctrl Pts',(105.8033193371,18.2992235241532,26.));
#93811=CARTESIAN_POINT('Ctrl Pts',(105.832060188363,18.3108907501027,31.));
#93812=CARTESIAN_POINT('Ctrl Pts',(105.832060188363,18.3108907501027,26.));
#93813=CARTESIAN_POINT('Ctrl Pts',(105.860464470601,18.3218724551924,31.));
#93814=CARTESIAN_POINT('Ctrl Pts',(105.860464470601,18.3218724551924,26.));
#93815=CARTESIAN_POINT('Ctrl Pts',(105.88848788051,18.3321722121141,31.));
#93816=CARTESIAN_POINT('Ctrl Pts',(105.88848788051,18.3321722121141,26.));
#93817=CARTESIAN_POINT('Ctrl Pts',(105.916086843341,18.3417926480007,31.));
#93818=CARTESIAN_POINT('Ctrl Pts',(105.916086843341,18.3417926480007,26.));
#93819=CARTESIAN_POINT('Ctrl Pts',(105.943225285516,18.3507355579176,31.));
#93820=CARTESIAN_POINT('Ctrl Pts',(105.943225285516,18.3507355579176,26.));
#93821=CARTESIAN_POINT('Ctrl Pts',(105.969880106239,18.3590021384258,31.));
#93822=CARTESIAN_POINT('Ctrl Pts',(105.969880106239,18.3590021384258,26.));
#93823=CARTESIAN_POINT('Ctrl Pts',(105.996051211954,18.3665933445037,31.));
#93824=CARTESIAN_POINT('Ctrl Pts',(105.996051211954,18.3665933445037,26.));
#93825=CARTESIAN_POINT('Ctrl Pts',(106.021754326667,18.3735102096776,31.));
#93826=CARTESIAN_POINT('Ctrl Pts',(106.021754326667,18.3735102096776,26.));
#93827=CARTESIAN_POINT('Ctrl Pts',(106.046999325018,18.3797541113929,31.));
#93828=CARTESIAN_POINT('Ctrl Pts',(106.046999325018,18.3797541113929,26.));
#93829=CARTESIAN_POINT('Ctrl Pts',(106.071771416337,18.3853272280346,31.));
#93830=CARTESIAN_POINT('Ctrl Pts',(106.071771416337,18.3853272280346,26.));
#93831=CARTESIAN_POINT('Ctrl Pts',(106.096013944053,18.3902329800424,31.));
#93832=CARTESIAN_POINT('Ctrl Pts',(106.096013944053,18.3902329800424,26.));
#93833=CARTESIAN_POINT('Ctrl Pts',(106.119603340517,18.3944768539199,31.));
#93834=CARTESIAN_POINT('Ctrl Pts',(106.119603340517,18.3944768539199,26.));
#93835=CARTESIAN_POINT('Ctrl Pts',(106.142356391658,18.3980662945134,31.));
#93836=CARTESIAN_POINT('Ctrl Pts',(106.142356391658,18.3980662945134,26.));
#93837=CARTESIAN_POINT('Ctrl Pts',(106.164063459768,18.4010098525282,31.));
#93838=CARTESIAN_POINT('Ctrl Pts',(106.164063459768,18.4010098525282,26.));
#93839=CARTESIAN_POINT('Ctrl Pts',(106.184515373837,18.4033166972663,31.));
#93840=CARTESIAN_POINT('Ctrl Pts',(106.184515373837,18.4033166972663,26.));
#93841=CARTESIAN_POINT('Ctrl Pts',(106.203530498282,18.4049960963551,31.));
#93842=CARTESIAN_POINT('Ctrl Pts',(106.203530498282,18.4049960963551,26.));
#93843=CARTESIAN_POINT('Ctrl Pts',(106.220988653688,18.4060571282417,31.));
#93844=CARTESIAN_POINT('Ctrl Pts',(106.220988653688,18.4060571282417,26.));
#93845=CARTESIAN_POINT('Ctrl Pts',(106.236827670446,18.4065080253827,31.));
#93846=CARTESIAN_POINT('Ctrl Pts',(106.236827670446,18.4065080253827,26.));
#93847=CARTESIAN_POINT('Ctrl Pts',(106.248183719867,18.4063859356555,31.));
#93848=CARTESIAN_POINT('Ctrl Pts',(106.248183719867,18.4063859356555,26.));
#93849=CARTESIAN_POINT('Ctrl Pts',(106.255960106942,18.4060247711612,31.));
#93850=CARTESIAN_POINT('Ctrl Pts',(106.255960106942,18.4060247711612,26.));
#93851=CARTESIAN_POINT('Ctrl Pts',(106.260815767337,18.4056643904459,31.));
#93852=CARTESIAN_POINT('Ctrl Pts',(106.260815767337,18.4056643904459,26.));
#93853=CARTESIAN_POINT('Ctrl Pts',(106.263161448981,18.4054542989899,31.));
#93854=CARTESIAN_POINT('Ctrl Pts',(106.263161448981,18.4054542989899,26.));
#93855=CARTESIAN_POINT('',(105.502301411201,18.1439006751855,31.));
#93856=CARTESIAN_POINT('Ctrl Pts',(106.263161448981,18.4054542989899,31.));
#93857=CARTESIAN_POINT('Ctrl Pts',(106.260815767337,18.4056643904459,31.));
#93858=CARTESIAN_POINT('Ctrl Pts',(106.255960106942,18.4060247711612,31.));
#93859=CARTESIAN_POINT('Ctrl Pts',(106.248183719867,18.4063859356555,31.));
#93860=CARTESIAN_POINT('Ctrl Pts',(106.236827670446,18.4065080253827,31.));
#93861=CARTESIAN_POINT('Ctrl Pts',(106.220988653688,18.4060571282417,31.));
#93862=CARTESIAN_POINT('Ctrl Pts',(106.203530498282,18.4049960963551,31.));
#93863=CARTESIAN_POINT('Ctrl Pts',(106.184515373837,18.4033166972663,31.));
#93864=CARTESIAN_POINT('Ctrl Pts',(106.164063459768,18.4010098525282,31.));
#93865=CARTESIAN_POINT('Ctrl Pts',(106.142356391658,18.3980662945134,31.));
#93866=CARTESIAN_POINT('Ctrl Pts',(106.119603340517,18.3944768539199,31.));
#93867=CARTESIAN_POINT('Ctrl Pts',(106.096013944053,18.3902329800424,31.));
#93868=CARTESIAN_POINT('Ctrl Pts',(106.071771416337,18.3853272280346,31.));
#93869=CARTESIAN_POINT('Ctrl Pts',(106.046999325018,18.3797541113929,31.));
#93870=CARTESIAN_POINT('Ctrl Pts',(106.021754326667,18.3735102096776,31.));
#93871=CARTESIAN_POINT('Ctrl Pts',(105.996051211954,18.3665933445037,31.));
#93872=CARTESIAN_POINT('Ctrl Pts',(105.969880106239,18.3590021384258,31.));
#93873=CARTESIAN_POINT('Ctrl Pts',(105.943225285516,18.3507355579176,31.));
#93874=CARTESIAN_POINT('Ctrl Pts',(105.916086843341,18.3417926480007,31.));
#93875=CARTESIAN_POINT('Ctrl Pts',(105.88848788051,18.3321722121141,31.));
#93876=CARTESIAN_POINT('Ctrl Pts',(105.860464470601,18.3218724551924,31.));
#93877=CARTESIAN_POINT('Ctrl Pts',(105.832060188363,18.3108907501027,31.));
#93878=CARTESIAN_POINT('Ctrl Pts',(105.8033193371,18.2992235241532,31.));
#93879=CARTESIAN_POINT('Ctrl Pts',(105.774279884316,18.2868661685787,31.));
#93880=CARTESIAN_POINT('Ctrl Pts',(105.744969939469,18.27381332019,31.));
#93881=CARTESIAN_POINT('Ctrl Pts',(105.715410367441,18.26005963895,31.));
#93882=CARTESIAN_POINT('Ctrl Pts',(105.685615951231,18.2456006428371,31.));
#93883=CARTESIAN_POINT('Ctrl Pts',(105.655597099378,18.2304335843199,31.));
#93884=CARTESIAN_POINT('Ctrl Pts',(105.625361451532,18.2145586926593,31.));
#93885=CARTESIAN_POINT('Ctrl Pts',(105.594915191446,18.1979797593792,31.));
#93886=CARTESIAN_POINT('Ctrl Pts',(105.564262914511,18.1807021883888,31.));
#93887=CARTESIAN_POINT('Ctrl Pts',(105.53957880272,18.1663257211454,31.));
#93888=CARTESIAN_POINT('Ctrl Pts',(105.520975232293,18.1552334892252,31.));
#93889=CARTESIAN_POINT('Ctrl Pts',(105.508532708783,18.1477011924717,31.));
#93890=CARTESIAN_POINT('Ctrl Pts',(105.502301411201,18.1439006751855,31.));
#93891=CARTESIAN_POINT('',(105.502301411201,18.1439006751855,26.));
#93892=CARTESIAN_POINT('Ctrl Pts',(105.502301411201,18.1439006751855,26.));
#93893=CARTESIAN_POINT('Ctrl Pts',(105.508532708783,18.1477011924717,26.));
#93894=CARTESIAN_POINT('Ctrl Pts',(105.520975232293,18.1552334892252,26.));
#93895=CARTESIAN_POINT('Ctrl Pts',(105.53957880272,18.1663257211454,26.));
#93896=CARTESIAN_POINT('Ctrl Pts',(105.564262914511,18.1807021883888,26.));
#93897=CARTESIAN_POINT('Ctrl Pts',(105.594915191446,18.1979797593792,26.));
#93898=CARTESIAN_POINT('Ctrl Pts',(105.625361451532,18.2145586926593,26.));
#93899=CARTESIAN_POINT('Ctrl Pts',(105.655597099378,18.2304335843199,26.));
#93900=CARTESIAN_POINT('Ctrl Pts',(105.685615951231,18.2456006428371,26.));
#93901=CARTESIAN_POINT('Ctrl Pts',(105.715410367441,18.26005963895,26.));
#93902=CARTESIAN_POINT('Ctrl Pts',(105.744969939469,18.27381332019,26.));
#93903=CARTESIAN_POINT('Ctrl Pts',(105.774279884316,18.2868661685787,26.));
#93904=CARTESIAN_POINT('Ctrl Pts',(105.8033193371,18.2992235241532,26.));
#93905=CARTESIAN_POINT('Ctrl Pts',(105.832060188363,18.3108907501027,26.));
#93906=CARTESIAN_POINT('Ctrl Pts',(105.860464470601,18.3218724551924,26.));
#93907=CARTESIAN_POINT('Ctrl Pts',(105.88848788051,18.3321722121141,26.));
#93908=CARTESIAN_POINT('Ctrl Pts',(105.916086843341,18.3417926480007,26.));
#93909=CARTESIAN_POINT('Ctrl Pts',(105.943225285516,18.3507355579176,26.));
#93910=CARTESIAN_POINT('Ctrl Pts',(105.969880106239,18.3590021384258,26.));
#93911=CARTESIAN_POINT('Ctrl Pts',(105.996051211954,18.3665933445037,26.));
#93912=CARTESIAN_POINT('Ctrl Pts',(106.021754326667,18.3735102096776,26.));
#93913=CARTESIAN_POINT('Ctrl Pts',(106.046999325018,18.3797541113929,26.));
#93914=CARTESIAN_POINT('Ctrl Pts',(106.071771416337,18.3853272280346,26.));
#93915=CARTESIAN_POINT('Ctrl Pts',(106.096013944053,18.3902329800424,26.));
#93916=CARTESIAN_POINT('Ctrl Pts',(106.119603340517,18.3944768539199,26.));
#93917=CARTESIAN_POINT('Ctrl Pts',(106.142356391658,18.3980662945134,26.));
#93918=CARTESIAN_POINT('Ctrl Pts',(106.164063459768,18.4010098525282,26.));
#93919=CARTESIAN_POINT('Ctrl Pts',(106.184515373837,18.4033166972663,26.));
#93920=CARTESIAN_POINT('Ctrl Pts',(106.203530498282,18.4049960963551,26.));
#93921=CARTESIAN_POINT('Ctrl Pts',(106.220988653688,18.4060571282417,26.));
#93922=CARTESIAN_POINT('Ctrl Pts',(106.236827670446,18.4065080253827,26.));
#93923=CARTESIAN_POINT('Ctrl Pts',(106.248183719867,18.4063859356555,26.));
#93924=CARTESIAN_POINT('Ctrl Pts',(106.255960106942,18.4060247711612,26.));
#93925=CARTESIAN_POINT('Ctrl Pts',(106.260815767337,18.4056643904459,26.));
#93926=CARTESIAN_POINT('Ctrl Pts',(106.263161448981,18.4054542989899,26.));
#93927=CARTESIAN_POINT('',(105.502301411201,18.1439006751855,31.));
#93928=CARTESIAN_POINT('Origin',(110.000000000003,18.,31.));
#93929=CARTESIAN_POINT('',(105.502301411201,17.8560993248145,31.));
#93930=CARTESIAN_POINT('Origin',(110.000000000003,18.,31.));
#93931=CARTESIAN_POINT('',(105.502301411201,17.8560993248145,26.));
#93932=CARTESIAN_POINT('Origin',(110.000000000003,18.,26.));
#93933=CARTESIAN_POINT('',(105.502301411201,17.8560993248145,31.));
#93934=CARTESIAN_POINT('Ctrl Pts',(106.263161448981,17.5945457010101,31.));
#93935=CARTESIAN_POINT('Ctrl Pts',(106.263161448981,17.5945457010101,26.));
#93936=CARTESIAN_POINT('Ctrl Pts',(106.260815767337,17.5943356095479,31.));
#93937=CARTESIAN_POINT('Ctrl Pts',(106.260815767337,17.5943356095479,26.));
#93938=CARTESIAN_POINT('Ctrl Pts',(106.255960106942,17.593975228822,31.));
#93939=CARTESIAN_POINT('Ctrl Pts',(106.255960106942,17.593975228822,26.));
#93940=CARTESIAN_POINT('Ctrl Pts',(106.248183719866,17.5936140643173,31.));
#93941=CARTESIAN_POINT('Ctrl Pts',(106.248183719866,17.5936140643173,26.));
#93942=CARTESIAN_POINT('Ctrl Pts',(106.236827670445,17.5934919745854,31.));
#93943=CARTESIAN_POINT('Ctrl Pts',(106.236827670445,17.5934919745854,26.));
#93944=CARTESIAN_POINT('Ctrl Pts',(106.220988653687,17.5939428717324,31.));
#93945=CARTESIAN_POINT('Ctrl Pts',(106.220988653687,17.5939428717324,26.));
#93946=CARTESIAN_POINT('Ctrl Pts',(106.203530498282,17.5950039036334,31.));
#93947=CARTESIAN_POINT('Ctrl Pts',(106.203530498282,17.5950039036334,26.));
#93948=CARTESIAN_POINT('Ctrl Pts',(106.184515373837,17.5966833027395,31.));
#93949=CARTESIAN_POINT('Ctrl Pts',(106.184515373837,17.5966833027395,26.));
#93950=CARTESIAN_POINT('Ctrl Pts',(106.164063459768,17.5989901474915,31.));
#93951=CARTESIAN_POINT('Ctrl Pts',(106.164063459768,17.5989901474915,26.));
#93952=CARTESIAN_POINT('Ctrl Pts',(106.142356391658,17.6019337055115,31.));
#93953=CARTESIAN_POINT('Ctrl Pts',(106.142356391658,17.6019337055115,26.));
#93954=CARTESIAN_POINT('Ctrl Pts',(106.119603340517,17.6055231461002,31.));
#93955=CARTESIAN_POINT('Ctrl Pts',(106.119603340517,17.6055231461002,26.));
#93956=CARTESIAN_POINT('Ctrl Pts',(106.096013944054,17.6097670199654,31.));
#93957=CARTESIAN_POINT('Ctrl Pts',(106.096013944054,17.6097670199654,26.));
#93958=CARTESIAN_POINT('Ctrl Pts',(106.071771416337,17.6146727719589,31.));
#93959=CARTESIAN_POINT('Ctrl Pts',(106.071771416337,17.6146727719589,26.));
#93960=CARTESIAN_POINT('Ctrl Pts',(106.046999325018,17.6202458885881,31.));
#93961=CARTESIAN_POINT('Ctrl Pts',(106.046999325018,17.6202458885881,26.));
#93962=CARTESIAN_POINT('Ctrl Pts',(106.021754326667,17.6264897902966,31.));
#93963=CARTESIAN_POINT('Ctrl Pts',(106.021754326667,17.6264897902966,26.));
#93964=CARTESIAN_POINT('Ctrl Pts',(105.996051211954,17.6334066554725,31.));
#93965=CARTESIAN_POINT('Ctrl Pts',(105.996051211954,17.6334066554725,26.));
#93966=CARTESIAN_POINT('Ctrl Pts',(105.969880106239,17.640997861563,31.));
#93967=CARTESIAN_POINT('Ctrl Pts',(105.969880106239,17.640997861563,26.));
#93968=CARTESIAN_POINT('Ctrl Pts',(105.943225285516,17.6492644420914,31.));
#93969=CARTESIAN_POINT('Ctrl Pts',(105.943225285516,17.6492644420914,26.));
#93970=CARTESIAN_POINT('Ctrl Pts',(105.916086843341,17.6582073520301,31.));
#93971=CARTESIAN_POINT('Ctrl Pts',(105.916086843341,17.6582073520301,26.));
#93972=CARTESIAN_POINT('Ctrl Pts',(105.88848788051,17.667827787931,31.));
#93973=CARTESIAN_POINT('Ctrl Pts',(105.88848788051,17.667827787931,26.));
#93974=CARTESIAN_POINT('Ctrl Pts',(105.860464470601,17.6781275448521,31.));
#93975=CARTESIAN_POINT('Ctrl Pts',(105.860464470601,17.6781275448521,26.));
#93976=CARTESIAN_POINT('Ctrl Pts',(105.832060188363,17.6891092499218,31.));
#93977=CARTESIAN_POINT('Ctrl Pts',(105.832060188363,17.6891092499218,26.));
#93978=CARTESIAN_POINT('Ctrl Pts',(105.8033193371,17.7007764758332,31.));
#93979=CARTESIAN_POINT('Ctrl Pts',(105.8033193371,17.7007764758332,26.));
#93980=CARTESIAN_POINT('Ctrl Pts',(105.774279884316,17.7131338313612,31.));
#93981=CARTESIAN_POINT('Ctrl Pts',(105.774279884316,17.7131338313612,26.));
#93982=CARTESIAN_POINT('Ctrl Pts',(105.744969939469,17.7261866797139,31.));
#93983=CARTESIAN_POINT('Ctrl Pts',(105.744969939469,17.7261866797139,26.));
#93984=CARTESIAN_POINT('Ctrl Pts',(105.715410367441,17.7399403609466,31.));
#93985=CARTESIAN_POINT('Ctrl Pts',(105.715410367441,17.7399403609466,26.));
#93986=CARTESIAN_POINT('Ctrl Pts',(105.685615951231,17.7543993570954,31.));
#93987=CARTESIAN_POINT('Ctrl Pts',(105.685615951231,17.7543993570954,26.));
#93988=CARTESIAN_POINT('Ctrl Pts',(105.655597099378,17.7695664156946,31.));
#93989=CARTESIAN_POINT('Ctrl Pts',(105.655597099378,17.7695664156946,26.));
#93990=CARTESIAN_POINT('Ctrl Pts',(105.625361451531,17.7854413074674,31.));
#93991=CARTESIAN_POINT('Ctrl Pts',(105.625361451531,17.7854413074674,26.));
#93992=CARTESIAN_POINT('Ctrl Pts',(105.594915191446,17.8020202408531,31.));
#93993=CARTESIAN_POINT('Ctrl Pts',(105.594915191446,17.8020202408531,26.));
#93994=CARTESIAN_POINT('Ctrl Pts',(105.564262914511,17.8192978118943,31.));
#93995=CARTESIAN_POINT('Ctrl Pts',(105.564262914511,17.8192978118943,26.));
#93996=CARTESIAN_POINT('Ctrl Pts',(105.539578802719,17.8336742790972,31.));
#93997=CARTESIAN_POINT('Ctrl Pts',(105.539578802719,17.8336742790972,26.));
#93998=CARTESIAN_POINT('Ctrl Pts',(105.520975232293,17.8447665109225,31.));
#93999=CARTESIAN_POINT('Ctrl Pts',(105.520975232293,17.8447665109225,26.));
#94000=CARTESIAN_POINT('Ctrl Pts',(105.508532708783,17.8522988075826,31.));
#94001=CARTESIAN_POINT('Ctrl Pts',(105.508532708783,17.8522988075826,26.));
#94002=CARTESIAN_POINT('Ctrl Pts',(105.502301411201,17.8560993248145,31.));
#94003=CARTESIAN_POINT('Ctrl Pts',(105.502301411201,17.8560993248145,26.));
#94004=CARTESIAN_POINT('Ctrl Pts',(106.263161448981,17.5945457010101,31.));
#94005=CARTESIAN_POINT('Ctrl Pts',(106.260815767337,17.5943356095479,31.));
#94006=CARTESIAN_POINT('Ctrl Pts',(106.255960106942,17.593975228822,31.));
#94007=CARTESIAN_POINT('Ctrl Pts',(106.248183719866,17.5936140643173,31.));
#94008=CARTESIAN_POINT('Ctrl Pts',(106.236827670445,17.5934919745854,31.));
#94009=CARTESIAN_POINT('Ctrl Pts',(106.220988653687,17.5939428717324,31.));
#94010=CARTESIAN_POINT('Ctrl Pts',(106.203530498282,17.5950039036334,31.));
#94011=CARTESIAN_POINT('Ctrl Pts',(106.184515373837,17.5966833027395,31.));
#94012=CARTESIAN_POINT('Ctrl Pts',(106.164063459768,17.5989901474915,31.));
#94013=CARTESIAN_POINT('Ctrl Pts',(106.142356391658,17.6019337055115,31.));
#94014=CARTESIAN_POINT('Ctrl Pts',(106.119603340517,17.6055231461002,31.));
#94015=CARTESIAN_POINT('Ctrl Pts',(106.096013944054,17.6097670199654,31.));
#94016=CARTESIAN_POINT('Ctrl Pts',(106.071771416337,17.6146727719589,31.));
#94017=CARTESIAN_POINT('Ctrl Pts',(106.046999325018,17.6202458885881,31.));
#94018=CARTESIAN_POINT('Ctrl Pts',(106.021754326667,17.6264897902966,31.));
#94019=CARTESIAN_POINT('Ctrl Pts',(105.996051211954,17.6334066554725,31.));
#94020=CARTESIAN_POINT('Ctrl Pts',(105.969880106239,17.640997861563,31.));
#94021=CARTESIAN_POINT('Ctrl Pts',(105.943225285516,17.6492644420914,31.));
#94022=CARTESIAN_POINT('Ctrl Pts',(105.916086843341,17.6582073520301,31.));
#94023=CARTESIAN_POINT('Ctrl Pts',(105.88848788051,17.667827787931,31.));
#94024=CARTESIAN_POINT('Ctrl Pts',(105.860464470601,17.6781275448521,31.));
#94025=CARTESIAN_POINT('Ctrl Pts',(105.832060188363,17.6891092499218,31.));
#94026=CARTESIAN_POINT('Ctrl Pts',(105.8033193371,17.7007764758332,31.));
#94027=CARTESIAN_POINT('Ctrl Pts',(105.774279884316,17.7131338313612,31.));
#94028=CARTESIAN_POINT('Ctrl Pts',(105.744969939469,17.7261866797139,31.));
#94029=CARTESIAN_POINT('Ctrl Pts',(105.715410367441,17.7399403609466,31.));
#94030=CARTESIAN_POINT('Ctrl Pts',(105.685615951231,17.7543993570954,31.));
#94031=CARTESIAN_POINT('Ctrl Pts',(105.655597099378,17.7695664156946,31.));
#94032=CARTESIAN_POINT('Ctrl Pts',(105.625361451531,17.7854413074674,31.));
#94033=CARTESIAN_POINT('Ctrl Pts',(105.594915191446,17.8020202408531,31.));
#94034=CARTESIAN_POINT('Ctrl Pts',(105.564262914511,17.8192978118943,31.));
#94035=CARTESIAN_POINT('Ctrl Pts',(105.539578802719,17.8336742790972,31.));
#94036=CARTESIAN_POINT('Ctrl Pts',(105.520975232293,17.8447665109225,31.));
#94037=CARTESIAN_POINT('Ctrl Pts',(105.508532708783,17.8522988075826,31.));
#94038=CARTESIAN_POINT('Ctrl Pts',(105.502301411201,17.8560993248145,31.));
#94039=CARTESIAN_POINT('Ctrl Pts',(106.263161448981,17.5945457010101,26.));
#94040=CARTESIAN_POINT('Ctrl Pts',(106.260815767337,17.5943356095479,26.));
#94041=CARTESIAN_POINT('Ctrl Pts',(106.255960106942,17.593975228822,26.));
#94042=CARTESIAN_POINT('Ctrl Pts',(106.248183719866,17.5936140643173,26.));
#94043=CARTESIAN_POINT('Ctrl Pts',(106.236827670445,17.5934919745854,26.));
#94044=CARTESIAN_POINT('Ctrl Pts',(106.220988653687,17.5939428717324,26.));
#94045=CARTESIAN_POINT('Ctrl Pts',(106.203530498282,17.5950039036334,26.));
#94046=CARTESIAN_POINT('Ctrl Pts',(106.184515373837,17.5966833027395,26.));
#94047=CARTESIAN_POINT('Ctrl Pts',(106.164063459768,17.5989901474915,26.));
#94048=CARTESIAN_POINT('Ctrl Pts',(106.142356391658,17.6019337055115,26.));
#94049=CARTESIAN_POINT('Ctrl Pts',(106.119603340517,17.6055231461002,26.));
#94050=CARTESIAN_POINT('Ctrl Pts',(106.096013944054,17.6097670199654,26.));
#94051=CARTESIAN_POINT('Ctrl Pts',(106.071771416337,17.6146727719589,26.));
#94052=CARTESIAN_POINT('Ctrl Pts',(106.046999325018,17.6202458885881,26.));
#94053=CARTESIAN_POINT('Ctrl Pts',(106.021754326667,17.6264897902966,26.));
#94054=CARTESIAN_POINT('Ctrl Pts',(105.996051211954,17.6334066554725,26.));
#94055=CARTESIAN_POINT('Ctrl Pts',(105.969880106239,17.640997861563,26.));
#94056=CARTESIAN_POINT('Ctrl Pts',(105.943225285516,17.6492644420914,26.));
#94057=CARTESIAN_POINT('Ctrl Pts',(105.916086843341,17.6582073520301,26.));
#94058=CARTESIAN_POINT('Ctrl Pts',(105.88848788051,17.667827787931,26.));
#94059=CARTESIAN_POINT('Ctrl Pts',(105.860464470601,17.6781275448521,26.));
#94060=CARTESIAN_POINT('Ctrl Pts',(105.832060188363,17.6891092499218,26.));
#94061=CARTESIAN_POINT('Ctrl Pts',(105.8033193371,17.7007764758332,26.));
#94062=CARTESIAN_POINT('Ctrl Pts',(105.774279884316,17.7131338313612,26.));
#94063=CARTESIAN_POINT('Ctrl Pts',(105.744969939469,17.7261866797139,26.));
#94064=CARTESIAN_POINT('Ctrl Pts',(105.715410367441,17.7399403609466,26.));
#94065=CARTESIAN_POINT('Ctrl Pts',(105.685615951231,17.7543993570954,26.));
#94066=CARTESIAN_POINT('Ctrl Pts',(105.655597099378,17.7695664156946,26.));
#94067=CARTESIAN_POINT('Ctrl Pts',(105.625361451531,17.7854413074674,26.));
#94068=CARTESIAN_POINT('Ctrl Pts',(105.594915191446,17.8020202408531,26.));
#94069=CARTESIAN_POINT('Ctrl Pts',(105.564262914511,17.8192978118943,26.));
#94070=CARTESIAN_POINT('Ctrl Pts',(105.539578802719,17.8336742790972,26.));
#94071=CARTESIAN_POINT('Ctrl Pts',(105.520975232293,17.8447665109225,26.));
#94072=CARTESIAN_POINT('Ctrl Pts',(105.508532708783,17.8522988075826,26.));
#94073=CARTESIAN_POINT('Ctrl Pts',(105.502301411201,17.8560993248145,26.));
#94074=CARTESIAN_POINT('Origin',(106.146908725728,17.999999999984,31.));
#94075=CARTESIAN_POINT('Origin',(106.904746769447,18.9055564249396,31.));
#94076=CARTESIAN_POINT('',(106.39245070361,19.0554352746927,31.));
#94077=CARTESIAN_POINT('',(106.39245070361,19.0554352746927,31.));
#94078=CARTESIAN_POINT('',(106.39245070361,19.0554352746927,26.));
#94079=CARTESIAN_POINT('',(106.39245070361,19.0554352746927,31.));
#94080=CARTESIAN_POINT('',(106.39245070361,19.0554352746927,26.));
#94081=CARTESIAN_POINT('Origin',(106.702771989219,19.8046171311037,31.));
#94082=CARTESIAN_POINT('',(106.702771989219,19.8046171311037,26.));
#94083=CARTESIAN_POINT('',(107.171000362364,19.548349459992,26.));
#94084=CARTESIAN_POINT('',(106.702771989219,19.8046171311037,31.));
#94085=CARTESIAN_POINT('',(106.702771989219,19.8046171311037,31.));
#94086=CARTESIAN_POINT('',(107.171000362364,19.548349459992,31.));
#94087=CARTESIAN_POINT('Ctrl Pts',(105.899736734704,19.8541416222235,31.));
#94088=CARTESIAN_POINT('Ctrl Pts',(105.899736734704,19.8541416222235,26.));
#94089=CARTESIAN_POINT('Ctrl Pts',(105.906948098,19.8552682280105,31.));
#94090=CARTESIAN_POINT('Ctrl Pts',(105.906948098,19.8552682280105,26.));
#94091=CARTESIAN_POINT('Ctrl Pts',(105.921325975979,19.8574656152097,31.));
#94092=CARTESIAN_POINT('Ctrl Pts',(105.921325975979,19.8574656152097,26.));
#94093=CARTESIAN_POINT('Ctrl Pts',(105.942758247312,19.8605942230657,31.));
#94094=CARTESIAN_POINT('Ctrl Pts',(105.942758247312,19.8605942230657,26.));
#94095=CARTESIAN_POINT('Ctrl Pts',(105.971065028804,19.8644301462764,31.));
#94096=CARTESIAN_POINT('Ctrl Pts',(105.971065028804,19.8644301462764,26.));
#94097=CARTESIAN_POINT('Ctrl Pts',(106.005995880259,19.8686624219385,31.));
#94098=CARTESIAN_POINT('Ctrl Pts',(106.005995880259,19.8686624219385,26.));
#94099=CARTESIAN_POINT('Ctrl Pts',(106.040469039886,19.8723280797549,31.));
#94100=CARTESIAN_POINT('Ctrl Pts',(106.040469039886,19.8723280797549,26.));
#94101=CARTESIAN_POINT('Ctrl Pts',(106.074478194113,19.8754238857432,31.));
#94102=CARTESIAN_POINT('Ctrl Pts',(106.074478194113,19.8754238857432,26.));
#94103=CARTESIAN_POINT('Ctrl Pts',(106.108016178941,19.8779487034129,31.));
#94104=CARTESIAN_POINT('Ctrl Pts',(106.108016178941,19.8779487034129,26.));
#94105=CARTESIAN_POINT('Ctrl Pts',(106.141075848522,19.8799052445217,31.));
#94106=CARTESIAN_POINT('Ctrl Pts',(106.141075848522,19.8799052445217,26.));
#94107=CARTESIAN_POINT('Ctrl Pts',(106.173648638053,19.8813000306331,31.));
#94108=CARTESIAN_POINT('Ctrl Pts',(106.173648638053,19.8813000306331,26.));
#94109=CARTESIAN_POINT('Ctrl Pts',(106.20572260502,19.8821428598039,31.));
#94110=CARTESIAN_POINT('Ctrl Pts',(106.20572260502,19.8821428598039,26.));
#94111=CARTESIAN_POINT('Ctrl Pts',(106.237280516328,19.8824466502299,31.));
#94112=CARTESIAN_POINT('Ctrl Pts',(106.237280516328,19.8824466502299,26.));
#94113=CARTESIAN_POINT('Ctrl Pts',(106.26829845463,19.8822271138752,31.));
#94114=CARTESIAN_POINT('Ctrl Pts',(106.26829845463,19.8822271138752,26.));
#94115=CARTESIAN_POINT('Ctrl Pts',(106.298743106222,19.8815030382192,31.));
#94116=CARTESIAN_POINT('Ctrl Pts',(106.298743106222,19.8815030382192,26.));
#94117=CARTESIAN_POINT('Ctrl Pts',(106.328574907399,19.8802946781383,31.));
#94118=CARTESIAN_POINT('Ctrl Pts',(106.328574907399,19.8802946781383,26.));
#94119=CARTESIAN_POINT('Ctrl Pts',(106.357754605704,19.8786211361218,31.));
#94120=CARTESIAN_POINT('Ctrl Pts',(106.357754605704,19.8786211361218,26.));
#94121=CARTESIAN_POINT('Ctrl Pts',(106.386249560435,19.8764978753546,31.));
#94122=CARTESIAN_POINT('Ctrl Pts',(106.386249560435,19.8764978753546,26.));
#94123=CARTESIAN_POINT('Ctrl Pts',(106.414038887147,19.8739348416065,31.));
#94124=CARTESIAN_POINT('Ctrl Pts',(106.414038887147,19.8739348416065,26.));
#94125=CARTESIAN_POINT('Ctrl Pts',(106.441122864858,19.8709329529652,31.));
#94126=CARTESIAN_POINT('Ctrl Pts',(106.441122864858,19.8709329529652,26.));
#94127=CARTESIAN_POINT('Ctrl Pts',(106.467516416169,19.8674871469678,31.));
#94128=CARTESIAN_POINT('Ctrl Pts',(106.467516416169,19.8674871469678,26.));
#94129=CARTESIAN_POINT('Ctrl Pts',(106.493229191184,19.8635949173464,31.));
#94130=CARTESIAN_POINT('Ctrl Pts',(106.493229191184,19.8635949173464,26.));
#94131=CARTESIAN_POINT('Ctrl Pts',(106.518248358736,19.8592639368112,31.));
#94132=CARTESIAN_POINT('Ctrl Pts',(106.518248358736,19.8592639368112,26.));
#94133=CARTESIAN_POINT('Ctrl Pts',(106.542522883926,19.8545190469672,31.));
#94134=CARTESIAN_POINT('Ctrl Pts',(106.542522883926,19.8545190469672,26.));
#94135=CARTESIAN_POINT('Ctrl Pts',(106.565940704725,19.8494126039752,31.));
#94136=CARTESIAN_POINT('Ctrl Pts',(106.565940704725,19.8494126039752,26.));
#94137=CARTESIAN_POINT('Ctrl Pts',(106.588335402423,19.8440215989653,31.));
#94138=CARTESIAN_POINT('Ctrl Pts',(106.588335402423,19.8440215989653,26.));
#94139=CARTESIAN_POINT('Ctrl Pts',(106.609516569245,19.838434156637,31.));
#94140=CARTESIAN_POINT('Ctrl Pts',(106.609516569245,19.838434156637,26.));
#94141=CARTESIAN_POINT('Ctrl Pts',(106.629294465316,19.8327387946007,31.));
#94142=CARTESIAN_POINT('Ctrl Pts',(106.629294465316,19.8327387946007,26.));
#94143=CARTESIAN_POINT('Ctrl Pts',(106.647504827807,19.8270135839562,31.));
#94144=CARTESIAN_POINT('Ctrl Pts',(106.647504827807,19.8270135839562,26.));
#94145=CARTESIAN_POINT('Ctrl Pts',(106.664040099586,19.821312902766,31.));
#94146=CARTESIAN_POINT('Ctrl Pts',(106.664040099586,19.821312902766,26.));
#94147=CARTESIAN_POINT('Ctrl Pts',(106.67884599385,19.8156681481077,31.));
#94148=CARTESIAN_POINT('Ctrl Pts',(106.67884599385,19.8156681481077,26.));
#94149=CARTESIAN_POINT('Ctrl Pts',(106.689290893764,19.811209579937,31.));
#94150=CARTESIAN_POINT('Ctrl Pts',(106.689290893764,19.811209579937,26.));
#94151=CARTESIAN_POINT('Ctrl Pts',(106.696337126951,19.8079000129555,31.));
#94152=CARTESIAN_POINT('Ctrl Pts',(106.696337126951,19.8079000129555,26.));
#94153=CARTESIAN_POINT('Ctrl Pts',(106.700685260478,19.8057088838026,31.));
#94154=CARTESIAN_POINT('Ctrl Pts',(106.700685260478,19.8057088838026,26.));
#94155=CARTESIAN_POINT('Ctrl Pts',(106.702771989219,19.8046171311037,31.));
#94156=CARTESIAN_POINT('Ctrl Pts',(106.702771989219,19.8046171311037,26.));
#94157=CARTESIAN_POINT('',(105.899736734704,19.8541416222235,31.));
#94158=CARTESIAN_POINT('Ctrl Pts',(106.702771989219,19.8046171311037,31.));
#94159=CARTESIAN_POINT('Ctrl Pts',(106.700685260478,19.8057088838026,31.));
#94160=CARTESIAN_POINT('Ctrl Pts',(106.696337126951,19.8079000129555,31.));
#94161=CARTESIAN_POINT('Ctrl Pts',(106.689290893764,19.811209579937,31.));
#94162=CARTESIAN_POINT('Ctrl Pts',(106.67884599385,19.8156681481077,31.));
#94163=CARTESIAN_POINT('Ctrl Pts',(106.664040099586,19.821312902766,31.));
#94164=CARTESIAN_POINT('Ctrl Pts',(106.647504827807,19.8270135839562,31.));
#94165=CARTESIAN_POINT('Ctrl Pts',(106.629294465316,19.8327387946007,31.));
#94166=CARTESIAN_POINT('Ctrl Pts',(106.609516569245,19.838434156637,31.));
#94167=CARTESIAN_POINT('Ctrl Pts',(106.588335402423,19.8440215989653,31.));
#94168=CARTESIAN_POINT('Ctrl Pts',(106.565940704725,19.8494126039752,31.));
#94169=CARTESIAN_POINT('Ctrl Pts',(106.542522883926,19.8545190469672,31.));
#94170=CARTESIAN_POINT('Ctrl Pts',(106.518248358736,19.8592639368112,31.));
#94171=CARTESIAN_POINT('Ctrl Pts',(106.493229191184,19.8635949173464,31.));
#94172=CARTESIAN_POINT('Ctrl Pts',(106.467516416169,19.8674871469678,31.));
#94173=CARTESIAN_POINT('Ctrl Pts',(106.441122864858,19.8709329529652,31.));
#94174=CARTESIAN_POINT('Ctrl Pts',(106.414038887147,19.8739348416065,31.));
#94175=CARTESIAN_POINT('Ctrl Pts',(106.386249560435,19.8764978753546,31.));
#94176=CARTESIAN_POINT('Ctrl Pts',(106.357754605704,19.8786211361218,31.));
#94177=CARTESIAN_POINT('Ctrl Pts',(106.328574907399,19.8802946781383,31.));
#94178=CARTESIAN_POINT('Ctrl Pts',(106.298743106222,19.8815030382192,31.));
#94179=CARTESIAN_POINT('Ctrl Pts',(106.26829845463,19.8822271138752,31.));
#94180=CARTESIAN_POINT('Ctrl Pts',(106.237280516328,19.8824466502299,31.));
#94181=CARTESIAN_POINT('Ctrl Pts',(106.20572260502,19.8821428598039,31.));
#94182=CARTESIAN_POINT('Ctrl Pts',(106.173648638053,19.8813000306331,31.));
#94183=CARTESIAN_POINT('Ctrl Pts',(106.141075848522,19.8799052445217,31.));
#94184=CARTESIAN_POINT('Ctrl Pts',(106.108016178941,19.8779487034129,31.));
#94185=CARTESIAN_POINT('Ctrl Pts',(106.074478194113,19.8754238857432,31.));
#94186=CARTESIAN_POINT('Ctrl Pts',(106.040469039886,19.8723280797549,31.));
#94187=CARTESIAN_POINT('Ctrl Pts',(106.005995880259,19.8686624219385,31.));
#94188=CARTESIAN_POINT('Ctrl Pts',(105.971065028804,19.8644301462764,31.));
#94189=CARTESIAN_POINT('Ctrl Pts',(105.942758247312,19.8605942230657,31.));
#94190=CARTESIAN_POINT('Ctrl Pts',(105.921325975979,19.8574656152097,31.));
#94191=CARTESIAN_POINT('Ctrl Pts',(105.906948098,19.8552682280105,31.));
#94192=CARTESIAN_POINT('Ctrl Pts',(105.899736734704,19.8541416222235,31.));
#94193=CARTESIAN_POINT('',(105.899736734704,19.8541416222235,26.));
#94194=CARTESIAN_POINT('Ctrl Pts',(105.899736734704,19.8541416222235,26.));
#94195=CARTESIAN_POINT('Ctrl Pts',(105.906948098,19.8552682280105,26.));
#94196=CARTESIAN_POINT('Ctrl Pts',(105.921325975979,19.8574656152097,26.));
#94197=CARTESIAN_POINT('Ctrl Pts',(105.942758247312,19.8605942230657,26.));
#94198=CARTESIAN_POINT('Ctrl Pts',(105.971065028804,19.8644301462764,26.));
#94199=CARTESIAN_POINT('Ctrl Pts',(106.005995880259,19.8686624219385,26.));
#94200=CARTESIAN_POINT('Ctrl Pts',(106.040469039886,19.8723280797549,26.));
#94201=CARTESIAN_POINT('Ctrl Pts',(106.074478194113,19.8754238857432,26.));
#94202=CARTESIAN_POINT('Ctrl Pts',(106.108016178941,19.8779487034129,26.));
#94203=CARTESIAN_POINT('Ctrl Pts',(106.141075848522,19.8799052445217,26.));
#94204=CARTESIAN_POINT('Ctrl Pts',(106.173648638053,19.8813000306331,26.));
#94205=CARTESIAN_POINT('Ctrl Pts',(106.20572260502,19.8821428598039,26.));
#94206=CARTESIAN_POINT('Ctrl Pts',(106.237280516328,19.8824466502299,26.));
#94207=CARTESIAN_POINT('Ctrl Pts',(106.26829845463,19.8822271138752,26.));
#94208=CARTESIAN_POINT('Ctrl Pts',(106.298743106222,19.8815030382192,26.));
#94209=CARTESIAN_POINT('Ctrl Pts',(106.328574907399,19.8802946781383,26.));
#94210=CARTESIAN_POINT('Ctrl Pts',(106.357754605704,19.8786211361218,26.));
#94211=CARTESIAN_POINT('Ctrl Pts',(106.386249560435,19.8764978753546,26.));
#94212=CARTESIAN_POINT('Ctrl Pts',(106.414038887147,19.8739348416065,26.));
#94213=CARTESIAN_POINT('Ctrl Pts',(106.441122864858,19.8709329529652,26.));
#94214=CARTESIAN_POINT('Ctrl Pts',(106.467516416169,19.8674871469678,26.));
#94215=CARTESIAN_POINT('Ctrl Pts',(106.493229191184,19.8635949173464,26.));
#94216=CARTESIAN_POINT('Ctrl Pts',(106.518248358736,19.8592639368112,26.));
#94217=CARTESIAN_POINT('Ctrl Pts',(106.542522883926,19.8545190469672,26.));
#94218=CARTESIAN_POINT('Ctrl Pts',(106.565940704725,19.8494126039752,26.));
#94219=CARTESIAN_POINT('Ctrl Pts',(106.588335402423,19.8440215989653,26.));
#94220=CARTESIAN_POINT('Ctrl Pts',(106.609516569245,19.838434156637,26.));
#94221=CARTESIAN_POINT('Ctrl Pts',(106.629294465316,19.8327387946007,26.));
#94222=CARTESIAN_POINT('Ctrl Pts',(106.647504827807,19.8270135839562,26.));
#94223=CARTESIAN_POINT('Ctrl Pts',(106.664040099586,19.821312902766,26.));
#94224=CARTESIAN_POINT('Ctrl Pts',(106.67884599385,19.8156681481077,26.));
#94225=CARTESIAN_POINT('Ctrl Pts',(106.689290893764,19.811209579937,26.));
#94226=CARTESIAN_POINT('Ctrl Pts',(106.696337126951,19.8079000129555,26.));
#94227=CARTESIAN_POINT('Ctrl Pts',(106.700685260478,19.8057088838026,26.));
#94228=CARTESIAN_POINT('Ctrl Pts',(106.702771989219,19.8046171311037,26.));
#94229=CARTESIAN_POINT('',(105.899736734704,19.8541416222235,31.));
#94230=CARTESIAN_POINT('Origin',(110.000000000003,17.9999999999989,31.));
#94231=CARTESIAN_POINT('',(105.789599926104,19.5882478451867,31.));
#94232=CARTESIAN_POINT('Origin',(110.000000000003,17.9999999999989,31.));
#94233=CARTESIAN_POINT('',(105.789599926104,19.5882478451867,26.));
#94234=CARTESIAN_POINT('Origin',(110.000000000003,17.9999999999989,26.));
#94235=CARTESIAN_POINT('',(105.789599926104,19.5882478451867,31.));
#94236=CARTESIAN_POINT('Ctrl Pts',(106.39245070361,19.0554352746927,31.));
#94237=CARTESIAN_POINT('Ctrl Pts',(106.39245070361,19.0554352746927,26.));
#94238=CARTESIAN_POINT('Ctrl Pts',(106.390203177827,19.0561388289937,31.));
#94239=CARTESIAN_POINT('Ctrl Pts',(106.390203177827,19.0561388289937,26.));
#94240=CARTESIAN_POINT('Ctrl Pts',(106.385579220838,19.0576640614035,31.));
#94241=CARTESIAN_POINT('Ctrl Pts',(106.385579220838,19.0576640614035,26.));
#94242=CARTESIAN_POINT('Ctrl Pts',(106.37825656431,19.0603062834071,31.));
#94243=CARTESIAN_POINT('Ctrl Pts',(106.37825656431,19.0603062834071,26.));
#94244=CARTESIAN_POINT('Ctrl Pts',(106.367718220961,19.0645392591734,31.));
#94245=CARTESIAN_POINT('Ctrl Pts',(106.367718220961,19.0645392591734,26.));
#94246=CARTESIAN_POINT('Ctrl Pts',(106.353257428432,19.0710171631169,31.));
#94247=CARTESIAN_POINT('Ctrl Pts',(106.353257428432,19.0710171631169,26.));
#94248=CARTESIAN_POINT('Ctrl Pts',(106.337534235307,19.0786783756069,31.));
#94249=CARTESIAN_POINT('Ctrl Pts',(106.337534235307,19.0786783756069,26.));
#94250=CARTESIAN_POINT('Ctrl Pts',(106.320609229239,19.0875067111573,31.));
#94251=CARTESIAN_POINT('Ctrl Pts',(106.320609229239,19.0875067111573,26.));
#94252=CARTESIAN_POINT('Ctrl Pts',(106.302596915698,19.0974645664826,31.));
#94253=CARTESIAN_POINT('Ctrl Pts',(106.302596915698,19.0974645664826,26.));
#94254=CARTESIAN_POINT('Ctrl Pts',(106.283668650646,19.108490994821,31.));
#94255=CARTESIAN_POINT('Ctrl Pts',(106.283668650646,19.108490994821,26.));
#94256=CARTESIAN_POINT('Ctrl Pts',(106.26402119184,19.1205144212215,31.));
#94257=CARTESIAN_POINT('Ctrl Pts',(106.26402119184,19.1205144212215,26.));
#94258=CARTESIAN_POINT('Ctrl Pts',(106.24385149148,19.1334625206302,31.));
#94259=CARTESIAN_POINT('Ctrl Pts',(106.24385149148,19.1334625206302,26.));
#94260=CARTESIAN_POINT('Ctrl Pts',(106.223331666318,19.1472720582043,31.));
#94261=CARTESIAN_POINT('Ctrl Pts',(106.223331666318,19.1472720582043,26.));
#94262=CARTESIAN_POINT('Ctrl Pts',(106.202577977571,19.1619008155231,31.));
#94263=CARTESIAN_POINT('Ctrl Pts',(106.202577977571,19.1619008155231,26.));
#94264=CARTESIAN_POINT('Ctrl Pts',(106.181644078033,19.1773302711338,31.));
#94265=CARTESIAN_POINT('Ctrl Pts',(106.181644078033,19.1773302711338,26.));
#94266=CARTESIAN_POINT('Ctrl Pts',(106.160544466135,19.1935567774596,31.));
#94267=CARTESIAN_POINT('Ctrl Pts',(106.160544466135,19.1935567774596,26.));
#94268=CARTESIAN_POINT('Ctrl Pts',(106.139270546025,19.2105853859574,31.));
#94269=CARTESIAN_POINT('Ctrl Pts',(106.139270546025,19.2105853859574,26.));
#94270=CARTESIAN_POINT('Ctrl Pts',(106.117808186126,19.228423068795,31.));
#94271=CARTESIAN_POINT('Ctrl Pts',(106.117808186126,19.228423068795,26.));
#94272=CARTESIAN_POINT('Ctrl Pts',(106.096157838327,19.2470706724489,31.));
#94273=CARTESIAN_POINT('Ctrl Pts',(106.096157838327,19.2470706724489,26.));
#94274=CARTESIAN_POINT('Ctrl Pts',(106.07434130288,19.2665204620976,31.));
#94275=CARTESIAN_POINT('Ctrl Pts',(106.07434130288,19.2665204620976,26.));
#94276=CARTESIAN_POINT('Ctrl Pts',(106.052392594365,19.2867602913975,31.));
#94277=CARTESIAN_POINT('Ctrl Pts',(106.052392594365,19.2867602913975,26.));
#94278=CARTESIAN_POINT('Ctrl Pts',(106.030352975959,19.3077759121639,31.));
#94279=CARTESIAN_POINT('Ctrl Pts',(106.030352975959,19.3077759121639,26.));
#94280=CARTESIAN_POINT('Ctrl Pts',(106.008264745788,19.3295536709952,31.));
#94281=CARTESIAN_POINT('Ctrl Pts',(106.008264745788,19.3295536709952,26.));
#94282=CARTESIAN_POINT('Ctrl Pts',(105.986164744955,19.3520832963087,31.));
#94283=CARTESIAN_POINT('Ctrl Pts',(105.986164744955,19.3520832963087,26.));
#94284=CARTESIAN_POINT('Ctrl Pts',(105.964080995621,19.3753589860392,31.));
#94285=CARTESIAN_POINT('Ctrl Pts',(105.964080995621,19.3753589860392,26.));
#94286=CARTESIAN_POINT('Ctrl Pts',(105.942034817977,19.3993776891096,31.));
#94287=CARTESIAN_POINT('Ctrl Pts',(105.942034817977,19.3993776891096,26.));
#94288=CARTESIAN_POINT('Ctrl Pts',(105.920041584931,19.4241378891729,31.));
#94289=CARTESIAN_POINT('Ctrl Pts',(105.920041584931,19.4241378891729,26.));
#94290=CARTESIAN_POINT('Ctrl Pts',(105.898111964159,19.4496381414438,31.));
#94291=CARTESIAN_POINT('Ctrl Pts',(105.898111964159,19.4496381414438,26.));
#94292=CARTESIAN_POINT('Ctrl Pts',(105.876252926033,19.4758753105314,31.));
#94293=CARTESIAN_POINT('Ctrl Pts',(105.876252926033,19.4758753105314,26.));
#94294=CARTESIAN_POINT('Ctrl Pts',(105.854468732632,19.5028435270694,31.));
#94295=CARTESIAN_POINT('Ctrl Pts',(105.854468732632,19.5028435270694,26.));
#94296=CARTESIAN_POINT('Ctrl Pts',(105.832761561535,19.5305360398732,31.));
#94297=CARTESIAN_POINT('Ctrl Pts',(105.832761561535,19.5305360398732,26.));
#94298=CARTESIAN_POINT('Ctrl Pts',(105.815458051687,19.5532643642971,31.));
#94299=CARTESIAN_POINT('Ctrl Pts',(105.815458051687,19.5532643642971,26.));
#94300=CARTESIAN_POINT('Ctrl Pts',(105.802515407086,19.5706315284352,31.));
#94301=CARTESIAN_POINT('Ctrl Pts',(105.802515407086,19.5706315284352,26.));
#94302=CARTESIAN_POINT('Ctrl Pts',(105.793902499422,19.5823520107564,31.));
#94303=CARTESIAN_POINT('Ctrl Pts',(105.793902499422,19.5823520107564,26.));
#94304=CARTESIAN_POINT('Ctrl Pts',(105.789599926104,19.5882478451867,31.));
#94305=CARTESIAN_POINT('Ctrl Pts',(105.789599926104,19.5882478451867,26.));
#94306=CARTESIAN_POINT('Ctrl Pts',(106.39245070361,19.0554352746927,31.));
#94307=CARTESIAN_POINT('Ctrl Pts',(106.390203177827,19.0561388289937,31.));
#94308=CARTESIAN_POINT('Ctrl Pts',(106.385579220838,19.0576640614035,31.));
#94309=CARTESIAN_POINT('Ctrl Pts',(106.37825656431,19.0603062834071,31.));
#94310=CARTESIAN_POINT('Ctrl Pts',(106.367718220961,19.0645392591734,31.));
#94311=CARTESIAN_POINT('Ctrl Pts',(106.353257428432,19.0710171631169,31.));
#94312=CARTESIAN_POINT('Ctrl Pts',(106.337534235307,19.0786783756069,31.));
#94313=CARTESIAN_POINT('Ctrl Pts',(106.320609229239,19.0875067111573,31.));
#94314=CARTESIAN_POINT('Ctrl Pts',(106.302596915698,19.0974645664826,31.));
#94315=CARTESIAN_POINT('Ctrl Pts',(106.283668650646,19.108490994821,31.));
#94316=CARTESIAN_POINT('Ctrl Pts',(106.26402119184,19.1205144212215,31.));
#94317=CARTESIAN_POINT('Ctrl Pts',(106.24385149148,19.1334625206302,31.));
#94318=CARTESIAN_POINT('Ctrl Pts',(106.223331666318,19.1472720582043,31.));
#94319=CARTESIAN_POINT('Ctrl Pts',(106.202577977571,19.1619008155231,31.));
#94320=CARTESIAN_POINT('Ctrl Pts',(106.181644078033,19.1773302711338,31.));
#94321=CARTESIAN_POINT('Ctrl Pts',(106.160544466135,19.1935567774596,31.));
#94322=CARTESIAN_POINT('Ctrl Pts',(106.139270546025,19.2105853859574,31.));
#94323=CARTESIAN_POINT('Ctrl Pts',(106.117808186126,19.228423068795,31.));
#94324=CARTESIAN_POINT('Ctrl Pts',(106.096157838327,19.2470706724489,31.));
#94325=CARTESIAN_POINT('Ctrl Pts',(106.07434130288,19.2665204620976,31.));
#94326=CARTESIAN_POINT('Ctrl Pts',(106.052392594365,19.2867602913975,31.));
#94327=CARTESIAN_POINT('Ctrl Pts',(106.030352975959,19.3077759121639,31.));
#94328=CARTESIAN_POINT('Ctrl Pts',(106.008264745788,19.3295536709952,31.));
#94329=CARTESIAN_POINT('Ctrl Pts',(105.986164744955,19.3520832963087,31.));
#94330=CARTESIAN_POINT('Ctrl Pts',(105.964080995621,19.3753589860392,31.));
#94331=CARTESIAN_POINT('Ctrl Pts',(105.942034817977,19.3993776891096,31.));
#94332=CARTESIAN_POINT('Ctrl Pts',(105.920041584931,19.4241378891729,31.));
#94333=CARTESIAN_POINT('Ctrl Pts',(105.898111964159,19.4496381414438,31.));
#94334=CARTESIAN_POINT('Ctrl Pts',(105.876252926033,19.4758753105314,31.));
#94335=CARTESIAN_POINT('Ctrl Pts',(105.854468732632,19.5028435270694,31.));
#94336=CARTESIAN_POINT('Ctrl Pts',(105.832761561535,19.5305360398732,31.));
#94337=CARTESIAN_POINT('Ctrl Pts',(105.815458051687,19.5532643642971,31.));
#94338=CARTESIAN_POINT('Ctrl Pts',(105.802515407086,19.5706315284352,31.));
#94339=CARTESIAN_POINT('Ctrl Pts',(105.793902499422,19.5823520107564,31.));
#94340=CARTESIAN_POINT('Ctrl Pts',(105.789599926104,19.5882478451867,31.));
#94341=CARTESIAN_POINT('Ctrl Pts',(106.39245070361,19.0554352746927,26.));
#94342=CARTESIAN_POINT('Ctrl Pts',(106.390203177827,19.0561388289937,26.));
#94343=CARTESIAN_POINT('Ctrl Pts',(106.385579220838,19.0576640614035,26.));
#94344=CARTESIAN_POINT('Ctrl Pts',(106.37825656431,19.0603062834071,26.));
#94345=CARTESIAN_POINT('Ctrl Pts',(106.367718220961,19.0645392591734,26.));
#94346=CARTESIAN_POINT('Ctrl Pts',(106.353257428432,19.0710171631169,26.));
#94347=CARTESIAN_POINT('Ctrl Pts',(106.337534235307,19.0786783756069,26.));
#94348=CARTESIAN_POINT('Ctrl Pts',(106.320609229239,19.0875067111573,26.));
#94349=CARTESIAN_POINT('Ctrl Pts',(106.302596915698,19.0974645664826,26.));
#94350=CARTESIAN_POINT('Ctrl Pts',(106.283668650646,19.108490994821,26.));
#94351=CARTESIAN_POINT('Ctrl Pts',(106.26402119184,19.1205144212215,26.));
#94352=CARTESIAN_POINT('Ctrl Pts',(106.24385149148,19.1334625206302,26.));
#94353=CARTESIAN_POINT('Ctrl Pts',(106.223331666318,19.1472720582043,26.));
#94354=CARTESIAN_POINT('Ctrl Pts',(106.202577977571,19.1619008155231,26.));
#94355=CARTESIAN_POINT('Ctrl Pts',(106.181644078033,19.1773302711338,26.));
#94356=CARTESIAN_POINT('Ctrl Pts',(106.160544466135,19.1935567774596,26.));
#94357=CARTESIAN_POINT('Ctrl Pts',(106.139270546025,19.2105853859574,26.));
#94358=CARTESIAN_POINT('Ctrl Pts',(106.117808186126,19.228423068795,26.));
#94359=CARTESIAN_POINT('Ctrl Pts',(106.096157838327,19.2470706724489,26.));
#94360=CARTESIAN_POINT('Ctrl Pts',(106.07434130288,19.2665204620976,26.));
#94361=CARTESIAN_POINT('Ctrl Pts',(106.052392594365,19.2867602913975,26.));
#94362=CARTESIAN_POINT('Ctrl Pts',(106.030352975959,19.3077759121639,26.));
#94363=CARTESIAN_POINT('Ctrl Pts',(106.008264745788,19.3295536709952,26.));
#94364=CARTESIAN_POINT('Ctrl Pts',(105.986164744955,19.3520832963087,26.));
#94365=CARTESIAN_POINT('Ctrl Pts',(105.964080995621,19.3753589860392,26.));
#94366=CARTESIAN_POINT('Ctrl Pts',(105.942034817977,19.3993776891096,26.));
#94367=CARTESIAN_POINT('Ctrl Pts',(105.920041584931,19.4241378891729,26.));
#94368=CARTESIAN_POINT('Ctrl Pts',(105.898111964159,19.4496381414438,26.));
#94369=CARTESIAN_POINT('Ctrl Pts',(105.876252926033,19.4758753105314,26.));
#94370=CARTESIAN_POINT('Ctrl Pts',(105.854468732632,19.5028435270694,26.));
#94371=CARTESIAN_POINT('Ctrl Pts',(105.832761561535,19.5305360398732,26.));
#94372=CARTESIAN_POINT('Ctrl Pts',(105.815458051687,19.5532643642971,26.));
#94373=CARTESIAN_POINT('Ctrl Pts',(105.802515407086,19.5706315284352,26.));
#94374=CARTESIAN_POINT('Ctrl Pts',(105.793902499422,19.5823520107564,26.));
#94375=CARTESIAN_POINT('Ctrl Pts',(105.789599926104,19.5882478451867,26.));
#94376=CARTESIAN_POINT('Origin',(106.440207834796,19.4745141940396,31.));
#94377=CARTESIAN_POINT('Origin',(107.486900333248,20.0211271768431,31.));
#94378=CARTESIAN_POINT('',(107.070956636098,20.3556443953479,31.));
#94379=CARTESIAN_POINT('',(107.070956636098,20.3556443953479,31.));
#94380=CARTESIAN_POINT('',(107.070956636098,20.3556443953479,26.));
#94381=CARTESIAN_POINT('',(107.070956636098,20.3556443953479,31.));
#94382=CARTESIAN_POINT('',(107.070956636098,20.3556443953479,26.));
#94383=CARTESIAN_POINT('Origin',(107.644355604652,20.9290433639019,31.));
#94384=CARTESIAN_POINT('',(107.644355604652,20.9290433639019,26.));
#94385=CARTESIAN_POINT('',(107.978872823157,20.5130996667515,26.));
#94386=CARTESIAN_POINT('',(107.644355604652,20.9290433639019,31.));
#94387=CARTESIAN_POINT('',(107.644355604652,20.9290433639019,31.));
#94388=CARTESIAN_POINT('',(107.978872823157,20.5130996667515,31.));
#94389=CARTESIAN_POINT('Ctrl Pts',(106.921399971368,21.2821063151137,31.));
#94390=CARTESIAN_POINT('Ctrl Pts',(106.921399971368,21.2821063151137,26.));
#94391=CARTESIAN_POINT('Ctrl Pts',(106.928493535689,21.2803874938831,31.));
#94392=CARTESIAN_POINT('Ctrl Pts',(106.928493535689,21.2803874938831,26.));
#94393=CARTESIAN_POINT('Ctrl Pts',(106.942617866551,21.2769154392463,31.));
#94394=CARTESIAN_POINT('Ctrl Pts',(106.942617866551,21.2769154392463,26.));
#94395=CARTESIAN_POINT('Ctrl Pts',(106.963615969762,21.2716041208528,31.));
#94396=CARTESIAN_POINT('Ctrl Pts',(106.963615969762,21.2716041208528,26.));
#94397=CARTESIAN_POINT('Ctrl Pts',(106.991235970075,21.2643155154947,31.));
#94398=CARTESIAN_POINT('Ctrl Pts',(106.991235970075,21.2643155154947,26.));
#94399=CARTESIAN_POINT('Ctrl Pts',(107.025127490565,21.2548581702248,31.));
#94400=CARTESIAN_POINT('Ctrl Pts',(107.025127490565,21.2548581702248,26.));
#94401=CARTESIAN_POINT('Ctrl Pts',(107.05837932368,21.2450524894041,31.));
#94402=CARTESIAN_POINT('Ctrl Pts',(107.05837932368,21.2450524894041,26.));
#94403=CARTESIAN_POINT('Ctrl Pts',(107.09098439885,21.2348979013219,31.));
#94404=CARTESIAN_POINT('Ctrl Pts',(107.09098439885,21.2348979013219,26.));
#94405=CARTESIAN_POINT('Ctrl Pts',(107.122935662486,21.2243960975415,31.));
#94406=CARTESIAN_POINT('Ctrl Pts',(107.122935662486,21.2243960975415,26.));
#94407=CARTESIAN_POINT('Ctrl Pts',(107.154227550431,21.2135523179983,31.));
#94408=CARTESIAN_POINT('Ctrl Pts',(107.154227550431,21.2135523179983,26.));
#94409=CARTESIAN_POINT('Ctrl Pts',(107.184854645532,21.2023758654395,31.));
#94410=CARTESIAN_POINT('Ctrl Pts',(107.184854645532,21.2023758654395,26.));
#94411=CARTESIAN_POINT('Ctrl Pts',(107.214809663899,21.1908803622914,31.));
#94412=CARTESIAN_POINT('Ctrl Pts',(107.214809663899,21.1908803622914,26.));
#94413=CARTESIAN_POINT('Ctrl Pts',(107.244081627808,21.1790843382305,31.));
#94414=CARTESIAN_POINT('Ctrl Pts',(107.244081627808,21.1790843382305,26.));
#94415=CARTESIAN_POINT('Ctrl Pts',(107.27265445322,21.1670114619914,31.));
#94416=CARTESIAN_POINT('Ctrl Pts',(107.27265445322,21.1670114619914,26.));
#94417=CARTESIAN_POINT('Ctrl Pts',(107.300504551943,21.1546918395446,31.));
#94418=CARTESIAN_POINT('Ctrl Pts',(107.300504551943,21.1546918395446,26.));
#94419=CARTESIAN_POINT('Ctrl Pts',(107.327603123085,21.1421593243297,31.));
#94420=CARTESIAN_POINT('Ctrl Pts',(107.327603123085,21.1421593243297,26.));
#94421=CARTESIAN_POINT('Ctrl Pts',(107.353921212311,21.1294465860113,31.));
#94422=CARTESIAN_POINT('Ctrl Pts',(107.353921212311,21.1294465860113,26.));
#94423=CARTESIAN_POINT('Ctrl Pts',(107.379434581049,21.1165804017645,31.));
#94424=CARTESIAN_POINT('Ctrl Pts',(107.379434581049,21.1165804017645,26.));
#94425=CARTESIAN_POINT('Ctrl Pts',(107.404127740668,21.1035779524142,31.));
#94426=CARTESIAN_POINT('Ctrl Pts',(107.404127740668,21.1035779524142,26.));
#94427=CARTESIAN_POINT('Ctrl Pts',(107.428001300286,21.0904399793871,31.));
#94428=CARTESIAN_POINT('Ctrl Pts',(107.428001300286,21.0904399793871,26.));
#94429=CARTESIAN_POINT('Ctrl Pts',(107.451067109266,21.0771560949453,31.));
#94430=CARTESIAN_POINT('Ctrl Pts',(107.451067109266,21.0771560949453,26.));
#94431=CARTESIAN_POINT('Ctrl Pts',(107.473333124035,21.0637202906639,31.));
#94432=CARTESIAN_POINT('Ctrl Pts',(107.473333124035,21.0637202906639,26.));
#94433=CARTESIAN_POINT('Ctrl Pts',(107.49479042636,21.0501445654779,31.));
#94434=CARTESIAN_POINT('Ctrl Pts',(107.49479042636,21.0501445654779,26.));
#94435=CARTESIAN_POINT('Ctrl Pts',(107.515401372613,21.0364714002482,31.));
#94436=CARTESIAN_POINT('Ctrl Pts',(107.515401372613,21.0364714002482,26.));
#94437=CARTESIAN_POINT('Ctrl Pts',(107.535082466814,21.0227920500422,31.));
#94438=CARTESIAN_POINT('Ctrl Pts',(107.535082466814,21.0227920500422,26.));
#94439=CARTESIAN_POINT('Ctrl Pts',(107.553709421352,21.0092413310722,31.));
#94440=CARTESIAN_POINT('Ctrl Pts',(107.553709421352,21.0092413310722,26.));
#94441=CARTESIAN_POINT('Ctrl Pts',(107.571140046246,20.9959735258449,31.));
#94442=CARTESIAN_POINT('Ctrl Pts',(107.571140046246,20.9959735258449,26.));
#94443=CARTESIAN_POINT('Ctrl Pts',(107.58723291893,20.9831430242758,31.));
#94444=CARTESIAN_POINT('Ctrl Pts',(107.58723291893,20.9831430242758,26.));
#94445=CARTESIAN_POINT('Ctrl Pts',(107.601866156854,20.9708848153193,31.));
#94446=CARTESIAN_POINT('Ctrl Pts',(107.601866156854,20.9708848153193,26.));
#94447=CARTESIAN_POINT('Ctrl Pts',(107.614961199771,20.9592902980868,31.));
#94448=CARTESIAN_POINT('Ctrl Pts',(107.614961199771,20.9592902980868,26.));
#94449=CARTESIAN_POINT('Ctrl Pts',(107.626479908354,20.9484092543561,31.));
#94450=CARTESIAN_POINT('Ctrl Pts',(107.626479908354,20.9484092543561,26.));
#94451=CARTESIAN_POINT('Ctrl Pts',(107.634423517433,20.9402929843288,31.));
#94452=CARTESIAN_POINT('Ctrl Pts',(107.634423517433,20.9402929843288,26.));
#94453=CARTESIAN_POINT('Ctrl Pts',(107.639666871604,20.9345388664318,31.));
#94454=CARTESIAN_POINT('Ctrl Pts',(107.639666871604,20.9345388664318,26.));
#94455=CARTESIAN_POINT('Ctrl Pts',(107.642845514348,20.9308505683922,31.));
#94456=CARTESIAN_POINT('Ctrl Pts',(107.642845514348,20.9308505683922,26.));
#94457=CARTESIAN_POINT('Ctrl Pts',(107.644355604652,20.9290433639019,31.));
#94458=CARTESIAN_POINT('Ctrl Pts',(107.644355604652,20.9290433639019,26.));
#94459=CARTESIAN_POINT('',(106.921399971368,21.2821063151137,31.));
#94460=CARTESIAN_POINT('Ctrl Pts',(107.644355604652,20.9290433639019,31.));
#94461=CARTESIAN_POINT('Ctrl Pts',(107.642845514348,20.9308505683922,31.));
#94462=CARTESIAN_POINT('Ctrl Pts',(107.639666871604,20.9345388664318,31.));
#94463=CARTESIAN_POINT('Ctrl Pts',(107.634423517433,20.9402929843288,31.));
#94464=CARTESIAN_POINT('Ctrl Pts',(107.626479908354,20.9484092543561,31.));
#94465=CARTESIAN_POINT('Ctrl Pts',(107.614961199771,20.9592902980868,31.));
#94466=CARTESIAN_POINT('Ctrl Pts',(107.601866156854,20.9708848153193,31.));
#94467=CARTESIAN_POINT('Ctrl Pts',(107.58723291893,20.9831430242758,31.));
#94468=CARTESIAN_POINT('Ctrl Pts',(107.571140046246,20.9959735258449,31.));
#94469=CARTESIAN_POINT('Ctrl Pts',(107.553709421352,21.0092413310722,31.));
#94470=CARTESIAN_POINT('Ctrl Pts',(107.535082466814,21.0227920500422,31.));
#94471=CARTESIAN_POINT('Ctrl Pts',(107.515401372613,21.0364714002482,31.));
#94472=CARTESIAN_POINT('Ctrl Pts',(107.49479042636,21.0501445654779,31.));
#94473=CARTESIAN_POINT('Ctrl Pts',(107.473333124035,21.0637202906639,31.));
#94474=CARTESIAN_POINT('Ctrl Pts',(107.451067109266,21.0771560949453,31.));
#94475=CARTESIAN_POINT('Ctrl Pts',(107.428001300286,21.0904399793871,31.));
#94476=CARTESIAN_POINT('Ctrl Pts',(107.404127740668,21.1035779524142,31.));
#94477=CARTESIAN_POINT('Ctrl Pts',(107.379434581049,21.1165804017645,31.));
#94478=CARTESIAN_POINT('Ctrl Pts',(107.353921212311,21.1294465860113,31.));
#94479=CARTESIAN_POINT('Ctrl Pts',(107.327603123085,21.1421593243297,31.));
#94480=CARTESIAN_POINT('Ctrl Pts',(107.300504551943,21.1546918395446,31.));
#94481=CARTESIAN_POINT('Ctrl Pts',(107.27265445322,21.1670114619914,31.));
#94482=CARTESIAN_POINT('Ctrl Pts',(107.244081627808,21.1790843382305,31.));
#94483=CARTESIAN_POINT('Ctrl Pts',(107.214809663899,21.1908803622914,31.));
#94484=CARTESIAN_POINT('Ctrl Pts',(107.184854645532,21.2023758654395,31.));
#94485=CARTESIAN_POINT('Ctrl Pts',(107.154227550431,21.2135523179983,31.));
#94486=CARTESIAN_POINT('Ctrl Pts',(107.122935662486,21.2243960975415,31.));
#94487=CARTESIAN_POINT('Ctrl Pts',(107.09098439885,21.2348979013219,31.));
#94488=CARTESIAN_POINT('Ctrl Pts',(107.05837932368,21.2450524894041,31.));
#94489=CARTESIAN_POINT('Ctrl Pts',(107.025127490565,21.2548581702248,31.));
#94490=CARTESIAN_POINT('Ctrl Pts',(106.991235970075,21.2643155154947,31.));
#94491=CARTESIAN_POINT('Ctrl Pts',(106.963615969762,21.2716041208528,31.));
#94492=CARTESIAN_POINT('Ctrl Pts',(106.942617866551,21.2769154392463,31.));
#94493=CARTESIAN_POINT('Ctrl Pts',(106.928493535689,21.2803874938831,31.));
#94494=CARTESIAN_POINT('Ctrl Pts',(106.921399971368,21.2821063151137,31.));
#94495=CARTESIAN_POINT('',(106.921399971368,21.2821063151137,26.));
#94496=CARTESIAN_POINT('Ctrl Pts',(106.921399971368,21.2821063151137,26.));
#94497=CARTESIAN_POINT('Ctrl Pts',(106.928493535689,21.2803874938831,26.));
#94498=CARTESIAN_POINT('Ctrl Pts',(106.942617866551,21.2769154392463,26.));
#94499=CARTESIAN_POINT('Ctrl Pts',(106.963615969762,21.2716041208528,26.));
#94500=CARTESIAN_POINT('Ctrl Pts',(106.991235970075,21.2643155154947,26.));
#94501=CARTESIAN_POINT('Ctrl Pts',(107.025127490565,21.2548581702248,26.));
#94502=CARTESIAN_POINT('Ctrl Pts',(107.05837932368,21.2450524894041,26.));
#94503=CARTESIAN_POINT('Ctrl Pts',(107.09098439885,21.2348979013219,26.));
#94504=CARTESIAN_POINT('Ctrl Pts',(107.122935662486,21.2243960975415,26.));
#94505=CARTESIAN_POINT('Ctrl Pts',(107.154227550431,21.2135523179983,26.));
#94506=CARTESIAN_POINT('Ctrl Pts',(107.184854645532,21.2023758654395,26.));
#94507=CARTESIAN_POINT('Ctrl Pts',(107.214809663899,21.1908803622914,26.));
#94508=CARTESIAN_POINT('Ctrl Pts',(107.244081627808,21.1790843382305,26.));
#94509=CARTESIAN_POINT('Ctrl Pts',(107.27265445322,21.1670114619914,26.));
#94510=CARTESIAN_POINT('Ctrl Pts',(107.300504551943,21.1546918395446,26.));
#94511=CARTESIAN_POINT('Ctrl Pts',(107.327603123085,21.1421593243297,26.));
#94512=CARTESIAN_POINT('Ctrl Pts',(107.353921212311,21.1294465860113,26.));
#94513=CARTESIAN_POINT('Ctrl Pts',(107.379434581049,21.1165804017645,26.));
#94514=CARTESIAN_POINT('Ctrl Pts',(107.404127740668,21.1035779524142,26.));
#94515=CARTESIAN_POINT('Ctrl Pts',(107.428001300286,21.0904399793871,26.));
#94516=CARTESIAN_POINT('Ctrl Pts',(107.451067109266,21.0771560949453,26.));
#94517=CARTESIAN_POINT('Ctrl Pts',(107.473333124035,21.0637202906639,26.));
#94518=CARTESIAN_POINT('Ctrl Pts',(107.49479042636,21.0501445654779,26.));
#94519=CARTESIAN_POINT('Ctrl Pts',(107.515401372613,21.0364714002482,26.));
#94520=CARTESIAN_POINT('Ctrl Pts',(107.535082466814,21.0227920500422,26.));
#94521=CARTESIAN_POINT('Ctrl Pts',(107.553709421352,21.0092413310722,26.));
#94522=CARTESIAN_POINT('Ctrl Pts',(107.571140046246,20.9959735258449,26.));
#94523=CARTESIAN_POINT('Ctrl Pts',(107.58723291893,20.9831430242758,26.));
#94524=CARTESIAN_POINT('Ctrl Pts',(107.601866156854,20.9708848153193,26.));
#94525=CARTESIAN_POINT('Ctrl Pts',(107.614961199771,20.9592902980868,26.));
#94526=CARTESIAN_POINT('Ctrl Pts',(107.626479908354,20.9484092543561,26.));
#94527=CARTESIAN_POINT('Ctrl Pts',(107.634423517433,20.9402929843288,26.));
#94528=CARTESIAN_POINT('Ctrl Pts',(107.639666871604,20.9345388664318,26.));
#94529=CARTESIAN_POINT('Ctrl Pts',(107.642845514348,20.9308505683922,26.));
#94530=CARTESIAN_POINT('Ctrl Pts',(107.644355604652,20.9290433639019,26.));
#94531=CARTESIAN_POINT('',(106.921399971368,21.2821063151137,31.));
#94532=CARTESIAN_POINT('Origin',(110.000000000002,17.9999999999979,31.));
#94533=CARTESIAN_POINT('',(106.717893684886,21.0786000286317,31.));
#94534=CARTESIAN_POINT('Origin',(110.000000000002,17.9999999999979,31.));
#94535=CARTESIAN_POINT('',(106.717893684886,21.0786000286317,26.));
#94536=CARTESIAN_POINT('Origin',(110.000000000002,17.9999999999979,26.));
#94537=CARTESIAN_POINT('',(106.717893684886,21.0786000286317,31.));
#94538=CARTESIAN_POINT('Ctrl Pts',(107.070956636098,20.3556443953479,31.));
#94539=CARTESIAN_POINT('Ctrl Pts',(107.070956636098,20.3556443953479,26.));
#94540=CARTESIAN_POINT('Ctrl Pts',(107.069149431603,20.3571544856476,31.));
#94541=CARTESIAN_POINT('Ctrl Pts',(107.069149431603,20.3571544856476,26.));
#94542=CARTESIAN_POINT('Ctrl Pts',(107.065461133556,20.3603331283848,31.));
#94543=CARTESIAN_POINT('Ctrl Pts',(107.065461133556,20.3603331283848,26.));
#94544=CARTESIAN_POINT('Ctrl Pts',(107.059707015651,20.3655764825486,31.));
#94545=CARTESIAN_POINT('Ctrl Pts',(107.059707015651,20.3655764825486,26.));
#94546=CARTESIAN_POINT('Ctrl Pts',(107.05159074562,20.3735200916247,31.));
#94547=CARTESIAN_POINT('Ctrl Pts',(107.05159074562,20.3735200916247,26.));
#94548=CARTESIAN_POINT('Ctrl Pts',(107.040709701894,20.3850388002116,31.));
#94549=CARTESIAN_POINT('Ctrl Pts',(107.040709701894,20.3850388002116,26.));
#94550=CARTESIAN_POINT('Ctrl Pts',(107.029115184672,20.3981338431379,31.));
#94551=CARTESIAN_POINT('Ctrl Pts',(107.029115184672,20.3981338431379,26.));
#94552=CARTESIAN_POINT('Ctrl Pts',(107.016856975728,20.4127670810742,31.));
#94553=CARTESIAN_POINT('Ctrl Pts',(107.016856975728,20.4127670810742,26.));
#94554=CARTESIAN_POINT('Ctrl Pts',(107.004026474169,20.4288599537678,31.));
#94555=CARTESIAN_POINT('Ctrl Pts',(107.004026474169,20.4288599537678,26.));
#94556=CARTESIAN_POINT('Ctrl Pts',(106.990758668946,20.4462905786649,31.));
#94557=CARTESIAN_POINT('Ctrl Pts',(106.990758668946,20.4462905786649,26.));
#94558=CARTESIAN_POINT('Ctrl Pts',(106.977207949972,20.4649175332003,31.));
#94559=CARTESIAN_POINT('Ctrl Pts',(106.977207949972,20.4649175332003,26.));
#94560=CARTESIAN_POINT('Ctrl Pts',(106.963528599757,20.4845986273924,31.));
#94561=CARTESIAN_POINT('Ctrl Pts',(106.963528599757,20.4845986273924,26.));
#94562=CARTESIAN_POINT('Ctrl Pts',(106.949855434517,20.5052095736352,31.));
#94563=CARTESIAN_POINT('Ctrl Pts',(106.949855434517,20.5052095736352,26.));
#94564=CARTESIAN_POINT('Ctrl Pts',(106.936279709323,20.5266668759518,31.));
#94565=CARTESIAN_POINT('Ctrl Pts',(106.936279709323,20.5266668759518,26.));
#94566=CARTESIAN_POINT('Ctrl Pts',(106.922843905036,20.5489328907163,31.));
#94567=CARTESIAN_POINT('Ctrl Pts',(106.922843905036,20.5489328907163,26.));
#94568=CARTESIAN_POINT('Ctrl Pts',(106.909560020596,20.5719986996976,31.));
#94569=CARTESIAN_POINT('Ctrl Pts',(106.909560020596,20.5719986996976,26.));
#94570=CARTESIAN_POINT('Ctrl Pts',(106.896422047578,20.5958722593236,31.));
#94571=CARTESIAN_POINT('Ctrl Pts',(106.896422047578,20.5958722593236,26.));
#94572=CARTESIAN_POINT('Ctrl Pts',(106.883419598242,20.6205654189573,31.));
#94573=CARTESIAN_POINT('Ctrl Pts',(106.883419598242,20.6205654189573,26.));
#94574=CARTESIAN_POINT('Ctrl Pts',(106.87055341401,20.6460787877111,31.));
#94575=CARTESIAN_POINT('Ctrl Pts',(106.87055341401,20.6460787877111,26.));
#94576=CARTESIAN_POINT('Ctrl Pts',(106.857840675702,20.6723968769464,31.));
#94577=CARTESIAN_POINT('Ctrl Pts',(106.857840675702,20.6723968769464,26.));
#94578=CARTESIAN_POINT('Ctrl Pts',(106.845308160487,20.6994954480886,31.));
#94579=CARTESIAN_POINT('Ctrl Pts',(106.845308160487,20.6994954480886,26.));
#94580=CARTESIAN_POINT('Ctrl Pts',(106.832988538026,20.7273455467972,31.));
#94581=CARTESIAN_POINT('Ctrl Pts',(106.832988538026,20.7273455467972,26.));
#94582=CARTESIAN_POINT('Ctrl Pts',(106.82091566176,20.7559183721823,31.));
#94583=CARTESIAN_POINT('Ctrl Pts',(106.82091566176,20.7559183721823,26.));
#94584=CARTESIAN_POINT('Ctrl Pts',(106.809119637666,20.7851903360588,31.));
#94585=CARTESIAN_POINT('Ctrl Pts',(106.809119637666,20.7851903360588,26.));
#94586=CARTESIAN_POINT('Ctrl Pts',(106.797624134493,20.8151453544004,31.));
#94587=CARTESIAN_POINT('Ctrl Pts',(106.797624134493,20.8151453544004,26.));
#94588=CARTESIAN_POINT('Ctrl Pts',(106.786447681929,20.8457724494961,31.));
#94589=CARTESIAN_POINT('Ctrl Pts',(106.786447681929,20.8457724494961,26.));
#94590=CARTESIAN_POINT('Ctrl Pts',(106.775603902411,20.8770643374659,31.));
#94591=CARTESIAN_POINT('Ctrl Pts',(106.775603902411,20.8770643374659,26.));
#94592=CARTESIAN_POINT('Ctrl Pts',(106.765102098688,20.9090156011607,31.));
#94593=CARTESIAN_POINT('Ctrl Pts',(106.765102098688,20.9090156011607,26.));
#94594=CARTESIAN_POINT('Ctrl Pts',(106.754947510685,20.9416206764099,31.));
#94595=CARTESIAN_POINT('Ctrl Pts',(106.754947510685,20.9416206764099,26.));
#94596=CARTESIAN_POINT('Ctrl Pts',(106.745141829939,20.9748725095998,31.));
#94597=CARTESIAN_POINT('Ctrl Pts',(106.745141829939,20.9748725095998,26.));
#94598=CARTESIAN_POINT('Ctrl Pts',(106.735684484705,21.0087640301252,31.));
#94599=CARTESIAN_POINT('Ctrl Pts',(106.735684484705,21.0087640301252,26.));
#94600=CARTESIAN_POINT('Ctrl Pts',(106.728395879318,21.0363840304093,31.));
#94601=CARTESIAN_POINT('Ctrl Pts',(106.728395879318,21.0363840304093,26.));
#94602=CARTESIAN_POINT('Ctrl Pts',(106.723084560858,21.057382133554,31.));
#94603=CARTESIAN_POINT('Ctrl Pts',(106.723084560858,21.057382133554,26.));
#94604=CARTESIAN_POINT('Ctrl Pts',(106.719612506155,21.0715064643493,31.));
#94605=CARTESIAN_POINT('Ctrl Pts',(106.719612506155,21.0715064643493,26.));
#94606=CARTESIAN_POINT('Ctrl Pts',(106.717893684886,21.0786000286317,31.));
#94607=CARTESIAN_POINT('Ctrl Pts',(106.717893684886,21.0786000286317,26.));
#94608=CARTESIAN_POINT('Ctrl Pts',(107.070956636098,20.3556443953479,31.));
#94609=CARTESIAN_POINT('Ctrl Pts',(107.069149431603,20.3571544856476,31.));
#94610=CARTESIAN_POINT('Ctrl Pts',(107.065461133556,20.3603331283848,31.));
#94611=CARTESIAN_POINT('Ctrl Pts',(107.059707015651,20.3655764825486,31.));
#94612=CARTESIAN_POINT('Ctrl Pts',(107.05159074562,20.3735200916247,31.));
#94613=CARTESIAN_POINT('Ctrl Pts',(107.040709701894,20.3850388002116,31.));
#94614=CARTESIAN_POINT('Ctrl Pts',(107.029115184672,20.3981338431379,31.));
#94615=CARTESIAN_POINT('Ctrl Pts',(107.016856975728,20.4127670810742,31.));
#94616=CARTESIAN_POINT('Ctrl Pts',(107.004026474169,20.4288599537678,31.));
#94617=CARTESIAN_POINT('Ctrl Pts',(106.990758668946,20.4462905786649,31.));
#94618=CARTESIAN_POINT('Ctrl Pts',(106.977207949972,20.4649175332003,31.));
#94619=CARTESIAN_POINT('Ctrl Pts',(106.963528599757,20.4845986273924,31.));
#94620=CARTESIAN_POINT('Ctrl Pts',(106.949855434517,20.5052095736352,31.));
#94621=CARTESIAN_POINT('Ctrl Pts',(106.936279709323,20.5266668759518,31.));
#94622=CARTESIAN_POINT('Ctrl Pts',(106.922843905036,20.5489328907163,31.));
#94623=CARTESIAN_POINT('Ctrl Pts',(106.909560020596,20.5719986996976,31.));
#94624=CARTESIAN_POINT('Ctrl Pts',(106.896422047578,20.5958722593236,31.));
#94625=CARTESIAN_POINT('Ctrl Pts',(106.883419598242,20.6205654189573,31.));
#94626=CARTESIAN_POINT('Ctrl Pts',(106.87055341401,20.6460787877111,31.));
#94627=CARTESIAN_POINT('Ctrl Pts',(106.857840675702,20.6723968769464,31.));
#94628=CARTESIAN_POINT('Ctrl Pts',(106.845308160487,20.6994954480886,31.));
#94629=CARTESIAN_POINT('Ctrl Pts',(106.832988538026,20.7273455467972,31.));
#94630=CARTESIAN_POINT('Ctrl Pts',(106.82091566176,20.7559183721823,31.));
#94631=CARTESIAN_POINT('Ctrl Pts',(106.809119637666,20.7851903360588,31.));
#94632=CARTESIAN_POINT('Ctrl Pts',(106.797624134493,20.8151453544004,31.));
#94633=CARTESIAN_POINT('Ctrl Pts',(106.786447681929,20.8457724494961,31.));
#94634=CARTESIAN_POINT('Ctrl Pts',(106.775603902411,20.8770643374659,31.));
#94635=CARTESIAN_POINT('Ctrl Pts',(106.765102098688,20.9090156011607,31.));
#94636=CARTESIAN_POINT('Ctrl Pts',(106.754947510685,20.9416206764099,31.));
#94637=CARTESIAN_POINT('Ctrl Pts',(106.745141829939,20.9748725095998,31.));
#94638=CARTESIAN_POINT('Ctrl Pts',(106.735684484705,21.0087640301252,31.));
#94639=CARTESIAN_POINT('Ctrl Pts',(106.728395879318,21.0363840304093,31.));
#94640=CARTESIAN_POINT('Ctrl Pts',(106.723084560858,21.057382133554,31.));
#94641=CARTESIAN_POINT('Ctrl Pts',(106.719612506155,21.0715064643493,31.));
#94642=CARTESIAN_POINT('Ctrl Pts',(106.717893684886,21.0786000286317,31.));
#94643=CARTESIAN_POINT('Ctrl Pts',(107.070956636098,20.3556443953479,26.));
#94644=CARTESIAN_POINT('Ctrl Pts',(107.069149431603,20.3571544856476,26.));
#94645=CARTESIAN_POINT('Ctrl Pts',(107.065461133556,20.3603331283848,26.));
#94646=CARTESIAN_POINT('Ctrl Pts',(107.059707015651,20.3655764825486,26.));
#94647=CARTESIAN_POINT('Ctrl Pts',(107.05159074562,20.3735200916247,26.));
#94648=CARTESIAN_POINT('Ctrl Pts',(107.040709701894,20.3850388002116,26.));
#94649=CARTESIAN_POINT('Ctrl Pts',(107.029115184672,20.3981338431379,26.));
#94650=CARTESIAN_POINT('Ctrl Pts',(107.016856975728,20.4127670810742,26.));
#94651=CARTESIAN_POINT('Ctrl Pts',(107.004026474169,20.4288599537678,26.));
#94652=CARTESIAN_POINT('Ctrl Pts',(106.990758668946,20.4462905786649,26.));
#94653=CARTESIAN_POINT('Ctrl Pts',(106.977207949972,20.4649175332003,26.));
#94654=CARTESIAN_POINT('Ctrl Pts',(106.963528599757,20.4845986273924,26.));
#94655=CARTESIAN_POINT('Ctrl Pts',(106.949855434517,20.5052095736352,26.));
#94656=CARTESIAN_POINT('Ctrl Pts',(106.936279709323,20.5266668759518,26.));
#94657=CARTESIAN_POINT('Ctrl Pts',(106.922843905036,20.5489328907163,26.));
#94658=CARTESIAN_POINT('Ctrl Pts',(106.909560020596,20.5719986996976,26.));
#94659=CARTESIAN_POINT('Ctrl Pts',(106.896422047578,20.5958722593236,26.));
#94660=CARTESIAN_POINT('Ctrl Pts',(106.883419598242,20.6205654189573,26.));
#94661=CARTESIAN_POINT('Ctrl Pts',(106.87055341401,20.6460787877111,26.));
#94662=CARTESIAN_POINT('Ctrl Pts',(106.857840675702,20.6723968769464,26.));
#94663=CARTESIAN_POINT('Ctrl Pts',(106.845308160487,20.6994954480886,26.));
#94664=CARTESIAN_POINT('Ctrl Pts',(106.832988538026,20.7273455467972,26.));
#94665=CARTESIAN_POINT('Ctrl Pts',(106.82091566176,20.7559183721823,26.));
#94666=CARTESIAN_POINT('Ctrl Pts',(106.809119637666,20.7851903360588,26.));
#94667=CARTESIAN_POINT('Ctrl Pts',(106.797624134493,20.8151453544004,26.));
#94668=CARTESIAN_POINT('Ctrl Pts',(106.786447681929,20.8457724494961,26.));
#94669=CARTESIAN_POINT('Ctrl Pts',(106.775603902411,20.8770643374659,26.));
#94670=CARTESIAN_POINT('Ctrl Pts',(106.765102098688,20.9090156011607,26.));
#94671=CARTESIAN_POINT('Ctrl Pts',(106.754947510685,20.9416206764099,26.));
#94672=CARTESIAN_POINT('Ctrl Pts',(106.745141829939,20.9748725095998,26.));
#94673=CARTESIAN_POINT('Ctrl Pts',(106.735684484705,21.0087640301252,26.));
#94674=CARTESIAN_POINT('Ctrl Pts',(106.728395879318,21.0363840304093,26.));
#94675=CARTESIAN_POINT('Ctrl Pts',(106.723084560858,21.057382133554,26.));
#94676=CARTESIAN_POINT('Ctrl Pts',(106.719612506155,21.0715064643493,26.));
#94677=CARTESIAN_POINT('Ctrl Pts',(106.717893684886,21.0786000286317,26.));
#94678=CARTESIAN_POINT('Origin',(107.27545303142,20.7245469685571,31.));
#94679=CARTESIAN_POINT('Origin',(108.451650540008,20.8289996376356,31.));
#94680=CARTESIAN_POINT('',(108.195382868896,21.297228010781,31.));
#94681=CARTESIAN_POINT('',(108.195382868896,21.297228010781,31.));
#94682=CARTESIAN_POINT('',(108.195382868896,21.297228010781,26.));
#94683=CARTESIAN_POINT('',(108.195382868896,21.297228010781,31.));
#94684=CARTESIAN_POINT('',(108.195382868896,21.297228010781,26.));
#94685=CARTESIAN_POINT('Origin',(108.944564725307,21.6075492963903,31.));
#94686=CARTESIAN_POINT('',(108.944564725307,21.6075492963903,26.));
#94687=CARTESIAN_POINT('',(109.09444357506,21.0952532305533,26.));
#94688=CARTESIAN_POINT('',(108.944564725307,21.6075492963903,31.));
#94689=CARTESIAN_POINT('',(108.944564725307,21.6075492963903,31.));
#94690=CARTESIAN_POINT('',(109.09444357506,21.0952532305533,31.));
#94691=CARTESIAN_POINT('Ctrl Pts',(108.411752154813,22.2104000738956,31.));
#94692=CARTESIAN_POINT('Ctrl Pts',(108.411752154813,22.2104000738956,26.));
#94693=CARTESIAN_POINT('Ctrl Pts',(108.417647989294,22.2060975005986,31.));
#94694=CARTESIAN_POINT('Ctrl Pts',(108.417647989294,22.2060975005986,26.));
#94695=CARTESIAN_POINT('Ctrl Pts',(108.429368471701,22.19748459297,31.));
#94696=CARTESIAN_POINT('Ctrl Pts',(108.429368471701,22.19748459297,26.));
#94697=CARTESIAN_POINT('Ctrl Pts',(108.446735635927,22.1845419484054,31.));
#94698=CARTESIAN_POINT('Ctrl Pts',(108.446735635927,22.1845419484054,26.));
#94699=CARTESIAN_POINT('Ctrl Pts',(108.469463960389,22.1672384385728,31.));
#94700=CARTESIAN_POINT('Ctrl Pts',(108.469463960389,22.1672384385728,26.));
#94701=CARTESIAN_POINT('Ctrl Pts',(108.497156473145,22.1455312674571,31.));
#94702=CARTESIAN_POINT('Ctrl Pts',(108.497156473145,22.1455312674571,26.));
#94703=CARTESIAN_POINT('Ctrl Pts',(108.524124689586,22.1237470740155,31.));
#94704=CARTESIAN_POINT('Ctrl Pts',(108.524124689586,22.1237470740155,26.));
#94705=CARTESIAN_POINT('Ctrl Pts',(108.55036185857,22.1018880358469,31.));
#94706=CARTESIAN_POINT('Ctrl Pts',(108.55036185857,22.1018880358469,26.));
#94707=CARTESIAN_POINT('Ctrl Pts',(108.575862110765,22.0799584150428,31.));
#94708=CARTESIAN_POINT('Ctrl Pts',(108.575862110765,22.0799584150428,26.));
#94709=CARTESIAN_POINT('Ctrl Pts',(108.600622310795,22.0579651819841,31.));
#94710=CARTESIAN_POINT('Ctrl Pts',(108.600622310795,22.0579651819841,26.));
#94711=CARTESIAN_POINT('Ctrl Pts',(108.624641013872,22.0359190043423,31.));
#94712=CARTESIAN_POINT('Ctrl Pts',(108.624641013872,22.0359190043423,26.));
#94713=CARTESIAN_POINT('Ctrl Pts',(108.647916703636,22.0138352550225,31.));
#94714=CARTESIAN_POINT('Ctrl Pts',(108.647916703636,22.0138352550225,26.));
#94715=CARTESIAN_POINT('Ctrl Pts',(108.670446328992,21.9917352542068,31.));
#94716=CARTESIAN_POINT('Ctrl Pts',(108.670446328992,21.9917352542068,26.));
#94717=CARTESIAN_POINT('Ctrl Pts',(108.692224087859,21.9696470240499,31.));
#94718=CARTESIAN_POINT('Ctrl Pts',(108.692224087859,21.9696470240499,26.));
#94719=CARTESIAN_POINT('Ctrl Pts',(108.713239708644,21.947607405652,31.));
#94720=CARTESIAN_POINT('Ctrl Pts',(108.713239708644,21.947607405652,26.));
#94721=CARTESIAN_POINT('Ctrl Pts',(108.733479537944,21.9256586971371,31.));
#94722=CARTESIAN_POINT('Ctrl Pts',(108.733479537944,21.9256586971371,26.));
#94723=CARTESIAN_POINT('Ctrl Pts',(108.75292932758,21.9038421616846,31.));
#94724=CARTESIAN_POINT('Ctrl Pts',(108.75292932758,21.9038421616846,26.));
#94725=CARTESIAN_POINT('Ctrl Pts',(108.771576931213,21.8821918138775,31.));
#94726=CARTESIAN_POINT('Ctrl Pts',(108.771576931213,21.8821918138775,26.));
#94727=CARTESIAN_POINT('Ctrl Pts',(108.789414614032,21.8607294539711,31.));
#94728=CARTESIAN_POINT('Ctrl Pts',(108.789414614032,21.8607294539711,26.));
#94729=CARTESIAN_POINT('Ctrl Pts',(108.806443222519,21.8394555338556,31.));
#94730=CARTESIAN_POINT('Ctrl Pts',(108.806443222519,21.8394555338556,26.));
#94731=CARTESIAN_POINT('Ctrl Pts',(108.822669728842,21.8183559219568,31.));
#94732=CARTESIAN_POINT('Ctrl Pts',(108.822669728842,21.8183559219568,26.));
#94733=CARTESIAN_POINT('Ctrl Pts',(108.838099184459,21.7974220224214,31.));
#94734=CARTESIAN_POINT('Ctrl Pts',(108.838099184459,21.7974220224214,26.));
#94735=CARTESIAN_POINT('Ctrl Pts',(108.85272794179,21.7766683336798,31.));
#94736=CARTESIAN_POINT('Ctrl Pts',(108.85272794179,21.7766683336798,26.));
#94737=CARTESIAN_POINT('Ctrl Pts',(108.866537479377,21.7561485085232,31.));
#94738=CARTESIAN_POINT('Ctrl Pts',(108.866537479377,21.7561485085232,26.));
#94739=CARTESIAN_POINT('Ctrl Pts',(108.879485578797,21.7359788081685,31.));
#94740=CARTESIAN_POINT('Ctrl Pts',(108.879485578797,21.7359788081685,26.));
#94741=CARTESIAN_POINT('Ctrl Pts',(108.891509005202,21.7163313493639,31.));
#94742=CARTESIAN_POINT('Ctrl Pts',(108.891509005202,21.7163313493639,26.));
#94743=CARTESIAN_POINT('Ctrl Pts',(108.902535433535,21.6974030843105,31.));
#94744=CARTESIAN_POINT('Ctrl Pts',(108.902535433535,21.6974030843105,26.));
#94745=CARTESIAN_POINT('Ctrl Pts',(108.912493288848,21.6793907707637,31.));
#94746=CARTESIAN_POINT('Ctrl Pts',(108.912493288848,21.6793907707637,26.));
#94747=CARTESIAN_POINT('Ctrl Pts',(108.921321624383,21.6624657646879,31.));
#94748=CARTESIAN_POINT('Ctrl Pts',(108.921321624383,21.6624657646879,26.));
#94749=CARTESIAN_POINT('Ctrl Pts',(108.92898283686,21.6467425715572,31.));
#94750=CARTESIAN_POINT('Ctrl Pts',(108.92898283686,21.6467425715572,26.));
#94751=CARTESIAN_POINT('Ctrl Pts',(108.935460740798,21.6322817790252,31.));
#94752=CARTESIAN_POINT('Ctrl Pts',(108.935460740798,21.6322817790252,26.));
#94753=CARTESIAN_POINT('Ctrl Pts',(108.939693716568,21.6217434356788,31.));
#94754=CARTESIAN_POINT('Ctrl Pts',(108.939693716568,21.6217434356788,26.));
#94755=CARTESIAN_POINT('Ctrl Pts',(108.942335938581,21.6144207791549,31.));
#94756=CARTESIAN_POINT('Ctrl Pts',(108.942335938581,21.6144207791549,26.));
#94757=CARTESIAN_POINT('Ctrl Pts',(108.943861171001,21.6097968221706,31.));
#94758=CARTESIAN_POINT('Ctrl Pts',(108.943861171001,21.6097968221706,26.));
#94759=CARTESIAN_POINT('Ctrl Pts',(108.944564725307,21.6075492963903,31.));
#94760=CARTESIAN_POINT('Ctrl Pts',(108.944564725307,21.6075492963903,26.));
#94761=CARTESIAN_POINT('',(108.411752154813,22.2104000738956,31.));
#94762=CARTESIAN_POINT('Ctrl Pts',(108.944564725307,21.6075492963903,31.));
#94763=CARTESIAN_POINT('Ctrl Pts',(108.943861171001,21.6097968221706,31.));
#94764=CARTESIAN_POINT('Ctrl Pts',(108.942335938581,21.6144207791549,31.));
#94765=CARTESIAN_POINT('Ctrl Pts',(108.939693716568,21.6217434356788,31.));
#94766=CARTESIAN_POINT('Ctrl Pts',(108.935460740798,21.6322817790252,31.));
#94767=CARTESIAN_POINT('Ctrl Pts',(108.92898283686,21.6467425715572,31.));
#94768=CARTESIAN_POINT('Ctrl Pts',(108.921321624383,21.6624657646879,31.));
#94769=CARTESIAN_POINT('Ctrl Pts',(108.912493288848,21.6793907707637,31.));
#94770=CARTESIAN_POINT('Ctrl Pts',(108.902535433535,21.6974030843105,31.));
#94771=CARTESIAN_POINT('Ctrl Pts',(108.891509005202,21.7163313493639,31.));
#94772=CARTESIAN_POINT('Ctrl Pts',(108.879485578797,21.7359788081685,31.));
#94773=CARTESIAN_POINT('Ctrl Pts',(108.866537479377,21.7561485085232,31.));
#94774=CARTESIAN_POINT('Ctrl Pts',(108.85272794179,21.7766683336798,31.));
#94775=CARTESIAN_POINT('Ctrl Pts',(108.838099184459,21.7974220224214,31.));
#94776=CARTESIAN_POINT('Ctrl Pts',(108.822669728842,21.8183559219568,31.));
#94777=CARTESIAN_POINT('Ctrl Pts',(108.806443222519,21.8394555338556,31.));
#94778=CARTESIAN_POINT('Ctrl Pts',(108.789414614032,21.8607294539711,31.));
#94779=CARTESIAN_POINT('Ctrl Pts',(108.771576931213,21.8821918138775,31.));
#94780=CARTESIAN_POINT('Ctrl Pts',(108.75292932758,21.9038421616846,31.));
#94781=CARTESIAN_POINT('Ctrl Pts',(108.733479537944,21.9256586971371,31.));
#94782=CARTESIAN_POINT('Ctrl Pts',(108.713239708644,21.947607405652,31.));
#94783=CARTESIAN_POINT('Ctrl Pts',(108.692224087859,21.9696470240499,31.));
#94784=CARTESIAN_POINT('Ctrl Pts',(108.670446328992,21.9917352542068,31.));
#94785=CARTESIAN_POINT('Ctrl Pts',(108.647916703636,22.0138352550225,31.));
#94786=CARTESIAN_POINT('Ctrl Pts',(108.624641013872,22.0359190043423,31.));
#94787=CARTESIAN_POINT('Ctrl Pts',(108.600622310795,22.0579651819841,31.));
#94788=CARTESIAN_POINT('Ctrl Pts',(108.575862110765,22.0799584150428,31.));
#94789=CARTESIAN_POINT('Ctrl Pts',(108.55036185857,22.1018880358469,31.));
#94790=CARTESIAN_POINT('Ctrl Pts',(108.524124689586,22.1237470740155,31.));
#94791=CARTESIAN_POINT('Ctrl Pts',(108.497156473145,22.1455312674571,31.));
#94792=CARTESIAN_POINT('Ctrl Pts',(108.469463960389,22.1672384385728,31.));
#94793=CARTESIAN_POINT('Ctrl Pts',(108.446735635927,22.1845419484054,31.));
#94794=CARTESIAN_POINT('Ctrl Pts',(108.429368471701,22.19748459297,31.));
#94795=CARTESIAN_POINT('Ctrl Pts',(108.417647989294,22.2060975005986,31.));
#94796=CARTESIAN_POINT('Ctrl Pts',(108.411752154813,22.2104000738956,31.));
#94797=CARTESIAN_POINT('',(108.411752154813,22.2104000738956,26.));
#94798=CARTESIAN_POINT('Ctrl Pts',(108.411752154813,22.2104000738956,26.));
#94799=CARTESIAN_POINT('Ctrl Pts',(108.417647989294,22.2060975005986,26.));
#94800=CARTESIAN_POINT('Ctrl Pts',(108.429368471701,22.19748459297,26.));
#94801=CARTESIAN_POINT('Ctrl Pts',(108.446735635927,22.1845419484054,26.));
#94802=CARTESIAN_POINT('Ctrl Pts',(108.469463960389,22.1672384385728,26.));
#94803=CARTESIAN_POINT('Ctrl Pts',(108.497156473145,22.1455312674571,26.));
#94804=CARTESIAN_POINT('Ctrl Pts',(108.524124689586,22.1237470740155,26.));
#94805=CARTESIAN_POINT('Ctrl Pts',(108.55036185857,22.1018880358469,26.));
#94806=CARTESIAN_POINT('Ctrl Pts',(108.575862110765,22.0799584150428,26.));
#94807=CARTESIAN_POINT('Ctrl Pts',(108.600622310795,22.0579651819841,26.));
#94808=CARTESIAN_POINT('Ctrl Pts',(108.624641013872,22.0359190043423,26.));
#94809=CARTESIAN_POINT('Ctrl Pts',(108.647916703636,22.0138352550225,26.));
#94810=CARTESIAN_POINT('Ctrl Pts',(108.670446328992,21.9917352542068,26.));
#94811=CARTESIAN_POINT('Ctrl Pts',(108.692224087859,21.9696470240499,26.));
#94812=CARTESIAN_POINT('Ctrl Pts',(108.713239708644,21.947607405652,26.));
#94813=CARTESIAN_POINT('Ctrl Pts',(108.733479537944,21.9256586971371,26.));
#94814=CARTESIAN_POINT('Ctrl Pts',(108.75292932758,21.9038421616846,26.));
#94815=CARTESIAN_POINT('Ctrl Pts',(108.771576931213,21.8821918138775,26.));
#94816=CARTESIAN_POINT('Ctrl Pts',(108.789414614032,21.8607294539711,26.));
#94817=CARTESIAN_POINT('Ctrl Pts',(108.806443222519,21.8394555338556,26.));
#94818=CARTESIAN_POINT('Ctrl Pts',(108.822669728842,21.8183559219568,26.));
#94819=CARTESIAN_POINT('Ctrl Pts',(108.838099184459,21.7974220224214,26.));
#94820=CARTESIAN_POINT('Ctrl Pts',(108.85272794179,21.7766683336798,26.));
#94821=CARTESIAN_POINT('Ctrl Pts',(108.866537479377,21.7561485085232,26.));
#94822=CARTESIAN_POINT('Ctrl Pts',(108.879485578797,21.7359788081685,26.));
#94823=CARTESIAN_POINT('Ctrl Pts',(108.891509005202,21.7163313493639,26.));
#94824=CARTESIAN_POINT('Ctrl Pts',(108.902535433535,21.6974030843105,26.));
#94825=CARTESIAN_POINT('Ctrl Pts',(108.912493288848,21.6793907707637,26.));
#94826=CARTESIAN_POINT('Ctrl Pts',(108.921321624383,21.6624657646879,26.));
#94827=CARTESIAN_POINT('Ctrl Pts',(108.92898283686,21.6467425715572,26.));
#94828=CARTESIAN_POINT('Ctrl Pts',(108.935460740798,21.6322817790252,26.));
#94829=CARTESIAN_POINT('Ctrl Pts',(108.939693716568,21.6217434356788,26.));
#94830=CARTESIAN_POINT('Ctrl Pts',(108.942335938581,21.6144207791549,26.));
#94831=CARTESIAN_POINT('Ctrl Pts',(108.943861171001,21.6097968221706,26.));
#94832=CARTESIAN_POINT('Ctrl Pts',(108.944564725307,21.6075492963903,26.));
#94833=CARTESIAN_POINT('',(108.411752154813,22.2104000738956,31.));
#94834=CARTESIAN_POINT('Origin',(110.000000000001,17.9999999999972,31.));
#94835=CARTESIAN_POINT('',(108.145858377777,22.1002632652963,31.));
#94836=CARTESIAN_POINT('Origin',(110.000000000001,17.9999999999972,31.));
#94837=CARTESIAN_POINT('',(108.145858377777,22.1002632652963,26.));
#94838=CARTESIAN_POINT('Origin',(110.000000000001,17.9999999999972,26.));
#94839=CARTESIAN_POINT('',(108.145858377777,22.1002632652963,31.));
#94840=CARTESIAN_POINT('Ctrl Pts',(108.195382868896,21.297228010781,31.));
#94841=CARTESIAN_POINT('Ctrl Pts',(108.195382868896,21.297228010781,26.));
#94842=CARTESIAN_POINT('Ctrl Pts',(108.194291116192,21.2993147395202,31.));
#94843=CARTESIAN_POINT('Ctrl Pts',(108.194291116192,21.2993147395202,26.));
#94844=CARTESIAN_POINT('Ctrl Pts',(108.192099987029,21.3036628730427,31.));
#94845=CARTESIAN_POINT('Ctrl Pts',(108.192099987029,21.3036628730427,26.));
#94846=CARTESIAN_POINT('Ctrl Pts',(108.188790420037,21.3107091062263,31.));
#94847=CARTESIAN_POINT('Ctrl Pts',(108.188790420037,21.3107091062263,26.));
#94848=CARTESIAN_POINT('Ctrl Pts',(108.184331851862,21.3211540061394,31.));
#94849=CARTESIAN_POINT('Ctrl Pts',(108.184331851862,21.3211540061394,26.));
#94850=CARTESIAN_POINT('Ctrl Pts',(108.17868709721,21.3359599004046,31.));
#94851=CARTESIAN_POINT('Ctrl Pts',(108.17868709721,21.3359599004046,26.));
#94852=CARTESIAN_POINT('Ctrl Pts',(108.172986416033,21.3524951721887,31.));
#94853=CARTESIAN_POINT('Ctrl Pts',(108.172986416033,21.3524951721887,26.));
#94854=CARTESIAN_POINT('Ctrl Pts',(108.167261205405,21.3707055346857,31.));
#94855=CARTESIAN_POINT('Ctrl Pts',(108.167261205405,21.3707055346857,26.));
#94856=CARTESIAN_POINT('Ctrl Pts',(108.161565843382,21.3904834307621,31.));
#94857=CARTESIAN_POINT('Ctrl Pts',(108.161565843382,21.3904834307621,26.));
#94858=CARTESIAN_POINT('Ctrl Pts',(108.155978401058,21.4116645975863,31.));
#94859=CARTESIAN_POINT('Ctrl Pts',(108.155978401058,21.4116645975863,26.));
#94860=CARTESIAN_POINT('Ctrl Pts',(108.150587396044,21.4340592952825,31.));
#94861=CARTESIAN_POINT('Ctrl Pts',(108.150587396044,21.4340592952825,26.));
#94862=CARTESIAN_POINT('Ctrl Pts',(108.14548095304,21.4574771160767,31.));
#94863=CARTESIAN_POINT('Ctrl Pts',(108.14548095304,21.4574771160767,26.));
#94864=CARTESIAN_POINT('Ctrl Pts',(108.140736063183,21.4817516412614,31.));
#94865=CARTESIAN_POINT('Ctrl Pts',(108.140736063183,21.4817516412614,26.));
#94866=CARTESIAN_POINT('Ctrl Pts',(108.136405082636,21.5067708088092,31.));
#94867=CARTESIAN_POINT('Ctrl Pts',(108.136405082636,21.5067708088092,26.));
#94868=CARTESIAN_POINT('Ctrl Pts',(108.132512853008,21.5324835838215,31.));
#94869=CARTESIAN_POINT('Ctrl Pts',(108.132512853008,21.5324835838215,26.));
#94870=CARTESIAN_POINT('Ctrl Pts',(108.129067047013,21.5588771351329,31.));
#94871=CARTESIAN_POINT('Ctrl Pts',(108.129067047013,21.5588771351329,26.));
#94872=CARTESIAN_POINT('Ctrl Pts',(108.126065158383,21.5859611128485,31.));
#94873=CARTESIAN_POINT('Ctrl Pts',(108.126065158383,21.5859611128485,26.));
#94874=CARTESIAN_POINT('Ctrl Pts',(108.123502124654,21.6137504395681,31.));
#94875=CARTESIAN_POINT('Ctrl Pts',(108.123502124654,21.6137504395681,26.));
#94876=CARTESIAN_POINT('Ctrl Pts',(108.121378863907,21.6422453943083,31.));
#94877=CARTESIAN_POINT('Ctrl Pts',(108.121378863907,21.6422453943083,26.));
#94878=CARTESIAN_POINT('Ctrl Pts',(108.119705321903,21.6714250926182,31.));
#94879=CARTESIAN_POINT('Ctrl Pts',(108.119705321903,21.6714250926182,26.));
#94880=CARTESIAN_POINT('Ctrl Pts',(108.118496961822,21.7012568937955,31.));
#94881=CARTESIAN_POINT('Ctrl Pts',(108.118496961822,21.7012568937955,26.));
#94882=CARTESIAN_POINT('Ctrl Pts',(108.117772886147,21.7317015453796,31.));
#94883=CARTESIAN_POINT('Ctrl Pts',(108.117772886147,21.7317015453796,26.));
#94884=CARTESIAN_POINT('Ctrl Pts',(108.117553349757,21.7627194836669,31.));
#94885=CARTESIAN_POINT('Ctrl Pts',(108.117553349757,21.7627194836669,26.));
#94886=CARTESIAN_POINT('Ctrl Pts',(108.117857140141,21.7942773949572,31.));
#94887=CARTESIAN_POINT('Ctrl Pts',(108.117857140141,21.7942773949572,26.));
#94888=CARTESIAN_POINT('Ctrl Pts',(108.118699969278,21.8263513619102,31.));
#94889=CARTESIAN_POINT('Ctrl Pts',(108.118699969278,21.8263513619102,26.));
#94890=CARTESIAN_POINT('Ctrl Pts',(108.120094755383,21.8589241514383,31.));
#94891=CARTESIAN_POINT('Ctrl Pts',(108.120094755383,21.8589241514383,26.));
#94892=CARTESIAN_POINT('Ctrl Pts',(108.122051296525,21.8919838210329,31.));
#94893=CARTESIAN_POINT('Ctrl Pts',(108.122051296525,21.8919838210329,26.));
#94894=CARTESIAN_POINT('Ctrl Pts',(108.12457611427,21.925521805893,31.));
#94895=CARTESIAN_POINT('Ctrl Pts',(108.12457611427,21.925521805893,26.));
#94896=CARTESIAN_POINT('Ctrl Pts',(108.127671920362,21.9595309601629,31.));
#94897=CARTESIAN_POINT('Ctrl Pts',(108.127671920362,21.9595309601629,26.));
#94898=CARTESIAN_POINT('Ctrl Pts',(108.131337578276,21.9940041198301,31.));
#94899=CARTESIAN_POINT('Ctrl Pts',(108.131337578276,21.9940041198301,26.));
#94900=CARTESIAN_POINT('Ctrl Pts',(108.135569853985,22.0289349713044,31.));
#94901=CARTESIAN_POINT('Ctrl Pts',(108.135569853985,22.0289349713044,26.));
#94902=CARTESIAN_POINT('Ctrl Pts',(108.139405777158,22.0572417527814,31.));
#94903=CARTESIAN_POINT('Ctrl Pts',(108.139405777158,22.0572417527814,26.));
#94904=CARTESIAN_POINT('Ctrl Pts',(108.142534384927,22.0786740240772,31.));
#94905=CARTESIAN_POINT('Ctrl Pts',(108.142534384927,22.0786740240772,26.));
#94906=CARTESIAN_POINT('Ctrl Pts',(108.14473177204,22.0930519020204,31.));
#94907=CARTESIAN_POINT('Ctrl Pts',(108.14473177204,22.0930519020204,26.));
#94908=CARTESIAN_POINT('Ctrl Pts',(108.145858377777,22.1002632652963,31.));
#94909=CARTESIAN_POINT('Ctrl Pts',(108.145858377777,22.1002632652963,26.));
#94910=CARTESIAN_POINT('Ctrl Pts',(108.195382868896,21.297228010781,31.));
#94911=CARTESIAN_POINT('Ctrl Pts',(108.194291116192,21.2993147395202,31.));
#94912=CARTESIAN_POINT('Ctrl Pts',(108.192099987029,21.3036628730427,31.));
#94913=CARTESIAN_POINT('Ctrl Pts',(108.188790420037,21.3107091062263,31.));
#94914=CARTESIAN_POINT('Ctrl Pts',(108.184331851862,21.3211540061394,31.));
#94915=CARTESIAN_POINT('Ctrl Pts',(108.17868709721,21.3359599004046,31.));
#94916=CARTESIAN_POINT('Ctrl Pts',(108.172986416033,21.3524951721887,31.));
#94917=CARTESIAN_POINT('Ctrl Pts',(108.167261205405,21.3707055346857,31.));
#94918=CARTESIAN_POINT('Ctrl Pts',(108.161565843382,21.3904834307621,31.));
#94919=CARTESIAN_POINT('Ctrl Pts',(108.155978401058,21.4116645975863,31.));
#94920=CARTESIAN_POINT('Ctrl Pts',(108.150587396044,21.4340592952825,31.));
#94921=CARTESIAN_POINT('Ctrl Pts',(108.14548095304,21.4574771160767,31.));
#94922=CARTESIAN_POINT('Ctrl Pts',(108.140736063183,21.4817516412614,31.));
#94923=CARTESIAN_POINT('Ctrl Pts',(108.136405082636,21.5067708088092,31.));
#94924=CARTESIAN_POINT('Ctrl Pts',(108.132512853008,21.5324835838215,31.));
#94925=CARTESIAN_POINT('Ctrl Pts',(108.129067047013,21.5588771351329,31.));
#94926=CARTESIAN_POINT('Ctrl Pts',(108.126065158383,21.5859611128485,31.));
#94927=CARTESIAN_POINT('Ctrl Pts',(108.123502124654,21.6137504395681,31.));
#94928=CARTESIAN_POINT('Ctrl Pts',(108.121378863907,21.6422453943083,31.));
#94929=CARTESIAN_POINT('Ctrl Pts',(108.119705321903,21.6714250926182,31.));
#94930=CARTESIAN_POINT('Ctrl Pts',(108.118496961822,21.7012568937955,31.));
#94931=CARTESIAN_POINT('Ctrl Pts',(108.117772886147,21.7317015453796,31.));
#94932=CARTESIAN_POINT('Ctrl Pts',(108.117553349757,21.7627194836669,31.));
#94933=CARTESIAN_POINT('Ctrl Pts',(108.117857140141,21.7942773949572,31.));
#94934=CARTESIAN_POINT('Ctrl Pts',(108.118699969278,21.8263513619102,31.));
#94935=CARTESIAN_POINT('Ctrl Pts',(108.120094755383,21.8589241514383,31.));
#94936=CARTESIAN_POINT('Ctrl Pts',(108.122051296525,21.8919838210329,31.));
#94937=CARTESIAN_POINT('Ctrl Pts',(108.12457611427,21.925521805893,31.));
#94938=CARTESIAN_POINT('Ctrl Pts',(108.127671920362,21.9595309601629,31.));
#94939=CARTESIAN_POINT('Ctrl Pts',(108.131337578276,21.9940041198301,31.));
#94940=CARTESIAN_POINT('Ctrl Pts',(108.135569853985,22.0289349713044,31.));
#94941=CARTESIAN_POINT('Ctrl Pts',(108.139405777158,22.0572417527814,31.));
#94942=CARTESIAN_POINT('Ctrl Pts',(108.142534384927,22.0786740240772,31.));
#94943=CARTESIAN_POINT('Ctrl Pts',(108.14473177204,22.0930519020204,31.));
#94944=CARTESIAN_POINT('Ctrl Pts',(108.145858377777,22.1002632652963,31.));
#94945=CARTESIAN_POINT('Ctrl Pts',(108.195382868896,21.297228010781,26.));
#94946=CARTESIAN_POINT('Ctrl Pts',(108.194291116192,21.2993147395202,26.));
#94947=CARTESIAN_POINT('Ctrl Pts',(108.192099987029,21.3036628730427,26.));
#94948=CARTESIAN_POINT('Ctrl Pts',(108.188790420037,21.3107091062263,26.));
#94949=CARTESIAN_POINT('Ctrl Pts',(108.184331851862,21.3211540061394,26.));
#94950=CARTESIAN_POINT('Ctrl Pts',(108.17868709721,21.3359599004046,26.));
#94951=CARTESIAN_POINT('Ctrl Pts',(108.172986416033,21.3524951721887,26.));
#94952=CARTESIAN_POINT('Ctrl Pts',(108.167261205405,21.3707055346857,26.));
#94953=CARTESIAN_POINT('Ctrl Pts',(108.161565843382,21.3904834307621,26.));
#94954=CARTESIAN_POINT('Ctrl Pts',(108.155978401058,21.4116645975863,26.));
#94955=CARTESIAN_POINT('Ctrl Pts',(108.150587396044,21.4340592952825,26.));
#94956=CARTESIAN_POINT('Ctrl Pts',(108.14548095304,21.4574771160767,26.));
#94957=CARTESIAN_POINT('Ctrl Pts',(108.140736063183,21.4817516412614,26.));
#94958=CARTESIAN_POINT('Ctrl Pts',(108.136405082636,21.5067708088092,26.));
#94959=CARTESIAN_POINT('Ctrl Pts',(108.132512853008,21.5324835838215,26.));
#94960=CARTESIAN_POINT('Ctrl Pts',(108.129067047013,21.5588771351329,26.));
#94961=CARTESIAN_POINT('Ctrl Pts',(108.126065158383,21.5859611128485,26.));
#94962=CARTESIAN_POINT('Ctrl Pts',(108.123502124654,21.6137504395681,26.));
#94963=CARTESIAN_POINT('Ctrl Pts',(108.121378863907,21.6422453943083,26.));
#94964=CARTESIAN_POINT('Ctrl Pts',(108.119705321903,21.6714250926182,26.));
#94965=CARTESIAN_POINT('Ctrl Pts',(108.118496961822,21.7012568937955,26.));
#94966=CARTESIAN_POINT('Ctrl Pts',(108.117772886147,21.7317015453796,26.));
#94967=CARTESIAN_POINT('Ctrl Pts',(108.117553349757,21.7627194836669,26.));
#94968=CARTESIAN_POINT('Ctrl Pts',(108.117857140141,21.7942773949572,26.));
#94969=CARTESIAN_POINT('Ctrl Pts',(108.118699969278,21.8263513619102,26.));
#94970=CARTESIAN_POINT('Ctrl Pts',(108.120094755383,21.8589241514383,26.));
#94971=CARTESIAN_POINT('Ctrl Pts',(108.122051296525,21.8919838210329,26.));
#94972=CARTESIAN_POINT('Ctrl Pts',(108.12457611427,21.925521805893,26.));
#94973=CARTESIAN_POINT('Ctrl Pts',(108.127671920362,21.9595309601629,26.));
#94974=CARTESIAN_POINT('Ctrl Pts',(108.131337578276,21.9940041198301,26.));
#94975=CARTESIAN_POINT('Ctrl Pts',(108.135569853985,22.0289349713044,26.));
#94976=CARTESIAN_POINT('Ctrl Pts',(108.139405777158,22.0572417527814,26.));
#94977=CARTESIAN_POINT('Ctrl Pts',(108.142534384927,22.0786740240772,26.));
#94978=CARTESIAN_POINT('Ctrl Pts',(108.14473177204,22.0930519020204,26.));
#94979=CARTESIAN_POINT('Ctrl Pts',(108.145858377777,22.1002632652963,26.));
#94980=CARTESIAN_POINT('Origin',(108.525485805931,21.5597921651915,31.));
#94981=CARTESIAN_POINT('Origin',(109.652122916228,21.2061825485438,31.));
#94982=CARTESIAN_POINT('',(109.59454570101,21.7368385510191,31.));
#94983=CARTESIAN_POINT('',(109.59454570101,21.7368385510191,31.));
#94984=CARTESIAN_POINT('',(109.59454570101,21.7368385510191,26.));
#94985=CARTESIAN_POINT('',(109.59454570101,21.7368385510191,31.));
#94986=CARTESIAN_POINT('',(109.59454570101,21.7368385510191,26.));
#94987=CARTESIAN_POINT('Origin',(110.40545429899,21.7368385510191,31.));
#94988=CARTESIAN_POINT('',(110.40545429899,21.7368385510191,26.));
#94989=CARTESIAN_POINT('',(110.347877083772,21.2061825485438,26.));
#94990=CARTESIAN_POINT('',(110.40545429899,21.7368385510191,31.));
#94991=CARTESIAN_POINT('',(110.40545429899,21.7368385510191,31.));
#94992=CARTESIAN_POINT('',(110.347877083772,21.2061825485438,31.));
#94993=CARTESIAN_POINT('Ctrl Pts',(110.143900675185,22.4976985887986,31.));
#94994=CARTESIAN_POINT('Ctrl Pts',(110.143900675185,22.4976985887986,26.));
#94995=CARTESIAN_POINT('Ctrl Pts',(110.147701192472,22.4914672912168,31.));
#94996=CARTESIAN_POINT('Ctrl Pts',(110.147701192472,22.4914672912168,26.));
#94997=CARTESIAN_POINT('Ctrl Pts',(110.155233489225,22.4790247677066,31.));
#94998=CARTESIAN_POINT('Ctrl Pts',(110.155233489225,22.4790247677066,26.));
#94999=CARTESIAN_POINT('Ctrl Pts',(110.166325721145,22.4604211972804,31.));
#95000=CARTESIAN_POINT('Ctrl Pts',(110.166325721145,22.4604211972804,26.));
#95001=CARTESIAN_POINT('Ctrl Pts',(110.180702188389,22.4357370854887,31.));
#95002=CARTESIAN_POINT('Ctrl Pts',(110.180702188389,22.4357370854887,26.));
#95003=CARTESIAN_POINT('Ctrl Pts',(110.197979759379,22.4050848085535,31.));
#95004=CARTESIAN_POINT('Ctrl Pts',(110.197979759379,22.4050848085535,26.));
#95005=CARTESIAN_POINT('Ctrl Pts',(110.214558692659,22.3746385484685,31.));
#95006=CARTESIAN_POINT('Ctrl Pts',(110.214558692659,22.3746385484685,26.));
#95007=CARTESIAN_POINT('Ctrl Pts',(110.23043358432,22.3444029006218,31.));
#95008=CARTESIAN_POINT('Ctrl Pts',(110.23043358432,22.3444029006218,26.));
#95009=CARTESIAN_POINT('Ctrl Pts',(110.245600642837,22.314384048769,31.));
#95010=CARTESIAN_POINT('Ctrl Pts',(110.245600642837,22.314384048769,26.));
#95011=CARTESIAN_POINT('Ctrl Pts',(110.26005963895,22.2845896325587,31.));
#95012=CARTESIAN_POINT('Ctrl Pts',(110.26005963895,22.2845896325587,26.));
#95013=CARTESIAN_POINT('Ctrl Pts',(110.27381332019,22.2550300605308,31.));
#95014=CARTESIAN_POINT('Ctrl Pts',(110.27381332019,22.2550300605308,26.));
#95015=CARTESIAN_POINT('Ctrl Pts',(110.286866168579,22.2257201156837,31.));
#95016=CARTESIAN_POINT('Ctrl Pts',(110.286866168579,22.2257201156837,26.));
#95017=CARTESIAN_POINT('Ctrl Pts',(110.299223524153,22.1966806629003,31.));
#95018=CARTESIAN_POINT('Ctrl Pts',(110.299223524153,22.1966806629003,26.));
#95019=CARTESIAN_POINT('Ctrl Pts',(110.310890750103,22.1679398116366,31.));
#95020=CARTESIAN_POINT('Ctrl Pts',(110.310890750103,22.1679398116366,26.));
#95021=CARTESIAN_POINT('Ctrl Pts',(110.321872455192,22.1395355293992,31.));
#95022=CARTESIAN_POINT('Ctrl Pts',(110.321872455192,22.1395355293992,26.));
#95023=CARTESIAN_POINT('Ctrl Pts',(110.332172212114,22.1115121194901,31.));
#95024=CARTESIAN_POINT('Ctrl Pts',(110.332172212114,22.1115121194901,26.));
#95025=CARTESIAN_POINT('Ctrl Pts',(110.341792648001,22.0839131566587,31.));
#95026=CARTESIAN_POINT('Ctrl Pts',(110.341792648001,22.0839131566587,26.));
#95027=CARTESIAN_POINT('Ctrl Pts',(110.350735557918,22.056774714484,31.));
#95028=CARTESIAN_POINT('Ctrl Pts',(110.350735557918,22.056774714484,26.));
#95029=CARTESIAN_POINT('Ctrl Pts',(110.359002138426,22.0301198937606,31.));
#95030=CARTESIAN_POINT('Ctrl Pts',(110.359002138426,22.0301198937606,26.));
#95031=CARTESIAN_POINT('Ctrl Pts',(110.366593344504,22.0039487880456,31.));
#95032=CARTESIAN_POINT('Ctrl Pts',(110.366593344504,22.0039487880456,26.));
#95033=CARTESIAN_POINT('Ctrl Pts',(110.373510209678,21.978245673333,31.));
#95034=CARTESIAN_POINT('Ctrl Pts',(110.373510209678,21.978245673333,26.));
#95035=CARTESIAN_POINT('Ctrl Pts',(110.379754111393,21.9530006749816,31.));
#95036=CARTESIAN_POINT('Ctrl Pts',(110.379754111393,21.9530006749816,26.));
#95037=CARTESIAN_POINT('Ctrl Pts',(110.385327228035,21.9282285836627,31.));
#95038=CARTESIAN_POINT('Ctrl Pts',(110.385327228035,21.9282285836627,26.));
#95039=CARTESIAN_POINT('Ctrl Pts',(110.390232980042,21.9039860559466,31.));
#95040=CARTESIAN_POINT('Ctrl Pts',(110.390232980042,21.9039860559466,26.));
#95041=CARTESIAN_POINT('Ctrl Pts',(110.39447685392,21.8803966594834,31.));
#95042=CARTESIAN_POINT('Ctrl Pts',(110.39447685392,21.8803966594834,26.));
#95043=CARTESIAN_POINT('Ctrl Pts',(110.398066294513,21.8576436083425,31.));
#95044=CARTESIAN_POINT('Ctrl Pts',(110.398066294513,21.8576436083425,26.));
#95045=CARTESIAN_POINT('Ctrl Pts',(110.401009852528,21.8359365402324,31.));
#95046=CARTESIAN_POINT('Ctrl Pts',(110.401009852528,21.8359365402324,26.));
#95047=CARTESIAN_POINT('Ctrl Pts',(110.403316697266,21.8154846261632,31.));
#95048=CARTESIAN_POINT('Ctrl Pts',(110.403316697266,21.8154846261632,26.));
#95049=CARTESIAN_POINT('Ctrl Pts',(110.404996096355,21.7964695017177,31.));
#95050=CARTESIAN_POINT('Ctrl Pts',(110.404996096355,21.7964695017177,26.));
#95051=CARTESIAN_POINT('Ctrl Pts',(110.406057128242,21.7790113463118,31.));
#95052=CARTESIAN_POINT('Ctrl Pts',(110.406057128242,21.7790113463118,26.));
#95053=CARTESIAN_POINT('Ctrl Pts',(110.406508025383,21.7631723295541,31.));
#95054=CARTESIAN_POINT('Ctrl Pts',(110.406508025383,21.7631723295541,26.));
#95055=CARTESIAN_POINT('Ctrl Pts',(110.406385935655,21.7518162801327,31.));
#95056=CARTESIAN_POINT('Ctrl Pts',(110.406385935655,21.7518162801327,26.));
#95057=CARTESIAN_POINT('Ctrl Pts',(110.406024771161,21.7440398930577,31.));
#95058=CARTESIAN_POINT('Ctrl Pts',(110.406024771161,21.7440398930577,26.));
#95059=CARTESIAN_POINT('Ctrl Pts',(110.405664390446,21.7391842326632,31.));
#95060=CARTESIAN_POINT('Ctrl Pts',(110.405664390446,21.7391842326632,26.));
#95061=CARTESIAN_POINT('Ctrl Pts',(110.40545429899,21.7368385510191,31.));
#95062=CARTESIAN_POINT('Ctrl Pts',(110.40545429899,21.7368385510191,26.));
#95063=CARTESIAN_POINT('',(110.143900675185,22.4976985887986,31.));
#95064=CARTESIAN_POINT('Ctrl Pts',(110.40545429899,21.7368385510191,31.));
#95065=CARTESIAN_POINT('Ctrl Pts',(110.405664390446,21.7391842326632,31.));
#95066=CARTESIAN_POINT('Ctrl Pts',(110.406024771161,21.7440398930577,31.));
#95067=CARTESIAN_POINT('Ctrl Pts',(110.406385935655,21.7518162801327,31.));
#95068=CARTESIAN_POINT('Ctrl Pts',(110.406508025383,21.7631723295541,31.));
#95069=CARTESIAN_POINT('Ctrl Pts',(110.406057128242,21.7790113463118,31.));
#95070=CARTESIAN_POINT('Ctrl Pts',(110.404996096355,21.7964695017177,31.));
#95071=CARTESIAN_POINT('Ctrl Pts',(110.403316697266,21.8154846261632,31.));
#95072=CARTESIAN_POINT('Ctrl Pts',(110.401009852528,21.8359365402324,31.));
#95073=CARTESIAN_POINT('Ctrl Pts',(110.398066294513,21.8576436083425,31.));
#95074=CARTESIAN_POINT('Ctrl Pts',(110.39447685392,21.8803966594834,31.));
#95075=CARTESIAN_POINT('Ctrl Pts',(110.390232980042,21.9039860559466,31.));
#95076=CARTESIAN_POINT('Ctrl Pts',(110.385327228035,21.9282285836627,31.));
#95077=CARTESIAN_POINT('Ctrl Pts',(110.379754111393,21.9530006749816,31.));
#95078=CARTESIAN_POINT('Ctrl Pts',(110.373510209678,21.978245673333,31.));
#95079=CARTESIAN_POINT('Ctrl Pts',(110.366593344504,22.0039487880456,31.));
#95080=CARTESIAN_POINT('Ctrl Pts',(110.359002138426,22.0301198937606,31.));
#95081=CARTESIAN_POINT('Ctrl Pts',(110.350735557918,22.056774714484,31.));
#95082=CARTESIAN_POINT('Ctrl Pts',(110.341792648001,22.0839131566587,31.));
#95083=CARTESIAN_POINT('Ctrl Pts',(110.332172212114,22.1115121194901,31.));
#95084=CARTESIAN_POINT('Ctrl Pts',(110.321872455192,22.1395355293992,31.));
#95085=CARTESIAN_POINT('Ctrl Pts',(110.310890750103,22.1679398116366,31.));
#95086=CARTESIAN_POINT('Ctrl Pts',(110.299223524153,22.1966806629003,31.));
#95087=CARTESIAN_POINT('Ctrl Pts',(110.286866168579,22.2257201156837,31.));
#95088=CARTESIAN_POINT('Ctrl Pts',(110.27381332019,22.2550300605308,31.));
#95089=CARTESIAN_POINT('Ctrl Pts',(110.26005963895,22.2845896325587,31.));
#95090=CARTESIAN_POINT('Ctrl Pts',(110.245600642837,22.314384048769,31.));
#95091=CARTESIAN_POINT('Ctrl Pts',(110.23043358432,22.3444029006218,31.));
#95092=CARTESIAN_POINT('Ctrl Pts',(110.214558692659,22.3746385484685,31.));
#95093=CARTESIAN_POINT('Ctrl Pts',(110.197979759379,22.4050848085535,31.));
#95094=CARTESIAN_POINT('Ctrl Pts',(110.180702188389,22.4357370854887,31.));
#95095=CARTESIAN_POINT('Ctrl Pts',(110.166325721145,22.4604211972804,31.));
#95096=CARTESIAN_POINT('Ctrl Pts',(110.155233489225,22.4790247677066,31.));
#95097=CARTESIAN_POINT('Ctrl Pts',(110.147701192472,22.4914672912168,31.));
#95098=CARTESIAN_POINT('Ctrl Pts',(110.143900675185,22.4976985887986,31.));
#95099=CARTESIAN_POINT('',(110.143900675185,22.4976985887986,26.));
#95100=CARTESIAN_POINT('Ctrl Pts',(110.143900675185,22.4976985887986,26.));
#95101=CARTESIAN_POINT('Ctrl Pts',(110.147701192472,22.4914672912168,26.));
#95102=CARTESIAN_POINT('Ctrl Pts',(110.155233489225,22.4790247677066,26.));
#95103=CARTESIAN_POINT('Ctrl Pts',(110.166325721145,22.4604211972804,26.));
#95104=CARTESIAN_POINT('Ctrl Pts',(110.180702188389,22.4357370854887,26.));
#95105=CARTESIAN_POINT('Ctrl Pts',(110.197979759379,22.4050848085535,26.));
#95106=CARTESIAN_POINT('Ctrl Pts',(110.214558692659,22.3746385484685,26.));
#95107=CARTESIAN_POINT('Ctrl Pts',(110.23043358432,22.3444029006218,26.));
#95108=CARTESIAN_POINT('Ctrl Pts',(110.245600642837,22.314384048769,26.));
#95109=CARTESIAN_POINT('Ctrl Pts',(110.26005963895,22.2845896325587,26.));
#95110=CARTESIAN_POINT('Ctrl Pts',(110.27381332019,22.2550300605308,26.));
#95111=CARTESIAN_POINT('Ctrl Pts',(110.286866168579,22.2257201156837,26.));
#95112=CARTESIAN_POINT('Ctrl Pts',(110.299223524153,22.1966806629003,26.));
#95113=CARTESIAN_POINT('Ctrl Pts',(110.310890750103,22.1679398116366,26.));
#95114=CARTESIAN_POINT('Ctrl Pts',(110.321872455192,22.1395355293992,26.));
#95115=CARTESIAN_POINT('Ctrl Pts',(110.332172212114,22.1115121194901,26.));
#95116=CARTESIAN_POINT('Ctrl Pts',(110.341792648001,22.0839131566587,26.));
#95117=CARTESIAN_POINT('Ctrl Pts',(110.350735557918,22.056774714484,26.));
#95118=CARTESIAN_POINT('Ctrl Pts',(110.359002138426,22.0301198937606,26.));
#95119=CARTESIAN_POINT('Ctrl Pts',(110.366593344504,22.0039487880456,26.));
#95120=CARTESIAN_POINT('Ctrl Pts',(110.373510209678,21.978245673333,26.));
#95121=CARTESIAN_POINT('Ctrl Pts',(110.379754111393,21.9530006749816,26.));
#95122=CARTESIAN_POINT('Ctrl Pts',(110.385327228035,21.9282285836627,26.));
#95123=CARTESIAN_POINT('Ctrl Pts',(110.390232980042,21.9039860559466,26.));
#95124=CARTESIAN_POINT('Ctrl Pts',(110.39447685392,21.8803966594834,26.));
#95125=CARTESIAN_POINT('Ctrl Pts',(110.398066294513,21.8576436083425,26.));
#95126=CARTESIAN_POINT('Ctrl Pts',(110.401009852528,21.8359365402324,26.));
#95127=CARTESIAN_POINT('Ctrl Pts',(110.403316697266,21.8154846261632,26.));
#95128=CARTESIAN_POINT('Ctrl Pts',(110.404996096355,21.7964695017177,26.));
#95129=CARTESIAN_POINT('Ctrl Pts',(110.406057128242,21.7790113463118,26.));
#95130=CARTESIAN_POINT('Ctrl Pts',(110.406508025383,21.7631723295541,26.));
#95131=CARTESIAN_POINT('Ctrl Pts',(110.406385935655,21.7518162801327,26.));
#95132=CARTESIAN_POINT('Ctrl Pts',(110.406024771161,21.7440398930577,26.));
#95133=CARTESIAN_POINT('Ctrl Pts',(110.405664390446,21.7391842326632,26.));
#95134=CARTESIAN_POINT('Ctrl Pts',(110.40545429899,21.7368385510191,26.));
#95135=CARTESIAN_POINT('',(110.143900675185,22.4976985887986,31.));
#95136=CARTESIAN_POINT('Origin',(110.,17.999999999997,31.));
#95137=CARTESIAN_POINT('',(109.856099324815,22.4976985887986,31.));
#95138=CARTESIAN_POINT('Origin',(110.,17.999999999997,31.));
#95139=CARTESIAN_POINT('',(109.856099324815,22.4976985887986,26.));
#95140=CARTESIAN_POINT('Origin',(110.,17.999999999997,26.));
#95141=CARTESIAN_POINT('',(109.856099324815,22.4976985887986,31.));
#95142=CARTESIAN_POINT('Ctrl Pts',(109.59454570101,21.7368385510191,31.));
#95143=CARTESIAN_POINT('Ctrl Pts',(109.59454570101,21.7368385510191,26.));
#95144=CARTESIAN_POINT('Ctrl Pts',(109.594335609548,21.7391842326635,31.));
#95145=CARTESIAN_POINT('Ctrl Pts',(109.594335609548,21.7391842326635,26.));
#95146=CARTESIAN_POINT('Ctrl Pts',(109.593975228822,21.7440398930583,31.));
#95147=CARTESIAN_POINT('Ctrl Pts',(109.593975228822,21.7440398930583,26.));
#95148=CARTESIAN_POINT('Ctrl Pts',(109.593614064317,21.7518162801338,31.));
#95149=CARTESIAN_POINT('Ctrl Pts',(109.593614064317,21.7518162801338,26.));
#95150=CARTESIAN_POINT('Ctrl Pts',(109.593491974585,21.7631723295554,31.));
#95151=CARTESIAN_POINT('Ctrl Pts',(109.593491974585,21.7631723295554,26.));
#95152=CARTESIAN_POINT('Ctrl Pts',(109.593942871732,21.7790113463128,31.));
#95153=CARTESIAN_POINT('Ctrl Pts',(109.593942871732,21.7790113463128,26.));
#95154=CARTESIAN_POINT('Ctrl Pts',(109.595003903633,21.7964695017181,31.));
#95155=CARTESIAN_POINT('Ctrl Pts',(109.595003903633,21.7964695017181,26.));
#95156=CARTESIAN_POINT('Ctrl Pts',(109.59668330274,21.815484626163,31.));
#95157=CARTESIAN_POINT('Ctrl Pts',(109.59668330274,21.815484626163,26.));
#95158=CARTESIAN_POINT('Ctrl Pts',(109.598990147492,21.8359365402318,31.));
#95159=CARTESIAN_POINT('Ctrl Pts',(109.598990147492,21.8359365402318,26.));
#95160=CARTESIAN_POINT('Ctrl Pts',(109.601933705511,21.8576436083419,31.));
#95161=CARTESIAN_POINT('Ctrl Pts',(109.601933705511,21.8576436083419,26.));
#95162=CARTESIAN_POINT('Ctrl Pts',(109.6055231461,21.8803966594829,31.));
#95163=CARTESIAN_POINT('Ctrl Pts',(109.6055231461,21.8803966594829,26.));
#95164=CARTESIAN_POINT('Ctrl Pts',(109.609767019965,21.9039860559465,31.));
#95165=CARTESIAN_POINT('Ctrl Pts',(109.609767019965,21.9039860559465,26.));
#95166=CARTESIAN_POINT('Ctrl Pts',(109.614672771959,21.9282285836629,31.));
#95167=CARTESIAN_POINT('Ctrl Pts',(109.614672771959,21.9282285836629,26.));
#95168=CARTESIAN_POINT('Ctrl Pts',(109.620245888588,21.9530006749818,31.));
#95169=CARTESIAN_POINT('Ctrl Pts',(109.620245888588,21.9530006749818,26.));
#95170=CARTESIAN_POINT('Ctrl Pts',(109.626489790297,21.9782456733333,31.));
#95171=CARTESIAN_POINT('Ctrl Pts',(109.626489790297,21.9782456733333,26.));
#95172=CARTESIAN_POINT('Ctrl Pts',(109.633406655472,22.0039487880458,31.));
#95173=CARTESIAN_POINT('Ctrl Pts',(109.633406655472,22.0039487880458,26.));
#95174=CARTESIAN_POINT('Ctrl Pts',(109.640997861563,22.0301198937606,31.));
#95175=CARTESIAN_POINT('Ctrl Pts',(109.640997861563,22.0301198937606,26.));
#95176=CARTESIAN_POINT('Ctrl Pts',(109.649264442091,22.056774714484,31.));
#95177=CARTESIAN_POINT('Ctrl Pts',(109.649264442091,22.056774714484,26.));
#95178=CARTESIAN_POINT('Ctrl Pts',(109.65820735203,22.0839131566587,31.));
#95179=CARTESIAN_POINT('Ctrl Pts',(109.65820735203,22.0839131566587,26.));
#95180=CARTESIAN_POINT('Ctrl Pts',(109.667827787931,22.1115121194901,31.));
#95181=CARTESIAN_POINT('Ctrl Pts',(109.667827787931,22.1115121194901,26.));
#95182=CARTESIAN_POINT('Ctrl Pts',(109.678127544852,22.1395355293993,31.));
#95183=CARTESIAN_POINT('Ctrl Pts',(109.678127544852,22.1395355293993,26.));
#95184=CARTESIAN_POINT('Ctrl Pts',(109.689109249922,22.1679398116367,31.));
#95185=CARTESIAN_POINT('Ctrl Pts',(109.689109249922,22.1679398116367,26.));
#95186=CARTESIAN_POINT('Ctrl Pts',(109.700776475833,22.1966806629002,31.));
#95187=CARTESIAN_POINT('Ctrl Pts',(109.700776475833,22.1966806629002,26.));
#95188=CARTESIAN_POINT('Ctrl Pts',(109.713133831361,22.2257201156836,31.));
#95189=CARTESIAN_POINT('Ctrl Pts',(109.713133831361,22.2257201156836,26.));
#95190=CARTESIAN_POINT('Ctrl Pts',(109.726186679714,22.2550300605307,31.));
#95191=CARTESIAN_POINT('Ctrl Pts',(109.726186679714,22.2550300605307,26.));
#95192=CARTESIAN_POINT('Ctrl Pts',(109.739940360947,22.2845896325585,31.));
#95193=CARTESIAN_POINT('Ctrl Pts',(109.739940360947,22.2845896325585,26.));
#95194=CARTESIAN_POINT('Ctrl Pts',(109.754399357095,22.3143840487689,31.));
#95195=CARTESIAN_POINT('Ctrl Pts',(109.754399357095,22.3143840487689,26.));
#95196=CARTESIAN_POINT('Ctrl Pts',(109.769566415695,22.3444029006219,31.));
#95197=CARTESIAN_POINT('Ctrl Pts',(109.769566415695,22.3444029006219,26.));
#95198=CARTESIAN_POINT('Ctrl Pts',(109.785441307467,22.3746385484687,31.));
#95199=CARTESIAN_POINT('Ctrl Pts',(109.785441307467,22.3746385484687,26.));
#95200=CARTESIAN_POINT('Ctrl Pts',(109.802020240853,22.4050848085539,31.));
#95201=CARTESIAN_POINT('Ctrl Pts',(109.802020240853,22.4050848085539,26.));
#95202=CARTESIAN_POINT('Ctrl Pts',(109.819297811894,22.435737085489,31.));
#95203=CARTESIAN_POINT('Ctrl Pts',(109.819297811894,22.435737085489,26.));
#95204=CARTESIAN_POINT('Ctrl Pts',(109.833674279097,22.4604211972807,31.));
#95205=CARTESIAN_POINT('Ctrl Pts',(109.833674279097,22.4604211972807,26.));
#95206=CARTESIAN_POINT('Ctrl Pts',(109.844766510922,22.4790247677067,31.));
#95207=CARTESIAN_POINT('Ctrl Pts',(109.844766510922,22.4790247677067,26.));
#95208=CARTESIAN_POINT('Ctrl Pts',(109.852298807583,22.4914672912169,31.));
#95209=CARTESIAN_POINT('Ctrl Pts',(109.852298807583,22.4914672912169,26.));
#95210=CARTESIAN_POINT('Ctrl Pts',(109.856099324815,22.4976985887986,31.));
#95211=CARTESIAN_POINT('Ctrl Pts',(109.856099324815,22.4976985887986,26.));
#95212=CARTESIAN_POINT('Ctrl Pts',(109.59454570101,21.7368385510191,31.));
#95213=CARTESIAN_POINT('Ctrl Pts',(109.594335609548,21.7391842326635,31.));
#95214=CARTESIAN_POINT('Ctrl Pts',(109.593975228822,21.7440398930583,31.));
#95215=CARTESIAN_POINT('Ctrl Pts',(109.593614064317,21.7518162801338,31.));
#95216=CARTESIAN_POINT('Ctrl Pts',(109.593491974585,21.7631723295554,31.));
#95217=CARTESIAN_POINT('Ctrl Pts',(109.593942871732,21.7790113463128,31.));
#95218=CARTESIAN_POINT('Ctrl Pts',(109.595003903633,21.7964695017181,31.));
#95219=CARTESIAN_POINT('Ctrl Pts',(109.59668330274,21.815484626163,31.));
#95220=CARTESIAN_POINT('Ctrl Pts',(109.598990147492,21.8359365402318,31.));
#95221=CARTESIAN_POINT('Ctrl Pts',(109.601933705511,21.8576436083419,31.));
#95222=CARTESIAN_POINT('Ctrl Pts',(109.6055231461,21.8803966594829,31.));
#95223=CARTESIAN_POINT('Ctrl Pts',(109.609767019965,21.9039860559465,31.));
#95224=CARTESIAN_POINT('Ctrl Pts',(109.614672771959,21.9282285836629,31.));
#95225=CARTESIAN_POINT('Ctrl Pts',(109.620245888588,21.9530006749818,31.));
#95226=CARTESIAN_POINT('Ctrl Pts',(109.626489790297,21.9782456733333,31.));
#95227=CARTESIAN_POINT('Ctrl Pts',(109.633406655472,22.0039487880458,31.));
#95228=CARTESIAN_POINT('Ctrl Pts',(109.640997861563,22.0301198937606,31.));
#95229=CARTESIAN_POINT('Ctrl Pts',(109.649264442091,22.056774714484,31.));
#95230=CARTESIAN_POINT('Ctrl Pts',(109.65820735203,22.0839131566587,31.));
#95231=CARTESIAN_POINT('Ctrl Pts',(109.667827787931,22.1115121194901,31.));
#95232=CARTESIAN_POINT('Ctrl Pts',(109.678127544852,22.1395355293993,31.));
#95233=CARTESIAN_POINT('Ctrl Pts',(109.689109249922,22.1679398116367,31.));
#95234=CARTESIAN_POINT('Ctrl Pts',(109.700776475833,22.1966806629002,31.));
#95235=CARTESIAN_POINT('Ctrl Pts',(109.713133831361,22.2257201156836,31.));
#95236=CARTESIAN_POINT('Ctrl Pts',(109.726186679714,22.2550300605307,31.));
#95237=CARTESIAN_POINT('Ctrl Pts',(109.739940360947,22.2845896325585,31.));
#95238=CARTESIAN_POINT('Ctrl Pts',(109.754399357095,22.3143840487689,31.));
#95239=CARTESIAN_POINT('Ctrl Pts',(109.769566415695,22.3444029006219,31.));
#95240=CARTESIAN_POINT('Ctrl Pts',(109.785441307467,22.3746385484687,31.));
#95241=CARTESIAN_POINT('Ctrl Pts',(109.802020240853,22.4050848085539,31.));
#95242=CARTESIAN_POINT('Ctrl Pts',(109.819297811894,22.435737085489,31.));
#95243=CARTESIAN_POINT('Ctrl Pts',(109.833674279097,22.4604211972807,31.));
#95244=CARTESIAN_POINT('Ctrl Pts',(109.844766510922,22.4790247677067,31.));
#95245=CARTESIAN_POINT('Ctrl Pts',(109.852298807583,22.4914672912169,31.));
#95246=CARTESIAN_POINT('Ctrl Pts',(109.856099324815,22.4976985887986,31.));
#95247=CARTESIAN_POINT('Ctrl Pts',(109.59454570101,21.7368385510191,26.));
#95248=CARTESIAN_POINT('Ctrl Pts',(109.594335609548,21.7391842326635,26.));
#95249=CARTESIAN_POINT('Ctrl Pts',(109.593975228822,21.7440398930583,26.));
#95250=CARTESIAN_POINT('Ctrl Pts',(109.593614064317,21.7518162801338,26.));
#95251=CARTESIAN_POINT('Ctrl Pts',(109.593491974585,21.7631723295554,26.));
#95252=CARTESIAN_POINT('Ctrl Pts',(109.593942871732,21.7790113463128,26.));
#95253=CARTESIAN_POINT('Ctrl Pts',(109.595003903633,21.7964695017181,26.));
#95254=CARTESIAN_POINT('Ctrl Pts',(109.59668330274,21.815484626163,26.));
#95255=CARTESIAN_POINT('Ctrl Pts',(109.598990147492,21.8359365402318,26.));
#95256=CARTESIAN_POINT('Ctrl Pts',(109.601933705511,21.8576436083419,26.));
#95257=CARTESIAN_POINT('Ctrl Pts',(109.6055231461,21.8803966594829,26.));
#95258=CARTESIAN_POINT('Ctrl Pts',(109.609767019965,21.9039860559465,26.));
#95259=CARTESIAN_POINT('Ctrl Pts',(109.614672771959,21.9282285836629,26.));
#95260=CARTESIAN_POINT('Ctrl Pts',(109.620245888588,21.9530006749818,26.));
#95261=CARTESIAN_POINT('Ctrl Pts',(109.626489790297,21.9782456733333,26.));
#95262=CARTESIAN_POINT('Ctrl Pts',(109.633406655472,22.0039487880458,26.));
#95263=CARTESIAN_POINT('Ctrl Pts',(109.640997861563,22.0301198937606,26.));
#95264=CARTESIAN_POINT('Ctrl Pts',(109.649264442091,22.056774714484,26.));
#95265=CARTESIAN_POINT('Ctrl Pts',(109.65820735203,22.0839131566587,26.));
#95266=CARTESIAN_POINT('Ctrl Pts',(109.667827787931,22.1115121194901,26.));
#95267=CARTESIAN_POINT('Ctrl Pts',(109.678127544852,22.1395355293993,26.));
#95268=CARTESIAN_POINT('Ctrl Pts',(109.689109249922,22.1679398116367,26.));
#95269=CARTESIAN_POINT('Ctrl Pts',(109.700776475833,22.1966806629002,26.));
#95270=CARTESIAN_POINT('Ctrl Pts',(109.713133831361,22.2257201156836,26.));
#95271=CARTESIAN_POINT('Ctrl Pts',(109.726186679714,22.2550300605307,26.));
#95272=CARTESIAN_POINT('Ctrl Pts',(109.739940360947,22.2845896325585,26.));
#95273=CARTESIAN_POINT('Ctrl Pts',(109.754399357095,22.3143840487689,26.));
#95274=CARTESIAN_POINT('Ctrl Pts',(109.769566415695,22.3444029006219,26.));
#95275=CARTESIAN_POINT('Ctrl Pts',(109.785441307467,22.3746385484687,26.));
#95276=CARTESIAN_POINT('Ctrl Pts',(109.802020240853,22.4050848085539,26.));
#95277=CARTESIAN_POINT('Ctrl Pts',(109.819297811894,22.435737085489,26.));
#95278=CARTESIAN_POINT('Ctrl Pts',(109.833674279097,22.4604211972807,26.));
#95279=CARTESIAN_POINT('Ctrl Pts',(109.844766510922,22.4790247677067,26.));
#95280=CARTESIAN_POINT('Ctrl Pts',(109.852298807583,22.4914672912169,26.));
#95281=CARTESIAN_POINT('Ctrl Pts',(109.856099324815,22.4976985887986,26.));
#95282=CARTESIAN_POINT('Origin',(109.999999999984,21.8530912742719,31.));
#95283=CARTESIAN_POINT('Origin',(110.90555642494,21.0952532305533,31.));
#95284=CARTESIAN_POINT('',(111.055435274693,21.6075492963903,31.));
#95285=CARTESIAN_POINT('',(111.055435274693,21.6075492963903,31.));
#95286=CARTESIAN_POINT('',(111.055435274693,21.6075492963903,26.));
#95287=CARTESIAN_POINT('',(111.055435274693,21.6075492963903,31.));
#95288=CARTESIAN_POINT('',(111.055435274693,21.6075492963903,26.));
#95289=CARTESIAN_POINT('Origin',(111.804617131104,21.297228010781,31.));
#95290=CARTESIAN_POINT('',(111.804617131104,21.297228010781,26.));
#95291=CARTESIAN_POINT('',(111.548349459992,20.8289996376356,26.));
#95292=CARTESIAN_POINT('',(111.804617131104,21.297228010781,31.));
#95293=CARTESIAN_POINT('',(111.804617131104,21.297228010781,31.));
#95294=CARTESIAN_POINT('',(111.548349459992,20.8289996376356,31.));
#95295=CARTESIAN_POINT('Ctrl Pts',(111.854141622223,22.1002632652963,31.));
#95296=CARTESIAN_POINT('Ctrl Pts',(111.854141622223,22.1002632652963,26.));
#95297=CARTESIAN_POINT('Ctrl Pts',(111.855268228011,22.0930519019996,31.));
#95298=CARTESIAN_POINT('Ctrl Pts',(111.855268228011,22.0930519019996,26.));
#95299=CARTESIAN_POINT('Ctrl Pts',(111.85746561521,22.0786740240205,31.));
#95300=CARTESIAN_POINT('Ctrl Pts',(111.85746561521,22.0786740240205,26.));
#95301=CARTESIAN_POINT('Ctrl Pts',(111.860594223066,22.0572417526884,31.));
#95302=CARTESIAN_POINT('Ctrl Pts',(111.860594223066,22.0572417526884,26.));
#95303=CARTESIAN_POINT('Ctrl Pts',(111.864430146276,22.0289349711957,31.));
#95304=CARTESIAN_POINT('Ctrl Pts',(111.864430146276,22.0289349711957,26.));
#95305=CARTESIAN_POINT('Ctrl Pts',(111.868662421939,21.994004119741,31.));
#95306=CARTESIAN_POINT('Ctrl Pts',(111.868662421939,21.994004119741,26.));
#95307=CARTESIAN_POINT('Ctrl Pts',(111.872328079755,21.9595309601143,31.));
#95308=CARTESIAN_POINT('Ctrl Pts',(111.872328079755,21.9595309601143,26.));
#95309=CARTESIAN_POINT('Ctrl Pts',(111.875423885743,21.9255218058874,31.));
#95310=CARTESIAN_POINT('Ctrl Pts',(111.875423885743,21.9255218058874,26.));
#95311=CARTESIAN_POINT('Ctrl Pts',(111.877948703413,21.8919838210589,31.));
#95312=CARTESIAN_POINT('Ctrl Pts',(111.877948703413,21.8919838210589,26.));
#95313=CARTESIAN_POINT('Ctrl Pts',(111.879905244522,21.858924151478,31.));
#95314=CARTESIAN_POINT('Ctrl Pts',(111.879905244522,21.858924151478,26.));
#95315=CARTESIAN_POINT('Ctrl Pts',(111.881300030633,21.8263513619471,31.));
#95316=CARTESIAN_POINT('Ctrl Pts',(111.881300030633,21.8263513619471,26.));
#95317=CARTESIAN_POINT('Ctrl Pts',(111.882142859804,21.7942773949803,31.));
#95318=CARTESIAN_POINT('Ctrl Pts',(111.882142859804,21.7942773949803,26.));
#95319=CARTESIAN_POINT('Ctrl Pts',(111.88244665023,21.7627194836722,31.));
#95320=CARTESIAN_POINT('Ctrl Pts',(111.88244665023,21.7627194836722,26.));
#95321=CARTESIAN_POINT('Ctrl Pts',(111.882227113875,21.7317015453702,31.));
#95322=CARTESIAN_POINT('Ctrl Pts',(111.882227113875,21.7317015453702,26.));
#95323=CARTESIAN_POINT('Ctrl Pts',(111.881503038219,21.7012568937784,31.));
#95324=CARTESIAN_POINT('Ctrl Pts',(111.881503038219,21.7012568937784,26.));
#95325=CARTESIAN_POINT('Ctrl Pts',(111.880294678138,21.6714250926009,31.));
#95326=CARTESIAN_POINT('Ctrl Pts',(111.880294678138,21.6714250926009,26.));
#95327=CARTESIAN_POINT('Ctrl Pts',(111.878621136122,21.6422453942965,31.));
#95328=CARTESIAN_POINT('Ctrl Pts',(111.878621136122,21.6422453942965,26.));
#95329=CARTESIAN_POINT('Ctrl Pts',(111.876497875355,21.6137504395647,31.));
#95330=CARTESIAN_POINT('Ctrl Pts',(111.876497875355,21.6137504395647,26.));
#95331=CARTESIAN_POINT('Ctrl Pts',(111.873934841606,21.5859611128528,31.));
#95332=CARTESIAN_POINT('Ctrl Pts',(111.873934841606,21.5859611128528,26.));
#95333=CARTESIAN_POINT('Ctrl Pts',(111.870932952965,21.5588771351418,31.));
#95334=CARTESIAN_POINT('Ctrl Pts',(111.870932952965,21.5588771351418,26.));
#95335=CARTESIAN_POINT('Ctrl Pts',(111.867487146968,21.5324835838312,31.));
#95336=CARTESIAN_POINT('Ctrl Pts',(111.867487146968,21.5324835838312,26.));
#95337=CARTESIAN_POINT('Ctrl Pts',(111.863594917346,21.5067708088162,31.));
#95338=CARTESIAN_POINT('Ctrl Pts',(111.863594917346,21.5067708088162,26.));
#95339=CARTESIAN_POINT('Ctrl Pts',(111.859263936811,21.4817516412638,31.));
#95340=CARTESIAN_POINT('Ctrl Pts',(111.859263936811,21.4817516412638,26.));
#95341=CARTESIAN_POINT('Ctrl Pts',(111.854519046967,21.4574771160738,31.));
#95342=CARTESIAN_POINT('Ctrl Pts',(111.854519046967,21.4574771160738,26.));
#95343=CARTESIAN_POINT('Ctrl Pts',(111.849412603975,21.4340592952752,31.));
#95344=CARTESIAN_POINT('Ctrl Pts',(111.849412603975,21.4340592952752,26.));
#95345=CARTESIAN_POINT('Ctrl Pts',(111.844021598965,21.4116645975774,31.));
#95346=CARTESIAN_POINT('Ctrl Pts',(111.844021598965,21.4116645975774,26.));
#95347=CARTESIAN_POINT('Ctrl Pts',(111.838434156637,21.3904834307551,31.));
#95348=CARTESIAN_POINT('Ctrl Pts',(111.838434156637,21.3904834307551,26.));
#95349=CARTESIAN_POINT('Ctrl Pts',(111.832738794601,21.3707055346837,31.));
#95350=CARTESIAN_POINT('Ctrl Pts',(111.832738794601,21.3707055346837,26.));
#95351=CARTESIAN_POINT('Ctrl Pts',(111.827013583956,21.3524951721927,31.));
#95352=CARTESIAN_POINT('Ctrl Pts',(111.827013583956,21.3524951721927,26.));
#95353=CARTESIAN_POINT('Ctrl Pts',(111.821312902766,21.3359599004136,31.));
#95354=CARTESIAN_POINT('Ctrl Pts',(111.821312902766,21.3359599004136,26.));
#95355=CARTESIAN_POINT('Ctrl Pts',(111.815668148108,21.3211540061504,31.));
#95356=CARTESIAN_POINT('Ctrl Pts',(111.815668148108,21.3211540061504,26.));
#95357=CARTESIAN_POINT('Ctrl Pts',(111.811209579937,21.3107091062357,31.));
#95358=CARTESIAN_POINT('Ctrl Pts',(111.811209579937,21.3107091062357,26.));
#95359=CARTESIAN_POINT('Ctrl Pts',(111.807900012956,21.3036628730485,31.));
#95360=CARTESIAN_POINT('Ctrl Pts',(111.807900012956,21.3036628730485,26.));
#95361=CARTESIAN_POINT('Ctrl Pts',(111.805708883803,21.2993147395223,31.));
#95362=CARTESIAN_POINT('Ctrl Pts',(111.805708883803,21.2993147395223,26.));
#95363=CARTESIAN_POINT('Ctrl Pts',(111.804617131104,21.297228010781,31.));
#95364=CARTESIAN_POINT('Ctrl Pts',(111.804617131104,21.297228010781,26.));
#95365=CARTESIAN_POINT('',(111.854141622223,22.1002632652963,31.));
#95366=CARTESIAN_POINT('Ctrl Pts',(111.804617131104,21.297228010781,31.));
#95367=CARTESIAN_POINT('Ctrl Pts',(111.805708883803,21.2993147395223,31.));
#95368=CARTESIAN_POINT('Ctrl Pts',(111.807900012956,21.3036628730485,31.));
#95369=CARTESIAN_POINT('Ctrl Pts',(111.811209579937,21.3107091062357,31.));
#95370=CARTESIAN_POINT('Ctrl Pts',(111.815668148108,21.3211540061504,31.));
#95371=CARTESIAN_POINT('Ctrl Pts',(111.821312902766,21.3359599004136,31.));
#95372=CARTESIAN_POINT('Ctrl Pts',(111.827013583956,21.3524951721927,31.));
#95373=CARTESIAN_POINT('Ctrl Pts',(111.832738794601,21.3707055346837,31.));
#95374=CARTESIAN_POINT('Ctrl Pts',(111.838434156637,21.3904834307551,31.));
#95375=CARTESIAN_POINT('Ctrl Pts',(111.844021598965,21.4116645975774,31.));
#95376=CARTESIAN_POINT('Ctrl Pts',(111.849412603975,21.4340592952752,31.));
#95377=CARTESIAN_POINT('Ctrl Pts',(111.854519046967,21.4574771160738,31.));
#95378=CARTESIAN_POINT('Ctrl Pts',(111.859263936811,21.4817516412638,31.));
#95379=CARTESIAN_POINT('Ctrl Pts',(111.863594917346,21.5067708088162,31.));
#95380=CARTESIAN_POINT('Ctrl Pts',(111.867487146968,21.5324835838312,31.));
#95381=CARTESIAN_POINT('Ctrl Pts',(111.870932952965,21.5588771351418,31.));
#95382=CARTESIAN_POINT('Ctrl Pts',(111.873934841606,21.5859611128528,31.));
#95383=CARTESIAN_POINT('Ctrl Pts',(111.876497875355,21.6137504395647,31.));
#95384=CARTESIAN_POINT('Ctrl Pts',(111.878621136122,21.6422453942965,31.));
#95385=CARTESIAN_POINT('Ctrl Pts',(111.880294678138,21.6714250926009,31.));
#95386=CARTESIAN_POINT('Ctrl Pts',(111.881503038219,21.7012568937784,31.));
#95387=CARTESIAN_POINT('Ctrl Pts',(111.882227113875,21.7317015453702,31.));
#95388=CARTESIAN_POINT('Ctrl Pts',(111.88244665023,21.7627194836722,31.));
#95389=CARTESIAN_POINT('Ctrl Pts',(111.882142859804,21.7942773949803,31.));
#95390=CARTESIAN_POINT('Ctrl Pts',(111.881300030633,21.8263513619471,31.));
#95391=CARTESIAN_POINT('Ctrl Pts',(111.879905244522,21.858924151478,31.));
#95392=CARTESIAN_POINT('Ctrl Pts',(111.877948703413,21.8919838210589,31.));
#95393=CARTESIAN_POINT('Ctrl Pts',(111.875423885743,21.9255218058874,31.));
#95394=CARTESIAN_POINT('Ctrl Pts',(111.872328079755,21.9595309601143,31.));
#95395=CARTESIAN_POINT('Ctrl Pts',(111.868662421939,21.994004119741,31.));
#95396=CARTESIAN_POINT('Ctrl Pts',(111.864430146276,22.0289349711957,31.));
#95397=CARTESIAN_POINT('Ctrl Pts',(111.860594223066,22.0572417526884,31.));
#95398=CARTESIAN_POINT('Ctrl Pts',(111.85746561521,22.0786740240205,31.));
#95399=CARTESIAN_POINT('Ctrl Pts',(111.855268228011,22.0930519019996,31.));
#95400=CARTESIAN_POINT('Ctrl Pts',(111.854141622223,22.1002632652963,31.));
#95401=CARTESIAN_POINT('',(111.854141622223,22.1002632652963,26.));
#95402=CARTESIAN_POINT('Ctrl Pts',(111.854141622223,22.1002632652963,26.));
#95403=CARTESIAN_POINT('Ctrl Pts',(111.855268228011,22.0930519019996,26.));
#95404=CARTESIAN_POINT('Ctrl Pts',(111.85746561521,22.0786740240205,26.));
#95405=CARTESIAN_POINT('Ctrl Pts',(111.860594223066,22.0572417526884,26.));
#95406=CARTESIAN_POINT('Ctrl Pts',(111.864430146276,22.0289349711957,26.));
#95407=CARTESIAN_POINT('Ctrl Pts',(111.868662421939,21.994004119741,26.));
#95408=CARTESIAN_POINT('Ctrl Pts',(111.872328079755,21.9595309601143,26.));
#95409=CARTESIAN_POINT('Ctrl Pts',(111.875423885743,21.9255218058874,26.));
#95410=CARTESIAN_POINT('Ctrl Pts',(111.877948703413,21.8919838210589,26.));
#95411=CARTESIAN_POINT('Ctrl Pts',(111.879905244522,21.858924151478,26.));
#95412=CARTESIAN_POINT('Ctrl Pts',(111.881300030633,21.8263513619471,26.));
#95413=CARTESIAN_POINT('Ctrl Pts',(111.882142859804,21.7942773949803,26.));
#95414=CARTESIAN_POINT('Ctrl Pts',(111.88244665023,21.7627194836722,26.));
#95415=CARTESIAN_POINT('Ctrl Pts',(111.882227113875,21.7317015453702,26.));
#95416=CARTESIAN_POINT('Ctrl Pts',(111.881503038219,21.7012568937784,26.));
#95417=CARTESIAN_POINT('Ctrl Pts',(111.880294678138,21.6714250926009,26.));
#95418=CARTESIAN_POINT('Ctrl Pts',(111.878621136122,21.6422453942965,26.));
#95419=CARTESIAN_POINT('Ctrl Pts',(111.876497875355,21.6137504395647,26.));
#95420=CARTESIAN_POINT('Ctrl Pts',(111.873934841606,21.5859611128528,26.));
#95421=CARTESIAN_POINT('Ctrl Pts',(111.870932952965,21.5588771351418,26.));
#95422=CARTESIAN_POINT('Ctrl Pts',(111.867487146968,21.5324835838312,26.));
#95423=CARTESIAN_POINT('Ctrl Pts',(111.863594917346,21.5067708088162,26.));
#95424=CARTESIAN_POINT('Ctrl Pts',(111.859263936811,21.4817516412638,26.));
#95425=CARTESIAN_POINT('Ctrl Pts',(111.854519046967,21.4574771160738,26.));
#95426=CARTESIAN_POINT('Ctrl Pts',(111.849412603975,21.4340592952752,26.));
#95427=CARTESIAN_POINT('Ctrl Pts',(111.844021598965,21.4116645975774,26.));
#95428=CARTESIAN_POINT('Ctrl Pts',(111.838434156637,21.3904834307551,26.));
#95429=CARTESIAN_POINT('Ctrl Pts',(111.832738794601,21.3707055346837,26.));
#95430=CARTESIAN_POINT('Ctrl Pts',(111.827013583956,21.3524951721927,26.));
#95431=CARTESIAN_POINT('Ctrl Pts',(111.821312902766,21.3359599004136,26.));
#95432=CARTESIAN_POINT('Ctrl Pts',(111.815668148108,21.3211540061504,26.));
#95433=CARTESIAN_POINT('Ctrl Pts',(111.811209579937,21.3107091062357,26.));
#95434=CARTESIAN_POINT('Ctrl Pts',(111.807900012956,21.3036628730485,26.));
#95435=CARTESIAN_POINT('Ctrl Pts',(111.805708883803,21.2993147395223,26.));
#95436=CARTESIAN_POINT('Ctrl Pts',(111.804617131104,21.297228010781,26.));
#95437=CARTESIAN_POINT('',(111.854141622223,22.1002632652963,31.));
#95438=CARTESIAN_POINT('Origin',(109.999999999999,17.9999999999972,31.));
#95439=CARTESIAN_POINT('',(111.588247845187,22.2104000738956,31.));
#95440=CARTESIAN_POINT('Origin',(109.999999999999,17.9999999999972,31.));
#95441=CARTESIAN_POINT('',(111.588247845187,22.2104000738956,26.));
#95442=CARTESIAN_POINT('Origin',(109.999999999999,17.9999999999972,26.));
#95443=CARTESIAN_POINT('',(111.588247845187,22.2104000738956,31.));
#95444=CARTESIAN_POINT('Ctrl Pts',(111.055435274693,21.6075492963903,31.));
#95445=CARTESIAN_POINT('Ctrl Pts',(111.055435274693,21.6075492963903,26.));
#95446=CARTESIAN_POINT('Ctrl Pts',(111.056138828994,21.6097968221732,31.));
#95447=CARTESIAN_POINT('Ctrl Pts',(111.056138828994,21.6097968221732,26.));
#95448=CARTESIAN_POINT('Ctrl Pts',(111.057664061403,21.6144207791619,31.));
#95449=CARTESIAN_POINT('Ctrl Pts',(111.057664061403,21.6144207791619,26.));
#95450=CARTESIAN_POINT('Ctrl Pts',(111.060306283407,21.6217434356902,31.));
#95451=CARTESIAN_POINT('Ctrl Pts',(111.060306283407,21.6217434356902,26.));
#95452=CARTESIAN_POINT('Ctrl Pts',(111.064539259173,21.6322817790386,31.));
#95453=CARTESIAN_POINT('Ctrl Pts',(111.064539259173,21.6322817790386,26.));
#95454=CARTESIAN_POINT('Ctrl Pts',(111.071017163117,21.6467425715681,31.));
#95455=CARTESIAN_POINT('Ctrl Pts',(111.071017163117,21.6467425715681,26.));
#95456=CARTESIAN_POINT('Ctrl Pts',(111.078678375607,21.6624657646927,31.));
#95457=CARTESIAN_POINT('Ctrl Pts',(111.078678375607,21.6624657646927,26.));
#95458=CARTESIAN_POINT('Ctrl Pts',(111.087506711157,21.6793907707612,31.));
#95459=CARTESIAN_POINT('Ctrl Pts',(111.087506711157,21.6793907707612,26.));
#95460=CARTESIAN_POINT('Ctrl Pts',(111.097464566483,21.6974030843025,31.));
#95461=CARTESIAN_POINT('Ctrl Pts',(111.097464566483,21.6974030843025,26.));
#95462=CARTESIAN_POINT('Ctrl Pts',(111.108490994821,21.7163313493538,31.));
#95463=CARTESIAN_POINT('Ctrl Pts',(111.108490994821,21.7163313493538,26.));
#95464=CARTESIAN_POINT('Ctrl Pts',(111.120514421221,21.7359788081604,31.));
#95465=CARTESIAN_POINT('Ctrl Pts',(111.120514421221,21.7359788081604,26.));
#95466=CARTESIAN_POINT('Ctrl Pts',(111.13346252063,21.7561485085201,31.));
#95467=CARTESIAN_POINT('Ctrl Pts',(111.13346252063,21.7561485085201,26.));
#95468=CARTESIAN_POINT('Ctrl Pts',(111.147272058204,21.7766683336824,31.));
#95469=CARTESIAN_POINT('Ctrl Pts',(111.147272058204,21.7766683336824,26.));
#95470=CARTESIAN_POINT('Ctrl Pts',(111.161900815523,21.7974220224288,31.));
#95471=CARTESIAN_POINT('Ctrl Pts',(111.161900815523,21.7974220224288,26.));
#95472=CARTESIAN_POINT('Ctrl Pts',(111.177330271134,21.8183559219669,31.));
#95473=CARTESIAN_POINT('Ctrl Pts',(111.177330271134,21.8183559219669,26.));
#95474=CARTESIAN_POINT('Ctrl Pts',(111.19355677746,21.8394555338648,31.));
#95475=CARTESIAN_POINT('Ctrl Pts',(111.19355677746,21.8394555338648,26.));
#95476=CARTESIAN_POINT('Ctrl Pts',(111.210585385957,21.8607294539754,31.));
#95477=CARTESIAN_POINT('Ctrl Pts',(111.210585385957,21.8607294539754,26.));
#95478=CARTESIAN_POINT('Ctrl Pts',(111.228423068795,21.882191813874,31.));
#95479=CARTESIAN_POINT('Ctrl Pts',(111.228423068795,21.882191813874,26.));
#95480=CARTESIAN_POINT('Ctrl Pts',(111.247070672449,21.9038421616728,31.));
#95481=CARTESIAN_POINT('Ctrl Pts',(111.247070672449,21.9038421616728,26.));
#95482=CARTESIAN_POINT('Ctrl Pts',(111.266520462098,21.9256586971199,31.));
#95483=CARTESIAN_POINT('Ctrl Pts',(111.266520462098,21.9256586971199,26.));
#95484=CARTESIAN_POINT('Ctrl Pts',(111.286760291397,21.9476074056351,31.));
#95485=CARTESIAN_POINT('Ctrl Pts',(111.286760291397,21.9476074056351,26.));
#95486=CARTESIAN_POINT('Ctrl Pts',(111.307775912164,21.9696470240406,31.));
#95487=CARTESIAN_POINT('Ctrl Pts',(111.307775912164,21.9696470240406,26.));
#95488=CARTESIAN_POINT('Ctrl Pts',(111.329553670995,21.991735254212,31.));
#95489=CARTESIAN_POINT('Ctrl Pts',(111.329553670995,21.991735254212,26.));
#95490=CARTESIAN_POINT('Ctrl Pts',(111.352083296309,22.0138352550454,31.));
#95491=CARTESIAN_POINT('Ctrl Pts',(111.352083296309,22.0138352550454,26.));
#95492=CARTESIAN_POINT('Ctrl Pts',(111.375358986039,22.0359190043789,31.));
#95493=CARTESIAN_POINT('Ctrl Pts',(111.375358986039,22.0359190043789,26.));
#95494=CARTESIAN_POINT('Ctrl Pts',(111.39937768911,22.0579651820235,31.));
#95495=CARTESIAN_POINT('Ctrl Pts',(111.39937768911,22.0579651820235,26.));
#95496=CARTESIAN_POINT('Ctrl Pts',(111.424137889173,22.0799584150686,31.));
#95497=CARTESIAN_POINT('Ctrl Pts',(111.424137889173,22.0799584150686,26.));
#95498=CARTESIAN_POINT('Ctrl Pts',(111.449638141444,22.1018880358414,31.));
#95499=CARTESIAN_POINT('Ctrl Pts',(111.449638141444,22.1018880358414,26.));
#95500=CARTESIAN_POINT('Ctrl Pts',(111.475875310531,22.1237470739672,31.));
#95501=CARTESIAN_POINT('Ctrl Pts',(111.475875310531,22.1237470739672,26.));
#95502=CARTESIAN_POINT('Ctrl Pts',(111.502843527069,22.1455312673685,31.));
#95503=CARTESIAN_POINT('Ctrl Pts',(111.502843527069,22.1455312673685,26.));
#95504=CARTESIAN_POINT('Ctrl Pts',(111.530536039873,22.1672384384647,31.));
#95505=CARTESIAN_POINT('Ctrl Pts',(111.530536039873,22.1672384384647,26.));
#95506=CARTESIAN_POINT('Ctrl Pts',(111.553264364297,22.1845419483128,31.));
#95507=CARTESIAN_POINT('Ctrl Pts',(111.553264364297,22.1845419483128,26.));
#95508=CARTESIAN_POINT('Ctrl Pts',(111.570631528435,22.1974845929136,31.));
#95509=CARTESIAN_POINT('Ctrl Pts',(111.570631528435,22.1974845929136,26.));
#95510=CARTESIAN_POINT('Ctrl Pts',(111.582352010756,22.2060975005779,31.));
#95511=CARTESIAN_POINT('Ctrl Pts',(111.582352010756,22.2060975005779,26.));
#95512=CARTESIAN_POINT('Ctrl Pts',(111.588247845187,22.2104000738956,31.));
#95513=CARTESIAN_POINT('Ctrl Pts',(111.588247845187,22.2104000738956,26.));
#95514=CARTESIAN_POINT('Ctrl Pts',(111.055435274693,21.6075492963903,31.));
#95515=CARTESIAN_POINT('Ctrl Pts',(111.056138828994,21.6097968221732,31.));
#95516=CARTESIAN_POINT('Ctrl Pts',(111.057664061403,21.6144207791619,31.));
#95517=CARTESIAN_POINT('Ctrl Pts',(111.060306283407,21.6217434356902,31.));
#95518=CARTESIAN_POINT('Ctrl Pts',(111.064539259173,21.6322817790386,31.));
#95519=CARTESIAN_POINT('Ctrl Pts',(111.071017163117,21.6467425715681,31.));
#95520=CARTESIAN_POINT('Ctrl Pts',(111.078678375607,21.6624657646927,31.));
#95521=CARTESIAN_POINT('Ctrl Pts',(111.087506711157,21.6793907707612,31.));
#95522=CARTESIAN_POINT('Ctrl Pts',(111.097464566483,21.6974030843025,31.));
#95523=CARTESIAN_POINT('Ctrl Pts',(111.108490994821,21.7163313493538,31.));
#95524=CARTESIAN_POINT('Ctrl Pts',(111.120514421221,21.7359788081604,31.));
#95525=CARTESIAN_POINT('Ctrl Pts',(111.13346252063,21.7561485085201,31.));
#95526=CARTESIAN_POINT('Ctrl Pts',(111.147272058204,21.7766683336824,31.));
#95527=CARTESIAN_POINT('Ctrl Pts',(111.161900815523,21.7974220224288,31.));
#95528=CARTESIAN_POINT('Ctrl Pts',(111.177330271134,21.8183559219669,31.));
#95529=CARTESIAN_POINT('Ctrl Pts',(111.19355677746,21.8394555338648,31.));
#95530=CARTESIAN_POINT('Ctrl Pts',(111.210585385957,21.8607294539754,31.));
#95531=CARTESIAN_POINT('Ctrl Pts',(111.228423068795,21.882191813874,31.));
#95532=CARTESIAN_POINT('Ctrl Pts',(111.247070672449,21.9038421616728,31.));
#95533=CARTESIAN_POINT('Ctrl Pts',(111.266520462098,21.9256586971199,31.));
#95534=CARTESIAN_POINT('Ctrl Pts',(111.286760291397,21.9476074056351,31.));
#95535=CARTESIAN_POINT('Ctrl Pts',(111.307775912164,21.9696470240406,31.));
#95536=CARTESIAN_POINT('Ctrl Pts',(111.329553670995,21.991735254212,31.));
#95537=CARTESIAN_POINT('Ctrl Pts',(111.352083296309,22.0138352550454,31.));
#95538=CARTESIAN_POINT('Ctrl Pts',(111.375358986039,22.0359190043789,31.));
#95539=CARTESIAN_POINT('Ctrl Pts',(111.39937768911,22.0579651820235,31.));
#95540=CARTESIAN_POINT('Ctrl Pts',(111.424137889173,22.0799584150686,31.));
#95541=CARTESIAN_POINT('Ctrl Pts',(111.449638141444,22.1018880358414,31.));
#95542=CARTESIAN_POINT('Ctrl Pts',(111.475875310531,22.1237470739672,31.));
#95543=CARTESIAN_POINT('Ctrl Pts',(111.502843527069,22.1455312673685,31.));
#95544=CARTESIAN_POINT('Ctrl Pts',(111.530536039873,22.1672384384647,31.));
#95545=CARTESIAN_POINT('Ctrl Pts',(111.553264364297,22.1845419483128,31.));
#95546=CARTESIAN_POINT('Ctrl Pts',(111.570631528435,22.1974845929136,31.));
#95547=CARTESIAN_POINT('Ctrl Pts',(111.582352010756,22.2060975005779,31.));
#95548=CARTESIAN_POINT('Ctrl Pts',(111.588247845187,22.2104000738956,31.));
#95549=CARTESIAN_POINT('Ctrl Pts',(111.055435274693,21.6075492963903,26.));
#95550=CARTESIAN_POINT('Ctrl Pts',(111.056138828994,21.6097968221732,26.));
#95551=CARTESIAN_POINT('Ctrl Pts',(111.057664061403,21.6144207791619,26.));
#95552=CARTESIAN_POINT('Ctrl Pts',(111.060306283407,21.6217434356902,26.));
#95553=CARTESIAN_POINT('Ctrl Pts',(111.064539259173,21.6322817790386,26.));
#95554=CARTESIAN_POINT('Ctrl Pts',(111.071017163117,21.6467425715681,26.));
#95555=CARTESIAN_POINT('Ctrl Pts',(111.078678375607,21.6624657646927,26.));
#95556=CARTESIAN_POINT('Ctrl Pts',(111.087506711157,21.6793907707612,26.));
#95557=CARTESIAN_POINT('Ctrl Pts',(111.097464566483,21.6974030843025,26.));
#95558=CARTESIAN_POINT('Ctrl Pts',(111.108490994821,21.7163313493538,26.));
#95559=CARTESIAN_POINT('Ctrl Pts',(111.120514421221,21.7359788081604,26.));
#95560=CARTESIAN_POINT('Ctrl Pts',(111.13346252063,21.7561485085201,26.));
#95561=CARTESIAN_POINT('Ctrl Pts',(111.147272058204,21.7766683336824,26.));
#95562=CARTESIAN_POINT('Ctrl Pts',(111.161900815523,21.7974220224288,26.));
#95563=CARTESIAN_POINT('Ctrl Pts',(111.177330271134,21.8183559219669,26.));
#95564=CARTESIAN_POINT('Ctrl Pts',(111.19355677746,21.8394555338648,26.));
#95565=CARTESIAN_POINT('Ctrl Pts',(111.210585385957,21.8607294539754,26.));
#95566=CARTESIAN_POINT('Ctrl Pts',(111.228423068795,21.882191813874,26.));
#95567=CARTESIAN_POINT('Ctrl Pts',(111.247070672449,21.9038421616728,26.));
#95568=CARTESIAN_POINT('Ctrl Pts',(111.266520462098,21.9256586971199,26.));
#95569=CARTESIAN_POINT('Ctrl Pts',(111.286760291397,21.9476074056351,26.));
#95570=CARTESIAN_POINT('Ctrl Pts',(111.307775912164,21.9696470240406,26.));
#95571=CARTESIAN_POINT('Ctrl Pts',(111.329553670995,21.991735254212,26.));
#95572=CARTESIAN_POINT('Ctrl Pts',(111.352083296309,22.0138352550454,26.));
#95573=CARTESIAN_POINT('Ctrl Pts',(111.375358986039,22.0359190043789,26.));
#95574=CARTESIAN_POINT('Ctrl Pts',(111.39937768911,22.0579651820235,26.));
#95575=CARTESIAN_POINT('Ctrl Pts',(111.424137889173,22.0799584150686,26.));
#95576=CARTESIAN_POINT('Ctrl Pts',(111.449638141444,22.1018880358414,26.));
#95577=CARTESIAN_POINT('Ctrl Pts',(111.475875310531,22.1237470739672,26.));
#95578=CARTESIAN_POINT('Ctrl Pts',(111.502843527069,22.1455312673685,26.));
#95579=CARTESIAN_POINT('Ctrl Pts',(111.530536039873,22.1672384384647,26.));
#95580=CARTESIAN_POINT('Ctrl Pts',(111.553264364297,22.1845419483128,26.));
#95581=CARTESIAN_POINT('Ctrl Pts',(111.570631528435,22.1974845929136,26.));
#95582=CARTESIAN_POINT('Ctrl Pts',(111.582352010756,22.2060975005779,26.));
#95583=CARTESIAN_POINT('Ctrl Pts',(111.588247845187,22.2104000738956,26.));
#95584=CARTESIAN_POINT('Origin',(111.47451419404,21.5597921652037,31.));
#95585=CARTESIAN_POINT('Origin',(112.021127176843,20.5130996667515,31.));
#95586=CARTESIAN_POINT('',(112.355644395348,20.9290433639019,31.));
#95587=CARTESIAN_POINT('',(112.355644395348,20.9290433639019,31.));
#95588=CARTESIAN_POINT('',(112.355644395348,20.9290433639019,26.));
#95589=CARTESIAN_POINT('',(112.355644395348,20.9290433639019,31.));
#95590=CARTESIAN_POINT('',(112.355644395348,20.9290433639019,26.));
#95591=CARTESIAN_POINT('Origin',(112.929043363902,20.3556443953479,31.));
#95592=CARTESIAN_POINT('',(112.929043363902,20.3556443953479,26.));
#95593=CARTESIAN_POINT('',(112.513099666752,20.021127176843,26.));
#95594=CARTESIAN_POINT('',(112.929043363902,20.3556443953479,31.));
#95595=CARTESIAN_POINT('',(112.929043363902,20.3556443953479,31.));
#95596=CARTESIAN_POINT('',(112.513099666752,20.021127176843,31.));
#95597=CARTESIAN_POINT('Ctrl Pts',(113.282106315114,21.0786000286317,31.));
#95598=CARTESIAN_POINT('Ctrl Pts',(113.282106315114,21.0786000286317,26.));
#95599=CARTESIAN_POINT('Ctrl Pts',(113.280387493883,21.0715064643109,31.));
#95600=CARTESIAN_POINT('Ctrl Pts',(113.280387493883,21.0715064643109,26.));
#95601=CARTESIAN_POINT('Ctrl Pts',(113.276915439246,21.0573821334494,31.));
#95602=CARTESIAN_POINT('Ctrl Pts',(113.276915439246,21.0573821334494,26.));
#95603=CARTESIAN_POINT('Ctrl Pts',(113.271604120853,21.0363840302376,31.));
#95604=CARTESIAN_POINT('Ctrl Pts',(113.271604120853,21.0363840302376,26.));
#95605=CARTESIAN_POINT('Ctrl Pts',(113.264315515495,21.0087640299247,31.));
#95606=CARTESIAN_POINT('Ctrl Pts',(113.264315515495,21.0087640299247,26.));
#95607=CARTESIAN_POINT('Ctrl Pts',(113.254858170225,20.9748725094354,31.));
#95608=CARTESIAN_POINT('Ctrl Pts',(113.254858170225,20.9748725094354,26.));
#95609=CARTESIAN_POINT('Ctrl Pts',(113.245052489404,20.9416206763202,31.));
#95610=CARTESIAN_POINT('Ctrl Pts',(113.245052489404,20.9416206763202,26.));
#95611=CARTESIAN_POINT('Ctrl Pts',(113.234897901322,20.9090156011505,31.));
#95612=CARTESIAN_POINT('Ctrl Pts',(113.234897901322,20.9090156011505,26.));
#95613=CARTESIAN_POINT('Ctrl Pts',(113.224396097542,20.8770643375138,31.));
#95614=CARTESIAN_POINT('Ctrl Pts',(113.224396097542,20.8770643375138,26.));
#95615=CARTESIAN_POINT('Ctrl Pts',(113.213552317998,20.8457724495694,31.));
#95616=CARTESIAN_POINT('Ctrl Pts',(113.213552317998,20.8457724495694,26.));
#95617=CARTESIAN_POINT('Ctrl Pts',(113.20237586544,20.8151453544684,31.));
#95618=CARTESIAN_POINT('Ctrl Pts',(113.20237586544,20.8151453544684,26.));
#95619=CARTESIAN_POINT('Ctrl Pts',(113.190880362291,20.7851903361014,31.));
#95620=CARTESIAN_POINT('Ctrl Pts',(113.190880362291,20.7851903361014,26.));
#95621=CARTESIAN_POINT('Ctrl Pts',(113.179084338231,20.755918372192,31.));
#95622=CARTESIAN_POINT('Ctrl Pts',(113.179084338231,20.755918372192,26.));
#95623=CARTESIAN_POINT('Ctrl Pts',(113.167011461991,20.7273455467799,31.));
#95624=CARTESIAN_POINT('Ctrl Pts',(113.167011461991,20.7273455467799,26.));
#95625=CARTESIAN_POINT('Ctrl Pts',(113.154691839545,20.6994954480571,31.));
#95626=CARTESIAN_POINT('Ctrl Pts',(113.154691839545,20.6994954480571,26.));
#95627=CARTESIAN_POINT('Ctrl Pts',(113.14215932433,20.6723968769145,31.));
#95628=CARTESIAN_POINT('Ctrl Pts',(113.14215932433,20.6723968769145,26.));
#95629=CARTESIAN_POINT('Ctrl Pts',(113.129446586011,20.6460787876893,31.));
#95630=CARTESIAN_POINT('Ctrl Pts',(113.129446586011,20.6460787876893,26.));
#95631=CARTESIAN_POINT('Ctrl Pts',(113.116580401765,20.620565418951,31.));
#95632=CARTESIAN_POINT('Ctrl Pts',(113.116580401765,20.620565418951,26.));
#95633=CARTESIAN_POINT('Ctrl Pts',(113.103577952414,20.5958722593316,31.));
#95634=CARTESIAN_POINT('Ctrl Pts',(113.103577952414,20.5958722593316,26.));
#95635=CARTESIAN_POINT('Ctrl Pts',(113.090439979387,20.5719986997143,31.));
#95636=CARTESIAN_POINT('Ctrl Pts',(113.090439979387,20.5719986997143,26.));
#95637=CARTESIAN_POINT('Ctrl Pts',(113.077156094945,20.5489328907344,31.));
#95638=CARTESIAN_POINT('Ctrl Pts',(113.077156094945,20.5489328907344,26.));
#95639=CARTESIAN_POINT('Ctrl Pts',(113.063720290664,20.5266668759651,31.));
#95640=CARTESIAN_POINT('Ctrl Pts',(113.063720290664,20.5266668759651,26.));
#95641=CARTESIAN_POINT('Ctrl Pts',(113.050144565478,20.5052095736397,31.));
#95642=CARTESIAN_POINT('Ctrl Pts',(113.050144565478,20.5052095736397,26.));
#95643=CARTESIAN_POINT('Ctrl Pts',(113.036471400248,20.4845986273869,31.));
#95644=CARTESIAN_POINT('Ctrl Pts',(113.036471400248,20.4845986273869,26.));
#95645=CARTESIAN_POINT('Ctrl Pts',(113.022792050042,20.4649175331864,31.));
#95646=CARTESIAN_POINT('Ctrl Pts',(113.022792050042,20.4649175331864,26.));
#95647=CARTESIAN_POINT('Ctrl Pts',(113.009241331072,20.4462905786477,31.));
#95648=CARTESIAN_POINT('Ctrl Pts',(113.009241331072,20.4462905786477,26.));
#95649=CARTESIAN_POINT('Ctrl Pts',(112.995973525845,20.4288599537543,31.));
#95650=CARTESIAN_POINT('Ctrl Pts',(112.995973525845,20.4288599537543,26.));
#95651=CARTESIAN_POINT('Ctrl Pts',(112.983143024276,20.4127670810703,31.));
#95652=CARTESIAN_POINT('Ctrl Pts',(112.983143024276,20.4127670810703,26.));
#95653=CARTESIAN_POINT('Ctrl Pts',(112.970884815319,20.3981338431457,31.));
#95654=CARTESIAN_POINT('Ctrl Pts',(112.970884815319,20.3981338431457,26.));
#95655=CARTESIAN_POINT('Ctrl Pts',(112.959290298087,20.3850388002292,31.));
#95656=CARTESIAN_POINT('Ctrl Pts',(112.959290298087,20.3850388002292,26.));
#95657=CARTESIAN_POINT('Ctrl Pts',(112.948409254356,20.3735200916464,31.));
#95658=CARTESIAN_POINT('Ctrl Pts',(112.948409254356,20.3735200916464,26.));
#95659=CARTESIAN_POINT('Ctrl Pts',(112.940292984329,20.3655764825671,31.));
#95660=CARTESIAN_POINT('Ctrl Pts',(112.940292984329,20.3655764825671,26.));
#95661=CARTESIAN_POINT('Ctrl Pts',(112.934538866432,20.3603331283963,31.));
#95662=CARTESIAN_POINT('Ctrl Pts',(112.934538866432,20.3603331283963,26.));
#95663=CARTESIAN_POINT('Ctrl Pts',(112.930850568392,20.3571544856518,31.));
#95664=CARTESIAN_POINT('Ctrl Pts',(112.930850568392,20.3571544856518,26.));
#95665=CARTESIAN_POINT('Ctrl Pts',(112.929043363902,20.3556443953479,31.));
#95666=CARTESIAN_POINT('Ctrl Pts',(112.929043363902,20.3556443953479,26.));
#95667=CARTESIAN_POINT('',(113.282106315114,21.0786000286317,31.));
#95668=CARTESIAN_POINT('Ctrl Pts',(112.929043363902,20.3556443953479,31.));
#95669=CARTESIAN_POINT('Ctrl Pts',(112.930850568392,20.3571544856518,31.));
#95670=CARTESIAN_POINT('Ctrl Pts',(112.934538866432,20.3603331283963,31.));
#95671=CARTESIAN_POINT('Ctrl Pts',(112.940292984329,20.3655764825671,31.));
#95672=CARTESIAN_POINT('Ctrl Pts',(112.948409254356,20.3735200916464,31.));
#95673=CARTESIAN_POINT('Ctrl Pts',(112.959290298087,20.3850388002292,31.));
#95674=CARTESIAN_POINT('Ctrl Pts',(112.970884815319,20.3981338431457,31.));
#95675=CARTESIAN_POINT('Ctrl Pts',(112.983143024276,20.4127670810703,31.));
#95676=CARTESIAN_POINT('Ctrl Pts',(112.995973525845,20.4288599537543,31.));
#95677=CARTESIAN_POINT('Ctrl Pts',(113.009241331072,20.4462905786477,31.));
#95678=CARTESIAN_POINT('Ctrl Pts',(113.022792050042,20.4649175331864,31.));
#95679=CARTESIAN_POINT('Ctrl Pts',(113.036471400248,20.4845986273869,31.));
#95680=CARTESIAN_POINT('Ctrl Pts',(113.050144565478,20.5052095736397,31.));
#95681=CARTESIAN_POINT('Ctrl Pts',(113.063720290664,20.5266668759651,31.));
#95682=CARTESIAN_POINT('Ctrl Pts',(113.077156094945,20.5489328907344,31.));
#95683=CARTESIAN_POINT('Ctrl Pts',(113.090439979387,20.5719986997143,31.));
#95684=CARTESIAN_POINT('Ctrl Pts',(113.103577952414,20.5958722593316,31.));
#95685=CARTESIAN_POINT('Ctrl Pts',(113.116580401765,20.620565418951,31.));
#95686=CARTESIAN_POINT('Ctrl Pts',(113.129446586011,20.6460787876893,31.));
#95687=CARTESIAN_POINT('Ctrl Pts',(113.14215932433,20.6723968769145,31.));
#95688=CARTESIAN_POINT('Ctrl Pts',(113.154691839545,20.6994954480571,31.));
#95689=CARTESIAN_POINT('Ctrl Pts',(113.167011461991,20.7273455467799,31.));
#95690=CARTESIAN_POINT('Ctrl Pts',(113.179084338231,20.755918372192,31.));
#95691=CARTESIAN_POINT('Ctrl Pts',(113.190880362291,20.7851903361014,31.));
#95692=CARTESIAN_POINT('Ctrl Pts',(113.20237586544,20.8151453544684,31.));
#95693=CARTESIAN_POINT('Ctrl Pts',(113.213552317998,20.8457724495694,31.));
#95694=CARTESIAN_POINT('Ctrl Pts',(113.224396097542,20.8770643375138,31.));
#95695=CARTESIAN_POINT('Ctrl Pts',(113.234897901322,20.9090156011505,31.));
#95696=CARTESIAN_POINT('Ctrl Pts',(113.245052489404,20.9416206763202,31.));
#95697=CARTESIAN_POINT('Ctrl Pts',(113.254858170225,20.9748725094354,31.));
#95698=CARTESIAN_POINT('Ctrl Pts',(113.264315515495,21.0087640299247,31.));
#95699=CARTESIAN_POINT('Ctrl Pts',(113.271604120853,21.0363840302376,31.));
#95700=CARTESIAN_POINT('Ctrl Pts',(113.276915439246,21.0573821334494,31.));
#95701=CARTESIAN_POINT('Ctrl Pts',(113.280387493883,21.0715064643109,31.));
#95702=CARTESIAN_POINT('Ctrl Pts',(113.282106315114,21.0786000286317,31.));
#95703=CARTESIAN_POINT('',(113.282106315114,21.0786000286317,26.));
#95704=CARTESIAN_POINT('Ctrl Pts',(113.282106315114,21.0786000286317,26.));
#95705=CARTESIAN_POINT('Ctrl Pts',(113.280387493883,21.0715064643109,26.));
#95706=CARTESIAN_POINT('Ctrl Pts',(113.276915439246,21.0573821334494,26.));
#95707=CARTESIAN_POINT('Ctrl Pts',(113.271604120853,21.0363840302376,26.));
#95708=CARTESIAN_POINT('Ctrl Pts',(113.264315515495,21.0087640299247,26.));
#95709=CARTESIAN_POINT('Ctrl Pts',(113.254858170225,20.9748725094354,26.));
#95710=CARTESIAN_POINT('Ctrl Pts',(113.245052489404,20.9416206763202,26.));
#95711=CARTESIAN_POINT('Ctrl Pts',(113.234897901322,20.9090156011505,26.));
#95712=CARTESIAN_POINT('Ctrl Pts',(113.224396097542,20.8770643375138,26.));
#95713=CARTESIAN_POINT('Ctrl Pts',(113.213552317998,20.8457724495694,26.));
#95714=CARTESIAN_POINT('Ctrl Pts',(113.20237586544,20.8151453544684,26.));
#95715=CARTESIAN_POINT('Ctrl Pts',(113.190880362291,20.7851903361014,26.));
#95716=CARTESIAN_POINT('Ctrl Pts',(113.179084338231,20.755918372192,26.));
#95717=CARTESIAN_POINT('Ctrl Pts',(113.167011461991,20.7273455467799,26.));
#95718=CARTESIAN_POINT('Ctrl Pts',(113.154691839545,20.6994954480571,26.));
#95719=CARTESIAN_POINT('Ctrl Pts',(113.14215932433,20.6723968769145,26.));
#95720=CARTESIAN_POINT('Ctrl Pts',(113.129446586011,20.6460787876893,26.));
#95721=CARTESIAN_POINT('Ctrl Pts',(113.116580401765,20.620565418951,26.));
#95722=CARTESIAN_POINT('Ctrl Pts',(113.103577952414,20.5958722593316,26.));
#95723=CARTESIAN_POINT('Ctrl Pts',(113.090439979387,20.5719986997143,26.));
#95724=CARTESIAN_POINT('Ctrl Pts',(113.077156094945,20.5489328907344,26.));
#95725=CARTESIAN_POINT('Ctrl Pts',(113.063720290664,20.5266668759651,26.));
#95726=CARTESIAN_POINT('Ctrl Pts',(113.050144565478,20.5052095736397,26.));
#95727=CARTESIAN_POINT('Ctrl Pts',(113.036471400248,20.4845986273869,26.));
#95728=CARTESIAN_POINT('Ctrl Pts',(113.022792050042,20.4649175331864,26.));
#95729=CARTESIAN_POINT('Ctrl Pts',(113.009241331072,20.4462905786477,26.));
#95730=CARTESIAN_POINT('Ctrl Pts',(112.995973525845,20.4288599537543,26.));
#95731=CARTESIAN_POINT('Ctrl Pts',(112.983143024276,20.4127670810703,26.));
#95732=CARTESIAN_POINT('Ctrl Pts',(112.970884815319,20.3981338431457,26.));
#95733=CARTESIAN_POINT('Ctrl Pts',(112.959290298087,20.3850388002292,26.));
#95734=CARTESIAN_POINT('Ctrl Pts',(112.948409254356,20.3735200916464,26.));
#95735=CARTESIAN_POINT('Ctrl Pts',(112.940292984329,20.3655764825671,26.));
#95736=CARTESIAN_POINT('Ctrl Pts',(112.934538866432,20.3603331283963,26.));
#95737=CARTESIAN_POINT('Ctrl Pts',(112.930850568392,20.3571544856518,26.));
#95738=CARTESIAN_POINT('Ctrl Pts',(112.929043363902,20.3556443953479,26.));
#95739=CARTESIAN_POINT('',(113.282106315114,21.0786000286317,31.));
#95740=CARTESIAN_POINT('Origin',(109.999999999998,17.9999999999978,31.));
#95741=CARTESIAN_POINT('',(113.078600028632,21.2821063151136,31.));
#95742=CARTESIAN_POINT('Origin',(109.999999999998,17.9999999999978,31.));
#95743=CARTESIAN_POINT('',(113.078600028632,21.2821063151136,26.));
#95744=CARTESIAN_POINT('Origin',(109.999999999998,17.9999999999978,26.));
#95745=CARTESIAN_POINT('',(113.078600028632,21.2821063151136,31.));
#95746=CARTESIAN_POINT('Ctrl Pts',(112.355644395348,20.9290433639019,31.));
#95747=CARTESIAN_POINT('Ctrl Pts',(112.355644395348,20.9290433639019,26.));
#95748=CARTESIAN_POINT('Ctrl Pts',(112.357154485648,20.9308505683967,31.));
#95749=CARTESIAN_POINT('Ctrl Pts',(112.357154485648,20.9308505683967,26.));
#95750=CARTESIAN_POINT('Ctrl Pts',(112.360333128385,20.9345388664441,31.));
#95751=CARTESIAN_POINT('Ctrl Pts',(112.360333128385,20.9345388664441,26.));
#95752=CARTESIAN_POINT('Ctrl Pts',(112.365576482549,20.9402929843488,31.));
#95753=CARTESIAN_POINT('Ctrl Pts',(112.365576482549,20.9402929843488,26.));
#95754=CARTESIAN_POINT('Ctrl Pts',(112.373520091625,20.9484092543796,31.));
#95755=CARTESIAN_POINT('Ctrl Pts',(112.373520091625,20.9484092543796,26.));
#95756=CARTESIAN_POINT('Ctrl Pts',(112.385038800212,20.9592902981059,31.));
#95757=CARTESIAN_POINT('Ctrl Pts',(112.385038800212,20.9592902981059,26.));
#95758=CARTESIAN_POINT('Ctrl Pts',(112.398133843138,20.9708848153277,31.));
#95759=CARTESIAN_POINT('Ctrl Pts',(112.398133843138,20.9708848153277,26.));
#95760=CARTESIAN_POINT('Ctrl Pts',(112.412767081074,20.9831430242715,31.));
#95761=CARTESIAN_POINT('Ctrl Pts',(112.412767081074,20.9831430242715,26.));
#95762=CARTESIAN_POINT('Ctrl Pts',(112.428859953768,20.9959735258305,31.));
#95763=CARTESIAN_POINT('Ctrl Pts',(112.428859953768,20.9959735258305,26.));
#95764=CARTESIAN_POINT('Ctrl Pts',(112.446290578665,21.0092413310541,31.));
#95765=CARTESIAN_POINT('Ctrl Pts',(112.446290578665,21.0092413310541,26.));
#95766=CARTESIAN_POINT('Ctrl Pts',(112.4649175332,21.0227920500277,31.));
#95767=CARTESIAN_POINT('Ctrl Pts',(112.4649175332,21.0227920500277,26.));
#95768=CARTESIAN_POINT('Ctrl Pts',(112.484598627392,21.0364714002426,31.));
#95769=CARTESIAN_POINT('Ctrl Pts',(112.484598627392,21.0364714002426,26.));
#95770=CARTESIAN_POINT('Ctrl Pts',(112.505209573635,21.0501445654825,31.));
#95771=CARTESIAN_POINT('Ctrl Pts',(112.505209573635,21.0501445654825,26.));
#95772=CARTESIAN_POINT('Ctrl Pts',(112.526666875952,21.0637202906774,31.));
#95773=CARTESIAN_POINT('Ctrl Pts',(112.526666875952,21.0637202906774,26.));
#95774=CARTESIAN_POINT('Ctrl Pts',(112.548932890716,21.0771560949637,31.));
#95775=CARTESIAN_POINT('Ctrl Pts',(112.548932890716,21.0771560949637,26.));
#95776=CARTESIAN_POINT('Ctrl Pts',(112.571998699698,21.0904399794041,31.));
#95777=CARTESIAN_POINT('Ctrl Pts',(112.571998699698,21.0904399794041,26.));
#95778=CARTESIAN_POINT('Ctrl Pts',(112.595872259324,21.1035779524222,31.));
#95779=CARTESIAN_POINT('Ctrl Pts',(112.595872259324,21.1035779524222,26.));
#95780=CARTESIAN_POINT('Ctrl Pts',(112.620565418957,21.1165804017582,31.));
#95781=CARTESIAN_POINT('Ctrl Pts',(112.620565418957,21.1165804017582,26.));
#95782=CARTESIAN_POINT('Ctrl Pts',(112.646078787711,21.1294465859895,31.));
#95783=CARTESIAN_POINT('Ctrl Pts',(112.646078787711,21.1294465859895,26.));
#95784=CARTESIAN_POINT('Ctrl Pts',(112.672396876946,21.1421593242979,31.));
#95785=CARTESIAN_POINT('Ctrl Pts',(112.672396876946,21.1421593242979,26.));
#95786=CARTESIAN_POINT('Ctrl Pts',(112.699495448089,21.1546918395131,31.));
#95787=CARTESIAN_POINT('Ctrl Pts',(112.699495448089,21.1546918395131,26.));
#95788=CARTESIAN_POINT('Ctrl Pts',(112.727345546797,21.1670114619741,31.));
#95789=CARTESIAN_POINT('Ctrl Pts',(112.727345546797,21.1670114619741,26.));
#95790=CARTESIAN_POINT('Ctrl Pts',(112.755918372182,21.1790843382401,31.));
#95791=CARTESIAN_POINT('Ctrl Pts',(112.755918372182,21.1790843382401,26.));
#95792=CARTESIAN_POINT('Ctrl Pts',(112.785190336059,21.1908803623338,31.));
#95793=CARTESIAN_POINT('Ctrl Pts',(112.785190336059,21.1908803623338,26.));
#95794=CARTESIAN_POINT('Ctrl Pts',(112.8151453544,21.2023758655074,31.));
#95795=CARTESIAN_POINT('Ctrl Pts',(112.8151453544,21.2023758655074,26.));
#95796=CARTESIAN_POINT('Ctrl Pts',(112.845772449496,21.2135523180713,31.));
#95797=CARTESIAN_POINT('Ctrl Pts',(112.845772449496,21.2135523180713,26.));
#95798=CARTESIAN_POINT('Ctrl Pts',(112.877064337466,21.2243960975892,31.));
#95799=CARTESIAN_POINT('Ctrl Pts',(112.877064337466,21.2243960975892,26.));
#95800=CARTESIAN_POINT('Ctrl Pts',(112.909015601161,21.2348979013117,31.));
#95801=CARTESIAN_POINT('Ctrl Pts',(112.909015601161,21.2348979013117,26.));
#95802=CARTESIAN_POINT('Ctrl Pts',(112.94162067641,21.2450524893146,31.));
#95803=CARTESIAN_POINT('Ctrl Pts',(112.94162067641,21.2450524893146,26.));
#95804=CARTESIAN_POINT('Ctrl Pts',(112.9748725096,21.2548581700607,31.));
#95805=CARTESIAN_POINT('Ctrl Pts',(112.9748725096,21.2548581700607,26.));
#95806=CARTESIAN_POINT('Ctrl Pts',(113.008764030125,21.2643155152947,31.));
#95807=CARTESIAN_POINT('Ctrl Pts',(113.008764030125,21.2643155152947,26.));
#95808=CARTESIAN_POINT('Ctrl Pts',(113.036384030409,21.2716041206815,31.));
#95809=CARTESIAN_POINT('Ctrl Pts',(113.036384030409,21.2716041206815,26.));
#95810=CARTESIAN_POINT('Ctrl Pts',(113.057382133554,21.2769154391419,31.));
#95811=CARTESIAN_POINT('Ctrl Pts',(113.057382133554,21.2769154391419,26.));
#95812=CARTESIAN_POINT('Ctrl Pts',(113.071506464349,21.2803874938447,31.));
#95813=CARTESIAN_POINT('Ctrl Pts',(113.071506464349,21.2803874938447,26.));
#95814=CARTESIAN_POINT('Ctrl Pts',(113.078600028632,21.2821063151136,31.));
#95815=CARTESIAN_POINT('Ctrl Pts',(113.078600028632,21.2821063151136,26.));
#95816=CARTESIAN_POINT('Ctrl Pts',(112.355644395348,20.9290433639019,31.));
#95817=CARTESIAN_POINT('Ctrl Pts',(112.357154485648,20.9308505683967,31.));
#95818=CARTESIAN_POINT('Ctrl Pts',(112.360333128385,20.9345388664441,31.));
#95819=CARTESIAN_POINT('Ctrl Pts',(112.365576482549,20.9402929843488,31.));
#95820=CARTESIAN_POINT('Ctrl Pts',(112.373520091625,20.9484092543796,31.));
#95821=CARTESIAN_POINT('Ctrl Pts',(112.385038800212,20.9592902981059,31.));
#95822=CARTESIAN_POINT('Ctrl Pts',(112.398133843138,20.9708848153277,31.));
#95823=CARTESIAN_POINT('Ctrl Pts',(112.412767081074,20.9831430242715,31.));
#95824=CARTESIAN_POINT('Ctrl Pts',(112.428859953768,20.9959735258305,31.));
#95825=CARTESIAN_POINT('Ctrl Pts',(112.446290578665,21.0092413310541,31.));
#95826=CARTESIAN_POINT('Ctrl Pts',(112.4649175332,21.0227920500277,31.));
#95827=CARTESIAN_POINT('Ctrl Pts',(112.484598627392,21.0364714002426,31.));
#95828=CARTESIAN_POINT('Ctrl Pts',(112.505209573635,21.0501445654825,31.));
#95829=CARTESIAN_POINT('Ctrl Pts',(112.526666875952,21.0637202906774,31.));
#95830=CARTESIAN_POINT('Ctrl Pts',(112.548932890716,21.0771560949637,31.));
#95831=CARTESIAN_POINT('Ctrl Pts',(112.571998699698,21.0904399794041,31.));
#95832=CARTESIAN_POINT('Ctrl Pts',(112.595872259324,21.1035779524222,31.));
#95833=CARTESIAN_POINT('Ctrl Pts',(112.620565418957,21.1165804017582,31.));
#95834=CARTESIAN_POINT('Ctrl Pts',(112.646078787711,21.1294465859895,31.));
#95835=CARTESIAN_POINT('Ctrl Pts',(112.672396876946,21.1421593242979,31.));
#95836=CARTESIAN_POINT('Ctrl Pts',(112.699495448089,21.1546918395131,31.));
#95837=CARTESIAN_POINT('Ctrl Pts',(112.727345546797,21.1670114619741,31.));
#95838=CARTESIAN_POINT('Ctrl Pts',(112.755918372182,21.1790843382401,31.));
#95839=CARTESIAN_POINT('Ctrl Pts',(112.785190336059,21.1908803623338,31.));
#95840=CARTESIAN_POINT('Ctrl Pts',(112.8151453544,21.2023758655074,31.));
#95841=CARTESIAN_POINT('Ctrl Pts',(112.845772449496,21.2135523180713,31.));
#95842=CARTESIAN_POINT('Ctrl Pts',(112.877064337466,21.2243960975892,31.));
#95843=CARTESIAN_POINT('Ctrl Pts',(112.909015601161,21.2348979013117,31.));
#95844=CARTESIAN_POINT('Ctrl Pts',(112.94162067641,21.2450524893146,31.));
#95845=CARTESIAN_POINT('Ctrl Pts',(112.9748725096,21.2548581700607,31.));
#95846=CARTESIAN_POINT('Ctrl Pts',(113.008764030125,21.2643155152947,31.));
#95847=CARTESIAN_POINT('Ctrl Pts',(113.036384030409,21.2716041206815,31.));
#95848=CARTESIAN_POINT('Ctrl Pts',(113.057382133554,21.2769154391419,31.));
#95849=CARTESIAN_POINT('Ctrl Pts',(113.071506464349,21.2803874938447,31.));
#95850=CARTESIAN_POINT('Ctrl Pts',(113.078600028632,21.2821063151136,31.));
#95851=CARTESIAN_POINT('Ctrl Pts',(112.355644395348,20.9290433639019,26.));
#95852=CARTESIAN_POINT('Ctrl Pts',(112.357154485648,20.9308505683967,26.));
#95853=CARTESIAN_POINT('Ctrl Pts',(112.360333128385,20.9345388664441,26.));
#95854=CARTESIAN_POINT('Ctrl Pts',(112.365576482549,20.9402929843488,26.));
#95855=CARTESIAN_POINT('Ctrl Pts',(112.373520091625,20.9484092543796,26.));
#95856=CARTESIAN_POINT('Ctrl Pts',(112.385038800212,20.9592902981059,26.));
#95857=CARTESIAN_POINT('Ctrl Pts',(112.398133843138,20.9708848153277,26.));
#95858=CARTESIAN_POINT('Ctrl Pts',(112.412767081074,20.9831430242715,26.));
#95859=CARTESIAN_POINT('Ctrl Pts',(112.428859953768,20.9959735258305,26.));
#95860=CARTESIAN_POINT('Ctrl Pts',(112.446290578665,21.0092413310541,26.));
#95861=CARTESIAN_POINT('Ctrl Pts',(112.4649175332,21.0227920500277,26.));
#95862=CARTESIAN_POINT('Ctrl Pts',(112.484598627392,21.0364714002426,26.));
#95863=CARTESIAN_POINT('Ctrl Pts',(112.505209573635,21.0501445654825,26.));
#95864=CARTESIAN_POINT('Ctrl Pts',(112.526666875952,21.0637202906774,26.));
#95865=CARTESIAN_POINT('Ctrl Pts',(112.548932890716,21.0771560949637,26.));
#95866=CARTESIAN_POINT('Ctrl Pts',(112.571998699698,21.0904399794041,26.));
#95867=CARTESIAN_POINT('Ctrl Pts',(112.595872259324,21.1035779524222,26.));
#95868=CARTESIAN_POINT('Ctrl Pts',(112.620565418957,21.1165804017582,26.));
#95869=CARTESIAN_POINT('Ctrl Pts',(112.646078787711,21.1294465859895,26.));
#95870=CARTESIAN_POINT('Ctrl Pts',(112.672396876946,21.1421593242979,26.));
#95871=CARTESIAN_POINT('Ctrl Pts',(112.699495448089,21.1546918395131,26.));
#95872=CARTESIAN_POINT('Ctrl Pts',(112.727345546797,21.1670114619741,26.));
#95873=CARTESIAN_POINT('Ctrl Pts',(112.755918372182,21.1790843382401,26.));
#95874=CARTESIAN_POINT('Ctrl Pts',(112.785190336059,21.1908803623338,26.));
#95875=CARTESIAN_POINT('Ctrl Pts',(112.8151453544,21.2023758655074,26.));
#95876=CARTESIAN_POINT('Ctrl Pts',(112.845772449496,21.2135523180713,26.));
#95877=CARTESIAN_POINT('Ctrl Pts',(112.877064337466,21.2243960975892,26.));
#95878=CARTESIAN_POINT('Ctrl Pts',(112.909015601161,21.2348979013117,26.));
#95879=CARTESIAN_POINT('Ctrl Pts',(112.94162067641,21.2450524893146,26.));
#95880=CARTESIAN_POINT('Ctrl Pts',(112.9748725096,21.2548581700607,26.));
#95881=CARTESIAN_POINT('Ctrl Pts',(113.008764030125,21.2643155152947,26.));
#95882=CARTESIAN_POINT('Ctrl Pts',(113.036384030409,21.2716041206815,26.));
#95883=CARTESIAN_POINT('Ctrl Pts',(113.057382133554,21.2769154391419,26.));
#95884=CARTESIAN_POINT('Ctrl Pts',(113.071506464349,21.2803874938447,26.));
#95885=CARTESIAN_POINT('Ctrl Pts',(113.078600028632,21.2821063151136,26.));
#95886=CARTESIAN_POINT('Origin',(112.724546968557,20.7245469685797,31.));
#95887=CARTESIAN_POINT('Origin',(112.828999637636,19.548349459992,31.));
#95888=CARTESIAN_POINT('',(113.297228010781,19.8046171311037,31.));
#95889=CARTESIAN_POINT('',(113.297228010781,19.8046171311037,31.));
#95890=CARTESIAN_POINT('',(113.297228010781,19.8046171311037,26.));
#95891=CARTESIAN_POINT('',(113.297228010781,19.8046171311037,31.));
#95892=CARTESIAN_POINT('',(113.297228010781,19.8046171311037,26.));
#95893=CARTESIAN_POINT('Origin',(113.60754929639,19.0554352746927,31.));
#95894=CARTESIAN_POINT('',(113.60754929639,19.0554352746927,26.));
#95895=CARTESIAN_POINT('',(113.095253230553,18.9055564249396,26.));
#95896=CARTESIAN_POINT('',(113.60754929639,19.0554352746927,31.));
#95897=CARTESIAN_POINT('',(113.60754929639,19.0554352746927,31.));
#95898=CARTESIAN_POINT('',(113.095253230553,18.9055564249396,31.));
#95899=CARTESIAN_POINT('Ctrl Pts',(114.210400073896,19.5882478451867,31.));
#95900=CARTESIAN_POINT('Ctrl Pts',(114.210400073896,19.5882478451867,26.));
#95901=CARTESIAN_POINT('Ctrl Pts',(114.206097500599,19.5823520107063,31.));
#95902=CARTESIAN_POINT('Ctrl Pts',(114.206097500599,19.5823520107063,26.));
#95903=CARTESIAN_POINT('Ctrl Pts',(114.19748459297,19.5706315282987,31.));
#95904=CARTESIAN_POINT('Ctrl Pts',(114.19748459297,19.5706315282987,26.));
#95905=CARTESIAN_POINT('Ctrl Pts',(114.184541948405,19.5532643640729,31.));
#95906=CARTESIAN_POINT('Ctrl Pts',(114.184541948405,19.5532643640729,26.));
#95907=CARTESIAN_POINT('Ctrl Pts',(114.167238438573,19.5305360396115,31.));
#95908=CARTESIAN_POINT('Ctrl Pts',(114.167238438573,19.5305360396115,26.));
#95909=CARTESIAN_POINT('Ctrl Pts',(114.145531267457,19.5028435268547,31.));
#95910=CARTESIAN_POINT('Ctrl Pts',(114.145531267457,19.5028435268547,26.));
#95911=CARTESIAN_POINT('Ctrl Pts',(114.123747074016,19.4758753104142,31.));
#95912=CARTESIAN_POINT('Ctrl Pts',(114.123747074016,19.4758753104142,26.));
#95913=CARTESIAN_POINT('Ctrl Pts',(114.101888035847,19.4496381414305,31.));
#95914=CARTESIAN_POINT('Ctrl Pts',(114.101888035847,19.4496381414305,26.));
#95915=CARTESIAN_POINT('Ctrl Pts',(114.079958415043,19.4241378892353,31.));
#95916=CARTESIAN_POINT('Ctrl Pts',(114.079958415043,19.4241378892353,26.));
#95917=CARTESIAN_POINT('Ctrl Pts',(114.057965181984,19.3993776892053,31.));
#95918=CARTESIAN_POINT('Ctrl Pts',(114.057965181984,19.3993776892053,26.));
#95919=CARTESIAN_POINT('Ctrl Pts',(114.035919004342,19.3753589861281,31.));
#95920=CARTESIAN_POINT('Ctrl Pts',(114.035919004342,19.3753589861281,26.));
#95921=CARTESIAN_POINT('Ctrl Pts',(114.013835255023,19.3520832963642,31.));
#95922=CARTESIAN_POINT('Ctrl Pts',(114.013835255023,19.3520832963642,26.));
#95923=CARTESIAN_POINT('Ctrl Pts',(113.991735254207,19.3295536710079,31.));
#95924=CARTESIAN_POINT('Ctrl Pts',(113.991735254207,19.3295536710079,26.));
#95925=CARTESIAN_POINT('Ctrl Pts',(113.96964702405,19.3077759121412,31.));
#95926=CARTESIAN_POINT('Ctrl Pts',(113.96964702405,19.3077759121412,26.));
#95927=CARTESIAN_POINT('Ctrl Pts',(113.947607405652,19.2867602913563,31.));
#95928=CARTESIAN_POINT('Ctrl Pts',(113.947607405652,19.2867602913563,26.));
#95929=CARTESIAN_POINT('Ctrl Pts',(113.925658697137,19.266520462056,31.));
#95930=CARTESIAN_POINT('Ctrl Pts',(113.925658697137,19.266520462056,26.));
#95931=CARTESIAN_POINT('Ctrl Pts',(113.903842161685,19.2470706724204,31.));
#95932=CARTESIAN_POINT('Ctrl Pts',(113.903842161685,19.2470706724204,26.));
#95933=CARTESIAN_POINT('Ctrl Pts',(113.882191813877,19.2284230687867,31.));
#95934=CARTESIAN_POINT('Ctrl Pts',(113.882191813877,19.2284230687867,26.));
#95935=CARTESIAN_POINT('Ctrl Pts',(113.860729453971,19.2105853859678,31.));
#95936=CARTESIAN_POINT('Ctrl Pts',(113.860729453971,19.2105853859678,26.));
#95937=CARTESIAN_POINT('Ctrl Pts',(113.839455533856,19.1935567774815,31.));
#95938=CARTESIAN_POINT('Ctrl Pts',(113.839455533856,19.1935567774815,26.));
#95939=CARTESIAN_POINT('Ctrl Pts',(113.818355921957,19.1773302711575,31.));
#95940=CARTESIAN_POINT('Ctrl Pts',(113.818355921957,19.1773302711575,26.));
#95941=CARTESIAN_POINT('Ctrl Pts',(113.797422022421,19.1619008155406,31.));
#95942=CARTESIAN_POINT('Ctrl Pts',(113.797422022421,19.1619008155406,26.));
#95943=CARTESIAN_POINT('Ctrl Pts',(113.77666833368,19.1472720582102,31.));
#95944=CARTESIAN_POINT('Ctrl Pts',(113.77666833368,19.1472720582102,26.));
#95945=CARTESIAN_POINT('Ctrl Pts',(113.756148508523,19.133462520623,31.));
#95946=CARTESIAN_POINT('Ctrl Pts',(113.756148508523,19.133462520623,26.));
#95947=CARTESIAN_POINT('Ctrl Pts',(113.735978808168,19.1205144212031,31.));
#95948=CARTESIAN_POINT('Ctrl Pts',(113.735978808168,19.1205144212031,26.));
#95949=CARTESIAN_POINT('Ctrl Pts',(113.716331349364,19.1084909947982,31.));
#95950=CARTESIAN_POINT('Ctrl Pts',(113.716331349364,19.1084909947982,26.));
#95951=CARTESIAN_POINT('Ctrl Pts',(113.697403084311,19.0974645664646,31.));
#95952=CARTESIAN_POINT('Ctrl Pts',(113.697403084311,19.0974645664646,26.));
#95953=CARTESIAN_POINT('Ctrl Pts',(113.679390770764,19.087506711152,31.));
#95954=CARTESIAN_POINT('Ctrl Pts',(113.679390770764,19.087506711152,26.));
#95955=CARTESIAN_POINT('Ctrl Pts',(113.662465764688,19.0786783756173,31.));
#95956=CARTESIAN_POINT('Ctrl Pts',(113.662465764688,19.0786783756173,26.));
#95957=CARTESIAN_POINT('Ctrl Pts',(113.646742571557,19.0710171631404,31.));
#95958=CARTESIAN_POINT('Ctrl Pts',(113.646742571557,19.0710171631404,26.));
#95959=CARTESIAN_POINT('Ctrl Pts',(113.632281779025,19.0645392592025,31.));
#95960=CARTESIAN_POINT('Ctrl Pts',(113.632281779025,19.0645392592025,26.));
#95961=CARTESIAN_POINT('Ctrl Pts',(113.621743435679,19.0603062834318,31.));
#95962=CARTESIAN_POINT('Ctrl Pts',(113.621743435679,19.0603062834318,26.));
#95963=CARTESIAN_POINT('Ctrl Pts',(113.614420779155,19.0576640614188,31.));
#95964=CARTESIAN_POINT('Ctrl Pts',(113.614420779155,19.0576640614188,26.));
#95965=CARTESIAN_POINT('Ctrl Pts',(113.609796822171,19.0561388289994,31.));
#95966=CARTESIAN_POINT('Ctrl Pts',(113.609796822171,19.0561388289994,26.));
#95967=CARTESIAN_POINT('Ctrl Pts',(113.60754929639,19.0554352746927,31.));
#95968=CARTESIAN_POINT('Ctrl Pts',(113.60754929639,19.0554352746927,26.));
#95969=CARTESIAN_POINT('',(114.210400073896,19.5882478451867,31.));
#95970=CARTESIAN_POINT('Ctrl Pts',(113.60754929639,19.0554352746927,31.));
#95971=CARTESIAN_POINT('Ctrl Pts',(113.609796822171,19.0561388289994,31.));
#95972=CARTESIAN_POINT('Ctrl Pts',(113.614420779155,19.0576640614188,31.));
#95973=CARTESIAN_POINT('Ctrl Pts',(113.621743435679,19.0603062834318,31.));
#95974=CARTESIAN_POINT('Ctrl Pts',(113.632281779025,19.0645392592025,31.));
#95975=CARTESIAN_POINT('Ctrl Pts',(113.646742571557,19.0710171631404,31.));
#95976=CARTESIAN_POINT('Ctrl Pts',(113.662465764688,19.0786783756173,31.));
#95977=CARTESIAN_POINT('Ctrl Pts',(113.679390770764,19.087506711152,31.));
#95978=CARTESIAN_POINT('Ctrl Pts',(113.697403084311,19.0974645664646,31.));
#95979=CARTESIAN_POINT('Ctrl Pts',(113.716331349364,19.1084909947982,31.));
#95980=CARTESIAN_POINT('Ctrl Pts',(113.735978808168,19.1205144212031,31.));
#95981=CARTESIAN_POINT('Ctrl Pts',(113.756148508523,19.133462520623,31.));
#95982=CARTESIAN_POINT('Ctrl Pts',(113.77666833368,19.1472720582102,31.));
#95983=CARTESIAN_POINT('Ctrl Pts',(113.797422022421,19.1619008155406,31.));
#95984=CARTESIAN_POINT('Ctrl Pts',(113.818355921957,19.1773302711575,31.));
#95985=CARTESIAN_POINT('Ctrl Pts',(113.839455533856,19.1935567774815,31.));
#95986=CARTESIAN_POINT('Ctrl Pts',(113.860729453971,19.2105853859678,31.));
#95987=CARTESIAN_POINT('Ctrl Pts',(113.882191813877,19.2284230687867,31.));
#95988=CARTESIAN_POINT('Ctrl Pts',(113.903842161685,19.2470706724204,31.));
#95989=CARTESIAN_POINT('Ctrl Pts',(113.925658697137,19.266520462056,31.));
#95990=CARTESIAN_POINT('Ctrl Pts',(113.947607405652,19.2867602913563,31.));
#95991=CARTESIAN_POINT('Ctrl Pts',(113.96964702405,19.3077759121412,31.));
#95992=CARTESIAN_POINT('Ctrl Pts',(113.991735254207,19.3295536710079,31.));
#95993=CARTESIAN_POINT('Ctrl Pts',(114.013835255023,19.3520832963642,31.));
#95994=CARTESIAN_POINT('Ctrl Pts',(114.035919004342,19.3753589861281,31.));
#95995=CARTESIAN_POINT('Ctrl Pts',(114.057965181984,19.3993776892053,31.));
#95996=CARTESIAN_POINT('Ctrl Pts',(114.079958415043,19.4241378892353,31.));
#95997=CARTESIAN_POINT('Ctrl Pts',(114.101888035847,19.4496381414305,31.));
#95998=CARTESIAN_POINT('Ctrl Pts',(114.123747074016,19.4758753104142,31.));
#95999=CARTESIAN_POINT('Ctrl Pts',(114.145531267457,19.5028435268547,31.));
#96000=CARTESIAN_POINT('Ctrl Pts',(114.167238438573,19.5305360396115,31.));
#96001=CARTESIAN_POINT('Ctrl Pts',(114.184541948405,19.5532643640729,31.));
#96002=CARTESIAN_POINT('Ctrl Pts',(114.19748459297,19.5706315282987,31.));
#96003=CARTESIAN_POINT('Ctrl Pts',(114.206097500599,19.5823520107063,31.));
#96004=CARTESIAN_POINT('Ctrl Pts',(114.210400073896,19.5882478451867,31.));
#96005=CARTESIAN_POINT('',(114.210400073896,19.5882478451867,26.));
#96006=CARTESIAN_POINT('Ctrl Pts',(114.210400073896,19.5882478451867,26.));
#96007=CARTESIAN_POINT('Ctrl Pts',(114.206097500599,19.5823520107063,26.));
#96008=CARTESIAN_POINT('Ctrl Pts',(114.19748459297,19.5706315282987,26.));
#96009=CARTESIAN_POINT('Ctrl Pts',(114.184541948405,19.5532643640729,26.));
#96010=CARTESIAN_POINT('Ctrl Pts',(114.167238438573,19.5305360396115,26.));
#96011=CARTESIAN_POINT('Ctrl Pts',(114.145531267457,19.5028435268547,26.));
#96012=CARTESIAN_POINT('Ctrl Pts',(114.123747074016,19.4758753104142,26.));
#96013=CARTESIAN_POINT('Ctrl Pts',(114.101888035847,19.4496381414305,26.));
#96014=CARTESIAN_POINT('Ctrl Pts',(114.079958415043,19.4241378892353,26.));
#96015=CARTESIAN_POINT('Ctrl Pts',(114.057965181984,19.3993776892053,26.));
#96016=CARTESIAN_POINT('Ctrl Pts',(114.035919004342,19.3753589861281,26.));
#96017=CARTESIAN_POINT('Ctrl Pts',(114.013835255023,19.3520832963642,26.));
#96018=CARTESIAN_POINT('Ctrl Pts',(113.991735254207,19.3295536710079,26.));
#96019=CARTESIAN_POINT('Ctrl Pts',(113.96964702405,19.3077759121412,26.));
#96020=CARTESIAN_POINT('Ctrl Pts',(113.947607405652,19.2867602913563,26.));
#96021=CARTESIAN_POINT('Ctrl Pts',(113.925658697137,19.266520462056,26.));
#96022=CARTESIAN_POINT('Ctrl Pts',(113.903842161685,19.2470706724204,26.));
#96023=CARTESIAN_POINT('Ctrl Pts',(113.882191813877,19.2284230687867,26.));
#96024=CARTESIAN_POINT('Ctrl Pts',(113.860729453971,19.2105853859678,26.));
#96025=CARTESIAN_POINT('Ctrl Pts',(113.839455533856,19.1935567774815,26.));
#96026=CARTESIAN_POINT('Ctrl Pts',(113.818355921957,19.1773302711575,26.));
#96027=CARTESIAN_POINT('Ctrl Pts',(113.797422022421,19.1619008155406,26.));
#96028=CARTESIAN_POINT('Ctrl Pts',(113.77666833368,19.1472720582102,26.));
#96029=CARTESIAN_POINT('Ctrl Pts',(113.756148508523,19.133462520623,26.));
#96030=CARTESIAN_POINT('Ctrl Pts',(113.735978808168,19.1205144212031,26.));
#96031=CARTESIAN_POINT('Ctrl Pts',(113.716331349364,19.1084909947982,26.));
#96032=CARTESIAN_POINT('Ctrl Pts',(113.697403084311,19.0974645664646,26.));
#96033=CARTESIAN_POINT('Ctrl Pts',(113.679390770764,19.087506711152,26.));
#96034=CARTESIAN_POINT('Ctrl Pts',(113.662465764688,19.0786783756173,26.));
#96035=CARTESIAN_POINT('Ctrl Pts',(113.646742571557,19.0710171631404,26.));
#96036=CARTESIAN_POINT('Ctrl Pts',(113.632281779025,19.0645392592025,26.));
#96037=CARTESIAN_POINT('Ctrl Pts',(113.621743435679,19.0603062834318,26.));
#96038=CARTESIAN_POINT('Ctrl Pts',(113.614420779155,19.0576640614188,26.));
#96039=CARTESIAN_POINT('Ctrl Pts',(113.609796822171,19.0561388289994,26.));
#96040=CARTESIAN_POINT('Ctrl Pts',(113.60754929639,19.0554352746927,26.));
#96041=CARTESIAN_POINT('',(114.210400073896,19.5882478451867,31.));
#96042=CARTESIAN_POINT('Origin',(109.999999999997,17.9999999999988,31.));
#96043=CARTESIAN_POINT('',(114.100263265296,19.8541416222235,31.));
#96044=CARTESIAN_POINT('Origin',(109.999999999997,17.9999999999988,31.));
#96045=CARTESIAN_POINT('',(114.100263265296,19.8541416222235,26.));
#96046=CARTESIAN_POINT('Origin',(109.999999999997,17.9999999999988,26.));
#96047=CARTESIAN_POINT('',(114.100263265296,19.8541416222235,31.));
#96048=CARTESIAN_POINT('Ctrl Pts',(113.297228010781,19.8046171311037,31.));
#96049=CARTESIAN_POINT('Ctrl Pts',(113.297228010781,19.8046171311037,26.));
#96050=CARTESIAN_POINT('Ctrl Pts',(113.29931473952,19.8057088838085,31.));
#96051=CARTESIAN_POINT('Ctrl Pts',(113.29931473952,19.8057088838085,26.));
#96052=CARTESIAN_POINT('Ctrl Pts',(113.303662873043,19.8079000129713,31.));
#96053=CARTESIAN_POINT('Ctrl Pts',(113.303662873043,19.8079000129713,26.));
#96054=CARTESIAN_POINT('Ctrl Pts',(113.310709106226,19.8112095799625,31.));
#96055=CARTESIAN_POINT('Ctrl Pts',(113.310709106226,19.8112095799625,26.));
#96056=CARTESIAN_POINT('Ctrl Pts',(113.321154006139,19.8156681481377,31.));
#96057=CARTESIAN_POINT('Ctrl Pts',(113.321154006139,19.8156681481377,26.));
#96058=CARTESIAN_POINT('Ctrl Pts',(113.335959900405,19.8213129027904,31.));
#96059=CARTESIAN_POINT('Ctrl Pts',(113.335959900405,19.8213129027904,26.));
#96060=CARTESIAN_POINT('Ctrl Pts',(113.352495172189,19.8270135839669,31.));
#96061=CARTESIAN_POINT('Ctrl Pts',(113.352495172189,19.8270135839669,26.));
#96062=CARTESIAN_POINT('Ctrl Pts',(113.370705534686,19.8327387945953,31.));
#96063=CARTESIAN_POINT('Ctrl Pts',(113.370705534686,19.8327387945953,26.));
#96064=CARTESIAN_POINT('Ctrl Pts',(113.390483430762,19.8384341566185,31.));
#96065=CARTESIAN_POINT('Ctrl Pts',(113.390483430762,19.8384341566185,26.));
#96066=CARTESIAN_POINT('Ctrl Pts',(113.411664597586,19.8440215989421,31.));
#96067=CARTESIAN_POINT('Ctrl Pts',(113.411664597586,19.8440215989421,26.));
#96068=CARTESIAN_POINT('Ctrl Pts',(113.434059295282,19.8494126039565,31.));
#96069=CARTESIAN_POINT('Ctrl Pts',(113.434059295282,19.8494126039565,26.));
#96070=CARTESIAN_POINT('Ctrl Pts',(113.457477116077,19.8545190469599,31.));
#96071=CARTESIAN_POINT('Ctrl Pts',(113.457477116077,19.8545190469599,26.));
#96072=CARTESIAN_POINT('Ctrl Pts',(113.481751641261,19.8592639368172,31.));
#96073=CARTESIAN_POINT('Ctrl Pts',(113.481751641261,19.8592639368172,26.));
#96074=CARTESIAN_POINT('Ctrl Pts',(113.506770808809,19.863594917364,31.));
#96075=CARTESIAN_POINT('Ctrl Pts',(113.506770808809,19.863594917364,26.));
#96076=CARTESIAN_POINT('Ctrl Pts',(113.532483583821,19.8674871469917,31.));
#96077=CARTESIAN_POINT('Ctrl Pts',(113.532483583821,19.8674871469917,26.));
#96078=CARTESIAN_POINT('Ctrl Pts',(113.558877135133,19.8709329529872,31.));
#96079=CARTESIAN_POINT('Ctrl Pts',(113.558877135133,19.8709329529872,26.));
#96080=CARTESIAN_POINT('Ctrl Pts',(113.585961112848,19.8739348416169,31.));
#96081=CARTESIAN_POINT('Ctrl Pts',(113.585961112848,19.8739348416169,26.));
#96082=CARTESIAN_POINT('Ctrl Pts',(113.613750439568,19.8764978753463,31.));
#96083=CARTESIAN_POINT('Ctrl Pts',(113.613750439568,19.8764978753463,26.));
#96084=CARTESIAN_POINT('Ctrl Pts',(113.642245394308,19.8786211360933,31.));
#96085=CARTESIAN_POINT('Ctrl Pts',(113.642245394308,19.8786211360933,26.));
#96086=CARTESIAN_POINT('Ctrl Pts',(113.671425092618,19.8802946780967,31.));
#96087=CARTESIAN_POINT('Ctrl Pts',(113.671425092618,19.8802946780967,26.));
#96088=CARTESIAN_POINT('Ctrl Pts',(113.701256893795,19.8815030381781,31.));
#96089=CARTESIAN_POINT('Ctrl Pts',(113.701256893795,19.8815030381781,26.));
#96090=CARTESIAN_POINT('Ctrl Pts',(113.73170154538,19.8822271138526,31.));
#96091=CARTESIAN_POINT('Ctrl Pts',(113.73170154538,19.8822271138526,26.));
#96092=CARTESIAN_POINT('Ctrl Pts',(113.762719483667,19.8824466502425,31.));
#96093=CARTESIAN_POINT('Ctrl Pts',(113.762719483667,19.8824466502425,26.));
#96094=CARTESIAN_POINT('Ctrl Pts',(113.794277394957,19.8821428598593,31.));
#96095=CARTESIAN_POINT('Ctrl Pts',(113.794277394957,19.8821428598593,26.));
#96096=CARTESIAN_POINT('Ctrl Pts',(113.82635136191,19.8813000307218,31.));
#96097=CARTESIAN_POINT('Ctrl Pts',(113.82635136191,19.8813000307218,26.));
#96098=CARTESIAN_POINT('Ctrl Pts',(113.858924151438,19.8799052446171,31.));
#96099=CARTESIAN_POINT('Ctrl Pts',(113.858924151438,19.8799052446171,26.));
#96100=CARTESIAN_POINT('Ctrl Pts',(113.891983821033,19.8779487034752,31.));
#96101=CARTESIAN_POINT('Ctrl Pts',(113.891983821033,19.8779487034752,26.));
#96102=CARTESIAN_POINT('Ctrl Pts',(113.925521805893,19.8754238857298,31.));
#96103=CARTESIAN_POINT('Ctrl Pts',(113.925521805893,19.8754238857298,26.));
#96104=CARTESIAN_POINT('Ctrl Pts',(113.959530960163,19.8723280796379,31.));
#96105=CARTESIAN_POINT('Ctrl Pts',(113.959530960163,19.8723280796379,26.));
#96106=CARTESIAN_POINT('Ctrl Pts',(113.99400411983,19.868662421724,31.));
#96107=CARTESIAN_POINT('Ctrl Pts',(113.99400411983,19.868662421724,26.));
#96108=CARTESIAN_POINT('Ctrl Pts',(114.028934971304,19.8644301460149,31.));
#96109=CARTESIAN_POINT('Ctrl Pts',(114.028934971304,19.8644301460149,26.));
#96110=CARTESIAN_POINT('Ctrl Pts',(114.057241752781,19.8605942228417,31.));
#96111=CARTESIAN_POINT('Ctrl Pts',(114.057241752781,19.8605942228417,26.));
#96112=CARTESIAN_POINT('Ctrl Pts',(114.078674024077,19.8574656150733,31.));
#96113=CARTESIAN_POINT('Ctrl Pts',(114.078674024077,19.8574656150733,26.));
#96114=CARTESIAN_POINT('Ctrl Pts',(114.09305190202,19.8552682279604,31.));
#96115=CARTESIAN_POINT('Ctrl Pts',(114.09305190202,19.8552682279604,26.));
#96116=CARTESIAN_POINT('Ctrl Pts',(114.100263265296,19.8541416222235,31.));
#96117=CARTESIAN_POINT('Ctrl Pts',(114.100263265296,19.8541416222235,26.));
#96118=CARTESIAN_POINT('Ctrl Pts',(113.297228010781,19.8046171311037,31.));
#96119=CARTESIAN_POINT('Ctrl Pts',(113.29931473952,19.8057088838085,31.));
#96120=CARTESIAN_POINT('Ctrl Pts',(113.303662873043,19.8079000129713,31.));
#96121=CARTESIAN_POINT('Ctrl Pts',(113.310709106226,19.8112095799625,31.));
#96122=CARTESIAN_POINT('Ctrl Pts',(113.321154006139,19.8156681481377,31.));
#96123=CARTESIAN_POINT('Ctrl Pts',(113.335959900405,19.8213129027904,31.));
#96124=CARTESIAN_POINT('Ctrl Pts',(113.352495172189,19.8270135839669,31.));
#96125=CARTESIAN_POINT('Ctrl Pts',(113.370705534686,19.8327387945953,31.));
#96126=CARTESIAN_POINT('Ctrl Pts',(113.390483430762,19.8384341566185,31.));
#96127=CARTESIAN_POINT('Ctrl Pts',(113.411664597586,19.8440215989421,31.));
#96128=CARTESIAN_POINT('Ctrl Pts',(113.434059295282,19.8494126039565,31.));
#96129=CARTESIAN_POINT('Ctrl Pts',(113.457477116077,19.8545190469599,31.));
#96130=CARTESIAN_POINT('Ctrl Pts',(113.481751641261,19.8592639368172,31.));
#96131=CARTESIAN_POINT('Ctrl Pts',(113.506770808809,19.863594917364,31.));
#96132=CARTESIAN_POINT('Ctrl Pts',(113.532483583821,19.8674871469917,31.));
#96133=CARTESIAN_POINT('Ctrl Pts',(113.558877135133,19.8709329529872,31.));
#96134=CARTESIAN_POINT('Ctrl Pts',(113.585961112848,19.8739348416169,31.));
#96135=CARTESIAN_POINT('Ctrl Pts',(113.613750439568,19.8764978753463,31.));
#96136=CARTESIAN_POINT('Ctrl Pts',(113.642245394308,19.8786211360933,31.));
#96137=CARTESIAN_POINT('Ctrl Pts',(113.671425092618,19.8802946780967,31.));
#96138=CARTESIAN_POINT('Ctrl Pts',(113.701256893795,19.8815030381781,31.));
#96139=CARTESIAN_POINT('Ctrl Pts',(113.73170154538,19.8822271138526,31.));
#96140=CARTESIAN_POINT('Ctrl Pts',(113.762719483667,19.8824466502425,31.));
#96141=CARTESIAN_POINT('Ctrl Pts',(113.794277394957,19.8821428598593,31.));
#96142=CARTESIAN_POINT('Ctrl Pts',(113.82635136191,19.8813000307218,31.));
#96143=CARTESIAN_POINT('Ctrl Pts',(113.858924151438,19.8799052446171,31.));
#96144=CARTESIAN_POINT('Ctrl Pts',(113.891983821033,19.8779487034752,31.));
#96145=CARTESIAN_POINT('Ctrl Pts',(113.925521805893,19.8754238857298,31.));
#96146=CARTESIAN_POINT('Ctrl Pts',(113.959530960163,19.8723280796379,31.));
#96147=CARTESIAN_POINT('Ctrl Pts',(113.99400411983,19.868662421724,31.));
#96148=CARTESIAN_POINT('Ctrl Pts',(114.028934971304,19.8644301460149,31.));
#96149=CARTESIAN_POINT('Ctrl Pts',(114.057241752781,19.8605942228417,31.));
#96150=CARTESIAN_POINT('Ctrl Pts',(114.078674024077,19.8574656150733,31.));
#96151=CARTESIAN_POINT('Ctrl Pts',(114.09305190202,19.8552682279604,31.));
#96152=CARTESIAN_POINT('Ctrl Pts',(114.100263265296,19.8541416222235,31.));
#96153=CARTESIAN_POINT('Ctrl Pts',(113.297228010781,19.8046171311037,26.));
#96154=CARTESIAN_POINT('Ctrl Pts',(113.29931473952,19.8057088838085,26.));
#96155=CARTESIAN_POINT('Ctrl Pts',(113.303662873043,19.8079000129713,26.));
#96156=CARTESIAN_POINT('Ctrl Pts',(113.310709106226,19.8112095799625,26.));
#96157=CARTESIAN_POINT('Ctrl Pts',(113.321154006139,19.8156681481377,26.));
#96158=CARTESIAN_POINT('Ctrl Pts',(113.335959900405,19.8213129027904,26.));
#96159=CARTESIAN_POINT('Ctrl Pts',(113.352495172189,19.8270135839669,26.));
#96160=CARTESIAN_POINT('Ctrl Pts',(113.370705534686,19.8327387945953,26.));
#96161=CARTESIAN_POINT('Ctrl Pts',(113.390483430762,19.8384341566185,26.));
#96162=CARTESIAN_POINT('Ctrl Pts',(113.411664597586,19.8440215989421,26.));
#96163=CARTESIAN_POINT('Ctrl Pts',(113.434059295282,19.8494126039565,26.));
#96164=CARTESIAN_POINT('Ctrl Pts',(113.457477116077,19.8545190469599,26.));
#96165=CARTESIAN_POINT('Ctrl Pts',(113.481751641261,19.8592639368172,26.));
#96166=CARTESIAN_POINT('Ctrl Pts',(113.506770808809,19.863594917364,26.));
#96167=CARTESIAN_POINT('Ctrl Pts',(113.532483583821,19.8674871469917,26.));
#96168=CARTESIAN_POINT('Ctrl Pts',(113.558877135133,19.8709329529872,26.));
#96169=CARTESIAN_POINT('Ctrl Pts',(113.585961112848,19.8739348416169,26.));
#96170=CARTESIAN_POINT('Ctrl Pts',(113.613750439568,19.8764978753463,26.));
#96171=CARTESIAN_POINT('Ctrl Pts',(113.642245394308,19.8786211360933,26.));
#96172=CARTESIAN_POINT('Ctrl Pts',(113.671425092618,19.8802946780967,26.));
#96173=CARTESIAN_POINT('Ctrl Pts',(113.701256893795,19.8815030381781,26.));
#96174=CARTESIAN_POINT('Ctrl Pts',(113.73170154538,19.8822271138526,26.));
#96175=CARTESIAN_POINT('Ctrl Pts',(113.762719483667,19.8824466502425,26.));
#96176=CARTESIAN_POINT('Ctrl Pts',(113.794277394957,19.8821428598593,26.));
#96177=CARTESIAN_POINT('Ctrl Pts',(113.82635136191,19.8813000307218,26.));
#96178=CARTESIAN_POINT('Ctrl Pts',(113.858924151438,19.8799052446171,26.));
#96179=CARTESIAN_POINT('Ctrl Pts',(113.891983821033,19.8779487034752,26.));
#96180=CARTESIAN_POINT('Ctrl Pts',(113.925521805893,19.8754238857298,26.));
#96181=CARTESIAN_POINT('Ctrl Pts',(113.959530960163,19.8723280796379,26.));
#96182=CARTESIAN_POINT('Ctrl Pts',(113.99400411983,19.868662421724,26.));
#96183=CARTESIAN_POINT('Ctrl Pts',(114.028934971304,19.8644301460149,26.));
#96184=CARTESIAN_POINT('Ctrl Pts',(114.057241752781,19.8605942228417,26.));
#96185=CARTESIAN_POINT('Ctrl Pts',(114.078674024077,19.8574656150733,26.));
#96186=CARTESIAN_POINT('Ctrl Pts',(114.09305190202,19.8552682279604,26.));
#96187=CARTESIAN_POINT('Ctrl Pts',(114.100263265296,19.8541416222235,26.));
#96188=CARTESIAN_POINT('Origin',(113.559792165192,19.4745141940691,31.));
#96189=CARTESIAN_POINT('Origin',(113.206182548544,18.3478770837715,31.));
#96190=CARTESIAN_POINT('',(113.736838551019,18.4054542989899,31.));
#96191=CARTESIAN_POINT('',(113.736838551019,18.4054542989899,31.));
#96192=CARTESIAN_POINT('',(113.736838551019,18.4054542989899,26.));
#96193=CARTESIAN_POINT('',(113.736838551019,18.4054542989899,31.));
#96194=CARTESIAN_POINT('',(113.736838551019,18.4054542989899,26.));
#96195=CARTESIAN_POINT('Origin',(113.736838551019,17.5945457010101,31.));
#96196=CARTESIAN_POINT('',(113.736838551019,17.5945457010101,26.));
#96197=CARTESIAN_POINT('',(113.206182548544,17.6521229162285,26.));
#96198=CARTESIAN_POINT('',(113.736838551019,17.5945457010101,31.));
#96199=CARTESIAN_POINT('',(113.736838551019,17.5945457010101,31.));
#96200=CARTESIAN_POINT('',(113.206182548544,17.6521229162285,31.));
#96201=CARTESIAN_POINT('Ctrl Pts',(114.497698588799,17.8560993248145,31.));
#96202=CARTESIAN_POINT('Ctrl Pts',(114.497698588799,17.8560993248145,26.));
#96203=CARTESIAN_POINT('Ctrl Pts',(114.491467291217,17.8522988075283,31.));
#96204=CARTESIAN_POINT('Ctrl Pts',(114.491467291217,17.8522988075283,26.));
#96205=CARTESIAN_POINT('Ctrl Pts',(114.479024767707,17.8447665107748,31.));
#96206=CARTESIAN_POINT('Ctrl Pts',(114.479024767707,17.8447665107748,26.));
#96207=CARTESIAN_POINT('Ctrl Pts',(114.46042119728,17.8336742788547,31.));
#96208=CARTESIAN_POINT('Ctrl Pts',(114.46042119728,17.8336742788547,26.));
#96209=CARTESIAN_POINT('Ctrl Pts',(114.435737085489,17.8192978116112,31.));
#96210=CARTESIAN_POINT('Ctrl Pts',(114.435737085489,17.8192978116112,26.));
#96211=CARTESIAN_POINT('Ctrl Pts',(114.405084808554,17.8020202406208,31.));
#96212=CARTESIAN_POINT('Ctrl Pts',(114.405084808554,17.8020202406208,26.));
#96213=CARTESIAN_POINT('Ctrl Pts',(114.374638548468,17.7854413073407,31.));
#96214=CARTESIAN_POINT('Ctrl Pts',(114.374638548468,17.7854413073407,26.));
#96215=CARTESIAN_POINT('Ctrl Pts',(114.344402900622,17.7695664156801,31.));
#96216=CARTESIAN_POINT('Ctrl Pts',(114.344402900622,17.7695664156801,26.));
#96217=CARTESIAN_POINT('Ctrl Pts',(114.314384048769,17.7543993571629,31.));
#96218=CARTESIAN_POINT('Ctrl Pts',(114.314384048769,17.7543993571629,26.));
#96219=CARTESIAN_POINT('Ctrl Pts',(114.284589632559,17.73994036105,31.));
#96220=CARTESIAN_POINT('Ctrl Pts',(114.284589632559,17.73994036105,26.));
#96221=CARTESIAN_POINT('Ctrl Pts',(114.255030060531,17.72618667981,31.));
#96222=CARTESIAN_POINT('Ctrl Pts',(114.255030060531,17.72618667981,26.));
#96223=CARTESIAN_POINT('Ctrl Pts',(114.225720115684,17.7131338314213,31.));
#96224=CARTESIAN_POINT('Ctrl Pts',(114.225720115684,17.7131338314213,26.));
#96225=CARTESIAN_POINT('Ctrl Pts',(114.1966806629,17.7007764758468,31.));
#96226=CARTESIAN_POINT('Ctrl Pts',(114.1966806629,17.7007764758468,26.));
#96227=CARTESIAN_POINT('Ctrl Pts',(114.167939811637,17.6891092498973,31.));
#96228=CARTESIAN_POINT('Ctrl Pts',(114.167939811637,17.6891092498973,26.));
#96229=CARTESIAN_POINT('Ctrl Pts',(114.139535529399,17.6781275448076,31.));
#96230=CARTESIAN_POINT('Ctrl Pts',(114.139535529399,17.6781275448076,26.));
#96231=CARTESIAN_POINT('Ctrl Pts',(114.11151211949,17.667827787886,31.));
#96232=CARTESIAN_POINT('Ctrl Pts',(114.11151211949,17.667827787886,26.));
#96233=CARTESIAN_POINT('Ctrl Pts',(114.083913156659,17.6582073519993,31.));
#96234=CARTESIAN_POINT('Ctrl Pts',(114.083913156659,17.6582073519993,26.));
#96235=CARTESIAN_POINT('Ctrl Pts',(114.056774714484,17.6492644420825,31.));
#96236=CARTESIAN_POINT('Ctrl Pts',(114.056774714484,17.6492644420825,26.));
#96237=CARTESIAN_POINT('Ctrl Pts',(114.030119893761,17.6409978615743,31.));
#96238=CARTESIAN_POINT('Ctrl Pts',(114.030119893761,17.6409978615743,26.));
#96239=CARTESIAN_POINT('Ctrl Pts',(114.003948788046,17.6334066554963,31.));
#96240=CARTESIAN_POINT('Ctrl Pts',(114.003948788046,17.6334066554963,26.));
#96241=CARTESIAN_POINT('Ctrl Pts',(113.978245673333,17.6264897903224,31.));
#96242=CARTESIAN_POINT('Ctrl Pts',(113.978245673333,17.6264897903224,26.));
#96243=CARTESIAN_POINT('Ctrl Pts',(113.953000674982,17.6202458886071,31.));
#96244=CARTESIAN_POINT('Ctrl Pts',(113.953000674982,17.6202458886071,26.));
#96245=CARTESIAN_POINT('Ctrl Pts',(113.928228583663,17.6146727719654,31.));
#96246=CARTESIAN_POINT('Ctrl Pts',(113.928228583663,17.6146727719654,26.));
#96247=CARTESIAN_POINT('Ctrl Pts',(113.903986055947,17.6097670199576,31.));
#96248=CARTESIAN_POINT('Ctrl Pts',(113.903986055947,17.6097670199576,26.));
#96249=CARTESIAN_POINT('Ctrl Pts',(113.880396659483,17.6055231460801,31.));
#96250=CARTESIAN_POINT('Ctrl Pts',(113.880396659483,17.6055231460801,26.));
#96251=CARTESIAN_POINT('Ctrl Pts',(113.857643608343,17.6019337054866,31.));
#96252=CARTESIAN_POINT('Ctrl Pts',(113.857643608343,17.6019337054866,26.));
#96253=CARTESIAN_POINT('Ctrl Pts',(113.835936540232,17.5989901474718,31.));
#96254=CARTESIAN_POINT('Ctrl Pts',(113.835936540232,17.5989901474718,26.));
#96255=CARTESIAN_POINT('Ctrl Pts',(113.815484626163,17.5966833027337,31.));
#96256=CARTESIAN_POINT('Ctrl Pts',(113.815484626163,17.5966833027337,26.));
#96257=CARTESIAN_POINT('Ctrl Pts',(113.796469501718,17.5950039036449,31.));
#96258=CARTESIAN_POINT('Ctrl Pts',(113.796469501718,17.5950039036449,26.));
#96259=CARTESIAN_POINT('Ctrl Pts',(113.779011346312,17.5939428717583,31.));
#96260=CARTESIAN_POINT('Ctrl Pts',(113.779011346312,17.5939428717583,26.));
#96261=CARTESIAN_POINT('Ctrl Pts',(113.763172329554,17.5934919746174,31.));
#96262=CARTESIAN_POINT('Ctrl Pts',(113.763172329554,17.5934919746174,26.));
#96263=CARTESIAN_POINT('Ctrl Pts',(113.751816280133,17.5936140643445,31.));
#96264=CARTESIAN_POINT('Ctrl Pts',(113.751816280133,17.5936140643445,26.));
#96265=CARTESIAN_POINT('Ctrl Pts',(113.744039893058,17.5939752288389,31.));
#96266=CARTESIAN_POINT('Ctrl Pts',(113.744039893058,17.5939752288389,26.));
#96267=CARTESIAN_POINT('Ctrl Pts',(113.739184232663,17.5943356095541,31.));
#96268=CARTESIAN_POINT('Ctrl Pts',(113.739184232663,17.5943356095541,26.));
#96269=CARTESIAN_POINT('Ctrl Pts',(113.736838551019,17.5945457010101,31.));
#96270=CARTESIAN_POINT('Ctrl Pts',(113.736838551019,17.5945457010101,26.));
#96271=CARTESIAN_POINT('',(114.497698588799,17.8560993248145,31.));
#96272=CARTESIAN_POINT('Ctrl Pts',(113.736838551019,17.5945457010101,31.));
#96273=CARTESIAN_POINT('Ctrl Pts',(113.739184232663,17.5943356095541,31.));
#96274=CARTESIAN_POINT('Ctrl Pts',(113.744039893058,17.5939752288389,31.));
#96275=CARTESIAN_POINT('Ctrl Pts',(113.751816280133,17.5936140643445,31.));
#96276=CARTESIAN_POINT('Ctrl Pts',(113.763172329554,17.5934919746174,31.));
#96277=CARTESIAN_POINT('Ctrl Pts',(113.779011346312,17.5939428717583,31.));
#96278=CARTESIAN_POINT('Ctrl Pts',(113.796469501718,17.5950039036449,31.));
#96279=CARTESIAN_POINT('Ctrl Pts',(113.815484626163,17.5966833027337,31.));
#96280=CARTESIAN_POINT('Ctrl Pts',(113.835936540232,17.5989901474718,31.));
#96281=CARTESIAN_POINT('Ctrl Pts',(113.857643608343,17.6019337054866,31.));
#96282=CARTESIAN_POINT('Ctrl Pts',(113.880396659483,17.6055231460801,31.));
#96283=CARTESIAN_POINT('Ctrl Pts',(113.903986055947,17.6097670199576,31.));
#96284=CARTESIAN_POINT('Ctrl Pts',(113.928228583663,17.6146727719654,31.));
#96285=CARTESIAN_POINT('Ctrl Pts',(113.953000674982,17.6202458886071,31.));
#96286=CARTESIAN_POINT('Ctrl Pts',(113.978245673333,17.6264897903224,31.));
#96287=CARTESIAN_POINT('Ctrl Pts',(114.003948788046,17.6334066554963,31.));
#96288=CARTESIAN_POINT('Ctrl Pts',(114.030119893761,17.6409978615743,31.));
#96289=CARTESIAN_POINT('Ctrl Pts',(114.056774714484,17.6492644420825,31.));
#96290=CARTESIAN_POINT('Ctrl Pts',(114.083913156659,17.6582073519993,31.));
#96291=CARTESIAN_POINT('Ctrl Pts',(114.11151211949,17.667827787886,31.));
#96292=CARTESIAN_POINT('Ctrl Pts',(114.139535529399,17.6781275448076,31.));
#96293=CARTESIAN_POINT('Ctrl Pts',(114.167939811637,17.6891092498973,31.));
#96294=CARTESIAN_POINT('Ctrl Pts',(114.1966806629,17.7007764758468,31.));
#96295=CARTESIAN_POINT('Ctrl Pts',(114.225720115684,17.7131338314213,31.));
#96296=CARTESIAN_POINT('Ctrl Pts',(114.255030060531,17.72618667981,31.));
#96297=CARTESIAN_POINT('Ctrl Pts',(114.284589632559,17.73994036105,31.));
#96298=CARTESIAN_POINT('Ctrl Pts',(114.314384048769,17.7543993571629,31.));
#96299=CARTESIAN_POINT('Ctrl Pts',(114.344402900622,17.7695664156801,31.));
#96300=CARTESIAN_POINT('Ctrl Pts',(114.374638548468,17.7854413073407,31.));
#96301=CARTESIAN_POINT('Ctrl Pts',(114.405084808554,17.8020202406208,31.));
#96302=CARTESIAN_POINT('Ctrl Pts',(114.435737085489,17.8192978116112,31.));
#96303=CARTESIAN_POINT('Ctrl Pts',(114.46042119728,17.8336742788547,31.));
#96304=CARTESIAN_POINT('Ctrl Pts',(114.479024767707,17.8447665107748,31.));
#96305=CARTESIAN_POINT('Ctrl Pts',(114.491467291217,17.8522988075283,31.));
#96306=CARTESIAN_POINT('Ctrl Pts',(114.497698588799,17.8560993248145,31.));
#96307=CARTESIAN_POINT('',(114.497698588799,17.8560993248145,26.));
#96308=CARTESIAN_POINT('Ctrl Pts',(114.497698588799,17.8560993248145,26.));
#96309=CARTESIAN_POINT('Ctrl Pts',(114.491467291217,17.8522988075283,26.));
#96310=CARTESIAN_POINT('Ctrl Pts',(114.479024767707,17.8447665107748,26.));
#96311=CARTESIAN_POINT('Ctrl Pts',(114.46042119728,17.8336742788547,26.));
#96312=CARTESIAN_POINT('Ctrl Pts',(114.435737085489,17.8192978116112,26.));
#96313=CARTESIAN_POINT('Ctrl Pts',(114.405084808554,17.8020202406208,26.));
#96314=CARTESIAN_POINT('Ctrl Pts',(114.374638548468,17.7854413073407,26.));
#96315=CARTESIAN_POINT('Ctrl Pts',(114.344402900622,17.7695664156801,26.));
#96316=CARTESIAN_POINT('Ctrl Pts',(114.314384048769,17.7543993571629,26.));
#96317=CARTESIAN_POINT('Ctrl Pts',(114.284589632559,17.73994036105,26.));
#96318=CARTESIAN_POINT('Ctrl Pts',(114.255030060531,17.72618667981,26.));
#96319=CARTESIAN_POINT('Ctrl Pts',(114.225720115684,17.7131338314213,26.));
#96320=CARTESIAN_POINT('Ctrl Pts',(114.1966806629,17.7007764758468,26.));
#96321=CARTESIAN_POINT('Ctrl Pts',(114.167939811637,17.6891092498973,26.));
#96322=CARTESIAN_POINT('Ctrl Pts',(114.139535529399,17.6781275448076,26.));
#96323=CARTESIAN_POINT('Ctrl Pts',(114.11151211949,17.667827787886,26.));
#96324=CARTESIAN_POINT('Ctrl Pts',(114.083913156659,17.6582073519993,26.));
#96325=CARTESIAN_POINT('Ctrl Pts',(114.056774714484,17.6492644420825,26.));
#96326=CARTESIAN_POINT('Ctrl Pts',(114.030119893761,17.6409978615743,26.));
#96327=CARTESIAN_POINT('Ctrl Pts',(114.003948788046,17.6334066554963,26.));
#96328=CARTESIAN_POINT('Ctrl Pts',(113.978245673333,17.6264897903224,26.));
#96329=CARTESIAN_POINT('Ctrl Pts',(113.953000674982,17.6202458886071,26.));
#96330=CARTESIAN_POINT('Ctrl Pts',(113.928228583663,17.6146727719654,26.));
#96331=CARTESIAN_POINT('Ctrl Pts',(113.903986055947,17.6097670199576,26.));
#96332=CARTESIAN_POINT('Ctrl Pts',(113.880396659483,17.6055231460801,26.));
#96333=CARTESIAN_POINT('Ctrl Pts',(113.857643608343,17.6019337054866,26.));
#96334=CARTESIAN_POINT('Ctrl Pts',(113.835936540232,17.5989901474718,26.));
#96335=CARTESIAN_POINT('Ctrl Pts',(113.815484626163,17.5966833027337,26.));
#96336=CARTESIAN_POINT('Ctrl Pts',(113.796469501718,17.5950039036449,26.));
#96337=CARTESIAN_POINT('Ctrl Pts',(113.779011346312,17.5939428717583,26.));
#96338=CARTESIAN_POINT('Ctrl Pts',(113.763172329554,17.5934919746174,26.));
#96339=CARTESIAN_POINT('Ctrl Pts',(113.751816280133,17.5936140643445,26.));
#96340=CARTESIAN_POINT('Ctrl Pts',(113.744039893058,17.5939752288389,26.));
#96341=CARTESIAN_POINT('Ctrl Pts',(113.739184232663,17.5943356095541,26.));
#96342=CARTESIAN_POINT('Ctrl Pts',(113.736838551019,17.5945457010101,26.));
#96343=CARTESIAN_POINT('',(114.497698588799,17.8560993248145,31.));
#96344=CARTESIAN_POINT('Origin',(109.999999999997,18.,31.));
#96345=CARTESIAN_POINT('',(114.497698588799,18.1439006751855,31.));
#96346=CARTESIAN_POINT('Origin',(109.999999999997,18.,31.));
#96347=CARTESIAN_POINT('',(114.497698588799,18.1439006751855,26.));
#96348=CARTESIAN_POINT('Origin',(109.999999999997,18.,26.));
#96349=CARTESIAN_POINT('',(114.497698588799,18.1439006751855,31.));
#96350=CARTESIAN_POINT('Ctrl Pts',(113.736838551019,18.4054542989899,31.));
#96351=CARTESIAN_POINT('Ctrl Pts',(113.736838551019,18.4054542989899,26.));
#96352=CARTESIAN_POINT('Ctrl Pts',(113.739184232663,18.4056643904521,31.));
#96353=CARTESIAN_POINT('Ctrl Pts',(113.739184232663,18.4056643904521,26.));
#96354=CARTESIAN_POINT('Ctrl Pts',(113.744039893058,18.406024771178,31.));
#96355=CARTESIAN_POINT('Ctrl Pts',(113.744039893058,18.406024771178,26.));
#96356=CARTESIAN_POINT('Ctrl Pts',(113.751816280134,18.4063859356827,31.));
#96357=CARTESIAN_POINT('Ctrl Pts',(113.751816280134,18.4063859356827,26.));
#96358=CARTESIAN_POINT('Ctrl Pts',(113.763172329555,18.4065080254146,31.));
#96359=CARTESIAN_POINT('Ctrl Pts',(113.763172329555,18.4065080254146,26.));
#96360=CARTESIAN_POINT('Ctrl Pts',(113.779011346313,18.4060571282676,31.));
#96361=CARTESIAN_POINT('Ctrl Pts',(113.779011346313,18.4060571282676,26.));
#96362=CARTESIAN_POINT('Ctrl Pts',(113.796469501718,18.4049960963666,31.));
#96363=CARTESIAN_POINT('Ctrl Pts',(113.796469501718,18.4049960963666,26.));
#96364=CARTESIAN_POINT('Ctrl Pts',(113.815484626163,18.4033166972605,31.));
#96365=CARTESIAN_POINT('Ctrl Pts',(113.815484626163,18.4033166972605,26.));
#96366=CARTESIAN_POINT('Ctrl Pts',(113.835936540232,18.4010098525085,31.));
#96367=CARTESIAN_POINT('Ctrl Pts',(113.835936540232,18.4010098525085,26.));
#96368=CARTESIAN_POINT('Ctrl Pts',(113.857643608342,18.3980662944885,31.));
#96369=CARTESIAN_POINT('Ctrl Pts',(113.857643608342,18.3980662944885,26.));
#96370=CARTESIAN_POINT('Ctrl Pts',(113.880396659483,18.3944768538998,31.));
#96371=CARTESIAN_POINT('Ctrl Pts',(113.880396659483,18.3944768538998,26.));
#96372=CARTESIAN_POINT('Ctrl Pts',(113.903986055946,18.3902329800346,31.));
#96373=CARTESIAN_POINT('Ctrl Pts',(113.903986055946,18.3902329800346,26.));
#96374=CARTESIAN_POINT('Ctrl Pts',(113.928228583663,18.3853272280411,31.));
#96375=CARTESIAN_POINT('Ctrl Pts',(113.928228583663,18.3853272280411,26.));
#96376=CARTESIAN_POINT('Ctrl Pts',(113.953000674982,18.3797541114119,31.));
#96377=CARTESIAN_POINT('Ctrl Pts',(113.953000674982,18.3797541114119,26.));
#96378=CARTESIAN_POINT('Ctrl Pts',(113.978245673333,18.3735102097034,31.));
#96379=CARTESIAN_POINT('Ctrl Pts',(113.978245673333,18.3735102097034,26.));
#96380=CARTESIAN_POINT('Ctrl Pts',(114.003948788046,18.3665933445275,31.));
#96381=CARTESIAN_POINT('Ctrl Pts',(114.003948788046,18.3665933445275,26.));
#96382=CARTESIAN_POINT('Ctrl Pts',(114.030119893761,18.359002138437,31.));
#96383=CARTESIAN_POINT('Ctrl Pts',(114.030119893761,18.359002138437,26.));
#96384=CARTESIAN_POINT('Ctrl Pts',(114.056774714484,18.3507355579086,31.));
#96385=CARTESIAN_POINT('Ctrl Pts',(114.056774714484,18.3507355579086,26.));
#96386=CARTESIAN_POINT('Ctrl Pts',(114.083913156659,18.3417926479699,31.));
#96387=CARTESIAN_POINT('Ctrl Pts',(114.083913156659,18.3417926479699,26.));
#96388=CARTESIAN_POINT('Ctrl Pts',(114.11151211949,18.332172212069,31.));
#96389=CARTESIAN_POINT('Ctrl Pts',(114.11151211949,18.332172212069,26.));
#96390=CARTESIAN_POINT('Ctrl Pts',(114.139535529399,18.3218724551479,31.));
#96391=CARTESIAN_POINT('Ctrl Pts',(114.139535529399,18.3218724551479,26.));
#96392=CARTESIAN_POINT('Ctrl Pts',(114.167939811637,18.3108907500782,31.));
#96393=CARTESIAN_POINT('Ctrl Pts',(114.167939811637,18.3108907500782,26.));
#96394=CARTESIAN_POINT('Ctrl Pts',(114.1966806629,18.2992235241669,31.));
#96395=CARTESIAN_POINT('Ctrl Pts',(114.1966806629,18.2992235241669,26.));
#96396=CARTESIAN_POINT('Ctrl Pts',(114.225720115684,18.2868661686388,31.));
#96397=CARTESIAN_POINT('Ctrl Pts',(114.225720115684,18.2868661686388,26.));
#96398=CARTESIAN_POINT('Ctrl Pts',(114.255030060531,18.2738133202861,31.));
#96399=CARTESIAN_POINT('Ctrl Pts',(114.255030060531,18.2738133202861,26.));
#96400=CARTESIAN_POINT('Ctrl Pts',(114.284589632559,18.2600596390535,31.));
#96401=CARTESIAN_POINT('Ctrl Pts',(114.284589632559,18.2600596390535,26.));
#96402=CARTESIAN_POINT('Ctrl Pts',(114.314384048769,18.2456006429046,31.));
#96403=CARTESIAN_POINT('Ctrl Pts',(114.314384048769,18.2456006429046,26.));
#96404=CARTESIAN_POINT('Ctrl Pts',(114.344402900622,18.2304335843055,31.));
#96405=CARTESIAN_POINT('Ctrl Pts',(114.344402900622,18.2304335843055,26.));
#96406=CARTESIAN_POINT('Ctrl Pts',(114.374638548469,18.2145586925326,31.));
#96407=CARTESIAN_POINT('Ctrl Pts',(114.374638548469,18.2145586925326,26.));
#96408=CARTESIAN_POINT('Ctrl Pts',(114.405084808554,18.1979797591469,31.));
#96409=CARTESIAN_POINT('Ctrl Pts',(114.405084808554,18.1979797591469,26.));
#96410=CARTESIAN_POINT('Ctrl Pts',(114.435737085489,18.1807021881057,31.));
#96411=CARTESIAN_POINT('Ctrl Pts',(114.435737085489,18.1807021881057,26.));
#96412=CARTESIAN_POINT('Ctrl Pts',(114.460421197281,18.1663257209028,31.));
#96413=CARTESIAN_POINT('Ctrl Pts',(114.460421197281,18.1663257209028,26.));
#96414=CARTESIAN_POINT('Ctrl Pts',(114.479024767707,18.1552334890775,31.));
#96415=CARTESIAN_POINT('Ctrl Pts',(114.479024767707,18.1552334890775,26.));
#96416=CARTESIAN_POINT('Ctrl Pts',(114.491467291217,18.1477011924174,31.));
#96417=CARTESIAN_POINT('Ctrl Pts',(114.491467291217,18.1477011924174,26.));
#96418=CARTESIAN_POINT('Ctrl Pts',(114.497698588799,18.1439006751855,31.));
#96419=CARTESIAN_POINT('Ctrl Pts',(114.497698588799,18.1439006751855,26.));
#96420=CARTESIAN_POINT('Ctrl Pts',(113.736838551019,18.4054542989899,31.));
#96421=CARTESIAN_POINT('Ctrl Pts',(113.739184232663,18.4056643904521,31.));
#96422=CARTESIAN_POINT('Ctrl Pts',(113.744039893058,18.406024771178,31.));
#96423=CARTESIAN_POINT('Ctrl Pts',(113.751816280134,18.4063859356827,31.));
#96424=CARTESIAN_POINT('Ctrl Pts',(113.763172329555,18.4065080254146,31.));
#96425=CARTESIAN_POINT('Ctrl Pts',(113.779011346313,18.4060571282676,31.));
#96426=CARTESIAN_POINT('Ctrl Pts',(113.796469501718,18.4049960963666,31.));
#96427=CARTESIAN_POINT('Ctrl Pts',(113.815484626163,18.4033166972605,31.));
#96428=CARTESIAN_POINT('Ctrl Pts',(113.835936540232,18.4010098525085,31.));
#96429=CARTESIAN_POINT('Ctrl Pts',(113.857643608342,18.3980662944885,31.));
#96430=CARTESIAN_POINT('Ctrl Pts',(113.880396659483,18.3944768538998,31.));
#96431=CARTESIAN_POINT('Ctrl Pts',(113.903986055946,18.3902329800346,31.));
#96432=CARTESIAN_POINT('Ctrl Pts',(113.928228583663,18.3853272280411,31.));
#96433=CARTESIAN_POINT('Ctrl Pts',(113.953000674982,18.3797541114119,31.));
#96434=CARTESIAN_POINT('Ctrl Pts',(113.978245673333,18.3735102097034,31.));
#96435=CARTESIAN_POINT('Ctrl Pts',(114.003948788046,18.3665933445275,31.));
#96436=CARTESIAN_POINT('Ctrl Pts',(114.030119893761,18.359002138437,31.));
#96437=CARTESIAN_POINT('Ctrl Pts',(114.056774714484,18.3507355579086,31.));
#96438=CARTESIAN_POINT('Ctrl Pts',(114.083913156659,18.3417926479699,31.));
#96439=CARTESIAN_POINT('Ctrl Pts',(114.11151211949,18.332172212069,31.));
#96440=CARTESIAN_POINT('Ctrl Pts',(114.139535529399,18.3218724551479,31.));
#96441=CARTESIAN_POINT('Ctrl Pts',(114.167939811637,18.3108907500782,31.));
#96442=CARTESIAN_POINT('Ctrl Pts',(114.1966806629,18.2992235241669,31.));
#96443=CARTESIAN_POINT('Ctrl Pts',(114.225720115684,18.2868661686388,31.));
#96444=CARTESIAN_POINT('Ctrl Pts',(114.255030060531,18.2738133202861,31.));
#96445=CARTESIAN_POINT('Ctrl Pts',(114.284589632559,18.2600596390535,31.));
#96446=CARTESIAN_POINT('Ctrl Pts',(114.314384048769,18.2456006429046,31.));
#96447=CARTESIAN_POINT('Ctrl Pts',(114.344402900622,18.2304335843055,31.));
#96448=CARTESIAN_POINT('Ctrl Pts',(114.374638548469,18.2145586925326,31.));
#96449=CARTESIAN_POINT('Ctrl Pts',(114.405084808554,18.1979797591469,31.));
#96450=CARTESIAN_POINT('Ctrl Pts',(114.435737085489,18.1807021881057,31.));
#96451=CARTESIAN_POINT('Ctrl Pts',(114.460421197281,18.1663257209028,31.));
#96452=CARTESIAN_POINT('Ctrl Pts',(114.479024767707,18.1552334890775,31.));
#96453=CARTESIAN_POINT('Ctrl Pts',(114.491467291217,18.1477011924174,31.));
#96454=CARTESIAN_POINT('Ctrl Pts',(114.497698588799,18.1439006751855,31.));
#96455=CARTESIAN_POINT('Ctrl Pts',(113.736838551019,18.4054542989899,26.));
#96456=CARTESIAN_POINT('Ctrl Pts',(113.739184232663,18.4056643904521,26.));
#96457=CARTESIAN_POINT('Ctrl Pts',(113.744039893058,18.406024771178,26.));
#96458=CARTESIAN_POINT('Ctrl Pts',(113.751816280134,18.4063859356827,26.));
#96459=CARTESIAN_POINT('Ctrl Pts',(113.763172329555,18.4065080254146,26.));
#96460=CARTESIAN_POINT('Ctrl Pts',(113.779011346313,18.4060571282676,26.));
#96461=CARTESIAN_POINT('Ctrl Pts',(113.796469501718,18.4049960963666,26.));
#96462=CARTESIAN_POINT('Ctrl Pts',(113.815484626163,18.4033166972605,26.));
#96463=CARTESIAN_POINT('Ctrl Pts',(113.835936540232,18.4010098525085,26.));
#96464=CARTESIAN_POINT('Ctrl Pts',(113.857643608342,18.3980662944885,26.));
#96465=CARTESIAN_POINT('Ctrl Pts',(113.880396659483,18.3944768538998,26.));
#96466=CARTESIAN_POINT('Ctrl Pts',(113.903986055946,18.3902329800346,26.));
#96467=CARTESIAN_POINT('Ctrl Pts',(113.928228583663,18.3853272280411,26.));
#96468=CARTESIAN_POINT('Ctrl Pts',(113.953000674982,18.3797541114119,26.));
#96469=CARTESIAN_POINT('Ctrl Pts',(113.978245673333,18.3735102097034,26.));
#96470=CARTESIAN_POINT('Ctrl Pts',(114.003948788046,18.3665933445275,26.));
#96471=CARTESIAN_POINT('Ctrl Pts',(114.030119893761,18.359002138437,26.));
#96472=CARTESIAN_POINT('Ctrl Pts',(114.056774714484,18.3507355579086,26.));
#96473=CARTESIAN_POINT('Ctrl Pts',(114.083913156659,18.3417926479699,26.));
#96474=CARTESIAN_POINT('Ctrl Pts',(114.11151211949,18.332172212069,26.));
#96475=CARTESIAN_POINT('Ctrl Pts',(114.139535529399,18.3218724551479,26.));
#96476=CARTESIAN_POINT('Ctrl Pts',(114.167939811637,18.3108907500782,26.));
#96477=CARTESIAN_POINT('Ctrl Pts',(114.1966806629,18.2992235241669,26.));
#96478=CARTESIAN_POINT('Ctrl Pts',(114.225720115684,18.2868661686388,26.));
#96479=CARTESIAN_POINT('Ctrl Pts',(114.255030060531,18.2738133202861,26.));
#96480=CARTESIAN_POINT('Ctrl Pts',(114.284589632559,18.2600596390535,26.));
#96481=CARTESIAN_POINT('Ctrl Pts',(114.314384048769,18.2456006429046,26.));
#96482=CARTESIAN_POINT('Ctrl Pts',(114.344402900622,18.2304335843055,26.));
#96483=CARTESIAN_POINT('Ctrl Pts',(114.374638548469,18.2145586925326,26.));
#96484=CARTESIAN_POINT('Ctrl Pts',(114.405084808554,18.1979797591469,26.));
#96485=CARTESIAN_POINT('Ctrl Pts',(114.435737085489,18.1807021881057,26.));
#96486=CARTESIAN_POINT('Ctrl Pts',(114.460421197281,18.1663257209028,26.));
#96487=CARTESIAN_POINT('Ctrl Pts',(114.479024767707,18.1552334890775,26.));
#96488=CARTESIAN_POINT('Ctrl Pts',(114.491467291217,18.1477011924174,26.));
#96489=CARTESIAN_POINT('Ctrl Pts',(114.497698588799,18.1439006751855,26.));
#96490=CARTESIAN_POINT('Origin',(113.853091274272,18.000000000016,31.));
#96491=CARTESIAN_POINT('Origin',(113.095253230553,17.0944435750604,31.));
#96492=CARTESIAN_POINT('',(113.60754929639,16.9445647253073,31.));
#96493=CARTESIAN_POINT('',(113.60754929639,16.9445647253073,31.));
#96494=CARTESIAN_POINT('',(113.60754929639,16.9445647253073,26.));
#96495=CARTESIAN_POINT('',(113.60754929639,16.9445647253073,31.));
#96496=CARTESIAN_POINT('',(113.60754929639,16.9445647253073,26.));
#96497=CARTESIAN_POINT('Origin',(113.297228010781,16.1953828688964,31.));
#96498=CARTESIAN_POINT('',(113.297228010781,16.1953828688964,26.));
#96499=CARTESIAN_POINT('',(112.828999637636,16.451650540008,26.));
#96500=CARTESIAN_POINT('',(113.297228010781,16.1953828688964,31.));
#96501=CARTESIAN_POINT('',(113.297228010781,16.1953828688964,31.));
#96502=CARTESIAN_POINT('',(112.828999637636,16.451650540008,31.));
#96503=CARTESIAN_POINT('Ctrl Pts',(114.100263265296,16.1458583777765,31.));
#96504=CARTESIAN_POINT('Ctrl Pts',(114.100263265296,16.1458583777765,26.));
#96505=CARTESIAN_POINT('Ctrl Pts',(114.093051902,16.1447317719895,31.));
#96506=CARTESIAN_POINT('Ctrl Pts',(114.093051902,16.1447317719895,26.));
#96507=CARTESIAN_POINT('Ctrl Pts',(114.078674024021,16.1425343847903,31.));
#96508=CARTESIAN_POINT('Ctrl Pts',(114.078674024021,16.1425343847903,26.));
#96509=CARTESIAN_POINT('Ctrl Pts',(114.057241752688,16.1394057769344,31.));
#96510=CARTESIAN_POINT('Ctrl Pts',(114.057241752688,16.1394057769344,26.));
#96511=CARTESIAN_POINT('Ctrl Pts',(114.028934971196,16.1355698537236,31.));
#96512=CARTESIAN_POINT('Ctrl Pts',(114.028934971196,16.1355698537236,26.));
#96513=CARTESIAN_POINT('Ctrl Pts',(113.994004119741,16.1313375780615,31.));
#96514=CARTESIAN_POINT('Ctrl Pts',(113.994004119741,16.1313375780615,26.));
#96515=CARTESIAN_POINT('Ctrl Pts',(113.959530960114,16.1276719202451,31.));
#96516=CARTESIAN_POINT('Ctrl Pts',(113.959530960114,16.1276719202451,26.));
#96517=CARTESIAN_POINT('Ctrl Pts',(113.925521805887,16.1245761142569,31.));
#96518=CARTESIAN_POINT('Ctrl Pts',(113.925521805887,16.1245761142569,26.));
#96519=CARTESIAN_POINT('Ctrl Pts',(113.891983821059,16.1220512965871,31.));
#96520=CARTESIAN_POINT('Ctrl Pts',(113.891983821059,16.1220512965871,26.));
#96521=CARTESIAN_POINT('Ctrl Pts',(113.858924151478,16.1200947554784,31.));
#96522=CARTESIAN_POINT('Ctrl Pts',(113.858924151478,16.1200947554784,26.));
#96523=CARTESIAN_POINT('Ctrl Pts',(113.826351361947,16.118699969367,31.));
#96524=CARTESIAN_POINT('Ctrl Pts',(113.826351361947,16.118699969367,26.));
#96525=CARTESIAN_POINT('Ctrl Pts',(113.79427739498,16.1178571401962,31.));
#96526=CARTESIAN_POINT('Ctrl Pts',(113.79427739498,16.1178571401962,26.));
#96527=CARTESIAN_POINT('Ctrl Pts',(113.762719483672,16.1175533497701,31.));
#96528=CARTESIAN_POINT('Ctrl Pts',(113.762719483672,16.1175533497701,26.));
#96529=CARTESIAN_POINT('Ctrl Pts',(113.73170154537,16.1177728861249,31.));
#96530=CARTESIAN_POINT('Ctrl Pts',(113.73170154537,16.1177728861249,26.));
#96531=CARTESIAN_POINT('Ctrl Pts',(113.701256893778,16.1184969617808,31.));
#96532=CARTESIAN_POINT('Ctrl Pts',(113.701256893778,16.1184969617808,26.));
#96533=CARTESIAN_POINT('Ctrl Pts',(113.671425092601,16.1197053218617,31.));
#96534=CARTESIAN_POINT('Ctrl Pts',(113.671425092601,16.1197053218617,26.));
#96535=CARTESIAN_POINT('Ctrl Pts',(113.642245394296,16.1213788638783,31.));
#96536=CARTESIAN_POINT('Ctrl Pts',(113.642245394296,16.1213788638783,26.));
#96537=CARTESIAN_POINT('Ctrl Pts',(113.613750439565,16.1235021246454,31.));
#96538=CARTESIAN_POINT('Ctrl Pts',(113.613750439565,16.1235021246454,26.));
#96539=CARTESIAN_POINT('Ctrl Pts',(113.585961112853,16.1260651583935,31.));
#96540=CARTESIAN_POINT('Ctrl Pts',(113.585961112853,16.1260651583935,26.));
#96541=CARTESIAN_POINT('Ctrl Pts',(113.558877135142,16.1290670470348,31.));
#96542=CARTESIAN_POINT('Ctrl Pts',(113.558877135142,16.1290670470348,26.));
#96543=CARTESIAN_POINT('Ctrl Pts',(113.532483583831,16.1325128530322,31.));
#96544=CARTESIAN_POINT('Ctrl Pts',(113.532483583831,16.1325128530322,26.));
#96545=CARTESIAN_POINT('Ctrl Pts',(113.506770808816,16.1364050826537,31.));
#96546=CARTESIAN_POINT('Ctrl Pts',(113.506770808816,16.1364050826537,26.));
#96547=CARTESIAN_POINT('Ctrl Pts',(113.481751641264,16.1407360631888,31.));
#96548=CARTESIAN_POINT('Ctrl Pts',(113.481751641264,16.1407360631888,26.));
#96549=CARTESIAN_POINT('Ctrl Pts',(113.457477116074,16.1454809530329,31.));
#96550=CARTESIAN_POINT('Ctrl Pts',(113.457477116074,16.1454809530329,26.));
#96551=CARTESIAN_POINT('Ctrl Pts',(113.434059295275,16.1505873960249,31.));
#96552=CARTESIAN_POINT('Ctrl Pts',(113.434059295275,16.1505873960249,26.));
#96553=CARTESIAN_POINT('Ctrl Pts',(113.411664597577,16.1559784010347,31.));
#96554=CARTESIAN_POINT('Ctrl Pts',(113.411664597577,16.1559784010347,26.));
#96555=CARTESIAN_POINT('Ctrl Pts',(113.390483430755,16.1615658433631,31.));
#96556=CARTESIAN_POINT('Ctrl Pts',(113.390483430755,16.1615658433631,26.));
#96557=CARTESIAN_POINT('Ctrl Pts',(113.370705534684,16.1672612053993,31.));
#96558=CARTESIAN_POINT('Ctrl Pts',(113.370705534684,16.1672612053993,26.));
#96559=CARTESIAN_POINT('Ctrl Pts',(113.352495172193,16.1729864160438,31.));
#96560=CARTESIAN_POINT('Ctrl Pts',(113.352495172193,16.1729864160438,26.));
#96561=CARTESIAN_POINT('Ctrl Pts',(113.335959900414,16.178687097234,31.));
#96562=CARTESIAN_POINT('Ctrl Pts',(113.335959900414,16.178687097234,26.));
#96563=CARTESIAN_POINT('Ctrl Pts',(113.32115400615,16.1843318518923,31.));
#96564=CARTESIAN_POINT('Ctrl Pts',(113.32115400615,16.1843318518923,26.));
#96565=CARTESIAN_POINT('Ctrl Pts',(113.310709106236,16.188790420063,31.));
#96566=CARTESIAN_POINT('Ctrl Pts',(113.310709106236,16.188790420063,26.));
#96567=CARTESIAN_POINT('Ctrl Pts',(113.303662873049,16.1920999870445,31.));
#96568=CARTESIAN_POINT('Ctrl Pts',(113.303662873049,16.1920999870445,26.));
#96569=CARTESIAN_POINT('Ctrl Pts',(113.299314739522,16.1942911161974,31.));
#96570=CARTESIAN_POINT('Ctrl Pts',(113.299314739522,16.1942911161974,26.));
#96571=CARTESIAN_POINT('Ctrl Pts',(113.297228010781,16.1953828688964,31.));
#96572=CARTESIAN_POINT('Ctrl Pts',(113.297228010781,16.1953828688964,26.));
#96573=CARTESIAN_POINT('',(114.100263265296,16.1458583777765,31.));
#96574=CARTESIAN_POINT('Ctrl Pts',(113.297228010781,16.1953828688964,31.));
#96575=CARTESIAN_POINT('Ctrl Pts',(113.299314739522,16.1942911161974,31.));
#96576=CARTESIAN_POINT('Ctrl Pts',(113.303662873049,16.1920999870445,31.));
#96577=CARTESIAN_POINT('Ctrl Pts',(113.310709106236,16.188790420063,31.));
#96578=CARTESIAN_POINT('Ctrl Pts',(113.32115400615,16.1843318518923,31.));
#96579=CARTESIAN_POINT('Ctrl Pts',(113.335959900414,16.178687097234,31.));
#96580=CARTESIAN_POINT('Ctrl Pts',(113.352495172193,16.1729864160438,31.));
#96581=CARTESIAN_POINT('Ctrl Pts',(113.370705534684,16.1672612053993,31.));
#96582=CARTESIAN_POINT('Ctrl Pts',(113.390483430755,16.1615658433631,31.));
#96583=CARTESIAN_POINT('Ctrl Pts',(113.411664597577,16.1559784010347,31.));
#96584=CARTESIAN_POINT('Ctrl Pts',(113.434059295275,16.1505873960249,31.));
#96585=CARTESIAN_POINT('Ctrl Pts',(113.457477116074,16.1454809530329,31.));
#96586=CARTESIAN_POINT('Ctrl Pts',(113.481751641264,16.1407360631888,31.));
#96587=CARTESIAN_POINT('Ctrl Pts',(113.506770808816,16.1364050826537,31.));
#96588=CARTESIAN_POINT('Ctrl Pts',(113.532483583831,16.1325128530322,31.));
#96589=CARTESIAN_POINT('Ctrl Pts',(113.558877135142,16.1290670470348,31.));
#96590=CARTESIAN_POINT('Ctrl Pts',(113.585961112853,16.1260651583935,31.));
#96591=CARTESIAN_POINT('Ctrl Pts',(113.613750439565,16.1235021246454,31.));
#96592=CARTESIAN_POINT('Ctrl Pts',(113.642245394296,16.1213788638783,31.));
#96593=CARTESIAN_POINT('Ctrl Pts',(113.671425092601,16.1197053218617,31.));
#96594=CARTESIAN_POINT('Ctrl Pts',(113.701256893778,16.1184969617808,31.));
#96595=CARTESIAN_POINT('Ctrl Pts',(113.73170154537,16.1177728861249,31.));
#96596=CARTESIAN_POINT('Ctrl Pts',(113.762719483672,16.1175533497701,31.));
#96597=CARTESIAN_POINT('Ctrl Pts',(113.79427739498,16.1178571401962,31.));
#96598=CARTESIAN_POINT('Ctrl Pts',(113.826351361947,16.118699969367,31.));
#96599=CARTESIAN_POINT('Ctrl Pts',(113.858924151478,16.1200947554784,31.));
#96600=CARTESIAN_POINT('Ctrl Pts',(113.891983821059,16.1220512965871,31.));
#96601=CARTESIAN_POINT('Ctrl Pts',(113.925521805887,16.1245761142569,31.));
#96602=CARTESIAN_POINT('Ctrl Pts',(113.959530960114,16.1276719202451,31.));
#96603=CARTESIAN_POINT('Ctrl Pts',(113.994004119741,16.1313375780615,31.));
#96604=CARTESIAN_POINT('Ctrl Pts',(114.028934971196,16.1355698537236,31.));
#96605=CARTESIAN_POINT('Ctrl Pts',(114.057241752688,16.1394057769344,31.));
#96606=CARTESIAN_POINT('Ctrl Pts',(114.078674024021,16.1425343847903,31.));
#96607=CARTESIAN_POINT('Ctrl Pts',(114.093051902,16.1447317719895,31.));
#96608=CARTESIAN_POINT('Ctrl Pts',(114.100263265296,16.1458583777765,31.));
#96609=CARTESIAN_POINT('',(114.100263265296,16.1458583777765,26.));
#96610=CARTESIAN_POINT('Ctrl Pts',(114.100263265296,16.1458583777765,26.));
#96611=CARTESIAN_POINT('Ctrl Pts',(114.093051902,16.1447317719895,26.));
#96612=CARTESIAN_POINT('Ctrl Pts',(114.078674024021,16.1425343847903,26.));
#96613=CARTESIAN_POINT('Ctrl Pts',(114.057241752688,16.1394057769344,26.));
#96614=CARTESIAN_POINT('Ctrl Pts',(114.028934971196,16.1355698537236,26.));
#96615=CARTESIAN_POINT('Ctrl Pts',(113.994004119741,16.1313375780615,26.));
#96616=CARTESIAN_POINT('Ctrl Pts',(113.959530960114,16.1276719202451,26.));
#96617=CARTESIAN_POINT('Ctrl Pts',(113.925521805887,16.1245761142569,26.));
#96618=CARTESIAN_POINT('Ctrl Pts',(113.891983821059,16.1220512965871,26.));
#96619=CARTESIAN_POINT('Ctrl Pts',(113.858924151478,16.1200947554784,26.));
#96620=CARTESIAN_POINT('Ctrl Pts',(113.826351361947,16.118699969367,26.));
#96621=CARTESIAN_POINT('Ctrl Pts',(113.79427739498,16.1178571401962,26.));
#96622=CARTESIAN_POINT('Ctrl Pts',(113.762719483672,16.1175533497701,26.));
#96623=CARTESIAN_POINT('Ctrl Pts',(113.73170154537,16.1177728861249,26.));
#96624=CARTESIAN_POINT('Ctrl Pts',(113.701256893778,16.1184969617808,26.));
#96625=CARTESIAN_POINT('Ctrl Pts',(113.671425092601,16.1197053218617,26.));
#96626=CARTESIAN_POINT('Ctrl Pts',(113.642245394296,16.1213788638783,26.));
#96627=CARTESIAN_POINT('Ctrl Pts',(113.613750439565,16.1235021246454,26.));
#96628=CARTESIAN_POINT('Ctrl Pts',(113.585961112853,16.1260651583935,26.));
#96629=CARTESIAN_POINT('Ctrl Pts',(113.558877135142,16.1290670470348,26.));
#96630=CARTESIAN_POINT('Ctrl Pts',(113.532483583831,16.1325128530322,26.));
#96631=CARTESIAN_POINT('Ctrl Pts',(113.506770808816,16.1364050826537,26.));
#96632=CARTESIAN_POINT('Ctrl Pts',(113.481751641264,16.1407360631888,26.));
#96633=CARTESIAN_POINT('Ctrl Pts',(113.457477116074,16.1454809530329,26.));
#96634=CARTESIAN_POINT('Ctrl Pts',(113.434059295275,16.1505873960249,26.));
#96635=CARTESIAN_POINT('Ctrl Pts',(113.411664597577,16.1559784010347,26.));
#96636=CARTESIAN_POINT('Ctrl Pts',(113.390483430755,16.1615658433631,26.));
#96637=CARTESIAN_POINT('Ctrl Pts',(113.370705534684,16.1672612053993,26.));
#96638=CARTESIAN_POINT('Ctrl Pts',(113.352495172193,16.1729864160438,26.));
#96639=CARTESIAN_POINT('Ctrl Pts',(113.335959900414,16.178687097234,26.));
#96640=CARTESIAN_POINT('Ctrl Pts',(113.32115400615,16.1843318518923,26.));
#96641=CARTESIAN_POINT('Ctrl Pts',(113.310709106236,16.188790420063,26.));
#96642=CARTESIAN_POINT('Ctrl Pts',(113.303662873049,16.1920999870445,26.));
#96643=CARTESIAN_POINT('Ctrl Pts',(113.299314739522,16.1942911161974,26.));
#96644=CARTESIAN_POINT('Ctrl Pts',(113.297228010781,16.1953828688964,26.));
#96645=CARTESIAN_POINT('',(114.100263265296,16.1458583777765,31.));
#96646=CARTESIAN_POINT('Origin',(109.999999999997,18.0000000000012,31.));
#96647=CARTESIAN_POINT('',(114.210400073896,16.4117521548133,31.));
#96648=CARTESIAN_POINT('Origin',(109.999999999997,18.0000000000012,31.));
#96649=CARTESIAN_POINT('',(114.210400073896,16.4117521548133,26.));
#96650=CARTESIAN_POINT('Origin',(109.999999999997,18.0000000000012,26.));
#96651=CARTESIAN_POINT('',(114.210400073896,16.4117521548133,31.));
#96652=CARTESIAN_POINT('Ctrl Pts',(113.60754929639,16.9445647253073,31.));
#96653=CARTESIAN_POINT('Ctrl Pts',(113.60754929639,16.9445647253073,26.));
#96654=CARTESIAN_POINT('Ctrl Pts',(113.609796822173,16.9438611710063,31.));
#96655=CARTESIAN_POINT('Ctrl Pts',(113.609796822173,16.9438611710063,26.));
#96656=CARTESIAN_POINT('Ctrl Pts',(113.614420779162,16.9423359385965,31.));
#96657=CARTESIAN_POINT('Ctrl Pts',(113.614420779162,16.9423359385965,26.));
#96658=CARTESIAN_POINT('Ctrl Pts',(113.62174343569,16.9396937165929,31.));
#96659=CARTESIAN_POINT('Ctrl Pts',(113.62174343569,16.9396937165929,26.));
#96660=CARTESIAN_POINT('Ctrl Pts',(113.632281779039,16.9354607408266,31.));
#96661=CARTESIAN_POINT('Ctrl Pts',(113.632281779039,16.9354607408266,26.));
#96662=CARTESIAN_POINT('Ctrl Pts',(113.646742571568,16.9289828368832,31.));
#96663=CARTESIAN_POINT('Ctrl Pts',(113.646742571568,16.9289828368832,26.));
#96664=CARTESIAN_POINT('Ctrl Pts',(113.662465764693,16.9213216243932,31.));
#96665=CARTESIAN_POINT('Ctrl Pts',(113.662465764693,16.9213216243932,26.));
#96666=CARTESIAN_POINT('Ctrl Pts',(113.679390770761,16.9124932888427,31.));
#96667=CARTESIAN_POINT('Ctrl Pts',(113.679390770761,16.9124932888427,26.));
#96668=CARTESIAN_POINT('Ctrl Pts',(113.697403084302,16.9025354335174,31.));
#96669=CARTESIAN_POINT('Ctrl Pts',(113.697403084302,16.9025354335174,26.));
#96670=CARTESIAN_POINT('Ctrl Pts',(113.716331349354,16.891509005179,31.));
#96671=CARTESIAN_POINT('Ctrl Pts',(113.716331349354,16.891509005179,26.));
#96672=CARTESIAN_POINT('Ctrl Pts',(113.73597880816,16.8794855787786,31.));
#96673=CARTESIAN_POINT('Ctrl Pts',(113.73597880816,16.8794855787786,26.));
#96674=CARTESIAN_POINT('Ctrl Pts',(113.75614850852,16.8665374793698,31.));
#96675=CARTESIAN_POINT('Ctrl Pts',(113.75614850852,16.8665374793698,26.));
#96676=CARTESIAN_POINT('Ctrl Pts',(113.776668333682,16.8527279417957,31.));
#96677=CARTESIAN_POINT('Ctrl Pts',(113.776668333682,16.8527279417957,26.));
#96678=CARTESIAN_POINT('Ctrl Pts',(113.797422022429,16.8380991844769,31.));
#96679=CARTESIAN_POINT('Ctrl Pts',(113.797422022429,16.8380991844769,26.));
#96680=CARTESIAN_POINT('Ctrl Pts',(113.818355921967,16.8226697288662,31.));
#96681=CARTESIAN_POINT('Ctrl Pts',(113.818355921967,16.8226697288662,26.));
#96682=CARTESIAN_POINT('Ctrl Pts',(113.839455533865,16.8064432225404,31.));
#96683=CARTESIAN_POINT('Ctrl Pts',(113.839455533865,16.8064432225404,26.));
#96684=CARTESIAN_POINT('Ctrl Pts',(113.860729453975,16.7894146140426,31.));
#96685=CARTESIAN_POINT('Ctrl Pts',(113.860729453975,16.7894146140426,26.));
#96686=CARTESIAN_POINT('Ctrl Pts',(113.882191813874,16.7715769312051,31.));
#96687=CARTESIAN_POINT('Ctrl Pts',(113.882191813874,16.7715769312051,26.));
#96688=CARTESIAN_POINT('Ctrl Pts',(113.903842161673,16.7529293275511,31.));
#96689=CARTESIAN_POINT('Ctrl Pts',(113.903842161673,16.7529293275511,26.));
#96690=CARTESIAN_POINT('Ctrl Pts',(113.92565869712,16.7334795379024,31.));
#96691=CARTESIAN_POINT('Ctrl Pts',(113.92565869712,16.7334795379024,26.));
#96692=CARTESIAN_POINT('Ctrl Pts',(113.947607405635,16.7132397086026,31.));
#96693=CARTESIAN_POINT('Ctrl Pts',(113.947607405635,16.7132397086026,26.));
#96694=CARTESIAN_POINT('Ctrl Pts',(113.969647024041,16.6922240878361,31.));
#96695=CARTESIAN_POINT('Ctrl Pts',(113.969647024041,16.6922240878361,26.));
#96696=CARTESIAN_POINT('Ctrl Pts',(113.991735254212,16.6704463290048,31.));
#96697=CARTESIAN_POINT('Ctrl Pts',(113.991735254212,16.6704463290048,26.));
#96698=CARTESIAN_POINT('Ctrl Pts',(114.013835255045,16.6479167036913,31.));
#96699=CARTESIAN_POINT('Ctrl Pts',(114.013835255045,16.6479167036913,26.));
#96700=CARTESIAN_POINT('Ctrl Pts',(114.035919004379,16.6246410139608,31.));
#96701=CARTESIAN_POINT('Ctrl Pts',(114.035919004379,16.6246410139608,26.));
#96702=CARTESIAN_POINT('Ctrl Pts',(114.057965182023,16.6006223108904,31.));
#96703=CARTESIAN_POINT('Ctrl Pts',(114.057965182023,16.6006223108904,26.));
#96704=CARTESIAN_POINT('Ctrl Pts',(114.079958415069,16.5758621108271,31.));
#96705=CARTESIAN_POINT('Ctrl Pts',(114.079958415069,16.5758621108271,26.));
#96706=CARTESIAN_POINT('Ctrl Pts',(114.101888035841,16.5503618585562,31.));
#96707=CARTESIAN_POINT('Ctrl Pts',(114.101888035841,16.5503618585562,26.));
#96708=CARTESIAN_POINT('Ctrl Pts',(114.123747073967,16.5241246894687,31.));
#96709=CARTESIAN_POINT('Ctrl Pts',(114.123747073967,16.5241246894687,26.));
#96710=CARTESIAN_POINT('Ctrl Pts',(114.145531267368,16.4971564729307,31.));
#96711=CARTESIAN_POINT('Ctrl Pts',(114.145531267368,16.4971564729307,26.));
#96712=CARTESIAN_POINT('Ctrl Pts',(114.167238438465,16.4694639601268,31.));
#96713=CARTESIAN_POINT('Ctrl Pts',(114.167238438465,16.4694639601268,26.));
#96714=CARTESIAN_POINT('Ctrl Pts',(114.184541948313,16.446735635703,31.));
#96715=CARTESIAN_POINT('Ctrl Pts',(114.184541948313,16.446735635703,26.));
#96716=CARTESIAN_POINT('Ctrl Pts',(114.197484592914,16.4293684715648,31.));
#96717=CARTESIAN_POINT('Ctrl Pts',(114.197484592914,16.4293684715648,26.));
#96718=CARTESIAN_POINT('Ctrl Pts',(114.206097500578,16.4176479892436,31.));
#96719=CARTESIAN_POINT('Ctrl Pts',(114.206097500578,16.4176479892436,26.));
#96720=CARTESIAN_POINT('Ctrl Pts',(114.210400073896,16.4117521548133,31.));
#96721=CARTESIAN_POINT('Ctrl Pts',(114.210400073896,16.4117521548133,26.));
#96722=CARTESIAN_POINT('Ctrl Pts',(113.60754929639,16.9445647253073,31.));
#96723=CARTESIAN_POINT('Ctrl Pts',(113.609796822173,16.9438611710063,31.));
#96724=CARTESIAN_POINT('Ctrl Pts',(113.614420779162,16.9423359385965,31.));
#96725=CARTESIAN_POINT('Ctrl Pts',(113.62174343569,16.9396937165929,31.));
#96726=CARTESIAN_POINT('Ctrl Pts',(113.632281779039,16.9354607408266,31.));
#96727=CARTESIAN_POINT('Ctrl Pts',(113.646742571568,16.9289828368832,31.));
#96728=CARTESIAN_POINT('Ctrl Pts',(113.662465764693,16.9213216243932,31.));
#96729=CARTESIAN_POINT('Ctrl Pts',(113.679390770761,16.9124932888427,31.));
#96730=CARTESIAN_POINT('Ctrl Pts',(113.697403084302,16.9025354335174,31.));
#96731=CARTESIAN_POINT('Ctrl Pts',(113.716331349354,16.891509005179,31.));
#96732=CARTESIAN_POINT('Ctrl Pts',(113.73597880816,16.8794855787786,31.));
#96733=CARTESIAN_POINT('Ctrl Pts',(113.75614850852,16.8665374793698,31.));
#96734=CARTESIAN_POINT('Ctrl Pts',(113.776668333682,16.8527279417957,31.));
#96735=CARTESIAN_POINT('Ctrl Pts',(113.797422022429,16.8380991844769,31.));
#96736=CARTESIAN_POINT('Ctrl Pts',(113.818355921967,16.8226697288662,31.));
#96737=CARTESIAN_POINT('Ctrl Pts',(113.839455533865,16.8064432225404,31.));
#96738=CARTESIAN_POINT('Ctrl Pts',(113.860729453975,16.7894146140426,31.));
#96739=CARTESIAN_POINT('Ctrl Pts',(113.882191813874,16.7715769312051,31.));
#96740=CARTESIAN_POINT('Ctrl Pts',(113.903842161673,16.7529293275511,31.));
#96741=CARTESIAN_POINT('Ctrl Pts',(113.92565869712,16.7334795379024,31.));
#96742=CARTESIAN_POINT('Ctrl Pts',(113.947607405635,16.7132397086026,31.));
#96743=CARTESIAN_POINT('Ctrl Pts',(113.969647024041,16.6922240878361,31.));
#96744=CARTESIAN_POINT('Ctrl Pts',(113.991735254212,16.6704463290048,31.));
#96745=CARTESIAN_POINT('Ctrl Pts',(114.013835255045,16.6479167036913,31.));
#96746=CARTESIAN_POINT('Ctrl Pts',(114.035919004379,16.6246410139608,31.));
#96747=CARTESIAN_POINT('Ctrl Pts',(114.057965182023,16.6006223108904,31.));
#96748=CARTESIAN_POINT('Ctrl Pts',(114.079958415069,16.5758621108271,31.));
#96749=CARTESIAN_POINT('Ctrl Pts',(114.101888035841,16.5503618585562,31.));
#96750=CARTESIAN_POINT('Ctrl Pts',(114.123747073967,16.5241246894687,31.));
#96751=CARTESIAN_POINT('Ctrl Pts',(114.145531267368,16.4971564729307,31.));
#96752=CARTESIAN_POINT('Ctrl Pts',(114.167238438465,16.4694639601268,31.));
#96753=CARTESIAN_POINT('Ctrl Pts',(114.184541948313,16.446735635703,31.));
#96754=CARTESIAN_POINT('Ctrl Pts',(114.197484592914,16.4293684715648,31.));
#96755=CARTESIAN_POINT('Ctrl Pts',(114.206097500578,16.4176479892436,31.));
#96756=CARTESIAN_POINT('Ctrl Pts',(114.210400073896,16.4117521548133,31.));
#96757=CARTESIAN_POINT('Ctrl Pts',(113.60754929639,16.9445647253073,26.));
#96758=CARTESIAN_POINT('Ctrl Pts',(113.609796822173,16.9438611710063,26.));
#96759=CARTESIAN_POINT('Ctrl Pts',(113.614420779162,16.9423359385965,26.));
#96760=CARTESIAN_POINT('Ctrl Pts',(113.62174343569,16.9396937165929,26.));
#96761=CARTESIAN_POINT('Ctrl Pts',(113.632281779039,16.9354607408266,26.));
#96762=CARTESIAN_POINT('Ctrl Pts',(113.646742571568,16.9289828368832,26.));
#96763=CARTESIAN_POINT('Ctrl Pts',(113.662465764693,16.9213216243932,26.));
#96764=CARTESIAN_POINT('Ctrl Pts',(113.679390770761,16.9124932888427,26.));
#96765=CARTESIAN_POINT('Ctrl Pts',(113.697403084302,16.9025354335174,26.));
#96766=CARTESIAN_POINT('Ctrl Pts',(113.716331349354,16.891509005179,26.));
#96767=CARTESIAN_POINT('Ctrl Pts',(113.73597880816,16.8794855787786,26.));
#96768=CARTESIAN_POINT('Ctrl Pts',(113.75614850852,16.8665374793698,26.));
#96769=CARTESIAN_POINT('Ctrl Pts',(113.776668333682,16.8527279417957,26.));
#96770=CARTESIAN_POINT('Ctrl Pts',(113.797422022429,16.8380991844769,26.));
#96771=CARTESIAN_POINT('Ctrl Pts',(113.818355921967,16.8226697288662,26.));
#96772=CARTESIAN_POINT('Ctrl Pts',(113.839455533865,16.8064432225404,26.));
#96773=CARTESIAN_POINT('Ctrl Pts',(113.860729453975,16.7894146140426,26.));
#96774=CARTESIAN_POINT('Ctrl Pts',(113.882191813874,16.7715769312051,26.));
#96775=CARTESIAN_POINT('Ctrl Pts',(113.903842161673,16.7529293275511,26.));
#96776=CARTESIAN_POINT('Ctrl Pts',(113.92565869712,16.7334795379024,26.));
#96777=CARTESIAN_POINT('Ctrl Pts',(113.947607405635,16.7132397086026,26.));
#96778=CARTESIAN_POINT('Ctrl Pts',(113.969647024041,16.6922240878361,26.));
#96779=CARTESIAN_POINT('Ctrl Pts',(113.991735254212,16.6704463290048,26.));
#96780=CARTESIAN_POINT('Ctrl Pts',(114.013835255045,16.6479167036913,26.));
#96781=CARTESIAN_POINT('Ctrl Pts',(114.035919004379,16.6246410139608,26.));
#96782=CARTESIAN_POINT('Ctrl Pts',(114.057965182023,16.6006223108904,26.));
#96783=CARTESIAN_POINT('Ctrl Pts',(114.079958415069,16.5758621108271,26.));
#96784=CARTESIAN_POINT('Ctrl Pts',(114.101888035841,16.5503618585562,26.));
#96785=CARTESIAN_POINT('Ctrl Pts',(114.123747073967,16.5241246894687,26.));
#96786=CARTESIAN_POINT('Ctrl Pts',(114.145531267368,16.4971564729307,26.));
#96787=CARTESIAN_POINT('Ctrl Pts',(114.167238438465,16.4694639601268,26.));
#96788=CARTESIAN_POINT('Ctrl Pts',(114.184541948313,16.446735635703,26.));
#96789=CARTESIAN_POINT('Ctrl Pts',(114.197484592914,16.4293684715648,26.));
#96790=CARTESIAN_POINT('Ctrl Pts',(114.206097500578,16.4176479892436,26.));
#96791=CARTESIAN_POINT('Ctrl Pts',(114.210400073896,16.4117521548133,26.));
#96792=CARTESIAN_POINT('Origin',(113.559792165204,16.5254858059605,31.));
#96793=CARTESIAN_POINT('Origin',(112.513099666751,15.978872823157,31.));
#96794=CARTESIAN_POINT('',(112.929043363902,15.6443556046521,31.));
#96795=CARTESIAN_POINT('',(112.929043363902,15.6443556046521,31.));
#96796=CARTESIAN_POINT('',(112.929043363902,15.6443556046521,26.));
#96797=CARTESIAN_POINT('',(112.929043363902,15.6443556046521,31.));
#96798=CARTESIAN_POINT('',(112.929043363902,15.6443556046521,26.));
#96799=CARTESIAN_POINT('Origin',(112.355644395348,15.0709566360981,31.));
#96800=CARTESIAN_POINT('',(112.355644395348,15.0709566360981,26.));
#96801=CARTESIAN_POINT('',(112.021127176843,15.4869003332485,26.));
#96802=CARTESIAN_POINT('',(112.355644395348,15.0709566360981,31.));
#96803=CARTESIAN_POINT('',(112.355644395348,15.0709566360981,31.));
#96804=CARTESIAN_POINT('',(112.021127176843,15.4869003332485,31.));
#96805=CARTESIAN_POINT('Ctrl Pts',(113.078600028632,14.7178936848864,31.));
#96806=CARTESIAN_POINT('Ctrl Pts',(113.078600028632,14.7178936848864,26.));
#96807=CARTESIAN_POINT('Ctrl Pts',(113.071506464311,14.719612506117,31.));
#96808=CARTESIAN_POINT('Ctrl Pts',(113.071506464311,14.719612506117,26.));
#96809=CARTESIAN_POINT('Ctrl Pts',(113.057382133449,14.7230845607538,31.));
#96810=CARTESIAN_POINT('Ctrl Pts',(113.057382133449,14.7230845607538,26.));
#96811=CARTESIAN_POINT('Ctrl Pts',(113.036384030238,14.7283958791472,31.));
#96812=CARTESIAN_POINT('Ctrl Pts',(113.036384030238,14.7283958791472,26.));
#96813=CARTESIAN_POINT('Ctrl Pts',(113.008764029925,14.7356844845053,31.));
#96814=CARTESIAN_POINT('Ctrl Pts',(113.008764029925,14.7356844845053,26.));
#96815=CARTESIAN_POINT('Ctrl Pts',(112.974872509435,14.7451418297753,31.));
#96816=CARTESIAN_POINT('Ctrl Pts',(112.974872509435,14.7451418297753,26.));
#96817=CARTESIAN_POINT('Ctrl Pts',(112.94162067632,14.7549475105959,31.));
#96818=CARTESIAN_POINT('Ctrl Pts',(112.94162067632,14.7549475105959,26.));
#96819=CARTESIAN_POINT('Ctrl Pts',(112.90901560115,14.7651020986781,31.));
#96820=CARTESIAN_POINT('Ctrl Pts',(112.90901560115,14.7651020986781,26.));
#96821=CARTESIAN_POINT('Ctrl Pts',(112.877064337514,14.7756039024585,31.));
#96822=CARTESIAN_POINT('Ctrl Pts',(112.877064337514,14.7756039024585,26.));
#96823=CARTESIAN_POINT('Ctrl Pts',(112.845772449569,14.7864476820017,31.));
#96824=CARTESIAN_POINT('Ctrl Pts',(112.845772449569,14.7864476820017,26.));
#96825=CARTESIAN_POINT('Ctrl Pts',(112.815145354468,14.7976241345605,31.));
#96826=CARTESIAN_POINT('Ctrl Pts',(112.815145354468,14.7976241345605,26.));
#96827=CARTESIAN_POINT('Ctrl Pts',(112.785190336101,14.8091196377086,31.));
#96828=CARTESIAN_POINT('Ctrl Pts',(112.785190336101,14.8091196377086,26.));
#96829=CARTESIAN_POINT('Ctrl Pts',(112.755918372192,14.8209156617695,31.));
#96830=CARTESIAN_POINT('Ctrl Pts',(112.755918372192,14.8209156617695,26.));
#96831=CARTESIAN_POINT('Ctrl Pts',(112.72734554678,14.8329885380086,31.));
#96832=CARTESIAN_POINT('Ctrl Pts',(112.72734554678,14.8329885380086,26.));
#96833=CARTESIAN_POINT('Ctrl Pts',(112.699495448057,14.8453081604554,31.));
#96834=CARTESIAN_POINT('Ctrl Pts',(112.699495448057,14.8453081604554,26.));
#96835=CARTESIAN_POINT('Ctrl Pts',(112.672396876915,14.8578406756703,31.));
#96836=CARTESIAN_POINT('Ctrl Pts',(112.672396876915,14.8578406756703,26.));
#96837=CARTESIAN_POINT('Ctrl Pts',(112.646078787689,14.8705534139887,31.));
#96838=CARTESIAN_POINT('Ctrl Pts',(112.646078787689,14.8705534139887,26.));
#96839=CARTESIAN_POINT('Ctrl Pts',(112.620565418951,14.8834195982355,31.));
#96840=CARTESIAN_POINT('Ctrl Pts',(112.620565418951,14.8834195982355,26.));
#96841=CARTESIAN_POINT('Ctrl Pts',(112.595872259332,14.8964220475858,31.));
#96842=CARTESIAN_POINT('Ctrl Pts',(112.595872259332,14.8964220475858,26.));
#96843=CARTESIAN_POINT('Ctrl Pts',(112.571998699714,14.9095600206129,31.));
#96844=CARTESIAN_POINT('Ctrl Pts',(112.571998699714,14.9095600206129,26.));
#96845=CARTESIAN_POINT('Ctrl Pts',(112.548932890734,14.9228439050547,31.));
#96846=CARTESIAN_POINT('Ctrl Pts',(112.548932890734,14.9228439050547,26.));
#96847=CARTESIAN_POINT('Ctrl Pts',(112.526666875965,14.9362797093362,31.));
#96848=CARTESIAN_POINT('Ctrl Pts',(112.526666875965,14.9362797093362,26.));
#96849=CARTESIAN_POINT('Ctrl Pts',(112.50520957364,14.9498554345222,31.));
#96850=CARTESIAN_POINT('Ctrl Pts',(112.50520957364,14.9498554345222,26.));
#96851=CARTESIAN_POINT('Ctrl Pts',(112.484598627387,14.9635285997518,31.));
#96852=CARTESIAN_POINT('Ctrl Pts',(112.484598627387,14.9635285997518,26.));
#96853=CARTESIAN_POINT('Ctrl Pts',(112.464917533186,14.9772079499578,31.));
#96854=CARTESIAN_POINT('Ctrl Pts',(112.464917533186,14.9772079499578,26.));
#96855=CARTESIAN_POINT('Ctrl Pts',(112.446290578648,14.9907586689278,31.));
#96856=CARTESIAN_POINT('Ctrl Pts',(112.446290578648,14.9907586689278,26.));
#96857=CARTESIAN_POINT('Ctrl Pts',(112.428859953754,15.0040264741551,31.));
#96858=CARTESIAN_POINT('Ctrl Pts',(112.428859953754,15.0040264741551,26.));
#96859=CARTESIAN_POINT('Ctrl Pts',(112.41276708107,15.0168569757243,31.));
#96860=CARTESIAN_POINT('Ctrl Pts',(112.41276708107,15.0168569757243,26.));
#96861=CARTESIAN_POINT('Ctrl Pts',(112.398133843146,15.0291151846807,31.));
#96862=CARTESIAN_POINT('Ctrl Pts',(112.398133843146,15.0291151846807,26.));
#96863=CARTESIAN_POINT('Ctrl Pts',(112.385038800229,15.0407097019132,31.));
#96864=CARTESIAN_POINT('Ctrl Pts',(112.385038800229,15.0407097019132,26.));
#96865=CARTESIAN_POINT('Ctrl Pts',(112.373520091646,15.0515907456439,31.));
#96866=CARTESIAN_POINT('Ctrl Pts',(112.373520091646,15.0515907456439,26.));
#96867=CARTESIAN_POINT('Ctrl Pts',(112.365576482567,15.0597070156712,31.));
#96868=CARTESIAN_POINT('Ctrl Pts',(112.365576482567,15.0597070156712,26.));
#96869=CARTESIAN_POINT('Ctrl Pts',(112.360333128396,15.0654611335682,31.));
#96870=CARTESIAN_POINT('Ctrl Pts',(112.360333128396,15.0654611335682,26.));
#96871=CARTESIAN_POINT('Ctrl Pts',(112.357154485652,15.0691494316078,31.));
#96872=CARTESIAN_POINT('Ctrl Pts',(112.357154485652,15.0691494316078,26.));
#96873=CARTESIAN_POINT('Ctrl Pts',(112.355644395348,15.0709566360981,31.));
#96874=CARTESIAN_POINT('Ctrl Pts',(112.355644395348,15.0709566360981,26.));
#96875=CARTESIAN_POINT('',(113.078600028632,14.7178936848864,31.));
#96876=CARTESIAN_POINT('Ctrl Pts',(112.355644395348,15.0709566360981,31.));
#96877=CARTESIAN_POINT('Ctrl Pts',(112.357154485652,15.0691494316078,31.));
#96878=CARTESIAN_POINT('Ctrl Pts',(112.360333128396,15.0654611335682,31.));
#96879=CARTESIAN_POINT('Ctrl Pts',(112.365576482567,15.0597070156712,31.));
#96880=CARTESIAN_POINT('Ctrl Pts',(112.373520091646,15.0515907456439,31.));
#96881=CARTESIAN_POINT('Ctrl Pts',(112.385038800229,15.0407097019132,31.));
#96882=CARTESIAN_POINT('Ctrl Pts',(112.398133843146,15.0291151846807,31.));
#96883=CARTESIAN_POINT('Ctrl Pts',(112.41276708107,15.0168569757243,31.));
#96884=CARTESIAN_POINT('Ctrl Pts',(112.428859953754,15.0040264741551,31.));
#96885=CARTESIAN_POINT('Ctrl Pts',(112.446290578648,14.9907586689278,31.));
#96886=CARTESIAN_POINT('Ctrl Pts',(112.464917533186,14.9772079499578,31.));
#96887=CARTESIAN_POINT('Ctrl Pts',(112.484598627387,14.9635285997518,31.));
#96888=CARTESIAN_POINT('Ctrl Pts',(112.50520957364,14.9498554345222,31.));
#96889=CARTESIAN_POINT('Ctrl Pts',(112.526666875965,14.9362797093362,31.));
#96890=CARTESIAN_POINT('Ctrl Pts',(112.548932890734,14.9228439050547,31.));
#96891=CARTESIAN_POINT('Ctrl Pts',(112.571998699714,14.9095600206129,31.));
#96892=CARTESIAN_POINT('Ctrl Pts',(112.595872259332,14.8964220475858,31.));
#96893=CARTESIAN_POINT('Ctrl Pts',(112.620565418951,14.8834195982355,31.));
#96894=CARTESIAN_POINT('Ctrl Pts',(112.646078787689,14.8705534139887,31.));
#96895=CARTESIAN_POINT('Ctrl Pts',(112.672396876915,14.8578406756703,31.));
#96896=CARTESIAN_POINT('Ctrl Pts',(112.699495448057,14.8453081604554,31.));
#96897=CARTESIAN_POINT('Ctrl Pts',(112.72734554678,14.8329885380086,31.));
#96898=CARTESIAN_POINT('Ctrl Pts',(112.755918372192,14.8209156617695,31.));
#96899=CARTESIAN_POINT('Ctrl Pts',(112.785190336101,14.8091196377086,31.));
#96900=CARTESIAN_POINT('Ctrl Pts',(112.815145354468,14.7976241345605,31.));
#96901=CARTESIAN_POINT('Ctrl Pts',(112.845772449569,14.7864476820017,31.));
#96902=CARTESIAN_POINT('Ctrl Pts',(112.877064337514,14.7756039024585,31.));
#96903=CARTESIAN_POINT('Ctrl Pts',(112.90901560115,14.7651020986781,31.));
#96904=CARTESIAN_POINT('Ctrl Pts',(112.94162067632,14.7549475105959,31.));
#96905=CARTESIAN_POINT('Ctrl Pts',(112.974872509435,14.7451418297753,31.));
#96906=CARTESIAN_POINT('Ctrl Pts',(113.008764029925,14.7356844845053,31.));
#96907=CARTESIAN_POINT('Ctrl Pts',(113.036384030238,14.7283958791472,31.));
#96908=CARTESIAN_POINT('Ctrl Pts',(113.057382133449,14.7230845607538,31.));
#96909=CARTESIAN_POINT('Ctrl Pts',(113.071506464311,14.719612506117,31.));
#96910=CARTESIAN_POINT('Ctrl Pts',(113.078600028632,14.7178936848864,31.));
#96911=CARTESIAN_POINT('',(113.078600028632,14.7178936848864,26.));
#96912=CARTESIAN_POINT('Ctrl Pts',(113.078600028632,14.7178936848864,26.));
#96913=CARTESIAN_POINT('Ctrl Pts',(113.071506464311,14.719612506117,26.));
#96914=CARTESIAN_POINT('Ctrl Pts',(113.057382133449,14.7230845607538,26.));
#96915=CARTESIAN_POINT('Ctrl Pts',(113.036384030238,14.7283958791472,26.));
#96916=CARTESIAN_POINT('Ctrl Pts',(113.008764029925,14.7356844845053,26.));
#96917=CARTESIAN_POINT('Ctrl Pts',(112.974872509435,14.7451418297753,26.));
#96918=CARTESIAN_POINT('Ctrl Pts',(112.94162067632,14.7549475105959,26.));
#96919=CARTESIAN_POINT('Ctrl Pts',(112.90901560115,14.7651020986781,26.));
#96920=CARTESIAN_POINT('Ctrl Pts',(112.877064337514,14.7756039024585,26.));
#96921=CARTESIAN_POINT('Ctrl Pts',(112.845772449569,14.7864476820017,26.));
#96922=CARTESIAN_POINT('Ctrl Pts',(112.815145354468,14.7976241345605,26.));
#96923=CARTESIAN_POINT('Ctrl Pts',(112.785190336101,14.8091196377086,26.));
#96924=CARTESIAN_POINT('Ctrl Pts',(112.755918372192,14.8209156617695,26.));
#96925=CARTESIAN_POINT('Ctrl Pts',(112.72734554678,14.8329885380086,26.));
#96926=CARTESIAN_POINT('Ctrl Pts',(112.699495448057,14.8453081604554,26.));
#96927=CARTESIAN_POINT('Ctrl Pts',(112.672396876915,14.8578406756703,26.));
#96928=CARTESIAN_POINT('Ctrl Pts',(112.646078787689,14.8705534139887,26.));
#96929=CARTESIAN_POINT('Ctrl Pts',(112.620565418951,14.8834195982355,26.));
#96930=CARTESIAN_POINT('Ctrl Pts',(112.595872259332,14.8964220475858,26.));
#96931=CARTESIAN_POINT('Ctrl Pts',(112.571998699714,14.9095600206129,26.));
#96932=CARTESIAN_POINT('Ctrl Pts',(112.548932890734,14.9228439050547,26.));
#96933=CARTESIAN_POINT('Ctrl Pts',(112.526666875965,14.9362797093362,26.));
#96934=CARTESIAN_POINT('Ctrl Pts',(112.50520957364,14.9498554345222,26.));
#96935=CARTESIAN_POINT('Ctrl Pts',(112.484598627387,14.9635285997518,26.));
#96936=CARTESIAN_POINT('Ctrl Pts',(112.464917533186,14.9772079499578,26.));
#96937=CARTESIAN_POINT('Ctrl Pts',(112.446290578648,14.9907586689278,26.));
#96938=CARTESIAN_POINT('Ctrl Pts',(112.428859953754,15.0040264741551,26.));
#96939=CARTESIAN_POINT('Ctrl Pts',(112.41276708107,15.0168569757243,26.));
#96940=CARTESIAN_POINT('Ctrl Pts',(112.398133843146,15.0291151846807,26.));
#96941=CARTESIAN_POINT('Ctrl Pts',(112.385038800229,15.0407097019132,26.));
#96942=CARTESIAN_POINT('Ctrl Pts',(112.373520091646,15.0515907456439,26.));
#96943=CARTESIAN_POINT('Ctrl Pts',(112.365576482567,15.0597070156712,26.));
#96944=CARTESIAN_POINT('Ctrl Pts',(112.360333128396,15.0654611335682,26.));
#96945=CARTESIAN_POINT('Ctrl Pts',(112.357154485652,15.0691494316078,26.));
#96946=CARTESIAN_POINT('Ctrl Pts',(112.355644395348,15.0709566360981,26.));
#96947=CARTESIAN_POINT('',(113.078600028632,14.7178936848864,31.));
#96948=CARTESIAN_POINT('Origin',(109.999999999998,18.0000000000022,31.));
#96949=CARTESIAN_POINT('',(113.282106315114,14.9213999713683,31.));
#96950=CARTESIAN_POINT('Origin',(109.999999999998,18.0000000000022,31.));
#96951=CARTESIAN_POINT('',(113.282106315114,14.9213999713683,26.));
#96952=CARTESIAN_POINT('Origin',(109.999999999998,18.0000000000022,26.));
#96953=CARTESIAN_POINT('',(113.282106315114,14.9213999713683,31.));
#96954=CARTESIAN_POINT('Ctrl Pts',(112.929043363902,15.6443556046521,31.));
#96955=CARTESIAN_POINT('Ctrl Pts',(112.929043363902,15.6443556046521,26.));
#96956=CARTESIAN_POINT('Ctrl Pts',(112.930850568397,15.6428455143525,31.));
#96957=CARTESIAN_POINT('Ctrl Pts',(112.930850568397,15.6428455143525,26.));
#96958=CARTESIAN_POINT('Ctrl Pts',(112.934538866444,15.6396668716152,31.));
#96959=CARTESIAN_POINT('Ctrl Pts',(112.934538866444,15.6396668716152,26.));
#96960=CARTESIAN_POINT('Ctrl Pts',(112.940292984349,15.6344235174514,31.));
#96961=CARTESIAN_POINT('Ctrl Pts',(112.940292984349,15.6344235174514,26.));
#96962=CARTESIAN_POINT('Ctrl Pts',(112.94840925438,15.6264799083753,31.));
#96963=CARTESIAN_POINT('Ctrl Pts',(112.94840925438,15.6264799083753,26.));
#96964=CARTESIAN_POINT('Ctrl Pts',(112.959290298106,15.6149611997885,31.));
#96965=CARTESIAN_POINT('Ctrl Pts',(112.959290298106,15.6149611997885,26.));
#96966=CARTESIAN_POINT('Ctrl Pts',(112.970884815328,15.6018661568621,31.));
#96967=CARTESIAN_POINT('Ctrl Pts',(112.970884815328,15.6018661568621,26.));
#96968=CARTESIAN_POINT('Ctrl Pts',(112.983143024272,15.5872329189258,31.));
#96969=CARTESIAN_POINT('Ctrl Pts',(112.983143024272,15.5872329189258,26.));
#96970=CARTESIAN_POINT('Ctrl Pts',(112.99597352583,15.5711400462322,31.));
#96971=CARTESIAN_POINT('Ctrl Pts',(112.99597352583,15.5711400462322,26.));
#96972=CARTESIAN_POINT('Ctrl Pts',(113.009241331054,15.5537094213352,31.));
#96973=CARTESIAN_POINT('Ctrl Pts',(113.009241331054,15.5537094213352,26.));
#96974=CARTESIAN_POINT('Ctrl Pts',(113.022792050028,15.5350824667997,31.));
#96975=CARTESIAN_POINT('Ctrl Pts',(113.022792050028,15.5350824667997,26.));
#96976=CARTESIAN_POINT('Ctrl Pts',(113.036471400243,15.5154013726076,31.));
#96977=CARTESIAN_POINT('Ctrl Pts',(113.036471400243,15.5154013726076,26.));
#96978=CARTESIAN_POINT('Ctrl Pts',(113.050144565483,15.4947904263648,31.));
#96979=CARTESIAN_POINT('Ctrl Pts',(113.050144565483,15.4947904263648,26.));
#96980=CARTESIAN_POINT('Ctrl Pts',(113.063720290677,15.4733331240482,31.));
#96981=CARTESIAN_POINT('Ctrl Pts',(113.063720290677,15.4733331240482,26.));
#96982=CARTESIAN_POINT('Ctrl Pts',(113.077156094964,15.4510671092837,31.));
#96983=CARTESIAN_POINT('Ctrl Pts',(113.077156094964,15.4510671092837,26.));
#96984=CARTESIAN_POINT('Ctrl Pts',(113.090439979404,15.4280013003025,31.));
#96985=CARTESIAN_POINT('Ctrl Pts',(113.090439979404,15.4280013003025,26.));
#96986=CARTESIAN_POINT('Ctrl Pts',(113.103577952422,15.4041277406764,31.));
#96987=CARTESIAN_POINT('Ctrl Pts',(113.103577952422,15.4041277406764,26.));
#96988=CARTESIAN_POINT('Ctrl Pts',(113.116580401758,15.3794345810427,31.));
#96989=CARTESIAN_POINT('Ctrl Pts',(113.116580401758,15.3794345810427,26.));
#96990=CARTESIAN_POINT('Ctrl Pts',(113.12944658599,15.3539212122889,31.));
#96991=CARTESIAN_POINT('Ctrl Pts',(113.12944658599,15.3539212122889,26.));
#96992=CARTESIAN_POINT('Ctrl Pts',(113.142159324298,15.3276031230536,31.));
#96993=CARTESIAN_POINT('Ctrl Pts',(113.142159324298,15.3276031230536,26.));
#96994=CARTESIAN_POINT('Ctrl Pts',(113.154691839513,15.3005045519114,31.));
#96995=CARTESIAN_POINT('Ctrl Pts',(113.154691839513,15.3005045519114,26.));
#96996=CARTESIAN_POINT('Ctrl Pts',(113.167011461974,15.2726544532028,31.));
#96997=CARTESIAN_POINT('Ctrl Pts',(113.167011461974,15.2726544532028,26.));
#96998=CARTESIAN_POINT('Ctrl Pts',(113.17908433824,15.2440816278177,31.));
#96999=CARTESIAN_POINT('Ctrl Pts',(113.17908433824,15.2440816278177,26.));
#97000=CARTESIAN_POINT('Ctrl Pts',(113.190880362334,15.2148096639412,31.));
#97001=CARTESIAN_POINT('Ctrl Pts',(113.190880362334,15.2148096639412,26.));
#97002=CARTESIAN_POINT('Ctrl Pts',(113.202375865507,15.1848546455997,31.));
#97003=CARTESIAN_POINT('Ctrl Pts',(113.202375865507,15.1848546455997,26.));
#97004=CARTESIAN_POINT('Ctrl Pts',(113.213552318071,15.1542275505039,31.));
#97005=CARTESIAN_POINT('Ctrl Pts',(113.213552318071,15.1542275505039,26.));
#97006=CARTESIAN_POINT('Ctrl Pts',(113.224396097589,15.1229356625341,31.));
#97007=CARTESIAN_POINT('Ctrl Pts',(113.224396097589,15.1229356625341,26.));
#97008=CARTESIAN_POINT('Ctrl Pts',(113.234897901312,15.0909843988393,31.));
#97009=CARTESIAN_POINT('Ctrl Pts',(113.234897901312,15.0909843988393,26.));
#97010=CARTESIAN_POINT('Ctrl Pts',(113.245052489315,15.0583793235901,31.));
#97011=CARTESIAN_POINT('Ctrl Pts',(113.245052489315,15.0583793235901,26.));
#97012=CARTESIAN_POINT('Ctrl Pts',(113.254858170061,15.0251274904002,31.));
#97013=CARTESIAN_POINT('Ctrl Pts',(113.254858170061,15.0251274904002,26.));
#97014=CARTESIAN_POINT('Ctrl Pts',(113.264315515295,14.9912359698749,31.));
#97015=CARTESIAN_POINT('Ctrl Pts',(113.264315515295,14.9912359698749,26.));
#97016=CARTESIAN_POINT('Ctrl Pts',(113.271604120682,14.9636159695907,31.));
#97017=CARTESIAN_POINT('Ctrl Pts',(113.271604120682,14.9636159695907,26.));
#97018=CARTESIAN_POINT('Ctrl Pts',(113.276915439142,14.942617866446,31.));
#97019=CARTESIAN_POINT('Ctrl Pts',(113.276915439142,14.942617866446,26.));
#97020=CARTESIAN_POINT('Ctrl Pts',(113.280387493845,14.9284935356507,31.));
#97021=CARTESIAN_POINT('Ctrl Pts',(113.280387493845,14.9284935356507,26.));
#97022=CARTESIAN_POINT('Ctrl Pts',(113.282106315114,14.9213999713683,31.));
#97023=CARTESIAN_POINT('Ctrl Pts',(113.282106315114,14.9213999713683,26.));
#97024=CARTESIAN_POINT('Ctrl Pts',(112.929043363902,15.6443556046521,31.));
#97025=CARTESIAN_POINT('Ctrl Pts',(112.930850568397,15.6428455143525,31.));
#97026=CARTESIAN_POINT('Ctrl Pts',(112.934538866444,15.6396668716152,31.));
#97027=CARTESIAN_POINT('Ctrl Pts',(112.940292984349,15.6344235174514,31.));
#97028=CARTESIAN_POINT('Ctrl Pts',(112.94840925438,15.6264799083753,31.));
#97029=CARTESIAN_POINT('Ctrl Pts',(112.959290298106,15.6149611997885,31.));
#97030=CARTESIAN_POINT('Ctrl Pts',(112.970884815328,15.6018661568621,31.));
#97031=CARTESIAN_POINT('Ctrl Pts',(112.983143024272,15.5872329189258,31.));
#97032=CARTESIAN_POINT('Ctrl Pts',(112.99597352583,15.5711400462322,31.));
#97033=CARTESIAN_POINT('Ctrl Pts',(113.009241331054,15.5537094213352,31.));
#97034=CARTESIAN_POINT('Ctrl Pts',(113.022792050028,15.5350824667997,31.));
#97035=CARTESIAN_POINT('Ctrl Pts',(113.036471400243,15.5154013726076,31.));
#97036=CARTESIAN_POINT('Ctrl Pts',(113.050144565483,15.4947904263648,31.));
#97037=CARTESIAN_POINT('Ctrl Pts',(113.063720290677,15.4733331240482,31.));
#97038=CARTESIAN_POINT('Ctrl Pts',(113.077156094964,15.4510671092837,31.));
#97039=CARTESIAN_POINT('Ctrl Pts',(113.090439979404,15.4280013003025,31.));
#97040=CARTESIAN_POINT('Ctrl Pts',(113.103577952422,15.4041277406764,31.));
#97041=CARTESIAN_POINT('Ctrl Pts',(113.116580401758,15.3794345810427,31.));
#97042=CARTESIAN_POINT('Ctrl Pts',(113.12944658599,15.3539212122889,31.));
#97043=CARTESIAN_POINT('Ctrl Pts',(113.142159324298,15.3276031230536,31.));
#97044=CARTESIAN_POINT('Ctrl Pts',(113.154691839513,15.3005045519114,31.));
#97045=CARTESIAN_POINT('Ctrl Pts',(113.167011461974,15.2726544532028,31.));
#97046=CARTESIAN_POINT('Ctrl Pts',(113.17908433824,15.2440816278177,31.));
#97047=CARTESIAN_POINT('Ctrl Pts',(113.190880362334,15.2148096639412,31.));
#97048=CARTESIAN_POINT('Ctrl Pts',(113.202375865507,15.1848546455997,31.));
#97049=CARTESIAN_POINT('Ctrl Pts',(113.213552318071,15.1542275505039,31.));
#97050=CARTESIAN_POINT('Ctrl Pts',(113.224396097589,15.1229356625341,31.));
#97051=CARTESIAN_POINT('Ctrl Pts',(113.234897901312,15.0909843988393,31.));
#97052=CARTESIAN_POINT('Ctrl Pts',(113.245052489315,15.0583793235901,31.));
#97053=CARTESIAN_POINT('Ctrl Pts',(113.254858170061,15.0251274904002,31.));
#97054=CARTESIAN_POINT('Ctrl Pts',(113.264315515295,14.9912359698749,31.));
#97055=CARTESIAN_POINT('Ctrl Pts',(113.271604120682,14.9636159695907,31.));
#97056=CARTESIAN_POINT('Ctrl Pts',(113.276915439142,14.942617866446,31.));
#97057=CARTESIAN_POINT('Ctrl Pts',(113.280387493845,14.9284935356507,31.));
#97058=CARTESIAN_POINT('Ctrl Pts',(113.282106315114,14.9213999713683,31.));
#97059=CARTESIAN_POINT('Ctrl Pts',(112.929043363902,15.6443556046521,26.));
#97060=CARTESIAN_POINT('Ctrl Pts',(112.930850568397,15.6428455143525,26.));
#97061=CARTESIAN_POINT('Ctrl Pts',(112.934538866444,15.6396668716152,26.));
#97062=CARTESIAN_POINT('Ctrl Pts',(112.940292984349,15.6344235174514,26.));
#97063=CARTESIAN_POINT('Ctrl Pts',(112.94840925438,15.6264799083753,26.));
#97064=CARTESIAN_POINT('Ctrl Pts',(112.959290298106,15.6149611997885,26.));
#97065=CARTESIAN_POINT('Ctrl Pts',(112.970884815328,15.6018661568621,26.));
#97066=CARTESIAN_POINT('Ctrl Pts',(112.983143024272,15.5872329189258,26.));
#97067=CARTESIAN_POINT('Ctrl Pts',(112.99597352583,15.5711400462322,26.));
#97068=CARTESIAN_POINT('Ctrl Pts',(113.009241331054,15.5537094213352,26.));
#97069=CARTESIAN_POINT('Ctrl Pts',(113.022792050028,15.5350824667997,26.));
#97070=CARTESIAN_POINT('Ctrl Pts',(113.036471400243,15.5154013726076,26.));
#97071=CARTESIAN_POINT('Ctrl Pts',(113.050144565483,15.4947904263648,26.));
#97072=CARTESIAN_POINT('Ctrl Pts',(113.063720290677,15.4733331240482,26.));
#97073=CARTESIAN_POINT('Ctrl Pts',(113.077156094964,15.4510671092837,26.));
#97074=CARTESIAN_POINT('Ctrl Pts',(113.090439979404,15.4280013003025,26.));
#97075=CARTESIAN_POINT('Ctrl Pts',(113.103577952422,15.4041277406764,26.));
#97076=CARTESIAN_POINT('Ctrl Pts',(113.116580401758,15.3794345810427,26.));
#97077=CARTESIAN_POINT('Ctrl Pts',(113.12944658599,15.3539212122889,26.));
#97078=CARTESIAN_POINT('Ctrl Pts',(113.142159324298,15.3276031230536,26.));
#97079=CARTESIAN_POINT('Ctrl Pts',(113.154691839513,15.3005045519114,26.));
#97080=CARTESIAN_POINT('Ctrl Pts',(113.167011461974,15.2726544532028,26.));
#97081=CARTESIAN_POINT('Ctrl Pts',(113.17908433824,15.2440816278177,26.));
#97082=CARTESIAN_POINT('Ctrl Pts',(113.190880362334,15.2148096639412,26.));
#97083=CARTESIAN_POINT('Ctrl Pts',(113.202375865507,15.1848546455997,26.));
#97084=CARTESIAN_POINT('Ctrl Pts',(113.213552318071,15.1542275505039,26.));
#97085=CARTESIAN_POINT('Ctrl Pts',(113.224396097589,15.1229356625341,26.));
#97086=CARTESIAN_POINT('Ctrl Pts',(113.234897901312,15.0909843988393,26.));
#97087=CARTESIAN_POINT('Ctrl Pts',(113.245052489315,15.0583793235901,26.));
#97088=CARTESIAN_POINT('Ctrl Pts',(113.254858170061,15.0251274904002,26.));
#97089=CARTESIAN_POINT('Ctrl Pts',(113.264315515295,14.9912359698749,26.));
#97090=CARTESIAN_POINT('Ctrl Pts',(113.271604120682,14.9636159695907,26.));
#97091=CARTESIAN_POINT('Ctrl Pts',(113.276915439142,14.942617866446,26.));
#97092=CARTESIAN_POINT('Ctrl Pts',(113.280387493845,14.9284935356507,26.));
#97093=CARTESIAN_POINT('Ctrl Pts',(113.282106315114,14.9213999713683,26.));
#97094=CARTESIAN_POINT('Origin',(112.72454696858,15.2754530314429,31.));
#97095=CARTESIAN_POINT('Origin',(111.548349459992,15.1710003623644,31.));
#97096=CARTESIAN_POINT('',(111.804617131104,14.702771989219,31.));
#97097=CARTESIAN_POINT('',(111.804617131104,14.702771989219,31.));
#97098=CARTESIAN_POINT('',(111.804617131104,14.702771989219,26.));
#97099=CARTESIAN_POINT('',(111.804617131104,14.702771989219,31.));
#97100=CARTESIAN_POINT('',(111.804617131104,14.702771989219,26.));
#97101=CARTESIAN_POINT('Origin',(111.055435274693,14.3924507036097,31.));
#97102=CARTESIAN_POINT('',(111.055435274693,14.3924507036097,26.));
#97103=CARTESIAN_POINT('',(110.90555642494,14.9047467694467,26.));
#97104=CARTESIAN_POINT('',(111.055435274693,14.3924507036097,31.));
#97105=CARTESIAN_POINT('',(111.055435274693,14.3924507036097,31.));
#97106=CARTESIAN_POINT('',(110.90555642494,14.9047467694467,31.));
#97107=CARTESIAN_POINT('Ctrl Pts',(111.588247845187,13.7895999261044,31.));
#97108=CARTESIAN_POINT('Ctrl Pts',(111.588247845187,13.7895999261044,26.));
#97109=CARTESIAN_POINT('Ctrl Pts',(111.582352010706,13.7939024994014,31.));
#97110=CARTESIAN_POINT('Ctrl Pts',(111.582352010706,13.7939024994014,26.));
#97111=CARTESIAN_POINT('Ctrl Pts',(111.570631528299,13.80251540703,31.));
#97112=CARTESIAN_POINT('Ctrl Pts',(111.570631528299,13.80251540703,26.));
#97113=CARTESIAN_POINT('Ctrl Pts',(111.553264364073,13.8154580515946,31.));
#97114=CARTESIAN_POINT('Ctrl Pts',(111.553264364073,13.8154580515946,26.));
#97115=CARTESIAN_POINT('Ctrl Pts',(111.530536039611,13.8327615614272,31.));
#97116=CARTESIAN_POINT('Ctrl Pts',(111.530536039611,13.8327615614272,26.));
#97117=CARTESIAN_POINT('Ctrl Pts',(111.502843526855,13.8544687325429,31.));
#97118=CARTESIAN_POINT('Ctrl Pts',(111.502843526855,13.8544687325429,26.));
#97119=CARTESIAN_POINT('Ctrl Pts',(111.475875310414,13.8762529259845,31.));
#97120=CARTESIAN_POINT('Ctrl Pts',(111.475875310414,13.8762529259845,26.));
#97121=CARTESIAN_POINT('Ctrl Pts',(111.44963814143,13.8981119641531,31.));
#97122=CARTESIAN_POINT('Ctrl Pts',(111.44963814143,13.8981119641531,26.));
#97123=CARTESIAN_POINT('Ctrl Pts',(111.424137889235,13.9200415849572,31.));
#97124=CARTESIAN_POINT('Ctrl Pts',(111.424137889235,13.9200415849572,26.));
#97125=CARTESIAN_POINT('Ctrl Pts',(111.399377689205,13.9420348180159,31.));
#97126=CARTESIAN_POINT('Ctrl Pts',(111.399377689205,13.9420348180159,26.));
#97127=CARTESIAN_POINT('Ctrl Pts',(111.375358986128,13.9640809956577,31.));
#97128=CARTESIAN_POINT('Ctrl Pts',(111.375358986128,13.9640809956577,26.));
#97129=CARTESIAN_POINT('Ctrl Pts',(111.352083296364,13.9861647449775,31.));
#97130=CARTESIAN_POINT('Ctrl Pts',(111.352083296364,13.9861647449775,26.));
#97131=CARTESIAN_POINT('Ctrl Pts',(111.329553671008,14.0082647457932,31.));
#97132=CARTESIAN_POINT('Ctrl Pts',(111.329553671008,14.0082647457932,26.));
#97133=CARTESIAN_POINT('Ctrl Pts',(111.307775912141,14.0303529759501,31.));
#97134=CARTESIAN_POINT('Ctrl Pts',(111.307775912141,14.0303529759501,26.));
#97135=CARTESIAN_POINT('Ctrl Pts',(111.286760291356,14.052392594348,31.));
#97136=CARTESIAN_POINT('Ctrl Pts',(111.286760291356,14.052392594348,26.));
#97137=CARTESIAN_POINT('Ctrl Pts',(111.266520462056,14.0743413028629,31.));
#97138=CARTESIAN_POINT('Ctrl Pts',(111.266520462056,14.0743413028629,26.));
#97139=CARTESIAN_POINT('Ctrl Pts',(111.24707067242,14.0961578383154,31.));
#97140=CARTESIAN_POINT('Ctrl Pts',(111.24707067242,14.0961578383154,26.));
#97141=CARTESIAN_POINT('Ctrl Pts',(111.228423068787,14.1178081861225,31.));
#97142=CARTESIAN_POINT('Ctrl Pts',(111.228423068787,14.1178081861225,26.));
#97143=CARTESIAN_POINT('Ctrl Pts',(111.210585385968,14.1392705460289,31.));
#97144=CARTESIAN_POINT('Ctrl Pts',(111.210585385968,14.1392705460289,26.));
#97145=CARTESIAN_POINT('Ctrl Pts',(111.193556777481,14.1605444661444,31.));
#97146=CARTESIAN_POINT('Ctrl Pts',(111.193556777481,14.1605444661444,26.));
#97147=CARTESIAN_POINT('Ctrl Pts',(111.177330271158,14.1816440780432,31.));
#97148=CARTESIAN_POINT('Ctrl Pts',(111.177330271158,14.1816440780432,26.));
#97149=CARTESIAN_POINT('Ctrl Pts',(111.161900815541,14.2025779775787,31.));
#97150=CARTESIAN_POINT('Ctrl Pts',(111.161900815541,14.2025779775787,26.));
#97151=CARTESIAN_POINT('Ctrl Pts',(111.14727205821,14.2233316663202,31.));
#97152=CARTESIAN_POINT('Ctrl Pts',(111.14727205821,14.2233316663202,26.));
#97153=CARTESIAN_POINT('Ctrl Pts',(111.133462520623,14.2438514914768,31.));
#97154=CARTESIAN_POINT('Ctrl Pts',(111.133462520623,14.2438514914768,26.));
#97155=CARTESIAN_POINT('Ctrl Pts',(111.120514421203,14.2640211918315,31.));
#97156=CARTESIAN_POINT('Ctrl Pts',(111.120514421203,14.2640211918315,26.));
#97157=CARTESIAN_POINT('Ctrl Pts',(111.108490994798,14.2836686506361,31.));
#97158=CARTESIAN_POINT('Ctrl Pts',(111.108490994798,14.2836686506361,26.));
#97159=CARTESIAN_POINT('Ctrl Pts',(111.097464566465,14.3025969156895,31.));
#97160=CARTESIAN_POINT('Ctrl Pts',(111.097464566465,14.3025969156895,26.));
#97161=CARTESIAN_POINT('Ctrl Pts',(111.087506711152,14.3206092292363,31.));
#97162=CARTESIAN_POINT('Ctrl Pts',(111.087506711152,14.3206092292363,26.));
#97163=CARTESIAN_POINT('Ctrl Pts',(111.078678375617,14.3375342353121,31.));
#97164=CARTESIAN_POINT('Ctrl Pts',(111.078678375617,14.3375342353121,26.));
#97165=CARTESIAN_POINT('Ctrl Pts',(111.07101716314,14.3532574284428,31.));
#97166=CARTESIAN_POINT('Ctrl Pts',(111.07101716314,14.3532574284428,26.));
#97167=CARTESIAN_POINT('Ctrl Pts',(111.064539259202,14.3677182209748,31.));
#97168=CARTESIAN_POINT('Ctrl Pts',(111.064539259202,14.3677182209748,26.));
#97169=CARTESIAN_POINT('Ctrl Pts',(111.060306283432,14.3782565643212,31.));
#97170=CARTESIAN_POINT('Ctrl Pts',(111.060306283432,14.3782565643212,26.));
#97171=CARTESIAN_POINT('Ctrl Pts',(111.057664061419,14.3855792208451,31.));
#97172=CARTESIAN_POINT('Ctrl Pts',(111.057664061419,14.3855792208451,26.));
#97173=CARTESIAN_POINT('Ctrl Pts',(111.056138828999,14.3902031778294,31.));
#97174=CARTESIAN_POINT('Ctrl Pts',(111.056138828999,14.3902031778294,26.));
#97175=CARTESIAN_POINT('Ctrl Pts',(111.055435274693,14.3924507036097,31.));
#97176=CARTESIAN_POINT('Ctrl Pts',(111.055435274693,14.3924507036097,26.));
#97177=CARTESIAN_POINT('',(111.588247845187,13.7895999261044,31.));
#97178=CARTESIAN_POINT('Ctrl Pts',(111.055435274693,14.3924507036097,31.));
#97179=CARTESIAN_POINT('Ctrl Pts',(111.056138828999,14.3902031778294,31.));
#97180=CARTESIAN_POINT('Ctrl Pts',(111.057664061419,14.3855792208451,31.));
#97181=CARTESIAN_POINT('Ctrl Pts',(111.060306283432,14.3782565643212,31.));
#97182=CARTESIAN_POINT('Ctrl Pts',(111.064539259202,14.3677182209748,31.));
#97183=CARTESIAN_POINT('Ctrl Pts',(111.07101716314,14.3532574284428,31.));
#97184=CARTESIAN_POINT('Ctrl Pts',(111.078678375617,14.3375342353121,31.));
#97185=CARTESIAN_POINT('Ctrl Pts',(111.087506711152,14.3206092292363,31.));
#97186=CARTESIAN_POINT('Ctrl Pts',(111.097464566465,14.3025969156895,31.));
#97187=CARTESIAN_POINT('Ctrl Pts',(111.108490994798,14.2836686506361,31.));
#97188=CARTESIAN_POINT('Ctrl Pts',(111.120514421203,14.2640211918315,31.));
#97189=CARTESIAN_POINT('Ctrl Pts',(111.133462520623,14.2438514914768,31.));
#97190=CARTESIAN_POINT('Ctrl Pts',(111.14727205821,14.2233316663202,31.));
#97191=CARTESIAN_POINT('Ctrl Pts',(111.161900815541,14.2025779775787,31.));
#97192=CARTESIAN_POINT('Ctrl Pts',(111.177330271158,14.1816440780432,31.));
#97193=CARTESIAN_POINT('Ctrl Pts',(111.193556777481,14.1605444661444,31.));
#97194=CARTESIAN_POINT('Ctrl Pts',(111.210585385968,14.1392705460289,31.));
#97195=CARTESIAN_POINT('Ctrl Pts',(111.228423068787,14.1178081861225,31.));
#97196=CARTESIAN_POINT('Ctrl Pts',(111.24707067242,14.0961578383154,31.));
#97197=CARTESIAN_POINT('Ctrl Pts',(111.266520462056,14.0743413028629,31.));
#97198=CARTESIAN_POINT('Ctrl Pts',(111.286760291356,14.052392594348,31.));
#97199=CARTESIAN_POINT('Ctrl Pts',(111.307775912141,14.0303529759501,31.));
#97200=CARTESIAN_POINT('Ctrl Pts',(111.329553671008,14.0082647457932,31.));
#97201=CARTESIAN_POINT('Ctrl Pts',(111.352083296364,13.9861647449775,31.));
#97202=CARTESIAN_POINT('Ctrl Pts',(111.375358986128,13.9640809956577,31.));
#97203=CARTESIAN_POINT('Ctrl Pts',(111.399377689205,13.9420348180159,31.));
#97204=CARTESIAN_POINT('Ctrl Pts',(111.424137889235,13.9200415849572,31.));
#97205=CARTESIAN_POINT('Ctrl Pts',(111.44963814143,13.8981119641531,31.));
#97206=CARTESIAN_POINT('Ctrl Pts',(111.475875310414,13.8762529259845,31.));
#97207=CARTESIAN_POINT('Ctrl Pts',(111.502843526855,13.8544687325429,31.));
#97208=CARTESIAN_POINT('Ctrl Pts',(111.530536039611,13.8327615614272,31.));
#97209=CARTESIAN_POINT('Ctrl Pts',(111.553264364073,13.8154580515946,31.));
#97210=CARTESIAN_POINT('Ctrl Pts',(111.570631528299,13.80251540703,31.));
#97211=CARTESIAN_POINT('Ctrl Pts',(111.582352010706,13.7939024994014,31.));
#97212=CARTESIAN_POINT('Ctrl Pts',(111.588247845187,13.7895999261044,31.));
#97213=CARTESIAN_POINT('',(111.588247845187,13.7895999261044,26.));
#97214=CARTESIAN_POINT('Ctrl Pts',(111.588247845187,13.7895999261044,26.));
#97215=CARTESIAN_POINT('Ctrl Pts',(111.582352010706,13.7939024994014,26.));
#97216=CARTESIAN_POINT('Ctrl Pts',(111.570631528299,13.80251540703,26.));
#97217=CARTESIAN_POINT('Ctrl Pts',(111.553264364073,13.8154580515946,26.));
#97218=CARTESIAN_POINT('Ctrl Pts',(111.530536039611,13.8327615614272,26.));
#97219=CARTESIAN_POINT('Ctrl Pts',(111.502843526855,13.8544687325429,26.));
#97220=CARTESIAN_POINT('Ctrl Pts',(111.475875310414,13.8762529259845,26.));
#97221=CARTESIAN_POINT('Ctrl Pts',(111.44963814143,13.8981119641531,26.));
#97222=CARTESIAN_POINT('Ctrl Pts',(111.424137889235,13.9200415849572,26.));
#97223=CARTESIAN_POINT('Ctrl Pts',(111.399377689205,13.9420348180159,26.));
#97224=CARTESIAN_POINT('Ctrl Pts',(111.375358986128,13.9640809956577,26.));
#97225=CARTESIAN_POINT('Ctrl Pts',(111.352083296364,13.9861647449775,26.));
#97226=CARTESIAN_POINT('Ctrl Pts',(111.329553671008,14.0082647457932,26.));
#97227=CARTESIAN_POINT('Ctrl Pts',(111.307775912141,14.0303529759501,26.));
#97228=CARTESIAN_POINT('Ctrl Pts',(111.286760291356,14.052392594348,26.));
#97229=CARTESIAN_POINT('Ctrl Pts',(111.266520462056,14.0743413028629,26.));
#97230=CARTESIAN_POINT('Ctrl Pts',(111.24707067242,14.0961578383154,26.));
#97231=CARTESIAN_POINT('Ctrl Pts',(111.228423068787,14.1178081861225,26.));
#97232=CARTESIAN_POINT('Ctrl Pts',(111.210585385968,14.1392705460289,26.));
#97233=CARTESIAN_POINT('Ctrl Pts',(111.193556777481,14.1605444661444,26.));
#97234=CARTESIAN_POINT('Ctrl Pts',(111.177330271158,14.1816440780432,26.));
#97235=CARTESIAN_POINT('Ctrl Pts',(111.161900815541,14.2025779775787,26.));
#97236=CARTESIAN_POINT('Ctrl Pts',(111.14727205821,14.2233316663202,26.));
#97237=CARTESIAN_POINT('Ctrl Pts',(111.133462520623,14.2438514914768,26.));
#97238=CARTESIAN_POINT('Ctrl Pts',(111.120514421203,14.2640211918315,26.));
#97239=CARTESIAN_POINT('Ctrl Pts',(111.108490994798,14.2836686506361,26.));
#97240=CARTESIAN_POINT('Ctrl Pts',(111.097464566465,14.3025969156895,26.));
#97241=CARTESIAN_POINT('Ctrl Pts',(111.087506711152,14.3206092292363,26.));
#97242=CARTESIAN_POINT('Ctrl Pts',(111.078678375617,14.3375342353121,26.));
#97243=CARTESIAN_POINT('Ctrl Pts',(111.07101716314,14.3532574284428,26.));
#97244=CARTESIAN_POINT('Ctrl Pts',(111.064539259202,14.3677182209748,26.));
#97245=CARTESIAN_POINT('Ctrl Pts',(111.060306283432,14.3782565643212,26.));
#97246=CARTESIAN_POINT('Ctrl Pts',(111.057664061419,14.3855792208451,26.));
#97247=CARTESIAN_POINT('Ctrl Pts',(111.056138828999,14.3902031778294,26.));
#97248=CARTESIAN_POINT('Ctrl Pts',(111.055435274693,14.3924507036097,26.));
#97249=CARTESIAN_POINT('',(111.588247845187,13.7895999261044,31.));
#97250=CARTESIAN_POINT('Origin',(109.999999999999,18.0000000000028,31.));
#97251=CARTESIAN_POINT('',(111.854141622223,13.8997367347037,31.));
#97252=CARTESIAN_POINT('Origin',(109.999999999999,18.0000000000028,31.));
#97253=CARTESIAN_POINT('',(111.854141622223,13.8997367347037,26.));
#97254=CARTESIAN_POINT('Origin',(109.999999999999,18.0000000000028,26.));
#97255=CARTESIAN_POINT('',(111.854141622223,13.8997367347037,31.));
#97256=CARTESIAN_POINT('Ctrl Pts',(111.804617131104,14.702771989219,31.));
#97257=CARTESIAN_POINT('Ctrl Pts',(111.804617131104,14.702771989219,26.));
#97258=CARTESIAN_POINT('Ctrl Pts',(111.805708883808,14.7006852604798,31.));
#97259=CARTESIAN_POINT('Ctrl Pts',(111.805708883808,14.7006852604798,26.));
#97260=CARTESIAN_POINT('Ctrl Pts',(111.807900012971,14.6963371269573,31.));
#97261=CARTESIAN_POINT('Ctrl Pts',(111.807900012971,14.6963371269573,26.));
#97262=CARTESIAN_POINT('Ctrl Pts',(111.811209579963,14.6892908937737,31.));
#97263=CARTESIAN_POINT('Ctrl Pts',(111.811209579963,14.6892908937737,26.));
#97264=CARTESIAN_POINT('Ctrl Pts',(111.815668148138,14.6788459938606,31.));
#97265=CARTESIAN_POINT('Ctrl Pts',(111.815668148138,14.6788459938606,26.));
#97266=CARTESIAN_POINT('Ctrl Pts',(111.82131290279,14.6640400995954,31.));
#97267=CARTESIAN_POINT('Ctrl Pts',(111.82131290279,14.6640400995954,26.));
#97268=CARTESIAN_POINT('Ctrl Pts',(111.827013583967,14.6475048278114,31.));
#97269=CARTESIAN_POINT('Ctrl Pts',(111.827013583967,14.6475048278114,26.));
#97270=CARTESIAN_POINT('Ctrl Pts',(111.832738794595,14.6292944653143,31.));
#97271=CARTESIAN_POINT('Ctrl Pts',(111.832738794595,14.6292944653143,26.));
#97272=CARTESIAN_POINT('Ctrl Pts',(111.838434156619,14.6095165692379,31.));
#97273=CARTESIAN_POINT('Ctrl Pts',(111.838434156619,14.6095165692379,26.));
#97274=CARTESIAN_POINT('Ctrl Pts',(111.844021598942,14.5883354024137,31.));
#97275=CARTESIAN_POINT('Ctrl Pts',(111.844021598942,14.5883354024137,26.));
#97276=CARTESIAN_POINT('Ctrl Pts',(111.849412603956,14.5659407047175,31.));
#97277=CARTESIAN_POINT('Ctrl Pts',(111.849412603956,14.5659407047175,26.));
#97278=CARTESIAN_POINT('Ctrl Pts',(111.85451904696,14.5425228839233,31.));
#97279=CARTESIAN_POINT('Ctrl Pts',(111.85451904696,14.5425228839233,26.));
#97280=CARTESIAN_POINT('Ctrl Pts',(111.859263936817,14.5182483587386,31.));
#97281=CARTESIAN_POINT('Ctrl Pts',(111.859263936817,14.5182483587386,26.));
#97282=CARTESIAN_POINT('Ctrl Pts',(111.863594917364,14.4932291911909,31.));
#97283=CARTESIAN_POINT('Ctrl Pts',(111.863594917364,14.4932291911909,26.));
#97284=CARTESIAN_POINT('Ctrl Pts',(111.867487146992,14.4675164161785,31.));
#97285=CARTESIAN_POINT('Ctrl Pts',(111.867487146992,14.4675164161785,26.));
#97286=CARTESIAN_POINT('Ctrl Pts',(111.870932952987,14.4411228648671,31.));
#97287=CARTESIAN_POINT('Ctrl Pts',(111.870932952987,14.4411228648671,26.));
#97288=CARTESIAN_POINT('Ctrl Pts',(111.873934841617,14.4140388871515,31.));
#97289=CARTESIAN_POINT('Ctrl Pts',(111.873934841617,14.4140388871515,26.));
#97290=CARTESIAN_POINT('Ctrl Pts',(111.876497875346,14.3862495604319,31.));
#97291=CARTESIAN_POINT('Ctrl Pts',(111.876497875346,14.3862495604319,26.));
#97292=CARTESIAN_POINT('Ctrl Pts',(111.878621136093,14.3577546056918,31.));
#97293=CARTESIAN_POINT('Ctrl Pts',(111.878621136093,14.3577546056918,26.));
#97294=CARTESIAN_POINT('Ctrl Pts',(111.880294678097,14.3285749073818,31.));
#97295=CARTESIAN_POINT('Ctrl Pts',(111.880294678097,14.3285749073818,26.));
#97296=CARTESIAN_POINT('Ctrl Pts',(111.881503038178,14.2987431062045,31.));
#97297=CARTESIAN_POINT('Ctrl Pts',(111.881503038178,14.2987431062045,26.));
#97298=CARTESIAN_POINT('Ctrl Pts',(111.882227113853,14.2682984546204,31.));
#97299=CARTESIAN_POINT('Ctrl Pts',(111.882227113853,14.2682984546204,26.));
#97300=CARTESIAN_POINT('Ctrl Pts',(111.882446650243,14.2372805163331,31.));
#97301=CARTESIAN_POINT('Ctrl Pts',(111.882446650243,14.2372805163331,26.));
#97302=CARTESIAN_POINT('Ctrl Pts',(111.882142859859,14.2057226050428,31.));
#97303=CARTESIAN_POINT('Ctrl Pts',(111.882142859859,14.2057226050428,26.));
#97304=CARTESIAN_POINT('Ctrl Pts',(111.881300030722,14.1736486380898,31.));
#97305=CARTESIAN_POINT('Ctrl Pts',(111.881300030722,14.1736486380898,26.));
#97306=CARTESIAN_POINT('Ctrl Pts',(111.879905244617,14.1410758485617,31.));
#97307=CARTESIAN_POINT('Ctrl Pts',(111.879905244617,14.1410758485617,26.));
#97308=CARTESIAN_POINT('Ctrl Pts',(111.877948703475,14.1080161789671,31.));
#97309=CARTESIAN_POINT('Ctrl Pts',(111.877948703475,14.1080161789671,26.));
#97310=CARTESIAN_POINT('Ctrl Pts',(111.87542388573,14.074478194107,31.));
#97311=CARTESIAN_POINT('Ctrl Pts',(111.87542388573,14.074478194107,26.));
#97312=CARTESIAN_POINT('Ctrl Pts',(111.872328079638,14.0404690398371,31.));
#97313=CARTESIAN_POINT('Ctrl Pts',(111.872328079638,14.0404690398371,26.));
#97314=CARTESIAN_POINT('Ctrl Pts',(111.868662421724,14.0059958801699,31.));
#97315=CARTESIAN_POINT('Ctrl Pts',(111.868662421724,14.0059958801699,26.));
#97316=CARTESIAN_POINT('Ctrl Pts',(111.864430146015,13.9710650286956,31.));
#97317=CARTESIAN_POINT('Ctrl Pts',(111.864430146015,13.9710650286956,26.));
#97318=CARTESIAN_POINT('Ctrl Pts',(111.860594222842,13.9427582472186,31.));
#97319=CARTESIAN_POINT('Ctrl Pts',(111.860594222842,13.9427582472186,26.));
#97320=CARTESIAN_POINT('Ctrl Pts',(111.857465615073,13.9213259759228,31.));
#97321=CARTESIAN_POINT('Ctrl Pts',(111.857465615073,13.9213259759228,26.));
#97322=CARTESIAN_POINT('Ctrl Pts',(111.85526822796,13.9069480979796,31.));
#97323=CARTESIAN_POINT('Ctrl Pts',(111.85526822796,13.9069480979796,26.));
#97324=CARTESIAN_POINT('Ctrl Pts',(111.854141622223,13.8997367347037,31.));
#97325=CARTESIAN_POINT('Ctrl Pts',(111.854141622223,13.8997367347037,26.));
#97326=CARTESIAN_POINT('Ctrl Pts',(111.804617131104,14.702771989219,31.));
#97327=CARTESIAN_POINT('Ctrl Pts',(111.805708883808,14.7006852604798,31.));
#97328=CARTESIAN_POINT('Ctrl Pts',(111.807900012971,14.6963371269573,31.));
#97329=CARTESIAN_POINT('Ctrl Pts',(111.811209579963,14.6892908937737,31.));
#97330=CARTESIAN_POINT('Ctrl Pts',(111.815668148138,14.6788459938606,31.));
#97331=CARTESIAN_POINT('Ctrl Pts',(111.82131290279,14.6640400995954,31.));
#97332=CARTESIAN_POINT('Ctrl Pts',(111.827013583967,14.6475048278114,31.));
#97333=CARTESIAN_POINT('Ctrl Pts',(111.832738794595,14.6292944653143,31.));
#97334=CARTESIAN_POINT('Ctrl Pts',(111.838434156619,14.6095165692379,31.));
#97335=CARTESIAN_POINT('Ctrl Pts',(111.844021598942,14.5883354024137,31.));
#97336=CARTESIAN_POINT('Ctrl Pts',(111.849412603956,14.5659407047175,31.));
#97337=CARTESIAN_POINT('Ctrl Pts',(111.85451904696,14.5425228839233,31.));
#97338=CARTESIAN_POINT('Ctrl Pts',(111.859263936817,14.5182483587386,31.));
#97339=CARTESIAN_POINT('Ctrl Pts',(111.863594917364,14.4932291911909,31.));
#97340=CARTESIAN_POINT('Ctrl Pts',(111.867487146992,14.4675164161785,31.));
#97341=CARTESIAN_POINT('Ctrl Pts',(111.870932952987,14.4411228648671,31.));
#97342=CARTESIAN_POINT('Ctrl Pts',(111.873934841617,14.4140388871515,31.));
#97343=CARTESIAN_POINT('Ctrl Pts',(111.876497875346,14.3862495604319,31.));
#97344=CARTESIAN_POINT('Ctrl Pts',(111.878621136093,14.3577546056918,31.));
#97345=CARTESIAN_POINT('Ctrl Pts',(111.880294678097,14.3285749073818,31.));
#97346=CARTESIAN_POINT('Ctrl Pts',(111.881503038178,14.2987431062045,31.));
#97347=CARTESIAN_POINT('Ctrl Pts',(111.882227113853,14.2682984546204,31.));
#97348=CARTESIAN_POINT('Ctrl Pts',(111.882446650243,14.2372805163331,31.));
#97349=CARTESIAN_POINT('Ctrl Pts',(111.882142859859,14.2057226050428,31.));
#97350=CARTESIAN_POINT('Ctrl Pts',(111.881300030722,14.1736486380898,31.));
#97351=CARTESIAN_POINT('Ctrl Pts',(111.879905244617,14.1410758485617,31.));
#97352=CARTESIAN_POINT('Ctrl Pts',(111.877948703475,14.1080161789671,31.));
#97353=CARTESIAN_POINT('Ctrl Pts',(111.87542388573,14.074478194107,31.));
#97354=CARTESIAN_POINT('Ctrl Pts',(111.872328079638,14.0404690398371,31.));
#97355=CARTESIAN_POINT('Ctrl Pts',(111.868662421724,14.0059958801699,31.));
#97356=CARTESIAN_POINT('Ctrl Pts',(111.864430146015,13.9710650286956,31.));
#97357=CARTESIAN_POINT('Ctrl Pts',(111.860594222842,13.9427582472186,31.));
#97358=CARTESIAN_POINT('Ctrl Pts',(111.857465615073,13.9213259759228,31.));
#97359=CARTESIAN_POINT('Ctrl Pts',(111.85526822796,13.9069480979796,31.));
#97360=CARTESIAN_POINT('Ctrl Pts',(111.854141622223,13.8997367347037,31.));
#97361=CARTESIAN_POINT('Ctrl Pts',(111.804617131104,14.702771989219,26.));
#97362=CARTESIAN_POINT('Ctrl Pts',(111.805708883808,14.7006852604798,26.));
#97363=CARTESIAN_POINT('Ctrl Pts',(111.807900012971,14.6963371269573,26.));
#97364=CARTESIAN_POINT('Ctrl Pts',(111.811209579963,14.6892908937737,26.));
#97365=CARTESIAN_POINT('Ctrl Pts',(111.815668148138,14.6788459938606,26.));
#97366=CARTESIAN_POINT('Ctrl Pts',(111.82131290279,14.6640400995954,26.));
#97367=CARTESIAN_POINT('Ctrl Pts',(111.827013583967,14.6475048278114,26.));
#97368=CARTESIAN_POINT('Ctrl Pts',(111.832738794595,14.6292944653143,26.));
#97369=CARTESIAN_POINT('Ctrl Pts',(111.838434156619,14.6095165692379,26.));
#97370=CARTESIAN_POINT('Ctrl Pts',(111.844021598942,14.5883354024137,26.));
#97371=CARTESIAN_POINT('Ctrl Pts',(111.849412603956,14.5659407047175,26.));
#97372=CARTESIAN_POINT('Ctrl Pts',(111.85451904696,14.5425228839233,26.));
#97373=CARTESIAN_POINT('Ctrl Pts',(111.859263936817,14.5182483587386,26.));
#97374=CARTESIAN_POINT('Ctrl Pts',(111.863594917364,14.4932291911909,26.));
#97375=CARTESIAN_POINT('Ctrl Pts',(111.867487146992,14.4675164161785,26.));
#97376=CARTESIAN_POINT('Ctrl Pts',(111.870932952987,14.4411228648671,26.));
#97377=CARTESIAN_POINT('Ctrl Pts',(111.873934841617,14.4140388871515,26.));
#97378=CARTESIAN_POINT('Ctrl Pts',(111.876497875346,14.3862495604319,26.));
#97379=CARTESIAN_POINT('Ctrl Pts',(111.878621136093,14.3577546056918,26.));
#97380=CARTESIAN_POINT('Ctrl Pts',(111.880294678097,14.3285749073818,26.));
#97381=CARTESIAN_POINT('Ctrl Pts',(111.881503038178,14.2987431062045,26.));
#97382=CARTESIAN_POINT('Ctrl Pts',(111.882227113853,14.2682984546204,26.));
#97383=CARTESIAN_POINT('Ctrl Pts',(111.882446650243,14.2372805163331,26.));
#97384=CARTESIAN_POINT('Ctrl Pts',(111.882142859859,14.2057226050428,26.));
#97385=CARTESIAN_POINT('Ctrl Pts',(111.881300030722,14.1736486380898,26.));
#97386=CARTESIAN_POINT('Ctrl Pts',(111.879905244617,14.1410758485617,26.));
#97387=CARTESIAN_POINT('Ctrl Pts',(111.877948703475,14.1080161789671,26.));
#97388=CARTESIAN_POINT('Ctrl Pts',(111.87542388573,14.074478194107,26.));
#97389=CARTESIAN_POINT('Ctrl Pts',(111.872328079638,14.0404690398371,26.));
#97390=CARTESIAN_POINT('Ctrl Pts',(111.868662421724,14.0059958801699,26.));
#97391=CARTESIAN_POINT('Ctrl Pts',(111.864430146015,13.9710650286956,26.));
#97392=CARTESIAN_POINT('Ctrl Pts',(111.860594222842,13.9427582472186,26.));
#97393=CARTESIAN_POINT('Ctrl Pts',(111.857465615073,13.9213259759228,26.));
#97394=CARTESIAN_POINT('Ctrl Pts',(111.85526822796,13.9069480979796,26.));
#97395=CARTESIAN_POINT('Ctrl Pts',(111.854141622223,13.8997367347037,26.));
#97396=CARTESIAN_POINT('Origin',(111.474514194069,14.4402078348085,31.));
#97397=CARTESIAN_POINT('Origin',(109.59454570101,14.2631614489809,31.));
#97398=CARTESIAN_POINT('',(109.59454570101,14.2631614489809,26.));
#97399=CARTESIAN_POINT('',(109.652122916228,14.7938174514562,26.));
#97400=CARTESIAN_POINT('',(109.59454570101,14.2631614489809,31.));
#97401=CARTESIAN_POINT('',(109.59454570101,14.2631614489809,31.));
#97402=CARTESIAN_POINT('',(109.652122916228,14.7938174514562,31.));
#97403=CARTESIAN_POINT('Ctrl Pts',(109.856099324815,13.5023014112014,31.));
#97404=CARTESIAN_POINT('Ctrl Pts',(109.856099324815,13.5023014112014,26.));
#97405=CARTESIAN_POINT('Ctrl Pts',(109.852298807528,13.5085327087832,31.));
#97406=CARTESIAN_POINT('Ctrl Pts',(109.852298807528,13.5085327087832,26.));
#97407=CARTESIAN_POINT('Ctrl Pts',(109.844766510775,13.5209752322934,31.));
#97408=CARTESIAN_POINT('Ctrl Pts',(109.844766510775,13.5209752322934,26.));
#97409=CARTESIAN_POINT('Ctrl Pts',(109.833674278855,13.5395788027196,31.));
#97410=CARTESIAN_POINT('Ctrl Pts',(109.833674278855,13.5395788027196,26.));
#97411=CARTESIAN_POINT('Ctrl Pts',(109.819297811611,13.5642629145113,31.));
#97412=CARTESIAN_POINT('Ctrl Pts',(109.819297811611,13.5642629145113,26.));
#97413=CARTESIAN_POINT('Ctrl Pts',(109.802020240621,13.5949151914465,31.));
#97414=CARTESIAN_POINT('Ctrl Pts',(109.802020240621,13.5949151914465,26.));
#97415=CARTESIAN_POINT('Ctrl Pts',(109.785441307341,13.6253614515315,31.));
#97416=CARTESIAN_POINT('Ctrl Pts',(109.785441307341,13.6253614515315,26.));
#97417=CARTESIAN_POINT('Ctrl Pts',(109.76956641568,13.6555970993782,31.));
#97418=CARTESIAN_POINT('Ctrl Pts',(109.76956641568,13.6555970993782,26.));
#97419=CARTESIAN_POINT('Ctrl Pts',(109.754399357163,13.685615951231,31.));
#97420=CARTESIAN_POINT('Ctrl Pts',(109.754399357163,13.685615951231,26.));
#97421=CARTESIAN_POINT('Ctrl Pts',(109.73994036105,13.7154103674413,31.));
#97422=CARTESIAN_POINT('Ctrl Pts',(109.73994036105,13.7154103674413,26.));
#97423=CARTESIAN_POINT('Ctrl Pts',(109.72618667981,13.7449699394692,31.));
#97424=CARTESIAN_POINT('Ctrl Pts',(109.72618667981,13.7449699394692,26.));
#97425=CARTESIAN_POINT('Ctrl Pts',(109.713133831421,13.7742798843163,31.));
#97426=CARTESIAN_POINT('Ctrl Pts',(109.713133831421,13.7742798843163,26.));
#97427=CARTESIAN_POINT('Ctrl Pts',(109.700776475847,13.8033193370997,31.));
#97428=CARTESIAN_POINT('Ctrl Pts',(109.700776475847,13.8033193370997,26.));
#97429=CARTESIAN_POINT('Ctrl Pts',(109.689109249897,13.8320601883634,31.));
#97430=CARTESIAN_POINT('Ctrl Pts',(109.689109249897,13.8320601883634,26.));
#97431=CARTESIAN_POINT('Ctrl Pts',(109.678127544808,13.8604644706008,31.));
#97432=CARTESIAN_POINT('Ctrl Pts',(109.678127544808,13.8604644706008,26.));
#97433=CARTESIAN_POINT('Ctrl Pts',(109.667827787886,13.8884878805099,31.));
#97434=CARTESIAN_POINT('Ctrl Pts',(109.667827787886,13.8884878805099,26.));
#97435=CARTESIAN_POINT('Ctrl Pts',(109.658207351999,13.9160868433413,31.));
#97436=CARTESIAN_POINT('Ctrl Pts',(109.658207351999,13.9160868433413,26.));
#97437=CARTESIAN_POINT('Ctrl Pts',(109.649264442082,13.943225285516,31.));
#97438=CARTESIAN_POINT('Ctrl Pts',(109.649264442082,13.943225285516,26.));
#97439=CARTESIAN_POINT('Ctrl Pts',(109.640997861574,13.9698801062394,31.));
#97440=CARTESIAN_POINT('Ctrl Pts',(109.640997861574,13.9698801062394,26.));
#97441=CARTESIAN_POINT('Ctrl Pts',(109.633406655496,13.9960512119544,31.));
#97442=CARTESIAN_POINT('Ctrl Pts',(109.633406655496,13.9960512119544,26.));
#97443=CARTESIAN_POINT('Ctrl Pts',(109.626489790322,14.021754326667,31.));
#97444=CARTESIAN_POINT('Ctrl Pts',(109.626489790322,14.021754326667,26.));
#97445=CARTESIAN_POINT('Ctrl Pts',(109.620245888607,14.0469993250184,31.));
#97446=CARTESIAN_POINT('Ctrl Pts',(109.620245888607,14.0469993250184,26.));
#97447=CARTESIAN_POINT('Ctrl Pts',(109.614672771965,14.0717714163373,31.));
#97448=CARTESIAN_POINT('Ctrl Pts',(109.614672771965,14.0717714163373,26.));
#97449=CARTESIAN_POINT('Ctrl Pts',(109.609767019958,14.0960139440534,31.));
#97450=CARTESIAN_POINT('Ctrl Pts',(109.609767019958,14.0960139440534,26.));
#97451=CARTESIAN_POINT('Ctrl Pts',(109.60552314608,14.1196033405166,31.));
#97452=CARTESIAN_POINT('Ctrl Pts',(109.60552314608,14.1196033405166,26.));
#97453=CARTESIAN_POINT('Ctrl Pts',(109.601933705487,14.1423563916575,31.));
#97454=CARTESIAN_POINT('Ctrl Pts',(109.601933705487,14.1423563916575,26.));
#97455=CARTESIAN_POINT('Ctrl Pts',(109.598990147472,14.1640634597676,31.));
#97456=CARTESIAN_POINT('Ctrl Pts',(109.598990147472,14.1640634597676,26.));
#97457=CARTESIAN_POINT('Ctrl Pts',(109.596683302734,14.1845153738368,31.));
#97458=CARTESIAN_POINT('Ctrl Pts',(109.596683302734,14.1845153738368,26.));
#97459=CARTESIAN_POINT('Ctrl Pts',(109.595003903645,14.2035304982823,31.));
#97460=CARTESIAN_POINT('Ctrl Pts',(109.595003903645,14.2035304982823,26.));
#97461=CARTESIAN_POINT('Ctrl Pts',(109.593942871758,14.2209886536882,31.));
#97462=CARTESIAN_POINT('Ctrl Pts',(109.593942871758,14.2209886536882,26.));
#97463=CARTESIAN_POINT('Ctrl Pts',(109.593491974617,14.2368276704459,31.));
#97464=CARTESIAN_POINT('Ctrl Pts',(109.593491974617,14.2368276704459,26.));
#97465=CARTESIAN_POINT('Ctrl Pts',(109.593614064345,14.2481837198673,31.));
#97466=CARTESIAN_POINT('Ctrl Pts',(109.593614064345,14.2481837198673,26.));
#97467=CARTESIAN_POINT('Ctrl Pts',(109.593975228839,14.2559601069423,31.));
#97468=CARTESIAN_POINT('Ctrl Pts',(109.593975228839,14.2559601069423,26.));
#97469=CARTESIAN_POINT('Ctrl Pts',(109.594335609554,14.2608157673368,31.));
#97470=CARTESIAN_POINT('Ctrl Pts',(109.594335609554,14.2608157673368,26.));
#97471=CARTESIAN_POINT('Ctrl Pts',(109.59454570101,14.2631614489809,31.));
#97472=CARTESIAN_POINT('Ctrl Pts',(109.59454570101,14.2631614489809,26.));
#97473=CARTESIAN_POINT('',(109.856099324815,13.5023014112014,31.));
#97474=CARTESIAN_POINT('Ctrl Pts',(109.59454570101,14.2631614489809,31.));
#97475=CARTESIAN_POINT('Ctrl Pts',(109.594335609554,14.2608157673368,31.));
#97476=CARTESIAN_POINT('Ctrl Pts',(109.593975228839,14.2559601069423,31.));
#97477=CARTESIAN_POINT('Ctrl Pts',(109.593614064345,14.2481837198673,31.));
#97478=CARTESIAN_POINT('Ctrl Pts',(109.593491974617,14.2368276704459,31.));
#97479=CARTESIAN_POINT('Ctrl Pts',(109.593942871758,14.2209886536882,31.));
#97480=CARTESIAN_POINT('Ctrl Pts',(109.595003903645,14.2035304982823,31.));
#97481=CARTESIAN_POINT('Ctrl Pts',(109.596683302734,14.1845153738368,31.));
#97482=CARTESIAN_POINT('Ctrl Pts',(109.598990147472,14.1640634597676,31.));
#97483=CARTESIAN_POINT('Ctrl Pts',(109.601933705487,14.1423563916575,31.));
#97484=CARTESIAN_POINT('Ctrl Pts',(109.60552314608,14.1196033405166,31.));
#97485=CARTESIAN_POINT('Ctrl Pts',(109.609767019958,14.0960139440534,31.));
#97486=CARTESIAN_POINT('Ctrl Pts',(109.614672771965,14.0717714163373,31.));
#97487=CARTESIAN_POINT('Ctrl Pts',(109.620245888607,14.0469993250184,31.));
#97488=CARTESIAN_POINT('Ctrl Pts',(109.626489790322,14.021754326667,31.));
#97489=CARTESIAN_POINT('Ctrl Pts',(109.633406655496,13.9960512119544,31.));
#97490=CARTESIAN_POINT('Ctrl Pts',(109.640997861574,13.9698801062394,31.));
#97491=CARTESIAN_POINT('Ctrl Pts',(109.649264442082,13.943225285516,31.));
#97492=CARTESIAN_POINT('Ctrl Pts',(109.658207351999,13.9160868433413,31.));
#97493=CARTESIAN_POINT('Ctrl Pts',(109.667827787886,13.8884878805099,31.));
#97494=CARTESIAN_POINT('Ctrl Pts',(109.678127544808,13.8604644706008,31.));
#97495=CARTESIAN_POINT('Ctrl Pts',(109.689109249897,13.8320601883634,31.));
#97496=CARTESIAN_POINT('Ctrl Pts',(109.700776475847,13.8033193370997,31.));
#97497=CARTESIAN_POINT('Ctrl Pts',(109.713133831421,13.7742798843163,31.));
#97498=CARTESIAN_POINT('Ctrl Pts',(109.72618667981,13.7449699394692,31.));
#97499=CARTESIAN_POINT('Ctrl Pts',(109.73994036105,13.7154103674413,31.));
#97500=CARTESIAN_POINT('Ctrl Pts',(109.754399357163,13.685615951231,31.));
#97501=CARTESIAN_POINT('Ctrl Pts',(109.76956641568,13.6555970993782,31.));
#97502=CARTESIAN_POINT('Ctrl Pts',(109.785441307341,13.6253614515315,31.));
#97503=CARTESIAN_POINT('Ctrl Pts',(109.802020240621,13.5949151914465,31.));
#97504=CARTESIAN_POINT('Ctrl Pts',(109.819297811611,13.5642629145113,31.));
#97505=CARTESIAN_POINT('Ctrl Pts',(109.833674278855,13.5395788027196,31.));
#97506=CARTESIAN_POINT('Ctrl Pts',(109.844766510775,13.5209752322934,31.));
#97507=CARTESIAN_POINT('Ctrl Pts',(109.852298807528,13.5085327087832,31.));
#97508=CARTESIAN_POINT('Ctrl Pts',(109.856099324815,13.5023014112014,31.));
#97509=CARTESIAN_POINT('',(109.856099324815,13.5023014112014,26.));
#97510=CARTESIAN_POINT('Ctrl Pts',(109.856099324815,13.5023014112014,26.));
#97511=CARTESIAN_POINT('Ctrl Pts',(109.852298807528,13.5085327087832,26.));
#97512=CARTESIAN_POINT('Ctrl Pts',(109.844766510775,13.5209752322934,26.));
#97513=CARTESIAN_POINT('Ctrl Pts',(109.833674278855,13.5395788027196,26.));
#97514=CARTESIAN_POINT('Ctrl Pts',(109.819297811611,13.5642629145113,26.));
#97515=CARTESIAN_POINT('Ctrl Pts',(109.802020240621,13.5949151914465,26.));
#97516=CARTESIAN_POINT('Ctrl Pts',(109.785441307341,13.6253614515315,26.));
#97517=CARTESIAN_POINT('Ctrl Pts',(109.76956641568,13.6555970993782,26.));
#97518=CARTESIAN_POINT('Ctrl Pts',(109.754399357163,13.685615951231,26.));
#97519=CARTESIAN_POINT('Ctrl Pts',(109.73994036105,13.7154103674413,26.));
#97520=CARTESIAN_POINT('Ctrl Pts',(109.72618667981,13.7449699394692,26.));
#97521=CARTESIAN_POINT('Ctrl Pts',(109.713133831421,13.7742798843163,26.));
#97522=CARTESIAN_POINT('Ctrl Pts',(109.700776475847,13.8033193370997,26.));
#97523=CARTESIAN_POINT('Ctrl Pts',(109.689109249897,13.8320601883634,26.));
#97524=CARTESIAN_POINT('Ctrl Pts',(109.678127544808,13.8604644706008,26.));
#97525=CARTESIAN_POINT('Ctrl Pts',(109.667827787886,13.8884878805099,26.));
#97526=CARTESIAN_POINT('Ctrl Pts',(109.658207351999,13.9160868433413,26.));
#97527=CARTESIAN_POINT('Ctrl Pts',(109.649264442082,13.943225285516,26.));
#97528=CARTESIAN_POINT('Ctrl Pts',(109.640997861574,13.9698801062394,26.));
#97529=CARTESIAN_POINT('Ctrl Pts',(109.633406655496,13.9960512119544,26.));
#97530=CARTESIAN_POINT('Ctrl Pts',(109.626489790322,14.021754326667,26.));
#97531=CARTESIAN_POINT('Ctrl Pts',(109.620245888607,14.0469993250184,26.));
#97532=CARTESIAN_POINT('Ctrl Pts',(109.614672771965,14.0717714163373,26.));
#97533=CARTESIAN_POINT('Ctrl Pts',(109.609767019958,14.0960139440534,26.));
#97534=CARTESIAN_POINT('Ctrl Pts',(109.60552314608,14.1196033405166,26.));
#97535=CARTESIAN_POINT('Ctrl Pts',(109.601933705487,14.1423563916575,26.));
#97536=CARTESIAN_POINT('Ctrl Pts',(109.598990147472,14.1640634597676,26.));
#97537=CARTESIAN_POINT('Ctrl Pts',(109.596683302734,14.1845153738368,26.));
#97538=CARTESIAN_POINT('Ctrl Pts',(109.595003903645,14.2035304982823,26.));
#97539=CARTESIAN_POINT('Ctrl Pts',(109.593942871758,14.2209886536882,26.));
#97540=CARTESIAN_POINT('Ctrl Pts',(109.593491974617,14.2368276704459,26.));
#97541=CARTESIAN_POINT('Ctrl Pts',(109.593614064345,14.2481837198673,26.));
#97542=CARTESIAN_POINT('Ctrl Pts',(109.593975228839,14.2559601069423,26.));
#97543=CARTESIAN_POINT('Ctrl Pts',(109.594335609554,14.2608157673368,26.));
#97544=CARTESIAN_POINT('Ctrl Pts',(109.59454570101,14.2631614489809,26.));
#97545=CARTESIAN_POINT('',(109.856099324815,13.5023014112014,31.));
#97546=CARTESIAN_POINT('Origin',(110.,18.000000000003,31.));
#97547=CARTESIAN_POINT('',(110.143900675185,13.5023014112014,31.));
#97548=CARTESIAN_POINT('Origin',(110.,18.000000000003,31.));
#97549=CARTESIAN_POINT('',(110.143900675185,13.5023014112014,26.));
#97550=CARTESIAN_POINT('Origin',(110.,18.000000000003,26.));
#97551=CARTESIAN_POINT('',(110.143900675185,13.5023014112014,31.));
#97552=CARTESIAN_POINT('Ctrl Pts',(110.40545429899,14.2631614489809,31.));
#97553=CARTESIAN_POINT('Ctrl Pts',(110.40545429899,14.2631614489809,26.));
#97554=CARTESIAN_POINT('Ctrl Pts',(110.405664390452,14.2608157673365,31.));
#97555=CARTESIAN_POINT('Ctrl Pts',(110.405664390452,14.2608157673365,26.));
#97556=CARTESIAN_POINT('Ctrl Pts',(110.406024771178,14.2559601069417,31.));
#97557=CARTESIAN_POINT('Ctrl Pts',(110.406024771178,14.2559601069417,26.));
#97558=CARTESIAN_POINT('Ctrl Pts',(110.406385935683,14.2481837198662,31.));
#97559=CARTESIAN_POINT('Ctrl Pts',(110.406385935683,14.2481837198662,26.));
#97560=CARTESIAN_POINT('Ctrl Pts',(110.406508025415,14.2368276704446,31.));
#97561=CARTESIAN_POINT('Ctrl Pts',(110.406508025415,14.2368276704446,26.));
#97562=CARTESIAN_POINT('Ctrl Pts',(110.406057128268,14.2209886536872,31.));
#97563=CARTESIAN_POINT('Ctrl Pts',(110.406057128268,14.2209886536872,26.));
#97564=CARTESIAN_POINT('Ctrl Pts',(110.404996096367,14.2035304982819,31.));
#97565=CARTESIAN_POINT('Ctrl Pts',(110.404996096367,14.2035304982819,26.));
#97566=CARTESIAN_POINT('Ctrl Pts',(110.40331669726,14.184515373837,31.));
#97567=CARTESIAN_POINT('Ctrl Pts',(110.40331669726,14.184515373837,26.));
#97568=CARTESIAN_POINT('Ctrl Pts',(110.401009852508,14.1640634597682,31.));
#97569=CARTESIAN_POINT('Ctrl Pts',(110.401009852508,14.1640634597682,26.));
#97570=CARTESIAN_POINT('Ctrl Pts',(110.398066294489,14.1423563916581,31.));
#97571=CARTESIAN_POINT('Ctrl Pts',(110.398066294489,14.1423563916581,26.));
#97572=CARTESIAN_POINT('Ctrl Pts',(110.3944768539,14.1196033405171,31.));
#97573=CARTESIAN_POINT('Ctrl Pts',(110.3944768539,14.1196033405171,26.));
#97574=CARTESIAN_POINT('Ctrl Pts',(110.390232980035,14.0960139440535,31.));
#97575=CARTESIAN_POINT('Ctrl Pts',(110.390232980035,14.0960139440535,26.));
#97576=CARTESIAN_POINT('Ctrl Pts',(110.385327228041,14.0717714163371,31.));
#97577=CARTESIAN_POINT('Ctrl Pts',(110.385327228041,14.0717714163371,26.));
#97578=CARTESIAN_POINT('Ctrl Pts',(110.379754111412,14.0469993250182,31.));
#97579=CARTESIAN_POINT('Ctrl Pts',(110.379754111412,14.0469993250182,26.));
#97580=CARTESIAN_POINT('Ctrl Pts',(110.373510209703,14.0217543266667,31.));
#97581=CARTESIAN_POINT('Ctrl Pts',(110.373510209703,14.0217543266667,26.));
#97582=CARTESIAN_POINT('Ctrl Pts',(110.366593344528,13.9960512119543,31.));
#97583=CARTESIAN_POINT('Ctrl Pts',(110.366593344528,13.9960512119543,26.));
#97584=CARTESIAN_POINT('Ctrl Pts',(110.359002138437,13.9698801062394,31.));
#97585=CARTESIAN_POINT('Ctrl Pts',(110.359002138437,13.9698801062394,26.));
#97586=CARTESIAN_POINT('Ctrl Pts',(110.350735557909,13.943225285516,31.));
#97587=CARTESIAN_POINT('Ctrl Pts',(110.350735557909,13.943225285516,26.));
#97588=CARTESIAN_POINT('Ctrl Pts',(110.34179264797,13.9160868433413,31.));
#97589=CARTESIAN_POINT('Ctrl Pts',(110.34179264797,13.9160868433413,26.));
#97590=CARTESIAN_POINT('Ctrl Pts',(110.332172212069,13.8884878805099,31.));
#97591=CARTESIAN_POINT('Ctrl Pts',(110.332172212069,13.8884878805099,26.));
#97592=CARTESIAN_POINT('Ctrl Pts',(110.321872455148,13.8604644706007,31.));
#97593=CARTESIAN_POINT('Ctrl Pts',(110.321872455148,13.8604644706007,26.));
#97594=CARTESIAN_POINT('Ctrl Pts',(110.310890750078,13.8320601883633,31.));
#97595=CARTESIAN_POINT('Ctrl Pts',(110.310890750078,13.8320601883633,26.));
#97596=CARTESIAN_POINT('Ctrl Pts',(110.299223524167,13.8033193370998,31.));
#97597=CARTESIAN_POINT('Ctrl Pts',(110.299223524167,13.8033193370998,26.));
#97598=CARTESIAN_POINT('Ctrl Pts',(110.286866168639,13.7742798843164,31.));
#97599=CARTESIAN_POINT('Ctrl Pts',(110.286866168639,13.7742798843164,26.));
#97600=CARTESIAN_POINT('Ctrl Pts',(110.273813320286,13.7449699394693,31.));
#97601=CARTESIAN_POINT('Ctrl Pts',(110.273813320286,13.7449699394693,26.));
#97602=CARTESIAN_POINT('Ctrl Pts',(110.260059639053,13.7154103674415,31.));
#97603=CARTESIAN_POINT('Ctrl Pts',(110.260059639053,13.7154103674415,26.));
#97604=CARTESIAN_POINT('Ctrl Pts',(110.245600642905,13.6856159512311,31.));
#97605=CARTESIAN_POINT('Ctrl Pts',(110.245600642905,13.6856159512311,26.));
#97606=CARTESIAN_POINT('Ctrl Pts',(110.230433584305,13.6555970993781,31.));
#97607=CARTESIAN_POINT('Ctrl Pts',(110.230433584305,13.6555970993781,26.));
#97608=CARTESIAN_POINT('Ctrl Pts',(110.214558692533,13.6253614515313,31.));
#97609=CARTESIAN_POINT('Ctrl Pts',(110.214558692533,13.6253614515313,26.));
#97610=CARTESIAN_POINT('Ctrl Pts',(110.197979759147,13.5949151914461,31.));
#97611=CARTESIAN_POINT('Ctrl Pts',(110.197979759147,13.5949151914461,26.));
#97612=CARTESIAN_POINT('Ctrl Pts',(110.180702188106,13.564262914511,31.));
#97613=CARTESIAN_POINT('Ctrl Pts',(110.180702188106,13.564262914511,26.));
#97614=CARTESIAN_POINT('Ctrl Pts',(110.166325720903,13.5395788027193,31.));
#97615=CARTESIAN_POINT('Ctrl Pts',(110.166325720903,13.5395788027193,26.));
#97616=CARTESIAN_POINT('Ctrl Pts',(110.155233489078,13.5209752322933,31.));
#97617=CARTESIAN_POINT('Ctrl Pts',(110.155233489078,13.5209752322933,26.));
#97618=CARTESIAN_POINT('Ctrl Pts',(110.147701192417,13.5085327087831,31.));
#97619=CARTESIAN_POINT('Ctrl Pts',(110.147701192417,13.5085327087831,26.));
#97620=CARTESIAN_POINT('Ctrl Pts',(110.143900675185,13.5023014112014,31.));
#97621=CARTESIAN_POINT('Ctrl Pts',(110.143900675185,13.5023014112014,26.));
#97622=CARTESIAN_POINT('',(110.40545429899,14.2631614489809,31.));
#97623=CARTESIAN_POINT('Ctrl Pts',(110.40545429899,14.2631614489809,31.));
#97624=CARTESIAN_POINT('Ctrl Pts',(110.405664390452,14.2608157673365,31.));
#97625=CARTESIAN_POINT('Ctrl Pts',(110.406024771178,14.2559601069417,31.));
#97626=CARTESIAN_POINT('Ctrl Pts',(110.406385935683,14.2481837198662,31.));
#97627=CARTESIAN_POINT('Ctrl Pts',(110.406508025415,14.2368276704446,31.));
#97628=CARTESIAN_POINT('Ctrl Pts',(110.406057128268,14.2209886536872,31.));
#97629=CARTESIAN_POINT('Ctrl Pts',(110.404996096367,14.2035304982819,31.));
#97630=CARTESIAN_POINT('Ctrl Pts',(110.40331669726,14.184515373837,31.));
#97631=CARTESIAN_POINT('Ctrl Pts',(110.401009852508,14.1640634597682,31.));
#97632=CARTESIAN_POINT('Ctrl Pts',(110.398066294489,14.1423563916581,31.));
#97633=CARTESIAN_POINT('Ctrl Pts',(110.3944768539,14.1196033405171,31.));
#97634=CARTESIAN_POINT('Ctrl Pts',(110.390232980035,14.0960139440535,31.));
#97635=CARTESIAN_POINT('Ctrl Pts',(110.385327228041,14.0717714163371,31.));
#97636=CARTESIAN_POINT('Ctrl Pts',(110.379754111412,14.0469993250182,31.));
#97637=CARTESIAN_POINT('Ctrl Pts',(110.373510209703,14.0217543266667,31.));
#97638=CARTESIAN_POINT('Ctrl Pts',(110.366593344528,13.9960512119543,31.));
#97639=CARTESIAN_POINT('Ctrl Pts',(110.359002138437,13.9698801062394,31.));
#97640=CARTESIAN_POINT('Ctrl Pts',(110.350735557909,13.943225285516,31.));
#97641=CARTESIAN_POINT('Ctrl Pts',(110.34179264797,13.9160868433413,31.));
#97642=CARTESIAN_POINT('Ctrl Pts',(110.332172212069,13.8884878805099,31.));
#97643=CARTESIAN_POINT('Ctrl Pts',(110.321872455148,13.8604644706007,31.));
#97644=CARTESIAN_POINT('Ctrl Pts',(110.310890750078,13.8320601883633,31.));
#97645=CARTESIAN_POINT('Ctrl Pts',(110.299223524167,13.8033193370998,31.));
#97646=CARTESIAN_POINT('Ctrl Pts',(110.286866168639,13.7742798843164,31.));
#97647=CARTESIAN_POINT('Ctrl Pts',(110.273813320286,13.7449699394693,31.));
#97648=CARTESIAN_POINT('Ctrl Pts',(110.260059639053,13.7154103674415,31.));
#97649=CARTESIAN_POINT('Ctrl Pts',(110.245600642905,13.6856159512311,31.));
#97650=CARTESIAN_POINT('Ctrl Pts',(110.230433584305,13.6555970993781,31.));
#97651=CARTESIAN_POINT('Ctrl Pts',(110.214558692533,13.6253614515313,31.));
#97652=CARTESIAN_POINT('Ctrl Pts',(110.197979759147,13.5949151914461,31.));
#97653=CARTESIAN_POINT('Ctrl Pts',(110.180702188106,13.564262914511,31.));
#97654=CARTESIAN_POINT('Ctrl Pts',(110.166325720903,13.5395788027193,31.));
#97655=CARTESIAN_POINT('Ctrl Pts',(110.155233489078,13.5209752322933,31.));
#97656=CARTESIAN_POINT('Ctrl Pts',(110.147701192417,13.5085327087831,31.));
#97657=CARTESIAN_POINT('Ctrl Pts',(110.143900675185,13.5023014112014,31.));
#97658=CARTESIAN_POINT('',(110.40545429899,14.2631614489809,26.));
#97659=CARTESIAN_POINT('Ctrl Pts',(110.40545429899,14.2631614489809,26.));
#97660=CARTESIAN_POINT('Ctrl Pts',(110.405664390452,14.2608157673365,26.));
#97661=CARTESIAN_POINT('Ctrl Pts',(110.406024771178,14.2559601069417,26.));
#97662=CARTESIAN_POINT('Ctrl Pts',(110.406385935683,14.2481837198662,26.));
#97663=CARTESIAN_POINT('Ctrl Pts',(110.406508025415,14.2368276704446,26.));
#97664=CARTESIAN_POINT('Ctrl Pts',(110.406057128268,14.2209886536872,26.));
#97665=CARTESIAN_POINT('Ctrl Pts',(110.404996096367,14.2035304982819,26.));
#97666=CARTESIAN_POINT('Ctrl Pts',(110.40331669726,14.184515373837,26.));
#97667=CARTESIAN_POINT('Ctrl Pts',(110.401009852508,14.1640634597682,26.));
#97668=CARTESIAN_POINT('Ctrl Pts',(110.398066294489,14.1423563916581,26.));
#97669=CARTESIAN_POINT('Ctrl Pts',(110.3944768539,14.1196033405171,26.));
#97670=CARTESIAN_POINT('Ctrl Pts',(110.390232980035,14.0960139440535,26.));
#97671=CARTESIAN_POINT('Ctrl Pts',(110.385327228041,14.0717714163371,26.));
#97672=CARTESIAN_POINT('Ctrl Pts',(110.379754111412,14.0469993250182,26.));
#97673=CARTESIAN_POINT('Ctrl Pts',(110.373510209703,14.0217543266667,26.));
#97674=CARTESIAN_POINT('Ctrl Pts',(110.366593344528,13.9960512119543,26.));
#97675=CARTESIAN_POINT('Ctrl Pts',(110.359002138437,13.9698801062394,26.));
#97676=CARTESIAN_POINT('Ctrl Pts',(110.350735557909,13.943225285516,26.));
#97677=CARTESIAN_POINT('Ctrl Pts',(110.34179264797,13.9160868433413,26.));
#97678=CARTESIAN_POINT('Ctrl Pts',(110.332172212069,13.8884878805099,26.));
#97679=CARTESIAN_POINT('Ctrl Pts',(110.321872455148,13.8604644706007,26.));
#97680=CARTESIAN_POINT('Ctrl Pts',(110.310890750078,13.8320601883633,26.));
#97681=CARTESIAN_POINT('Ctrl Pts',(110.299223524167,13.8033193370998,26.));
#97682=CARTESIAN_POINT('Ctrl Pts',(110.286866168639,13.7742798843164,26.));
#97683=CARTESIAN_POINT('Ctrl Pts',(110.273813320286,13.7449699394693,26.));
#97684=CARTESIAN_POINT('Ctrl Pts',(110.260059639053,13.7154103674415,26.));
#97685=CARTESIAN_POINT('Ctrl Pts',(110.245600642905,13.6856159512311,26.));
#97686=CARTESIAN_POINT('Ctrl Pts',(110.230433584305,13.6555970993781,26.));
#97687=CARTESIAN_POINT('Ctrl Pts',(110.214558692533,13.6253614515313,26.));
#97688=CARTESIAN_POINT('Ctrl Pts',(110.197979759147,13.5949151914461,26.));
#97689=CARTESIAN_POINT('Ctrl Pts',(110.180702188106,13.564262914511,26.));
#97690=CARTESIAN_POINT('Ctrl Pts',(110.166325720903,13.5395788027193,26.));
#97691=CARTESIAN_POINT('Ctrl Pts',(110.155233489078,13.5209752322933,26.));
#97692=CARTESIAN_POINT('Ctrl Pts',(110.147701192417,13.5085327087831,26.));
#97693=CARTESIAN_POINT('Ctrl Pts',(110.143900675185,13.5023014112014,26.));
#97694=CARTESIAN_POINT('',(110.40545429899,14.2631614489809,31.));
#97695=CARTESIAN_POINT('Origin',(110.347877083772,14.7938174514562,31.));
#97696=CARTESIAN_POINT('',(110.40545429899,14.2631614489809,31.));
#97697=CARTESIAN_POINT('',(110.40545429899,14.2631614489809,26.));
#97698=CARTESIAN_POINT('Origin',(110.000000000016,14.1469087257281,31.));
#97699=CARTESIAN_POINT('Origin',(110.,18.,30.4));
#97700=CARTESIAN_POINT('',(107.5,18.,34.8));
#97701=CARTESIAN_POINT('Origin',(110.,18.,34.8));
#97702=CARTESIAN_POINT('',(107.5,18.,26.));
#97703=CARTESIAN_POINT('',(107.5,18.,30.4));
#97704=CARTESIAN_POINT('Origin',(110.,18.,26.));
#97705=CARTESIAN_POINT('Origin',(113.375,18.,26.));
#97706=CARTESIAN_POINT('Origin',(114.5,18.,31.8));
#97707=CARTESIAN_POINT('',(105.5,18.,31.8));
#97708=CARTESIAN_POINT('Origin',(110.,18.,31.8));
#97709=CARTESIAN_POINT('Origin',(110.,18.,33.15));
#97710=CARTESIAN_POINT('',(105.5,18.,34.5));
#97711=CARTESIAN_POINT('Origin',(110.,18.,34.5));
#97712=CARTESIAN_POINT('',(105.5,18.,33.15));
#97713=CARTESIAN_POINT('Origin',(110.,18.,34.65));
#97714=CARTESIAN_POINT('',(105.8,18.,34.8));
#97715=CARTESIAN_POINT('Origin',(110.,18.,34.8));
#97716=CARTESIAN_POINT('',(105.65,18.,34.65));
#97717=CARTESIAN_POINT('Origin',(112.5,18.,34.8));
#97718=CARTESIAN_POINT('',(0.,0.,0.));
#97719=CARTESIAN_POINT('Origin',(110.,20.,63.));
#97720=CARTESIAN_POINT('',(108.483391942524,20.,62.6800000000001));
#97721=CARTESIAN_POINT('',(108.483391942524,20.,63.3199999999999));
#97722=CARTESIAN_POINT('',(108.483391942524,20.,64.05));
#97723=CARTESIAN_POINT('',(108.45,20.,63.));
#97724=CARTESIAN_POINT('Origin',(110.,20.,63.));
#97725=CARTESIAN_POINT('Origin',(110.,20.,63.));
#97726=CARTESIAN_POINT('Origin',(110.,24.,63.));
#97727=CARTESIAN_POINT('',(110.,24.,64.55));
#97728=CARTESIAN_POINT('',(108.45,23.7963350489771,63.));
#97729=CARTESIAN_POINT('Ctrl Pts',(110.,24.,64.55));
#97730=CARTESIAN_POINT('Ctrl Pts',(109.804434914878,24.,64.55));
#97731=CARTESIAN_POINT('Ctrl Pts',(109.596431057671,23.9894828311411,64.5107353587906));
#97732=CARTESIAN_POINT('Ctrl Pts',(109.214794582034,23.9514893035012,64.3522727655961));
#97733=CARTESIAN_POINT('Ctrl Pts',(109.041091716494,23.9245204206378,64.233122738172));
#97734=CARTESIAN_POINT('Ctrl Pts',(108.766855310829,23.8735685672227,63.9588863325073));
#97735=CARTESIAN_POINT('Ctrl Pts',(108.647722381438,23.8461953948893,63.7851925753203));
#97736=CARTESIAN_POINT('Ctrl Pts',(108.489272290211,23.8072676307453,63.4035885188397));
#97737=CARTESIAN_POINT('Ctrl Pts',(108.45,23.7963350489771,63.19559639528));
#97738=CARTESIAN_POINT('Ctrl Pts',(108.45,23.7963350489771,63.));
#97739=CARTESIAN_POINT('',(110.,24.,61.45));
#97740=CARTESIAN_POINT('Ctrl Pts',(110.,24.,61.45));
#97741=CARTESIAN_POINT('Ctrl Pts',(110.195565085122,24.,61.45));
#97742=CARTESIAN_POINT('Ctrl Pts',(110.403568942329,23.9894828311411,61.4892646412094));
#97743=CARTESIAN_POINT('Ctrl Pts',(110.785205417966,23.9514893035012,61.6477272344039));
#97744=CARTESIAN_POINT('Ctrl Pts',(110.958908283506,23.9245204206378,61.766877261828));
#97745=CARTESIAN_POINT('Ctrl Pts',(111.233144689171,23.8735685672227,62.0411136674927));
#97746=CARTESIAN_POINT('Ctrl Pts',(111.352277618562,23.8461953948893,62.2148074246797));
#97747=CARTESIAN_POINT('Ctrl Pts',(111.510727709789,23.8072676307453,62.5964114811603));
#97748=CARTESIAN_POINT('Ctrl Pts',(111.55,23.7963350489771,62.80440360472));
#97749=CARTESIAN_POINT('Ctrl Pts',(111.55,23.7963350489771,63.));
#97750=CARTESIAN_POINT('Ctrl Pts',(111.55,23.7963350489771,63.19559639528));
#97751=CARTESIAN_POINT('Ctrl Pts',(111.510727709789,23.8072676307453,63.4035885188397));
#97752=CARTESIAN_POINT('Ctrl Pts',(111.352277618562,23.8461953948893,63.7851925753203));
#97753=CARTESIAN_POINT('Ctrl Pts',(111.233144689171,23.8735685672227,63.9588863325073));
#97754=CARTESIAN_POINT('Ctrl Pts',(110.958908283506,23.9245204206378,64.233122738172));
#97755=CARTESIAN_POINT('Ctrl Pts',(110.785205417966,23.9514893035012,64.3522727655961));
#97756=CARTESIAN_POINT('Ctrl Pts',(110.403568942329,23.9894828311411,64.5107353587906));
#97757=CARTESIAN_POINT('Ctrl Pts',(110.195565085122,24.,64.55));
#97758=CARTESIAN_POINT('Ctrl Pts',(110.,24.,64.55));
#97759=CARTESIAN_POINT('Ctrl Pts',(108.45,23.7963350489771,63.));
#97760=CARTESIAN_POINT('Ctrl Pts',(108.45,23.7963350489771,62.80440360472));
#97761=CARTESIAN_POINT('Ctrl Pts',(108.489272290211,23.8072676307453,62.5964114811603));
#97762=CARTESIAN_POINT('Ctrl Pts',(108.647722381438,23.8461953948893,62.2148074246797));
#97763=CARTESIAN_POINT('Ctrl Pts',(108.766855310829,23.8735685672227,62.0411136674927));
#97764=CARTESIAN_POINT('Ctrl Pts',(109.041091716494,23.9245204206378,61.766877261828));
#97765=CARTESIAN_POINT('Ctrl Pts',(109.214794582034,23.9514893035012,61.6477272344039));
#97766=CARTESIAN_POINT('Ctrl Pts',(109.596431057671,23.9894828311411,61.4892646412094));
#97767=CARTESIAN_POINT('Ctrl Pts',(109.804434914878,24.,61.45));
#97768=CARTESIAN_POINT('Ctrl Pts',(110.,24.,61.45));
#97769=CARTESIAN_POINT('',(108.45,24.,63.));
#97770=CARTESIAN_POINT('',(111.516608057476,20.,62.6800000000001));
#97771=CARTESIAN_POINT('Ctrl Pts',(111.516608057476,20.,62.6800000000001));
#97772=CARTESIAN_POINT('Ctrl Pts',(111.496300804331,20.0153990718724,62.5837558007975));
#97773=CARTESIAN_POINT('Ctrl Pts',(111.466684099523,20.0374168042622,62.4892051739527));
#97774=CARTESIAN_POINT('Ctrl Pts',(111.34901672214,20.118881048826,62.2094698392625));
#97775=CARTESIAN_POINT('Ctrl Pts',(111.231113753811,20.1924895398432,62.0390827321322));
#97776=CARTESIAN_POINT('Ctrl Pts',(110.961922515843,20.3231491933349,61.7698914941652));
#97777=CARTESIAN_POINT('Ctrl Pts',(110.791272112782,20.3900618513488,61.6512969408763));
#97778=CARTESIAN_POINT('Ctrl Pts',(110.410718369409,20.4839117719612,61.4912183468773));
#97779=CARTESIAN_POINT('Ctrl Pts',(110.200494469465,20.51,61.45));
#97780=CARTESIAN_POINT('Ctrl Pts',(109.799505530535,20.51,61.45));
#97781=CARTESIAN_POINT('Ctrl Pts',(109.589281630591,20.4839117719612,61.4912183468773));
#97782=CARTESIAN_POINT('Ctrl Pts',(109.208727887218,20.3900618513488,61.6512969408763));
#97783=CARTESIAN_POINT('Ctrl Pts',(109.038077484157,20.3231491933349,61.7698914941652));
#97784=CARTESIAN_POINT('Ctrl Pts',(108.768886246189,20.1924895398432,62.0390827321322));
#97785=CARTESIAN_POINT('Ctrl Pts',(108.65098327786,20.118881048826,62.2094698392625));
#97786=CARTESIAN_POINT('Ctrl Pts',(108.533315900477,20.0374168042622,62.4892051739528));
#97787=CARTESIAN_POINT('Ctrl Pts',(108.503699195669,20.0153990718724,62.5837558007975));
#97788=CARTESIAN_POINT('Ctrl Pts',(108.483391942524,20.,62.6800000000001));
#97789=CARTESIAN_POINT('',(111.516608057476,20.,63.3199999999999));
#97790=CARTESIAN_POINT('Origin',(110.,20.,63.));
#97791=CARTESIAN_POINT('Ctrl Pts',(108.483391942524,20.,63.3199999999999));
#97792=CARTESIAN_POINT('Ctrl Pts',(108.503699195669,20.0153990718724,63.4162441992025));
#97793=CARTESIAN_POINT('Ctrl Pts',(108.533315900477,20.0374168042622,63.5107948260473));
#97794=CARTESIAN_POINT('Ctrl Pts',(108.65098327786,20.118881048826,63.7905301607375));
#97795=CARTESIAN_POINT('Ctrl Pts',(108.768886246189,20.1924895398432,63.9609172678678));
#97796=CARTESIAN_POINT('Ctrl Pts',(109.038077484157,20.3231491933349,64.2301085058348));
#97797=CARTESIAN_POINT('Ctrl Pts',(109.208727887218,20.3900618513488,64.3487030591237));
#97798=CARTESIAN_POINT('Ctrl Pts',(109.589281630591,20.4839117719612,64.5087816531227));
#97799=CARTESIAN_POINT('Ctrl Pts',(109.799505530535,20.51,64.55));
#97800=CARTESIAN_POINT('Ctrl Pts',(110.200494469465,20.51,64.55));
#97801=CARTESIAN_POINT('Ctrl Pts',(110.410718369409,20.4839117719612,64.5087816531227));
#97802=CARTESIAN_POINT('Ctrl Pts',(110.791272112782,20.3900618513488,64.3487030591237));
#97803=CARTESIAN_POINT('Ctrl Pts',(110.961922515843,20.3231491933349,64.2301085058348));
#97804=CARTESIAN_POINT('Ctrl Pts',(111.231113753811,20.1924895398432,63.9609172678678));
#97805=CARTESIAN_POINT('Ctrl Pts',(111.34901672214,20.118881048826,63.7905301607375));
#97806=CARTESIAN_POINT('Ctrl Pts',(111.466684099523,20.0374168042622,63.5107948260473));
#97807=CARTESIAN_POINT('Ctrl Pts',(111.496300804331,20.0153990718724,63.4162441992025));
#97808=CARTESIAN_POINT('Ctrl Pts',(111.516608057476,20.,63.3199999999999));
#97809=CARTESIAN_POINT('Origin',(110.,20.,63.));
#97810=CARTESIAN_POINT('',(111.516608057476,20.,64.05));
#97811=CARTESIAN_POINT('Origin',(119.481808069713,16.4982291356138,81.));
#97812=CARTESIAN_POINT('',(119.481808069713,16.4982291356138,80.6));
#97813=CARTESIAN_POINT('',(119.913569220132,16.6880757195422,80.2));
#97814=CARTESIAN_POINT('Ctrl Pts',(119.481808069713,16.4982291356138,80.6));
#97815=CARTESIAN_POINT('Ctrl Pts',(119.693282918898,16.5912152175378,80.4056749851136));
#97816=CARTESIAN_POINT('Ctrl Pts',(119.913569220132,16.6880757195422,80.2));
#97817=CARTESIAN_POINT('',(119.481808069713,16.4982291356138,66.4));
#97818=CARTESIAN_POINT('',(119.481808069713,16.4982291356138,81.));
#97819=CARTESIAN_POINT('',(119.913569220132,16.6880757195422,66.8));
#97820=CARTESIAN_POINT('Ctrl Pts',(119.913569220132,16.6880757195423,66.8));
#97821=CARTESIAN_POINT('Ctrl Pts',(119.693282918896,16.5912152175369,66.5943250148847));
#97822=CARTESIAN_POINT('Ctrl Pts',(119.481808069713,16.4982291356138,66.4));
#97823=CARTESIAN_POINT('',(119.913569220132,16.6880757195422,73.5));
#97824=CARTESIAN_POINT('Origin',(120.102794398862,15.9442652568178,81.));
#97825=CARTESIAN_POINT('',(119.833771504544,16.184252771882,80.2));
#97826=CARTESIAN_POINT('Ctrl Pts',(119.833771504544,16.184252771882,80.2));
#97827=CARTESIAN_POINT('Ctrl Pts',(119.654198323508,16.3444447941938,80.4056749851128));
#97828=CARTESIAN_POINT('Ctrl Pts',(119.481808069713,16.4982291356138,80.6));
#97829=CARTESIAN_POINT('',(119.833771504544,16.184252771882,66.8));
#97830=CARTESIAN_POINT('',(119.833771504544,16.184252771882,73.5));
#97831=CARTESIAN_POINT('Ctrl Pts',(119.481808069713,16.4982291356138,66.4));
#97832=CARTESIAN_POINT('Ctrl Pts',(119.654198323507,16.344444794195,66.5943250148856));
#97833=CARTESIAN_POINT('Ctrl Pts',(119.833771504544,16.184252771882,66.8));
#97834=CARTESIAN_POINT('Origin',(110.,18.,66.4));
#97835=CARTESIAN_POINT('',(119.58628655942,15.1534037868576,66.8));
#97836=CARTESIAN_POINT('Origin',(110.,18.,66.8));
#97837=CARTESIAN_POINT('',(119.130142556433,15.0334368540005,66.4));
#97838=CARTESIAN_POINT('Ctrl Pts',(119.58628655942,15.1534037868576,66.8));
#97839=CARTESIAN_POINT('Ctrl Pts',(119.353560027287,15.0921961680536,66.5943250148888));
#97840=CARTESIAN_POINT('Ctrl Pts',(119.130142556433,15.0334368540005,66.4));
#97841=CARTESIAN_POINT('',(119.428656012836,14.6682668486787,66.8));
#97842=CARTESIAN_POINT('Ctrl Pts',(119.130142556433,15.0334368540005,66.4));
#97843=CARTESIAN_POINT('Ctrl Pts',(119.276353228958,14.8545780758826,66.5943250148879));
#97844=CARTESIAN_POINT('Ctrl Pts',(119.428656012836,14.6682668486787,66.8));
#97845=CARTESIAN_POINT('',(119.022957708555,13.6888245002517,66.8));
#97846=CARTESIAN_POINT('Origin',(110.,18.,66.8));
#97847=CARTESIAN_POINT('',(118.553662632208,13.6416912025004,66.4));
#97848=CARTESIAN_POINT('Ctrl Pts',(119.022957708555,13.6888245002517,66.8));
#97849=CARTESIAN_POINT('Ctrl Pts',(118.783521445114,13.6647768993582,66.5943250148874));
#97850=CARTESIAN_POINT('Ctrl Pts',(118.553662632208,13.6416912025004,66.4));
#97851=CARTESIAN_POINT('',(118.791375718177,13.2343192530493,66.8));
#97852=CARTESIAN_POINT('Ctrl Pts',(118.553662632208,13.6416912025004,66.4));
#97853=CARTESIAN_POINT('Ctrl Pts',(118.670093531459,13.4421620844006,66.594325014888));
#97854=CARTESIAN_POINT('Ctrl Pts',(118.791375718177,13.2343192530493,66.8));
#97855=CARTESIAN_POINT('',(118.237453693425,12.3304006624208,66.8));
#97856=CARTESIAN_POINT('Origin',(110.,18.,66.8));
#97857=CARTESIAN_POINT('',(117.766563145999,12.3572615779923,66.4));
#97858=CARTESIAN_POINT('Ctrl Pts',(118.237453693425,12.3304006624208,66.8));
#97859=CARTESIAN_POINT('Ctrl Pts',(117.997203414127,12.3441052111817,66.5943250148877));
#97860=CARTESIAN_POINT('Ctrl Pts',(117.766563145999,12.3572615779923,66.4));
#97861=CARTESIAN_POINT('',(117.937622576432,11.9177185337975,66.8));
#97862=CARTESIAN_POINT('Ctrl Pts',(117.766563145999,12.3572615779923,66.4));
#97863=CARTESIAN_POINT('Ctrl Pts',(117.850347356823,12.1419751889999,66.5943250148858));
#97864=CARTESIAN_POINT('Ctrl Pts',(117.937622576432,11.9177185337974,66.8));
#97865=CARTESIAN_POINT('',(117.249116229822,11.1115811766025,66.8));
#97866=CARTESIAN_POINT('Origin',(110.,18.,66.8));
#97867=CARTESIAN_POINT('',(116.788225099391,11.2117749006091,66.4));
#97868=CARTESIAN_POINT('Ctrl Pts',(117.249116229822,11.1115811766024,66.8));
#97869=CARTESIAN_POINT('Ctrl Pts',(117.01396769389,11.1627004235442,66.5943250148884));
#97870=CARTESIAN_POINT('Ctrl Pts',(116.788225099391,11.2117749006091,66.4));
#97871=CARTESIAN_POINT('',(116.888418823398,10.7508837701784,66.8));
#97872=CARTESIAN_POINT('Ctrl Pts',(116.788225099391,11.2117749006091,66.4));
#97873=CARTESIAN_POINT('Ctrl Pts',(116.837299576456,10.9860323061102,66.5943250148886));
#97874=CARTESIAN_POINT('Ctrl Pts',(116.888418823398,10.7508837701784,66.8));
#97875=CARTESIAN_POINT('',(116.082281466203,10.0623774235676,66.8));
#97876=CARTESIAN_POINT('Origin',(110.,18.,66.8));
#97877=CARTESIAN_POINT('',(115.642738422008,10.2334368540005,66.4));
#97878=CARTESIAN_POINT('Ctrl Pts',(116.082281466203,10.0623774235676,66.8));
#97879=CARTESIAN_POINT('Ctrl Pts',(115.858024811002,10.1496526431758,66.5943250148877));
#97880=CARTESIAN_POINT('Ctrl Pts',(115.642738422008,10.2334368540005,66.4));
#97881=CARTESIAN_POINT('',(115.669599337579,9.762546306575,66.8));
#97882=CARTESIAN_POINT('Ctrl Pts',(115.642738422008,10.2334368540005,66.4));
#97883=CARTESIAN_POINT('Ctrl Pts',(115.655894788818,10.0027965858723,66.5943250148879));
#97884=CARTESIAN_POINT('Ctrl Pts',(115.669599337579,9.76254630657496,66.8));
#97885=CARTESIAN_POINT('',(114.765680746951,9.20862428182348,66.8));
#97886=CARTESIAN_POINT('Origin',(110.,18.,66.8));
#97887=CARTESIAN_POINT('',(114.3583087975,9.44633736779169,66.4));
#97888=CARTESIAN_POINT('Ctrl Pts',(114.765680746951,9.20862428182346,66.8));
#97889=CARTESIAN_POINT('Ctrl Pts',(114.557837915599,9.32990646854147,66.5943250148875));
#97890=CARTESIAN_POINT('Ctrl Pts',(114.3583087975,9.44633736779169,66.4));
#97891=CARTESIAN_POINT('',(114.311175499748,8.97704229144512,66.8));
#97892=CARTESIAN_POINT('Ctrl Pts',(114.3583087975,9.44633736779169,66.4));
#97893=CARTESIAN_POINT('Ctrl Pts',(114.335223100642,9.21647855488602,66.5943250148877));
#97894=CARTESIAN_POINT('Ctrl Pts',(114.311175499748,8.97704229144508,66.8));
#97895=CARTESIAN_POINT('',(113.331733151321,8.57134398716408,66.8));
#97896=CARTESIAN_POINT('Origin',(110.,18.,66.8));
#97897=CARTESIAN_POINT('',(112.966563146,8.86985744356654,66.4));
#97898=CARTESIAN_POINT('Ctrl Pts',(113.331733151321,8.57134398716406,66.8));
#97899=CARTESIAN_POINT('Ctrl Pts',(113.145421924117,8.72364677104231,66.5943250148875));
#97900=CARTESIAN_POINT('Ctrl Pts',(112.966563146,8.86985744356654,66.4));
#97901=CARTESIAN_POINT('',(112.846596213142,8.41371344057965,66.8));
#97902=CARTESIAN_POINT('Ctrl Pts',(112.966563146,8.86985744356654,66.4));
#97903=CARTESIAN_POINT('Ctrl Pts',(112.907803831947,8.64643997271467,66.5943250148877));
#97904=CARTESIAN_POINT('Ctrl Pts',(112.846596213142,8.41371344057961,66.8));
#97905=CARTESIAN_POINT('',(111.815747228118,8.16622849545598,66.8));
#97906=CARTESIAN_POINT('Origin',(110.,18.,66.8));
#97907=CARTESIAN_POINT('',(111.501770864386,8.51819193028669,66.4));
#97908=CARTESIAN_POINT('Ctrl Pts',(111.815747228118,8.16622849545595,66.8));
#97909=CARTESIAN_POINT('Ctrl Pts',(111.655555205807,8.34580167649132,66.5943250148875));
#97910=CARTESIAN_POINT('Ctrl Pts',(111.501770864386,8.51819193028669,66.4));
#97911=CARTESIAN_POINT('',(111.311924280458,8.08643077986816,66.8));
#97912=CARTESIAN_POINT('Ctrl Pts',(111.501770864386,8.51819193028669,66.4));
#97913=CARTESIAN_POINT('Ctrl Pts',(111.408784782462,8.3067170811009,66.5943250148878));
#97914=CARTESIAN_POINT('Ctrl Pts',(111.311924280458,8.08643077986812,66.8));
#97915=CARTESIAN_POINT('',(110.255051582039,8.00325309460625,66.8));
#97916=CARTESIAN_POINT('Origin',(110.,18.,66.8));
#97917=CARTESIAN_POINT('',(110.,8.40000000000002,66.4));
#97918=CARTESIAN_POINT('Ctrl Pts',(110.255051582039,8.00325309460621,66.8));
#97919=CARTESIAN_POINT('Ctrl Pts',(110.124923223856,8.20567498511282,66.5943250148871));
#97920=CARTESIAN_POINT('Ctrl Pts',(110.,8.40000000000002,66.4));
#97921=CARTESIAN_POINT('',(109.744948417961,8.00325309460625,66.8));
#97922=CARTESIAN_POINT('Ctrl Pts',(110.,8.40000000000002,66.4));
#97923=CARTESIAN_POINT('Ctrl Pts',(109.875076776144,8.20567498511234,66.5943250148876));
#97924=CARTESIAN_POINT('Ctrl Pts',(109.744948417961,8.00325309460622,66.8));
#97925=CARTESIAN_POINT('',(108.688075719542,8.08643077986816,66.8));
#97926=CARTESIAN_POINT('Origin',(110.,18.,66.8));
#97927=CARTESIAN_POINT('',(108.498229135614,8.51819193028669,66.4));
#97928=CARTESIAN_POINT('Ctrl Pts',(108.688075719542,8.08643077986812,66.8));
#97929=CARTESIAN_POINT('Ctrl Pts',(108.591215217539,8.30671708110066,66.594325014888));
#97930=CARTESIAN_POINT('Ctrl Pts',(108.498229135614,8.51819193028669,66.4));
#97931=CARTESIAN_POINT('',(108.184252771882,8.16622849545598,66.8));
#97932=CARTESIAN_POINT('Ctrl Pts',(108.498229135614,8.51819193028669,66.4));
#97933=CARTESIAN_POINT('Ctrl Pts',(108.344444794193,8.34580167649075,66.5943250148882));
#97934=CARTESIAN_POINT('Ctrl Pts',(108.184252771882,8.16622849545595,66.8));
#97935=CARTESIAN_POINT('',(107.153403786858,8.41371344057964,66.8));
#97936=CARTESIAN_POINT('Origin',(110.,18.,66.8));
#97937=CARTESIAN_POINT('',(107.033436854001,8.86985744356654,66.4));
#97938=CARTESIAN_POINT('Ctrl Pts',(107.153403786858,8.4137134405796,66.8));
#97939=CARTESIAN_POINT('Ctrl Pts',(107.092196168053,8.64643997271458,66.5943250148878));
#97940=CARTESIAN_POINT('Ctrl Pts',(107.033436854001,8.86985744356654,66.4));
#97941=CARTESIAN_POINT('',(106.668266848679,8.57134398716408,66.8));
#97942=CARTESIAN_POINT('Ctrl Pts',(107.033436854,8.86985744356654,66.4));
#97943=CARTESIAN_POINT('Ctrl Pts',(106.854578075882,8.72364677104165,66.5943250148884));
#97944=CARTESIAN_POINT('Ctrl Pts',(106.668266848679,8.57134398716406,66.8));
#97945=CARTESIAN_POINT('',(105.688824500252,8.97704229144512,66.8));
#97946=CARTESIAN_POINT('Origin',(110.,18.,66.8));
#97947=CARTESIAN_POINT('',(105.6416912025,9.44633736779169,66.4));
#97948=CARTESIAN_POINT('Ctrl Pts',(105.688824500252,8.97704229144508,66.8));
#97949=CARTESIAN_POINT('Ctrl Pts',(105.664776899358,9.21647855488566,66.5943250148881));
#97950=CARTESIAN_POINT('Ctrl Pts',(105.6416912025,9.44633736779169,66.4));
#97951=CARTESIAN_POINT('',(105.234319253049,9.20862428182348,66.8));
#97952=CARTESIAN_POINT('Ctrl Pts',(105.6416912025,9.44633736779169,66.4));
#97953=CARTESIAN_POINT('Ctrl Pts',(105.442162084401,9.32990646854146,66.5943250148875));
#97954=CARTESIAN_POINT('Ctrl Pts',(105.234319253049,9.20862428182346,66.8));
#97955=CARTESIAN_POINT('',(104.330400662421,9.76254630657499,66.8));
#97956=CARTESIAN_POINT('Origin',(110.,18.,66.8));
#97957=CARTESIAN_POINT('',(104.357261577992,10.2334368540005,66.4));
#97958=CARTESIAN_POINT('Ctrl Pts',(104.330400662421,9.76254630657495,66.8));
#97959=CARTESIAN_POINT('Ctrl Pts',(104.344105211182,10.0027965858725,66.5943250148878));
#97960=CARTESIAN_POINT('Ctrl Pts',(104.357261577992,10.2334368540005,66.4));
#97961=CARTESIAN_POINT('',(103.917718533797,10.0623774235676,66.8));
#97962=CARTESIAN_POINT('Ctrl Pts',(104.357261577992,10.2334368540005,66.4));
#97963=CARTESIAN_POINT('Ctrl Pts',(104.141975188998,10.1496526431757,66.5943250148879));
#97964=CARTESIAN_POINT('Ctrl Pts',(103.917718533797,10.0623774235676,66.8));
#97965=CARTESIAN_POINT('',(103.111581176602,10.7508837701784,66.8));
#97966=CARTESIAN_POINT('Origin',(110.,18.,66.8));
#97967=CARTESIAN_POINT('',(103.211774900609,11.2117749006092,66.4));
#97968=CARTESIAN_POINT('Ctrl Pts',(103.111581176602,10.7508837701784,66.8));
#97969=CARTESIAN_POINT('Ctrl Pts',(103.162700423544,10.9860323061103,66.5943250148885));
#97970=CARTESIAN_POINT('Ctrl Pts',(103.211774900609,11.2117749006092,66.4));
#97971=CARTESIAN_POINT('',(102.750883770178,11.1115811766025,66.8));
#97972=CARTESIAN_POINT('Ctrl Pts',(103.211774900609,11.2117749006092,66.4));
#97973=CARTESIAN_POINT('Ctrl Pts',(102.98603230611,11.1627004235442,66.5943250148886));
#97974=CARTESIAN_POINT('Ctrl Pts',(102.750883770178,11.1115811766025,66.8));
#97975=CARTESIAN_POINT('',(102.062377423568,11.9177185337975,66.8));
#97976=CARTESIAN_POINT('Origin',(110.,18.,66.8));
#97977=CARTESIAN_POINT('',(102.233436854001,12.3572615779923,66.4));
#97978=CARTESIAN_POINT('Ctrl Pts',(102.062377423568,11.9177185337975,66.8));
#97979=CARTESIAN_POINT('Ctrl Pts',(102.149652643177,12.1419751889998,66.5943250148859));
#97980=CARTESIAN_POINT('Ctrl Pts',(102.233436854001,12.3572615779923,66.4));
#97981=CARTESIAN_POINT('',(101.762546306575,12.3304006624208,66.8));
#97982=CARTESIAN_POINT('Ctrl Pts',(102.233436854001,12.3572615779923,66.4));
#97983=CARTESIAN_POINT('Ctrl Pts',(102.002796585872,12.3441052111816,66.594325014888));
#97984=CARTESIAN_POINT('Ctrl Pts',(101.762546306575,12.3304006624208,66.8));
#97985=CARTESIAN_POINT('',(101.208624281823,13.2343192530494,66.8));
#97986=CARTESIAN_POINT('Origin',(110.,18.,66.8));
#97987=CARTESIAN_POINT('',(101.446337367792,13.6416912025004,66.3999999999999));
#97988=CARTESIAN_POINT('Ctrl Pts',(101.208624281823,13.2343192530493,66.8));
#97989=CARTESIAN_POINT('Ctrl Pts',(101.329906468541,13.442162084401,66.5943250148876));
#97990=CARTESIAN_POINT('Ctrl Pts',(101.446337367792,13.6416912025004,66.3999999999999));
#97991=CARTESIAN_POINT('',(100.977042291445,13.6888245002517,66.8));
#97992=CARTESIAN_POINT('Ctrl Pts',(101.446337367792,13.6416912025004,66.3999999999999));
#97993=CARTESIAN_POINT('Ctrl Pts',(101.216478554886,13.6647768993583,66.5943250148876));
#97994=CARTESIAN_POINT('Ctrl Pts',(100.977042291445,13.6888245002517,66.8));
#97995=CARTESIAN_POINT('',(100.571343987164,14.6682668486788,66.8));
#97996=CARTESIAN_POINT('Origin',(110.,18.,66.8));
#97997=CARTESIAN_POINT('',(100.869857443567,15.0334368540005,66.4));
#97998=CARTESIAN_POINT('Ctrl Pts',(100.571343987164,14.6682668486787,66.8));
#97999=CARTESIAN_POINT('Ctrl Pts',(100.723646771041,14.8545780758816,66.5943250148891));
#98000=CARTESIAN_POINT('Ctrl Pts',(100.869857443567,15.0334368540005,66.4));
#98001=CARTESIAN_POINT('',(100.41371344058,15.1534037868576,66.8));
#98002=CARTESIAN_POINT('Ctrl Pts',(100.869857443567,15.0334368540005,66.4));
#98003=CARTESIAN_POINT('Ctrl Pts',(100.646439972716,15.092196168053,66.5943250148869));
#98004=CARTESIAN_POINT('Ctrl Pts',(100.41371344058,15.1534037868576,66.8));
#98005=CARTESIAN_POINT('',(100.166228495456,16.184252771882,66.8));
#98006=CARTESIAN_POINT('Origin',(110.,18.,66.8));
#98007=CARTESIAN_POINT('',(100.518191930287,16.4982291356138,66.4));
#98008=CARTESIAN_POINT('Ctrl Pts',(100.166228495456,16.184252771882,66.8));
#98009=CARTESIAN_POINT('Ctrl Pts',(100.345801676491,16.3444447941935,66.5943250148876));
#98010=CARTESIAN_POINT('Ctrl Pts',(100.518191930287,16.4982291356138,66.4));
#98011=CARTESIAN_POINT('',(100.086430779868,16.6880757195422,66.8));
#98012=CARTESIAN_POINT('Ctrl Pts',(100.518191930287,16.4982291356138,66.4));
#98013=CARTESIAN_POINT('Ctrl Pts',(100.306717081102,16.5912152175381,66.594325014887));
#98014=CARTESIAN_POINT('Ctrl Pts',(100.086430779868,16.6880757195423,66.8));
#98015=CARTESIAN_POINT('',(100.003253094606,17.7449484179612,66.8));
#98016=CARTESIAN_POINT('Origin',(110.,18.,66.8));
#98017=CARTESIAN_POINT('',(100.4,18.,66.4));
#98018=CARTESIAN_POINT('Ctrl Pts',(100.003253094606,17.7449484179611,66.8));
#98019=CARTESIAN_POINT('Ctrl Pts',(100.205674985111,17.8750767761431,66.5943250148885));
#98020=CARTESIAN_POINT('Ctrl Pts',(100.4,18.,66.4));
#98021=CARTESIAN_POINT('',(100.8,18.,66.));
#98022=CARTESIAN_POINT('',(100.4,18.,66.4));
#98023=CARTESIAN_POINT('Origin',(110.,18.,66.));
#98024=CARTESIAN_POINT('',(100.003253094606,18.2550515820388,66.8));
#98025=CARTESIAN_POINT('Ctrl Pts',(100.4,18.,66.4));
#98026=CARTESIAN_POINT('Ctrl Pts',(100.205674985111,18.1249232238571,66.5943250148889));
#98027=CARTESIAN_POINT('Ctrl Pts',(100.003253094606,18.2550515820389,66.8));
#98028=CARTESIAN_POINT('',(100.086430779868,19.3119242804578,66.8));
#98029=CARTESIAN_POINT('Origin',(110.,18.,66.8));
#98030=CARTESIAN_POINT('',(100.518191930287,19.5017708643862,66.4));
#98031=CARTESIAN_POINT('Ctrl Pts',(100.086430779868,19.3119242804577,66.8));
#98032=CARTESIAN_POINT('Ctrl Pts',(100.306717081101,19.4087847824617,66.5943250148874));
#98033=CARTESIAN_POINT('Ctrl Pts',(100.518191930287,19.5017708643862,66.4));
#98034=CARTESIAN_POINT('',(100.166228495456,19.815747228118,66.8));
#98035=CARTESIAN_POINT('Ctrl Pts',(100.518191930287,19.5017708643862,66.4));
#98036=CARTESIAN_POINT('Ctrl Pts',(100.345801676492,19.6555552058062,66.5943250148871));
#98037=CARTESIAN_POINT('Ctrl Pts',(100.166228495456,19.815747228118,66.8));
#98038=CARTESIAN_POINT('',(100.41371344058,20.8465962131424,66.8));
#98039=CARTESIAN_POINT('Origin',(110.,18.,66.8));
#98040=CARTESIAN_POINT('',(100.869857443567,20.9665631459995,66.4));
#98041=CARTESIAN_POINT('Ctrl Pts',(100.41371344058,20.8465962131424,66.8));
#98042=CARTESIAN_POINT('Ctrl Pts',(100.646439972714,20.9078038319467,66.5943250148879));
#98043=CARTESIAN_POINT('Ctrl Pts',(100.869857443567,20.9665631459995,66.4));
#98044=CARTESIAN_POINT('',(100.571343987164,21.3317331513213,66.8));
#98045=CARTESIAN_POINT('Ctrl Pts',(100.869857443567,20.9665631459995,66.4));
#98046=CARTESIAN_POINT('Ctrl Pts',(100.723646771042,21.1454219241175,66.594325014888));
#98047=CARTESIAN_POINT('Ctrl Pts',(100.571343987164,21.3317331513213,66.8));
#98048=CARTESIAN_POINT('',(100.977042291445,22.3111754997483,66.8));
#98049=CARTESIAN_POINT('Origin',(110.,18.,66.8));
#98050=CARTESIAN_POINT('',(101.446337367792,22.3583087974996,66.3999999999999));
#98051=CARTESIAN_POINT('Ctrl Pts',(100.977042291445,22.3111754997483,66.8));
#98052=CARTESIAN_POINT('Ctrl Pts',(101.216478554886,22.3352231006417,66.5943250148875));
#98053=CARTESIAN_POINT('Ctrl Pts',(101.446337367792,22.3583087974996,66.3999999999999));
#98054=CARTESIAN_POINT('',(101.208624281823,22.7656807469507,66.8));
#98055=CARTESIAN_POINT('Ctrl Pts',(101.446337367792,22.3583087974996,66.3999999999999));
#98056=CARTESIAN_POINT('Ctrl Pts',(101.329906468541,22.5578379155989,66.5943250148875));
#98057=CARTESIAN_POINT('Ctrl Pts',(101.208624281823,22.7656807469507,66.8));
#98058=CARTESIAN_POINT('',(101.762546306575,23.6695993375792,66.8));
#98059=CARTESIAN_POINT('Origin',(110.,18.,66.8));
#98060=CARTESIAN_POINT('',(102.233436854001,23.6427384220077,66.4));
#98061=CARTESIAN_POINT('Ctrl Pts',(101.762546306575,23.6695993375792,66.8));
#98062=CARTESIAN_POINT('Ctrl Pts',(102.002796585873,23.6558947888183,66.5943250148876));
#98063=CARTESIAN_POINT('Ctrl Pts',(102.233436854001,23.6427384220077,66.4));
#98064=CARTESIAN_POINT('',(102.062377423568,24.0822814662025,66.8));
#98065=CARTESIAN_POINT('Ctrl Pts',(102.233436854001,23.6427384220077,66.4));
#98066=CARTESIAN_POINT('Ctrl Pts',(102.149652643175,23.858024811003,66.5943250148884));
#98067=CARTESIAN_POINT('Ctrl Pts',(102.062377423568,24.0822814662026,66.8));
#98068=CARTESIAN_POINT('',(102.750883770178,24.8884188233975,66.8));
#98069=CARTESIAN_POINT('Origin',(110.,18.,66.8));
#98070=CARTESIAN_POINT('',(103.211774900609,24.7882250993908,66.4));
#98071=CARTESIAN_POINT('Ctrl Pts',(102.750883770178,24.8884188233975,66.8));
#98072=CARTESIAN_POINT('Ctrl Pts',(102.986032306111,24.8372995764558,66.5943250148883));
#98073=CARTESIAN_POINT('Ctrl Pts',(103.211774900609,24.7882250993908,66.4));
#98074=CARTESIAN_POINT('',(103.111581176602,25.2491162298216,66.8));
#98075=CARTESIAN_POINT('Ctrl Pts',(103.211774900609,24.7882250993908,66.4));
#98076=CARTESIAN_POINT('Ctrl Pts',(103.162700423544,25.0139676938896,66.5943250148885));
#98077=CARTESIAN_POINT('Ctrl Pts',(103.111581176602,25.2491162298216,66.8));
#98078=CARTESIAN_POINT('',(103.917718533797,25.9376225764324,66.8));
#98079=CARTESIAN_POINT('Origin',(110.,18.,66.8));
#98080=CARTESIAN_POINT('',(104.357261577992,25.7665631459995,66.4));
#98081=CARTESIAN_POINT('Ctrl Pts',(103.917718533797,25.9376225764324,66.8));
#98082=CARTESIAN_POINT('Ctrl Pts',(104.141975188999,25.8503473568237,66.5943250148866));
#98083=CARTESIAN_POINT('Ctrl Pts',(104.357261577992,25.7665631459995,66.4));
#98084=CARTESIAN_POINT('',(104.330400662421,26.237453693425,66.8));
#98085=CARTESIAN_POINT('Ctrl Pts',(104.357261577992,25.7665631459995,66.4));
#98086=CARTESIAN_POINT('Ctrl Pts',(104.344105211182,25.9972034141269,66.5943250148872));
#98087=CARTESIAN_POINT('Ctrl Pts',(104.330400662421,26.237453693425,66.8));
#98088=CARTESIAN_POINT('',(105.234319253049,26.7913757181765,66.8));
#98089=CARTESIAN_POINT('Origin',(110.,18.,66.8));
#98090=CARTESIAN_POINT('',(105.6416912025,26.5536626322083,66.4));
#98091=CARTESIAN_POINT('Ctrl Pts',(105.234319253049,26.7913757181765,66.8));
#98092=CARTESIAN_POINT('Ctrl Pts',(105.4421620844,26.670093531459,66.5943250148883));
#98093=CARTESIAN_POINT('Ctrl Pts',(105.6416912025,26.5536626322083,66.3999999999999));
#98094=CARTESIAN_POINT('',(105.688824500252,27.0229577085549,66.8));
#98095=CARTESIAN_POINT('Ctrl Pts',(105.6416912025,26.5536626322083,66.4));
#98096=CARTESIAN_POINT('Ctrl Pts',(105.664776899358,26.7835214451143,66.594325014888));
#98097=CARTESIAN_POINT('Ctrl Pts',(105.688824500252,27.0229577085549,66.8));
#98098=CARTESIAN_POINT('',(106.668266848679,27.4286560128359,66.8));
#98099=CARTESIAN_POINT('Origin',(110.,18.,66.8));
#98100=CARTESIAN_POINT('',(107.033436854,27.1301425564335,66.4));
#98101=CARTESIAN_POINT('Ctrl Pts',(106.668266848679,27.4286560128359,66.8));
#98102=CARTESIAN_POINT('Ctrl Pts',(106.854578075883,27.2763532289579,66.5943250148878));
#98103=CARTESIAN_POINT('Ctrl Pts',(107.033436854,27.1301425564335,66.4));
#98104=CARTESIAN_POINT('',(107.153403786858,27.5862865594204,66.8));
#98105=CARTESIAN_POINT('Ctrl Pts',(107.033436854,27.1301425564335,66.4));
#98106=CARTESIAN_POINT('Ctrl Pts',(107.092196168053,27.3535600272857,66.594325014888));
#98107=CARTESIAN_POINT('Ctrl Pts',(107.153403786858,27.5862865594204,66.8));
#98108=CARTESIAN_POINT('',(108.184252771882,27.833771504544,66.8));
#98109=CARTESIAN_POINT('Origin',(110.,18.,66.8));
#98110=CARTESIAN_POINT('',(108.498229135614,27.4818080697133,66.4));
#98111=CARTESIAN_POINT('Ctrl Pts',(108.184252771882,27.833771504544,66.8));
#98112=CARTESIAN_POINT('Ctrl Pts',(108.344444794194,27.6541983235085,66.5943250148873));
#98113=CARTESIAN_POINT('Ctrl Pts',(108.498229135614,27.4818080697133,66.4));
#98114=CARTESIAN_POINT('',(108.688075719542,27.9135692201318,66.8));
#98115=CARTESIAN_POINT('Ctrl Pts',(108.498229135614,27.4818080697133,66.4));
#98116=CARTESIAN_POINT('Ctrl Pts',(108.591215217538,27.6932829188985,66.5943250148872));
#98117=CARTESIAN_POINT('Ctrl Pts',(108.688075719542,27.9135692201319,66.8));
#98118=CARTESIAN_POINT('',(109.744948417961,27.9967469053937,66.8));
#98119=CARTESIAN_POINT('Origin',(110.,18.,66.8));
#98120=CARTESIAN_POINT('',(110.,27.6,66.4));
#98121=CARTESIAN_POINT('Ctrl Pts',(109.744948417961,27.9967469053938,66.8));
#98122=CARTESIAN_POINT('Ctrl Pts',(109.875076776144,27.794325014887,66.594325014887));
#98123=CARTESIAN_POINT('Ctrl Pts',(110.,27.6,66.4));
#98124=CARTESIAN_POINT('',(110.255051582039,27.9967469053937,66.8));
#98125=CARTESIAN_POINT('Ctrl Pts',(110.,27.6,66.4));
#98126=CARTESIAN_POINT('Ctrl Pts',(110.124923223856,27.7943250148865,66.5943250148864));
#98127=CARTESIAN_POINT('Ctrl Pts',(110.255051582039,27.9967469053937,66.8));
#98128=CARTESIAN_POINT('',(111.311924280458,27.9135692201318,66.8));
#98129=CARTESIAN_POINT('Origin',(110.,18.,66.8));
#98130=CARTESIAN_POINT('',(111.501770864386,27.4818080697133,66.4));
#98131=CARTESIAN_POINT('Ctrl Pts',(111.311924280458,27.9135692201318,66.8));
#98132=CARTESIAN_POINT('Ctrl Pts',(111.408784782462,27.693282918898,66.5943250148868));
#98133=CARTESIAN_POINT('Ctrl Pts',(111.501770864386,27.4818080697133,66.4));
#98134=CARTESIAN_POINT('',(111.815747228118,27.833771504544,66.8));
#98135=CARTESIAN_POINT('Ctrl Pts',(111.501770864386,27.4818080697133,66.4));
#98136=CARTESIAN_POINT('Ctrl Pts',(111.655555205806,27.6541983235077,66.5943250148865));
#98137=CARTESIAN_POINT('Ctrl Pts',(111.815747228118,27.833771504544,66.8));
#98138=CARTESIAN_POINT('',(112.846596213142,27.5862865594204,66.8));
#98139=CARTESIAN_POINT('Origin',(110.,18.,66.8));
#98140=CARTESIAN_POINT('',(112.966563146,27.1301425564335,66.4));
#98141=CARTESIAN_POINT('Ctrl Pts',(112.846596213142,27.5862865594204,66.8));
#98142=CARTESIAN_POINT('Ctrl Pts',(112.907803831947,27.3535600272835,66.5943250148861));
#98143=CARTESIAN_POINT('Ctrl Pts',(112.966563146,27.1301425564335,66.4));
#98144=CARTESIAN_POINT('',(113.331733151321,27.4286560128359,66.8));
#98145=CARTESIAN_POINT('Ctrl Pts',(112.966563146,27.1301425564335,66.4));
#98146=CARTESIAN_POINT('Ctrl Pts',(113.145421924116,27.2763532289572,66.5943250148869));
#98147=CARTESIAN_POINT('Ctrl Pts',(113.331733151321,27.4286560128359,66.8));
#98148=CARTESIAN_POINT('',(114.311175499748,27.0229577085549,66.8));
#98149=CARTESIAN_POINT('Origin',(110.,18.,66.8));
#98150=CARTESIAN_POINT('',(114.3583087975,26.5536626322083,66.4));
#98151=CARTESIAN_POINT('Ctrl Pts',(114.311175499748,27.0229577085549,66.8));
#98152=CARTESIAN_POINT('Ctrl Pts',(114.335223100642,26.7835214451131,66.594325014887));
#98153=CARTESIAN_POINT('Ctrl Pts',(114.3583087975,26.5536626322083,66.4));
#98154=CARTESIAN_POINT('',(114.765680746951,26.7913757181765,66.8));
#98155=CARTESIAN_POINT('Ctrl Pts',(114.3583087975,26.5536626322083,66.4));
#98156=CARTESIAN_POINT('Ctrl Pts',(114.557837915598,26.6700935314582,66.594325014887));
#98157=CARTESIAN_POINT('Ctrl Pts',(114.765680746951,26.7913757181765,66.8));
#98158=CARTESIAN_POINT('',(115.669599337579,26.237453693425,66.8));
#98159=CARTESIAN_POINT('Origin',(110.,18.,66.8));
#98160=CARTESIAN_POINT('',(115.642738422008,25.7665631459995,66.4));
#98161=CARTESIAN_POINT('Ctrl Pts',(115.669599337579,26.237453693425,66.8));
#98162=CARTESIAN_POINT('Ctrl Pts',(115.655894788818,25.9972034141256,66.5943250148862));
#98163=CARTESIAN_POINT('Ctrl Pts',(115.642738422008,25.7665631459995,66.4));
#98164=CARTESIAN_POINT('',(116.082281466203,25.9376225764324,66.8));
#98165=CARTESIAN_POINT('Ctrl Pts',(115.642738422008,25.7665631459995,66.4));
#98166=CARTESIAN_POINT('Ctrl Pts',(115.858024811,25.8503473568235,66.5943250148862));
#98167=CARTESIAN_POINT('Ctrl Pts',(116.082281466202,25.9376225764324,66.8));
#98168=CARTESIAN_POINT('',(116.888418823398,25.2491162298216,66.8));
#98169=CARTESIAN_POINT('Origin',(110.,18.,66.8));
#98170=CARTESIAN_POINT('',(116.788225099391,24.7882250993908,66.4));
#98171=CARTESIAN_POINT('Ctrl Pts',(116.888418823398,25.2491162298216,66.8));
#98172=CARTESIAN_POINT('Ctrl Pts',(116.837299576455,25.0139676938873,66.5943250148865));
#98173=CARTESIAN_POINT('Ctrl Pts',(116.788225099391,24.7882250993908,66.4));
#98174=CARTESIAN_POINT('',(117.249116229822,24.8884188233975,66.8));
#98175=CARTESIAN_POINT('Ctrl Pts',(116.788225099391,24.7882250993908,66.4));
#98176=CARTESIAN_POINT('Ctrl Pts',(117.013967693887,24.8372995764551,66.5943250148859));
#98177=CARTESIAN_POINT('Ctrl Pts',(117.249116229822,24.8884188233975,66.8));
#98178=CARTESIAN_POINT('',(117.937622576432,24.0822814662025,66.8));
#98179=CARTESIAN_POINT('Origin',(110.,18.,66.8));
#98180=CARTESIAN_POINT('',(117.766563145999,23.6427384220077,66.4));
#98181=CARTESIAN_POINT('Ctrl Pts',(117.937622576432,24.0822814662025,66.8));
#98182=CARTESIAN_POINT('Ctrl Pts',(117.850347356824,23.8580248110013,66.5943250148869));
#98183=CARTESIAN_POINT('Ctrl Pts',(117.766563146,23.6427384220077,66.4));
#98184=CARTESIAN_POINT('',(118.237453693425,23.6695993375792,66.8));
#98185=CARTESIAN_POINT('Ctrl Pts',(117.766563145999,23.6427384220077,66.4));
#98186=CARTESIAN_POINT('Ctrl Pts',(117.997203414128,23.6558947888183,66.5943250148878));
#98187=CARTESIAN_POINT('Ctrl Pts',(118.237453693425,23.6695993375792,66.8));
#98188=CARTESIAN_POINT('',(118.791375718177,22.7656807469507,66.8));
#98189=CARTESIAN_POINT('Origin',(110.,18.,66.8));
#98190=CARTESIAN_POINT('',(118.553662632208,22.3583087974996,66.4));
#98191=CARTESIAN_POINT('Ctrl Pts',(118.791375718177,22.7656807469507,66.8));
#98192=CARTESIAN_POINT('Ctrl Pts',(118.670093531458,22.5578379155986,66.5943250148872));
#98193=CARTESIAN_POINT('Ctrl Pts',(118.553662632208,22.3583087974996,66.4));
#98194=CARTESIAN_POINT('',(119.022957708555,22.3111754997483,66.8));
#98195=CARTESIAN_POINT('Ctrl Pts',(118.553662632208,22.3583087974996,66.4));
#98196=CARTESIAN_POINT('Ctrl Pts',(118.783521445112,22.3352231006419,66.5943250148863));
#98197=CARTESIAN_POINT('Ctrl Pts',(119.022957708555,22.3111754997483,66.8));
#98198=CARTESIAN_POINT('',(119.428656012836,21.3317331513213,66.8));
#98199=CARTESIAN_POINT('Origin',(110.,18.,66.8));
#98200=CARTESIAN_POINT('',(119.130142556433,20.9665631459995,66.4));
#98201=CARTESIAN_POINT('Ctrl Pts',(119.428656012836,21.3317331513213,66.8));
#98202=CARTESIAN_POINT('Ctrl Pts',(119.276353228957,21.145421924116,66.5943250148865));
#98203=CARTESIAN_POINT('Ctrl Pts',(119.130142556433,20.9665631459995,66.4));
#98204=CARTESIAN_POINT('',(119.58628655942,20.8465962131424,66.8));
#98205=CARTESIAN_POINT('Ctrl Pts',(119.130142556433,20.9665631459995,66.4));
#98206=CARTESIAN_POINT('Ctrl Pts',(119.353560027284,20.9078038319471,66.5943250148866));
#98207=CARTESIAN_POINT('Ctrl Pts',(119.58628655942,20.8465962131424,66.8));
#98208=CARTESIAN_POINT('',(119.833771504544,19.815747228118,66.8));
#98209=CARTESIAN_POINT('Origin',(110.,18.,66.8));
#98210=CARTESIAN_POINT('',(119.481808069713,19.5017708643862,66.4));
#98211=CARTESIAN_POINT('Ctrl Pts',(119.833771504544,19.815747228118,66.8));
#98212=CARTESIAN_POINT('Ctrl Pts',(119.654198323508,19.6555552058055,66.5943250148863));
#98213=CARTESIAN_POINT('Ctrl Pts',(119.481808069713,19.5017708643862,66.4));
#98214=CARTESIAN_POINT('',(119.913569220132,19.3119242804578,66.8));
#98215=CARTESIAN_POINT('Ctrl Pts',(119.481808069713,19.5017708643862,66.4));
#98216=CARTESIAN_POINT('Ctrl Pts',(119.693282918898,19.4087847824621,66.5943250148865));
#98217=CARTESIAN_POINT('Ctrl Pts',(119.913569220132,19.3119242804577,66.8));
#98218=CARTESIAN_POINT('',(119.996746905394,18.2550515820388,66.8));
#98219=CARTESIAN_POINT('Origin',(110.,18.,66.8));
#98220=CARTESIAN_POINT('',(119.6,18.,66.4));
#98221=CARTESIAN_POINT('Ctrl Pts',(119.996746905394,18.2550515820388,66.8));
#98222=CARTESIAN_POINT('Ctrl Pts',(119.794325014887,18.1249232238558,66.5943250148867));
#98223=CARTESIAN_POINT('Ctrl Pts',(119.6,18.,66.4));
#98224=CARTESIAN_POINT('',(119.996746905394,17.7449484179612,66.8));
#98225=CARTESIAN_POINT('Ctrl Pts',(119.6,18.,66.4));
#98226=CARTESIAN_POINT('Ctrl Pts',(119.794325014887,17.8750767761443,66.5943250148866));
#98227=CARTESIAN_POINT('Ctrl Pts',(119.996746905394,17.7449484179612,66.8));
#98228=CARTESIAN_POINT('Origin',(110.,18.,66.8));
#98229=CARTESIAN_POINT('Origin',(110.,18.,73.5));
#98230=CARTESIAN_POINT('',(119.58628655942,15.1534037868576,80.2));
#98231=CARTESIAN_POINT('Origin',(110.,18.,80.2));
#98232=CARTESIAN_POINT('',(119.58628655942,15.1534037868576,73.5));
#98233=CARTESIAN_POINT('Origin',(110.,18.,73.5));
#98234=CARTESIAN_POINT('',(119.996746905394,17.7449484179612,80.2));
#98235=CARTESIAN_POINT('',(119.996746905394,17.7449484179612,73.5));
#98236=CARTESIAN_POINT('Origin',(110.,18.,80.2));
#98237=CARTESIAN_POINT('Origin',(119.656824470371,14.3891495256052,81.));
#98238=CARTESIAN_POINT('',(119.130142556433,15.0334368540005,80.6));
#98239=CARTESIAN_POINT('',(119.130142556433,15.0334368540005,81.));
#98240=CARTESIAN_POINT('',(119.428656012836,14.6682668486787,80.2));
#98241=CARTESIAN_POINT('Ctrl Pts',(119.428656012836,14.6682668486787,80.2));
#98242=CARTESIAN_POINT('Ctrl Pts',(119.276353228957,14.8545780758837,80.4056749851132));
#98243=CARTESIAN_POINT('Ctrl Pts',(119.130142556433,15.0334368540005,80.6));
#98244=CARTESIAN_POINT('',(119.428656012836,14.6682668486787,73.5));
#98245=CARTESIAN_POINT('Origin',(119.130142556433,15.0334368540005,81.));
#98246=CARTESIAN_POINT('Ctrl Pts',(119.130142556433,15.0334368540005,80.6));
#98247=CARTESIAN_POINT('Ctrl Pts',(119.353560027284,15.092196168053,80.4056749851132));
#98248=CARTESIAN_POINT('Ctrl Pts',(119.58628655942,15.1534037868576,80.2));
#98249=CARTESIAN_POINT('Origin',(110.,18.,73.5));
#98250=CARTESIAN_POINT('',(119.022957708555,13.6888245002517,80.2));
#98251=CARTESIAN_POINT('Origin',(110.,18.,80.2));
#98252=CARTESIAN_POINT('',(119.022957708555,13.6888245002517,73.5));
#98253=CARTESIAN_POINT('Origin',(110.,18.,80.6));
#98254=CARTESIAN_POINT('',(100.8,18.,81.));
#98255=CARTESIAN_POINT('Origin',(110.,18.,81.));
#98256=CARTESIAN_POINT('',(100.4,18.,80.6));
#98257=CARTESIAN_POINT('',(100.4,18.,80.6));
#98258=CARTESIAN_POINT('',(100.003253094606,17.7449484179612,80.2));
#98259=CARTESIAN_POINT('Ctrl Pts',(100.4,18.,80.6));
#98260=CARTESIAN_POINT('Ctrl Pts',(100.205674985113,17.8750767761442,80.4056749851132));
#98261=CARTESIAN_POINT('Ctrl Pts',(100.003253094606,17.7449484179612,80.2));
#98262=CARTESIAN_POINT('',(100.086430779868,16.6880757195422,80.2));
#98263=CARTESIAN_POINT('Origin',(110.,18.,80.2));
#98264=CARTESIAN_POINT('',(100.518191930287,16.4982291356138,80.6));
#98265=CARTESIAN_POINT('Ctrl Pts',(100.086430779868,16.6880757195422,80.2));
#98266=CARTESIAN_POINT('Ctrl Pts',(100.306717081103,16.5912152175373,80.4056749851144));
#98267=CARTESIAN_POINT('Ctrl Pts',(100.518191930287,16.4982291356138,80.6));
#98268=CARTESIAN_POINT('',(100.166228495456,16.184252771882,80.2));
#98269=CARTESIAN_POINT('Ctrl Pts',(100.518191930287,16.4982291356138,80.6));
#98270=CARTESIAN_POINT('Ctrl Pts',(100.345801676493,16.3444447941946,80.4056749851138));
#98271=CARTESIAN_POINT('Ctrl Pts',(100.166228495456,16.184252771882,80.2));
#98272=CARTESIAN_POINT('',(100.41371344058,15.1534037868576,80.2));
#98273=CARTESIAN_POINT('Origin',(110.,18.,80.2));
#98274=CARTESIAN_POINT('',(100.869857443567,15.0334368540005,80.6));
#98275=CARTESIAN_POINT('Ctrl Pts',(100.41371344058,15.1534037868576,80.2));
#98276=CARTESIAN_POINT('Ctrl Pts',(100.646439972715,15.0921961680531,80.4056749851129));
#98277=CARTESIAN_POINT('Ctrl Pts',(100.869857443567,15.0334368540005,80.6));
#98278=CARTESIAN_POINT('',(100.571343987164,14.6682668486788,80.2));
#98279=CARTESIAN_POINT('Ctrl Pts',(100.869857443567,15.0334368540005,80.6));
#98280=CARTESIAN_POINT('Ctrl Pts',(100.723646771043,14.854578075884,80.4056749851136));
#98281=CARTESIAN_POINT('Ctrl Pts',(100.571343987164,14.6682668486787,80.2));
#98282=CARTESIAN_POINT('',(100.977042291445,13.6888245002517,80.2));
#98283=CARTESIAN_POINT('Origin',(110.,18.,80.2));
#98284=CARTESIAN_POINT('',(101.446337367792,13.6416912025004,80.6));
#98285=CARTESIAN_POINT('Ctrl Pts',(100.977042291445,13.6888245002517,80.2));
#98286=CARTESIAN_POINT('Ctrl Pts',(101.216478554888,13.6647768993581,80.405674985114));
#98287=CARTESIAN_POINT('Ctrl Pts',(101.446337367792,13.6416912025004,80.6));
#98288=CARTESIAN_POINT('',(101.208624281823,13.2343192530494,80.2));
#98289=CARTESIAN_POINT('Ctrl Pts',(101.446337367792,13.6416912025004,80.6));
#98290=CARTESIAN_POINT('Ctrl Pts',(101.329906468542,13.4421620844021,80.4056749851134));
#98291=CARTESIAN_POINT('Ctrl Pts',(101.208624281823,13.2343192530494,80.2));
#98292=CARTESIAN_POINT('',(101.762546306575,12.3304006624208,80.2));
#98293=CARTESIAN_POINT('Origin',(110.,18.,80.2));
#98294=CARTESIAN_POINT('',(102.233436854001,12.3572615779923,80.6));
#98295=CARTESIAN_POINT('Ctrl Pts',(101.762546306575,12.3304006624208,80.2));
#98296=CARTESIAN_POINT('Ctrl Pts',(102.002796585874,12.3441052111818,80.4056749851137));
#98297=CARTESIAN_POINT('Ctrl Pts',(102.233436854001,12.3572615779923,80.6));
#98298=CARTESIAN_POINT('',(102.062377423568,11.9177185337975,80.2));
#98299=CARTESIAN_POINT('Ctrl Pts',(102.233436854001,12.3572615779923,80.6));
#98300=CARTESIAN_POINT('Ctrl Pts',(102.149652643177,12.1419751889997,80.405674985114));
#98301=CARTESIAN_POINT('Ctrl Pts',(102.062377423568,11.9177185337975,80.2));
#98302=CARTESIAN_POINT('',(102.750883770178,11.1115811766025,80.2));
#98303=CARTESIAN_POINT('Origin',(110.,18.,80.2));
#98304=CARTESIAN_POINT('',(103.211774900609,11.2117749006092,80.6));
#98305=CARTESIAN_POINT('Ctrl Pts',(102.750883770178,11.1115811766025,80.2));
#98306=CARTESIAN_POINT('Ctrl Pts',(102.986032306113,11.1627004235447,80.4056749851135));
#98307=CARTESIAN_POINT('Ctrl Pts',(103.211774900609,11.2117749006092,80.6));
#98308=CARTESIAN_POINT('',(103.111581176602,10.7508837701784,80.2));
#98309=CARTESIAN_POINT('Ctrl Pts',(103.211774900609,11.2117749006092,80.6));
#98310=CARTESIAN_POINT('Ctrl Pts',(103.162700423545,10.9860323061126,80.4056749851134));
#98311=CARTESIAN_POINT('Ctrl Pts',(103.111581176602,10.7508837701784,80.2));
#98312=CARTESIAN_POINT('',(103.917718533797,10.0623774235676,80.2));
#98313=CARTESIAN_POINT('Origin',(110.,18.,80.2));
#98314=CARTESIAN_POINT('',(104.357261577992,10.2334368540005,80.6));
#98315=CARTESIAN_POINT('Ctrl Pts',(103.917718533797,10.0623774235676,80.2));
#98316=CARTESIAN_POINT('Ctrl Pts',(104.141975188999,10.1496526431763,80.4056749851136));
#98317=CARTESIAN_POINT('Ctrl Pts',(104.357261577992,10.2334368540005,80.6));
#98318=CARTESIAN_POINT('',(104.330400662421,9.76254630657499,80.2));
#98319=CARTESIAN_POINT('Ctrl Pts',(104.357261577992,10.2334368540005,80.6));
#98320=CARTESIAN_POINT('Ctrl Pts',(104.344105211182,10.0027965858746,80.4056749851139));
#98321=CARTESIAN_POINT('Ctrl Pts',(104.330400662421,9.76254630657499,80.2));
#98322=CARTESIAN_POINT('',(105.234319253049,9.20862428182348,80.2));
#98323=CARTESIAN_POINT('Origin',(110.,18.,80.2));
#98324=CARTESIAN_POINT('',(105.6416912025,9.44633736779169,80.6));
#98325=CARTESIAN_POINT('Ctrl Pts',(105.234319253049,9.20862428182348,80.2));
#98326=CARTESIAN_POINT('Ctrl Pts',(105.442162084402,9.32990646854195,80.4056749851133));
#98327=CARTESIAN_POINT('Ctrl Pts',(105.6416912025,9.44633736779169,80.6));
#98328=CARTESIAN_POINT('',(105.688824500252,8.97704229144512,80.2));
#98329=CARTESIAN_POINT('Ctrl Pts',(105.6416912025,9.44633736779169,80.6));
#98330=CARTESIAN_POINT('Ctrl Pts',(105.664776899358,9.21647855488777,80.4056749851137));
#98331=CARTESIAN_POINT('Ctrl Pts',(105.688824500252,8.97704229144512,80.2));
#98332=CARTESIAN_POINT('',(106.668266848679,8.57134398716408,80.2));
#98333=CARTESIAN_POINT('Origin',(110.,18.,80.2));
#98334=CARTESIAN_POINT('',(107.033436854001,8.86985744356654,80.6));
#98335=CARTESIAN_POINT('Ctrl Pts',(106.668266848679,8.57134398716408,80.2));
#98336=CARTESIAN_POINT('Ctrl Pts',(106.854578075884,8.72364677104273,80.4056749851131));
#98337=CARTESIAN_POINT('Ctrl Pts',(107.033436854001,8.86985744356654,80.6));
#98338=CARTESIAN_POINT('',(107.153403786858,8.41371344057964,80.2));
#98339=CARTESIAN_POINT('Ctrl Pts',(107.033436854001,8.86985744356654,80.6));
#98340=CARTESIAN_POINT('Ctrl Pts',(107.092196168053,8.64643997271655,80.4056749851139));
#98341=CARTESIAN_POINT('Ctrl Pts',(107.153403786858,8.41371344057964,80.2));
#98342=CARTESIAN_POINT('',(108.184252771882,8.16622849545598,80.2));
#98343=CARTESIAN_POINT('Origin',(110.,18.,80.2));
#98344=CARTESIAN_POINT('',(108.498229135614,8.51819193028669,80.6));
#98345=CARTESIAN_POINT('Ctrl Pts',(108.184252771882,8.16622849545598,80.2));
#98346=CARTESIAN_POINT('Ctrl Pts',(108.344444794194,8.34580167649242,80.4056749851137));
#98347=CARTESIAN_POINT('Ctrl Pts',(108.498229135614,8.51819193028669,80.6));
#98348=CARTESIAN_POINT('',(108.688075719542,8.08643077986816,80.2));
#98349=CARTESIAN_POINT('Ctrl Pts',(108.498229135614,8.51819193028669,80.6));
#98350=CARTESIAN_POINT('Ctrl Pts',(108.591215217538,8.30671708110244,80.4056749851136));
#98351=CARTESIAN_POINT('Ctrl Pts',(108.688075719542,8.08643077986816,80.2));
#98352=CARTESIAN_POINT('',(109.744948417961,8.00325309460625,80.2));
#98353=CARTESIAN_POINT('Origin',(110.,18.,80.2));
#98354=CARTESIAN_POINT('',(110.,8.40000000000002,80.6));
#98355=CARTESIAN_POINT('Ctrl Pts',(109.744948417961,8.00325309460625,80.2));
#98356=CARTESIAN_POINT('Ctrl Pts',(109.875076776144,8.20567498511359,80.4056749851136));
#98357=CARTESIAN_POINT('Ctrl Pts',(110.,8.40000000000002,80.6));
#98358=CARTESIAN_POINT('',(110.255051582039,8.00325309460625,80.2));
#98359=CARTESIAN_POINT('Ctrl Pts',(110.,8.40000000000002,80.6));
#98360=CARTESIAN_POINT('Ctrl Pts',(110.124923223856,8.20567498511304,80.405674985113));
#98361=CARTESIAN_POINT('Ctrl Pts',(110.255051582039,8.00325309460625,80.2));
#98362=CARTESIAN_POINT('',(111.311924280458,8.08643077986816,80.2));
#98363=CARTESIAN_POINT('Origin',(110.,18.,80.2));
#98364=CARTESIAN_POINT('',(111.501770864386,8.51819193028669,80.6));
#98365=CARTESIAN_POINT('Ctrl Pts',(111.311924280458,8.08643077986816,80.2));
#98366=CARTESIAN_POINT('Ctrl Pts',(111.408784782462,8.30671708110237,80.4056749851135));
#98367=CARTESIAN_POINT('Ctrl Pts',(111.501770864386,8.51819193028669,80.6));
#98368=CARTESIAN_POINT('',(111.815747228118,8.16622849545598,80.2));
#98369=CARTESIAN_POINT('Ctrl Pts',(111.501770864386,8.51819193028669,80.6));
#98370=CARTESIAN_POINT('Ctrl Pts',(111.655555205805,8.34580167649278,80.4056749851141));
#98371=CARTESIAN_POINT('Ctrl Pts',(111.815747228118,8.16622849545598,80.2));
#98372=CARTESIAN_POINT('',(112.846596213142,8.41371344057965,80.2));
#98373=CARTESIAN_POINT('Origin',(110.,18.,80.2));
#98374=CARTESIAN_POINT('',(112.966563146,8.86985744356654,80.6));
#98375=CARTESIAN_POINT('Ctrl Pts',(112.846596213142,8.41371344057965,80.2));
#98376=CARTESIAN_POINT('Ctrl Pts',(112.907803831947,8.64643997271638,80.4056749851138));
#98377=CARTESIAN_POINT('Ctrl Pts',(112.966563146,8.86985744356654,80.6));
#98378=CARTESIAN_POINT('',(113.331733151321,8.57134398716408,80.2));
#98379=CARTESIAN_POINT('Ctrl Pts',(112.966563146,8.86985744356654,80.6));
#98380=CARTESIAN_POINT('Ctrl Pts',(113.145421924116,8.72364677104327,80.4056749851138));
#98381=CARTESIAN_POINT('Ctrl Pts',(113.331733151321,8.57134398716408,80.2));
#98382=CARTESIAN_POINT('',(114.311175499748,8.97704229144512,80.2));
#98383=CARTESIAN_POINT('Origin',(110.,18.,80.2));
#98384=CARTESIAN_POINT('',(114.3583087975,9.44633736779169,80.6));
#98385=CARTESIAN_POINT('Ctrl Pts',(114.311175499748,8.97704229144512,80.2));
#98386=CARTESIAN_POINT('Ctrl Pts',(114.335223100642,9.21647855488781,80.4056749851138));
#98387=CARTESIAN_POINT('Ctrl Pts',(114.3583087975,9.44633736779169,80.6));
#98388=CARTESIAN_POINT('',(114.765680746951,9.20862428182348,80.2));
#98389=CARTESIAN_POINT('Ctrl Pts',(114.3583087975,9.44633736779169,80.6));
#98390=CARTESIAN_POINT('Ctrl Pts',(114.557837915597,9.32990646854248,80.4056749851141));
#98391=CARTESIAN_POINT('Ctrl Pts',(114.765680746951,9.20862428182348,80.2));
#98392=CARTESIAN_POINT('',(115.669599337579,9.762546306575,80.2));
#98393=CARTESIAN_POINT('Origin',(110.,18.,80.2));
#98394=CARTESIAN_POINT('',(115.642738422008,10.2334368540005,80.6));
#98395=CARTESIAN_POINT('Ctrl Pts',(115.669599337579,9.762546306575,80.2));
#98396=CARTESIAN_POINT('Ctrl Pts',(115.655894788818,10.0027965858745,80.4056749851139));
#98397=CARTESIAN_POINT('Ctrl Pts',(115.642738422008,10.2334368540005,80.6));
#98398=CARTESIAN_POINT('',(116.082281466203,10.0623774235676,80.2));
#98399=CARTESIAN_POINT('Ctrl Pts',(115.642738422008,10.2334368540005,80.6));
#98400=CARTESIAN_POINT('Ctrl Pts',(115.858024811002,10.1496526431759,80.4056749851125));
#98401=CARTESIAN_POINT('Ctrl Pts',(116.082281466203,10.0623774235676,80.2));
#98402=CARTESIAN_POINT('',(116.888418823398,10.7508837701784,80.2));
#98403=CARTESIAN_POINT('Origin',(110.,18.,80.2));
#98404=CARTESIAN_POINT('',(116.788225099391,11.2117749006091,80.6));
#98405=CARTESIAN_POINT('Ctrl Pts',(116.888418823398,10.7508837701784,80.2));
#98406=CARTESIAN_POINT('Ctrl Pts',(116.837299576455,10.9860323061133,80.4056749851139));
#98407=CARTESIAN_POINT('Ctrl Pts',(116.788225099391,11.2117749006091,80.6));
#98408=CARTESIAN_POINT('',(117.249116229822,11.1115811766025,80.2));
#98409=CARTESIAN_POINT('Ctrl Pts',(116.788225099391,11.2117749006091,80.6));
#98410=CARTESIAN_POINT('Ctrl Pts',(117.013967693888,11.1627004235446,80.405674985113));
#98411=CARTESIAN_POINT('Ctrl Pts',(117.249116229822,11.1115811766025,80.2));
#98412=CARTESIAN_POINT('',(117.937622576432,11.9177185337975,80.2));
#98413=CARTESIAN_POINT('Origin',(110.,18.,80.2));
#98414=CARTESIAN_POINT('',(117.766563145999,12.3572615779923,80.6));
#98415=CARTESIAN_POINT('Ctrl Pts',(117.937622576432,11.9177185337975,80.2));
#98416=CARTESIAN_POINT('Ctrl Pts',(117.850347356824,12.141975188999,80.4056749851133));
#98417=CARTESIAN_POINT('Ctrl Pts',(117.766563145999,12.3572615779923,80.6));
#98418=CARTESIAN_POINT('',(118.237453693425,12.3304006624208,80.2));
#98419=CARTESIAN_POINT('Ctrl Pts',(117.766563145999,12.3572615779923,80.6));
#98420=CARTESIAN_POINT('Ctrl Pts',(117.997203414126,12.3441052111817,80.4056749851134));
#98421=CARTESIAN_POINT('Ctrl Pts',(118.237453693425,12.3304006624208,80.2));
#98422=CARTESIAN_POINT('',(118.791375718177,13.2343192530493,80.2));
#98423=CARTESIAN_POINT('Origin',(110.,18.,80.2));
#98424=CARTESIAN_POINT('',(118.553662632208,13.6416912025004,80.6));
#98425=CARTESIAN_POINT('Ctrl Pts',(118.791375718177,13.2343192530493,80.2));
#98426=CARTESIAN_POINT('Ctrl Pts',(118.670093531458,13.4421620844014,80.4056749851128));
#98427=CARTESIAN_POINT('Ctrl Pts',(118.553662632208,13.6416912025004,80.6));
#98428=CARTESIAN_POINT('Ctrl Pts',(118.553662632208,13.6416912025004,80.6));
#98429=CARTESIAN_POINT('Ctrl Pts',(118.783521445112,13.6647768993581,80.4056749851135));
#98430=CARTESIAN_POINT('Ctrl Pts',(119.022957708555,13.6888245002517,80.2));
#98431=CARTESIAN_POINT('',(119.6,18.,80.6));
#98432=CARTESIAN_POINT('Ctrl Pts',(119.996746905394,17.7449484179612,80.2));
#98433=CARTESIAN_POINT('Ctrl Pts',(119.794325014887,17.8750767761442,80.4056749851131));
#98434=CARTESIAN_POINT('Ctrl Pts',(119.6,18.,80.6));
#98435=CARTESIAN_POINT('',(119.996746905394,18.2550515820388,80.2));
#98436=CARTESIAN_POINT('Ctrl Pts',(119.6,18.,80.6));
#98437=CARTESIAN_POINT('Ctrl Pts',(119.794325014887,18.124923223856,80.4056749851128));
#98438=CARTESIAN_POINT('Ctrl Pts',(119.996746905394,18.2550515820388,80.2));
#98439=CARTESIAN_POINT('',(119.913569220132,19.3119242804578,80.2));
#98440=CARTESIAN_POINT('Origin',(110.,18.,80.2));
#98441=CARTESIAN_POINT('',(119.481808069713,19.5017708643862,80.6));
#98442=CARTESIAN_POINT('Ctrl Pts',(119.913569220132,19.3119242804577,80.2));
#98443=CARTESIAN_POINT('Ctrl Pts',(119.693282918898,19.4087847824621,80.4056749851132));
#98444=CARTESIAN_POINT('Ctrl Pts',(119.481808069713,19.5017708643862,80.6));
#98445=CARTESIAN_POINT('',(119.833771504544,19.815747228118,80.2));
#98446=CARTESIAN_POINT('Ctrl Pts',(119.481808069713,19.5017708643862,80.6));
#98447=CARTESIAN_POINT('Ctrl Pts',(119.654198323507,19.655555205805,80.4056749851143));
#98448=CARTESIAN_POINT('Ctrl Pts',(119.833771504544,19.815747228118,80.2));
#98449=CARTESIAN_POINT('',(119.58628655942,20.8465962131424,80.2));
#98450=CARTESIAN_POINT('Origin',(110.,18.,80.2));
#98451=CARTESIAN_POINT('',(119.130142556433,20.9665631459995,80.6));
#98452=CARTESIAN_POINT('Ctrl Pts',(119.58628655942,20.8465962131424,80.2));
#98453=CARTESIAN_POINT('Ctrl Pts',(119.353560027284,20.907803831947,80.4056749851133));
#98454=CARTESIAN_POINT('Ctrl Pts',(119.130142556433,20.9665631459995,80.6));
#98455=CARTESIAN_POINT('',(119.428656012836,21.3317331513213,80.2));
#98456=CARTESIAN_POINT('Ctrl Pts',(119.130142556433,20.9665631459995,80.6));
#98457=CARTESIAN_POINT('Ctrl Pts',(119.276353228957,21.1454219241167,80.4056749851128));
#98458=CARTESIAN_POINT('Ctrl Pts',(119.428656012836,21.3317331513213,80.2));
#98459=CARTESIAN_POINT('',(119.022957708555,22.3111754997483,80.2));
#98460=CARTESIAN_POINT('Origin',(110.,18.,80.2));
#98461=CARTESIAN_POINT('',(118.553662632208,22.3583087974996,80.6));
#98462=CARTESIAN_POINT('Ctrl Pts',(119.022957708555,22.3111754997483,80.2));
#98463=CARTESIAN_POINT('Ctrl Pts',(118.783521445111,22.335223100642,80.4056749851144));
#98464=CARTESIAN_POINT('Ctrl Pts',(118.553662632208,22.3583087974996,80.6));
#98465=CARTESIAN_POINT('',(118.791375718177,22.7656807469507,80.2));
#98466=CARTESIAN_POINT('Ctrl Pts',(118.553662632208,22.3583087974996,80.6));
#98467=CARTESIAN_POINT('Ctrl Pts',(118.670093531459,22.5578379155991,80.4056749851123));
#98468=CARTESIAN_POINT('Ctrl Pts',(118.791375718177,22.7656807469507,80.2));
#98469=CARTESIAN_POINT('',(118.237453693425,23.6695993375792,80.2));
#98470=CARTESIAN_POINT('Origin',(110.,18.,80.2));
#98471=CARTESIAN_POINT('',(117.766563145999,23.6427384220077,80.6));
#98472=CARTESIAN_POINT('Ctrl Pts',(118.237453693425,23.6695993375792,80.2));
#98473=CARTESIAN_POINT('Ctrl Pts',(117.997203414127,23.6558947888183,80.4056749851127));
#98474=CARTESIAN_POINT('Ctrl Pts',(117.766563145999,23.6427384220077,80.6));
#98475=CARTESIAN_POINT('',(117.937622576432,24.0822814662025,80.2));
#98476=CARTESIAN_POINT('Ctrl Pts',(117.766563145999,23.6427384220077,80.6));
#98477=CARTESIAN_POINT('Ctrl Pts',(117.850347356824,23.8580248110013,80.4056749851131));
#98478=CARTESIAN_POINT('Ctrl Pts',(117.937622576432,24.0822814662025,80.2));
#98479=CARTESIAN_POINT('',(117.249116229822,24.8884188233975,80.2));
#98480=CARTESIAN_POINT('Origin',(110.,18.,80.2));
#98481=CARTESIAN_POINT('',(116.788225099391,24.7882250993908,80.6));
#98482=CARTESIAN_POINT('Ctrl Pts',(117.249116229822,24.8884188233975,80.2));
#98483=CARTESIAN_POINT('Ctrl Pts',(117.013967693888,24.8372995764555,80.4056749851127));
#98484=CARTESIAN_POINT('Ctrl Pts',(116.788225099391,24.7882250993908,80.6));
#98485=CARTESIAN_POINT('',(116.888418823398,25.2491162298216,80.2));
#98486=CARTESIAN_POINT('Ctrl Pts',(116.788225099391,24.7882250993908,80.6));
#98487=CARTESIAN_POINT('Ctrl Pts',(116.837299576455,25.0139676938872,80.4056749851135));
#98488=CARTESIAN_POINT('Ctrl Pts',(116.888418823398,25.2491162298216,80.2));
#98489=CARTESIAN_POINT('',(116.082281466203,25.9376225764324,80.2));
#98490=CARTESIAN_POINT('Origin',(110.,18.,80.2));
#98491=CARTESIAN_POINT('',(115.642738422008,25.7665631459995,80.6));
#98492=CARTESIAN_POINT('Ctrl Pts',(116.082281466202,25.9376225764324,80.2));
#98493=CARTESIAN_POINT('Ctrl Pts',(115.858024811001,25.8503473568238,80.4056749851132));
#98494=CARTESIAN_POINT('Ctrl Pts',(115.642738422008,25.7665631459995,80.6));
#98495=CARTESIAN_POINT('',(115.669599337579,26.237453693425,80.2));
#98496=CARTESIAN_POINT('Ctrl Pts',(115.642738422008,25.7665631459995,80.6));
#98497=CARTESIAN_POINT('Ctrl Pts',(115.655894788818,25.9972034141258,80.4056749851137));
#98498=CARTESIAN_POINT('Ctrl Pts',(115.669599337579,26.237453693425,80.2));
#98499=CARTESIAN_POINT('',(114.765680746951,26.7913757181765,80.2));
#98500=CARTESIAN_POINT('Origin',(110.,18.,80.2));
#98501=CARTESIAN_POINT('',(114.3583087975,26.5536626322083,80.6));
#98502=CARTESIAN_POINT('Ctrl Pts',(114.765680746951,26.7913757181765,80.2));
#98503=CARTESIAN_POINT('Ctrl Pts',(114.557837915598,26.670093531458,80.4056749851134));
#98504=CARTESIAN_POINT('Ctrl Pts',(114.3583087975,26.5536626322083,80.6));
#98505=CARTESIAN_POINT('',(114.311175499748,27.0229577085549,80.2));
#98506=CARTESIAN_POINT('Ctrl Pts',(114.3583087975,26.5536626322083,80.6));
#98507=CARTESIAN_POINT('Ctrl Pts',(114.335223100642,26.783521445112,80.4056749851139));
#98508=CARTESIAN_POINT('Ctrl Pts',(114.311175499748,27.0229577085549,80.2));
#98509=CARTESIAN_POINT('',(113.331733151321,27.4286560128359,80.2));
#98510=CARTESIAN_POINT('Origin',(110.,18.,80.2));
#98511=CARTESIAN_POINT('',(112.966563146,27.1301425564335,80.6));
#98512=CARTESIAN_POINT('Ctrl Pts',(113.331733151321,27.4286560128359,80.2));
#98513=CARTESIAN_POINT('Ctrl Pts',(113.145421924116,27.276353228957,80.4056749851134));
#98514=CARTESIAN_POINT('Ctrl Pts',(112.966563146,27.1301425564335,80.6));
#98515=CARTESIAN_POINT('',(112.846596213142,27.5862865594204,80.2));
#98516=CARTESIAN_POINT('Ctrl Pts',(112.966563146,27.1301425564335,80.6));
#98517=CARTESIAN_POINT('Ctrl Pts',(112.907803831947,27.3535600272837,80.4056749851137));
#98518=CARTESIAN_POINT('Ctrl Pts',(112.846596213142,27.5862865594204,80.2));
#98519=CARTESIAN_POINT('',(111.815747228118,27.833771504544,80.2));
#98520=CARTESIAN_POINT('Origin',(110.,18.,80.2));
#98521=CARTESIAN_POINT('',(111.501770864386,27.4818080697133,80.6));
#98522=CARTESIAN_POINT('Ctrl Pts',(111.815747228118,27.833771504544,80.2));
#98523=CARTESIAN_POINT('Ctrl Pts',(111.655555205806,27.6541983235079,80.4056749851134));
#98524=CARTESIAN_POINT('Ctrl Pts',(111.501770864386,27.4818080697133,80.6));
#98525=CARTESIAN_POINT('',(111.311924280458,27.9135692201318,80.2));
#98526=CARTESIAN_POINT('Ctrl Pts',(111.501770864386,27.4818080697133,80.6));
#98527=CARTESIAN_POINT('Ctrl Pts',(111.408784782462,27.6932829188972,80.4056749851139));
#98528=CARTESIAN_POINT('Ctrl Pts',(111.311924280458,27.9135692201318,80.2));
#98529=CARTESIAN_POINT('',(110.255051582039,27.9967469053937,80.2));
#98530=CARTESIAN_POINT('Origin',(110.,18.,80.2));
#98531=CARTESIAN_POINT('',(110.,27.6,80.6));
#98532=CARTESIAN_POINT('Ctrl Pts',(110.255051582039,27.9967469053937,80.2));
#98533=CARTESIAN_POINT('Ctrl Pts',(110.124923223856,27.7943250148868,80.4056749851132));
#98534=CARTESIAN_POINT('Ctrl Pts',(110.,27.6,80.6));
#98535=CARTESIAN_POINT('',(109.744948417961,27.9967469053937,80.2));
#98536=CARTESIAN_POINT('Ctrl Pts',(110.,27.6,80.6));
#98537=CARTESIAN_POINT('Ctrl Pts',(109.875076776144,27.7943250148865,80.4056749851135));
#98538=CARTESIAN_POINT('Ctrl Pts',(109.744948417961,27.9967469053938,80.2));
#98539=CARTESIAN_POINT('',(108.688075719542,27.9135692201318,80.2));
#98540=CARTESIAN_POINT('Origin',(110.,18.,80.2));
#98541=CARTESIAN_POINT('',(108.498229135614,27.4818080697133,80.6));
#98542=CARTESIAN_POINT('Ctrl Pts',(108.688075719542,27.9135692201318,80.2));
#98543=CARTESIAN_POINT('Ctrl Pts',(108.591215217538,27.693282918897,80.4056749851141));
#98544=CARTESIAN_POINT('Ctrl Pts',(108.498229135614,27.4818080697133,80.6));
#98545=CARTESIAN_POINT('',(108.184252771882,27.833771504544,80.2));
#98546=CARTESIAN_POINT('Ctrl Pts',(108.498229135614,27.4818080697133,80.6));
#98547=CARTESIAN_POINT('Ctrl Pts',(108.344444794194,27.6541983235076,80.4056749851136));
#98548=CARTESIAN_POINT('Ctrl Pts',(108.184252771882,27.833771504544,80.2));
#98549=CARTESIAN_POINT('',(107.153403786858,27.5862865594204,80.2));
#98550=CARTESIAN_POINT('Origin',(110.,18.,80.2));
#98551=CARTESIAN_POINT('',(107.033436854,27.1301425564335,80.6));
#98552=CARTESIAN_POINT('Ctrl Pts',(107.153403786858,27.5862865594204,80.2));
#98553=CARTESIAN_POINT('Ctrl Pts',(107.092196168053,27.3535600272838,80.4056749851136));
#98554=CARTESIAN_POINT('Ctrl Pts',(107.033436854,27.1301425564335,80.6));
#98555=CARTESIAN_POINT('',(106.668266848679,27.4286560128359,80.2));
#98556=CARTESIAN_POINT('Ctrl Pts',(107.033436854,27.1301425564335,80.6));
#98557=CARTESIAN_POINT('Ctrl Pts',(106.854578075884,27.276353228957,80.4056749851134));
#98558=CARTESIAN_POINT('Ctrl Pts',(106.668266848679,27.4286560128359,80.2));
#98559=CARTESIAN_POINT('',(105.688824500252,27.0229577085549,80.2));
#98560=CARTESIAN_POINT('Origin',(110.,18.,80.2));
#98561=CARTESIAN_POINT('',(105.6416912025,26.5536626322083,80.6));
#98562=CARTESIAN_POINT('Ctrl Pts',(105.688824500252,27.0229577085549,80.2));
#98563=CARTESIAN_POINT('Ctrl Pts',(105.664776899358,26.7835214451122,80.4056749851137));
#98564=CARTESIAN_POINT('Ctrl Pts',(105.6416912025,26.5536626322083,80.6));
#98565=CARTESIAN_POINT('',(105.234319253049,26.7913757181765,80.2));
#98566=CARTESIAN_POINT('Ctrl Pts',(105.6416912025,26.5536626322083,80.6));
#98567=CARTESIAN_POINT('Ctrl Pts',(105.442162084403,26.6700935314577,80.4056749851139));
#98568=CARTESIAN_POINT('Ctrl Pts',(105.234319253049,26.7913757181765,80.2));
#98569=CARTESIAN_POINT('',(104.330400662421,26.237453693425,80.2));
#98570=CARTESIAN_POINT('Origin',(110.,18.,80.2));
#98571=CARTESIAN_POINT('',(104.357261577992,25.7665631459995,80.6));
#98572=CARTESIAN_POINT('Ctrl Pts',(104.330400662421,26.237453693425,80.2));
#98573=CARTESIAN_POINT('Ctrl Pts',(104.344105211182,25.9972034141259,80.4056749851136));
#98574=CARTESIAN_POINT('Ctrl Pts',(104.357261577992,25.7665631459995,80.6));
#98575=CARTESIAN_POINT('',(103.917718533797,25.9376225764324,80.2));
#98576=CARTESIAN_POINT('Ctrl Pts',(104.357261577992,25.7665631459995,80.6));
#98577=CARTESIAN_POINT('Ctrl Pts',(104.141975188998,25.8503473568243,80.4056749851121));
#98578=CARTESIAN_POINT('Ctrl Pts',(103.917718533797,25.9376225764324,80.2));
#98579=CARTESIAN_POINT('',(103.111581176602,25.2491162298216,80.2));
#98580=CARTESIAN_POINT('Origin',(110.,18.,80.2));
#98581=CARTESIAN_POINT('',(103.211774900609,24.7882250993908,80.6));
#98582=CARTESIAN_POINT('Ctrl Pts',(103.111581176602,25.2491162298216,80.2));
#98583=CARTESIAN_POINT('Ctrl Pts',(103.162700423545,25.013967693886,80.4056749851146));
#98584=CARTESIAN_POINT('Ctrl Pts',(103.211774900609,24.7882250993908,80.6));
#98585=CARTESIAN_POINT('',(102.750883770178,24.8884188233975,80.2));
#98586=CARTESIAN_POINT('Ctrl Pts',(103.211774900609,24.7882250993908,80.6));
#98587=CARTESIAN_POINT('Ctrl Pts',(102.986032306113,24.8372995764552,80.4056749851138));
#98588=CARTESIAN_POINT('Ctrl Pts',(102.750883770178,24.8884188233975,80.2));
#98589=CARTESIAN_POINT('',(102.062377423568,24.0822814662025,80.2));
#98590=CARTESIAN_POINT('Origin',(110.,18.,80.2));
#98591=CARTESIAN_POINT('',(102.233436854001,23.6427384220077,80.6));
#98592=CARTESIAN_POINT('Ctrl Pts',(102.062377423568,24.0822814662025,80.2));
#98593=CARTESIAN_POINT('Ctrl Pts',(102.149652643176,23.8580248110016,80.4056749851128));
#98594=CARTESIAN_POINT('Ctrl Pts',(102.233436854001,23.6427384220077,80.6));
#98595=CARTESIAN_POINT('',(101.762546306575,23.6695993375792,80.2));
#98596=CARTESIAN_POINT('Ctrl Pts',(102.233436854001,23.6427384220077,80.6));
#98597=CARTESIAN_POINT('Ctrl Pts',(102.002796585873,23.6558947888183,80.4056749851127));
#98598=CARTESIAN_POINT('Ctrl Pts',(101.762546306575,23.6695993375792,80.2));
#98599=CARTESIAN_POINT('',(101.208624281823,22.7656807469507,80.2));
#98600=CARTESIAN_POINT('Origin',(110.,18.,80.2));
#98601=CARTESIAN_POINT('',(101.446337367792,22.3583087974996,80.6));
#98602=CARTESIAN_POINT('Ctrl Pts',(101.208624281823,22.7656807469507,80.2));
#98603=CARTESIAN_POINT('Ctrl Pts',(101.329906468542,22.5578379155986,80.4056749851127));
#98604=CARTESIAN_POINT('Ctrl Pts',(101.446337367792,22.3583087974996,80.6));
#98605=CARTESIAN_POINT('',(100.977042291445,22.3111754997483,80.2));
#98606=CARTESIAN_POINT('Ctrl Pts',(101.446337367792,22.3583087974996,80.6));
#98607=CARTESIAN_POINT('Ctrl Pts',(101.216478554888,22.3352231006419,80.405674985114));
#98608=CARTESIAN_POINT('Ctrl Pts',(100.977042291445,22.3111754997483,80.2));
#98609=CARTESIAN_POINT('',(100.571343987164,21.3317331513213,80.2));
#98610=CARTESIAN_POINT('Origin',(110.,18.,80.2));
#98611=CARTESIAN_POINT('',(100.869857443567,20.9665631459995,80.6));
#98612=CARTESIAN_POINT('Ctrl Pts',(100.571343987164,21.3317331513213,80.2));
#98613=CARTESIAN_POINT('Ctrl Pts',(100.723646771043,21.145421924116,80.4056749851135));
#98614=CARTESIAN_POINT('Ctrl Pts',(100.869857443567,20.9665631459995,80.6));
#98615=CARTESIAN_POINT('',(100.41371344058,20.8465962131424,80.2));
#98616=CARTESIAN_POINT('Ctrl Pts',(100.869857443567,20.9665631459995,80.6));
#98617=CARTESIAN_POINT('Ctrl Pts',(100.646439972715,20.9078038319469,80.4056749851127));
#98618=CARTESIAN_POINT('Ctrl Pts',(100.41371344058,20.8465962131424,80.2));
#98619=CARTESIAN_POINT('',(100.166228495456,19.815747228118,80.2));
#98620=CARTESIAN_POINT('Origin',(110.,18.,80.2));
#98621=CARTESIAN_POINT('',(100.518191930287,19.5017708643862,80.6));
#98622=CARTESIAN_POINT('Ctrl Pts',(100.166228495456,19.815747228118,80.2));
#98623=CARTESIAN_POINT('Ctrl Pts',(100.345801676492,19.655555205806,80.4056749851131));
#98624=CARTESIAN_POINT('Ctrl Pts',(100.518191930287,19.5017708643862,80.6));
#98625=CARTESIAN_POINT('',(100.086430779868,19.3119242804578,80.2));
#98626=CARTESIAN_POINT('Ctrl Pts',(100.518191930287,19.5017708643862,80.6));
#98627=CARTESIAN_POINT('Ctrl Pts',(100.306717081102,19.4087847824621,80.4056749851134));
#98628=CARTESIAN_POINT('Ctrl Pts',(100.086430779868,19.3119242804578,80.2));
#98629=CARTESIAN_POINT('',(100.003253094606,18.2550515820388,80.2));
#98630=CARTESIAN_POINT('Origin',(110.,18.,80.2));
#98631=CARTESIAN_POINT('Ctrl Pts',(100.003253094606,18.2550515820388,80.2));
#98632=CARTESIAN_POINT('Ctrl Pts',(100.205674985113,18.1249232238562,80.4056749851126));
#98633=CARTESIAN_POINT('Ctrl Pts',(100.4,18.,80.6));
#98634=CARTESIAN_POINT('Origin',(118.553662632208,13.6416912025004,81.));
#98635=CARTESIAN_POINT('',(118.553662632208,13.6416912025004,81.));
#98636=CARTESIAN_POINT('Origin',(118.973071474257,12.9229449167979,81.));
#98637=CARTESIAN_POINT('',(118.791375718177,13.2343192530493,73.5));
#98638=CARTESIAN_POINT('Origin',(117.766563145999,12.3572615779923,81.));
#98639=CARTESIAN_POINT('',(117.766563145999,12.3572615779923,81.));
#98640=CARTESIAN_POINT('',(118.237453693425,12.3304006624208,73.5));
#98641=CARTESIAN_POINT('Origin',(118.06837167853,11.5817542539188,81.));
#98642=CARTESIAN_POINT('',(117.937622576432,11.9177185337975,73.5));
#98643=CARTESIAN_POINT('Origin',(110.,18.,73.5));
#98644=CARTESIAN_POINT('',(117.249116229822,11.1115811766025,73.5));
#98645=CARTESIAN_POINT('Origin',(110.,18.,73.5));
#98646=CARTESIAN_POINT('Origin',(116.965001794687,10.3986021022446,81.));
#98647=CARTESIAN_POINT('',(116.788225099391,11.2117749006091,81.));
#98648=CARTESIAN_POINT('',(116.888418823398,10.7508837701784,73.5));
#98649=CARTESIAN_POINT('Origin',(116.788225099391,11.2117749006091,81.));
#98650=CARTESIAN_POINT('Origin',(110.,18.,73.5));
#98651=CARTESIAN_POINT('',(116.082281466203,10.0623774235676,73.5));
#98652=CARTESIAN_POINT('Origin',(115.642738422008,10.2334368540005,81.));
#98653=CARTESIAN_POINT('',(115.642738422008,10.2334368540005,81.));
#98654=CARTESIAN_POINT('Origin',(115.690130451144,9.40262159440644,81.));
#98655=CARTESIAN_POINT('',(115.669599337579,9.762546306575,73.5));
#98656=CARTESIAN_POINT('Origin',(114.3583087975,9.44633736779169,81.));
#98657=CARTESIAN_POINT('',(114.3583087975,9.44633736779169,81.));
#98658=CARTESIAN_POINT('',(114.765680746951,9.20862428182348,73.5));
#98659=CARTESIAN_POINT('Origin',(114.275149211433,8.61833707597702,81.));
#98660=CARTESIAN_POINT('',(114.311175499748,8.97704229144512,73.5));
#98661=CARTESIAN_POINT('Origin',(110.,18.,73.5));
#98662=CARTESIAN_POINT('',(113.331733151321,8.57134398716408,73.5));
#98663=CARTESIAN_POINT('Origin',(110.,18.,73.5));
#98664=CARTESIAN_POINT('Origin',(112.754899609729,8.06506023469121,81.));
#98665=CARTESIAN_POINT('',(112.966563146,8.86985744356654,81.));
#98666=CARTESIAN_POINT('',(112.846596213142,8.41371344057965,73.5));
#98667=CARTESIAN_POINT('Origin',(112.966563146,8.86985744356654,81.));
#98668=CARTESIAN_POINT('Origin',(110.,18.,73.5));
#98669=CARTESIAN_POINT('',(111.815747228118,8.16622849545598,73.5));
#98670=CARTESIAN_POINT('Origin',(111.501770864386,8.51819193028669,81.));
#98671=CARTESIAN_POINT('',(111.501770864386,8.51819193028669,81.));
#98672=CARTESIAN_POINT('Origin',(111.166815236647,7.75641458260198,81.));
#98673=CARTESIAN_POINT('',(111.311924280458,8.08643077986816,73.5));
#98674=CARTESIAN_POINT('Origin',(110.,8.40000000000002,81.));
#98675=CARTESIAN_POINT('',(110.,8.40000000000002,81.));
#98676=CARTESIAN_POINT('',(110.255051582039,8.00325309460625,73.5));
#98677=CARTESIAN_POINT('Origin',(109.55,7.70000000000001,81.));
#98678=CARTESIAN_POINT('',(109.744948417961,8.00325309460625,73.5));
#98679=CARTESIAN_POINT('Origin',(110.,18.,73.5));
#98680=CARTESIAN_POINT('',(108.688075719542,8.08643077986816,73.5));
#98681=CARTESIAN_POINT('Origin',(110.,18.,73.5));
#98682=CARTESIAN_POINT('Origin',(107.944265256818,7.89720560113819,81.));
#98683=CARTESIAN_POINT('',(108.498229135614,8.51819193028669,81.));
#98684=CARTESIAN_POINT('',(108.184252771882,8.16622849545598,73.5));
#98685=CARTESIAN_POINT('Origin',(108.498229135614,8.51819193028669,81.));
#98686=CARTESIAN_POINT('Origin',(110.,18.,73.5));
#98687=CARTESIAN_POINT('',(107.153403786858,8.41371344057964,73.5));
#98688=CARTESIAN_POINT('Origin',(107.033436854001,8.86985744356654,81.));
#98689=CARTESIAN_POINT('',(107.033436854001,8.86985744356654,81.));
#98690=CARTESIAN_POINT('Origin',(106.389149525605,8.34317552962865,81.));
#98691=CARTESIAN_POINT('',(106.668266848679,8.57134398716408,73.5));
#98692=CARTESIAN_POINT('Origin',(105.6416912025,9.44633736779169,81.));
#98693=CARTESIAN_POINT('',(105.6416912025,9.44633736779169,81.));
#98694=CARTESIAN_POINT('',(105.688824500252,8.97704229144512,73.5));
#98695=CARTESIAN_POINT('Origin',(104.922944916798,9.02692852574262,81.));
#98696=CARTESIAN_POINT('',(105.234319253049,9.20862428182348,73.5));
#98697=CARTESIAN_POINT('Origin',(110.,18.,73.5));
#98698=CARTESIAN_POINT('',(104.330400662421,9.76254630657499,73.5));
#98699=CARTESIAN_POINT('Origin',(110.,18.,73.5));
#98700=CARTESIAN_POINT('Origin',(103.581754253919,9.93162832146966,81.));
#98701=CARTESIAN_POINT('',(104.357261577992,10.2334368540005,81.));
#98702=CARTESIAN_POINT('',(103.917718533797,10.0623774235676,73.5));
#98703=CARTESIAN_POINT('Origin',(104.357261577992,10.2334368540005,81.));
#98704=CARTESIAN_POINT('Origin',(110.,18.,73.5));
#98705=CARTESIAN_POINT('',(103.111581176602,10.7508837701784,73.5));
#98706=CARTESIAN_POINT('Origin',(103.211774900609,11.2117749006092,81.));
#98707=CARTESIAN_POINT('',(103.211774900609,11.2117749006092,81.));
#98708=CARTESIAN_POINT('Origin',(102.398602102245,11.0349982053125,81.));
#98709=CARTESIAN_POINT('',(102.750883770178,11.1115811766025,73.5));
#98710=CARTESIAN_POINT('Origin',(102.233436854001,12.3572615779923,81.));
#98711=CARTESIAN_POINT('',(102.233436854001,12.3572615779923,81.));
#98712=CARTESIAN_POINT('',(102.062377423568,11.9177185337975,73.5));
#98713=CARTESIAN_POINT('Origin',(101.402621594406,12.3098695488563,81.));
#98714=CARTESIAN_POINT('',(101.762546306575,12.3304006624208,73.5));
#98715=CARTESIAN_POINT('Origin',(110.,18.,73.5));
#98716=CARTESIAN_POINT('',(101.208624281823,13.2343192530494,73.5));
#98717=CARTESIAN_POINT('Origin',(110.,18.,73.5));
#98718=CARTESIAN_POINT('Origin',(100.618337075977,13.7248507885675,81.));
#98719=CARTESIAN_POINT('',(101.446337367792,13.6416912025004,81.));
#98720=CARTESIAN_POINT('',(100.977042291445,13.6888245002517,73.5));
#98721=CARTESIAN_POINT('Origin',(101.446337367792,13.6416912025004,81.));
#98722=CARTESIAN_POINT('Origin',(110.,18.,73.5));
#98723=CARTESIAN_POINT('',(100.571343987164,14.6682668486788,73.5));
#98724=CARTESIAN_POINT('Origin',(100.869857443567,15.0334368540005,81.));
#98725=CARTESIAN_POINT('',(100.869857443567,15.0334368540005,81.));
#98726=CARTESIAN_POINT('Origin',(100.065060234691,15.2451003902709,81.));
#98727=CARTESIAN_POINT('',(100.41371344058,15.1534037868576,73.5));
#98728=CARTESIAN_POINT('Origin',(100.518191930287,16.4982291356138,81.));
#98729=CARTESIAN_POINT('',(100.518191930287,16.4982291356138,81.));
#98730=CARTESIAN_POINT('',(100.166228495456,16.184252771882,73.5));
#98731=CARTESIAN_POINT('Origin',(99.756414582602,16.8331847633534,81.));
#98732=CARTESIAN_POINT('',(100.086430779868,16.6880757195422,73.5));
#98733=CARTESIAN_POINT('Origin',(110.,18.,73.5));
#98734=CARTESIAN_POINT('',(100.003253094606,17.7449484179612,73.5));
#98735=CARTESIAN_POINT('Origin',(110.,18.,73.5));
#98736=CARTESIAN_POINT('Origin',(99.7,18.45,81.));
#98737=CARTESIAN_POINT('',(100.4,18.,81.));
#98738=CARTESIAN_POINT('',(100.003253094606,18.2550515820388,73.5));
#98739=CARTESIAN_POINT('Origin',(100.4,18.,81.));
#98740=CARTESIAN_POINT('Origin',(110.,18.,73.5));
#98741=CARTESIAN_POINT('',(100.086430779868,19.3119242804578,73.5));
#98742=CARTESIAN_POINT('Origin',(100.518191930287,19.5017708643862,81.));
#98743=CARTESIAN_POINT('',(100.518191930287,19.5017708643862,81.));
#98744=CARTESIAN_POINT('Origin',(99.8972056011382,20.0557347431822,81.));
#98745=CARTESIAN_POINT('',(100.166228495456,19.815747228118,73.5));
#98746=CARTESIAN_POINT('Origin',(100.869857443567,20.9665631459995,81.));
#98747=CARTESIAN_POINT('',(100.869857443567,20.9665631459995,81.));
#98748=CARTESIAN_POINT('',(100.41371344058,20.8465962131424,73.5));
#98749=CARTESIAN_POINT('Origin',(100.343175529629,21.6108504743948,81.));
#98750=CARTESIAN_POINT('',(100.571343987164,21.3317331513213,73.5));
#98751=CARTESIAN_POINT('Origin',(110.,18.,73.5));
#98752=CARTESIAN_POINT('',(100.977042291445,22.3111754997483,73.5));
#98753=CARTESIAN_POINT('Origin',(110.,18.,73.5));
#98754=CARTESIAN_POINT('Origin',(101.026928525743,23.0770550832021,81.));
#98755=CARTESIAN_POINT('',(101.446337367792,22.3583087974996,81.));
#98756=CARTESIAN_POINT('',(101.208624281823,22.7656807469507,73.5));
#98757=CARTESIAN_POINT('Origin',(101.446337367792,22.3583087974996,81.));
#98758=CARTESIAN_POINT('Origin',(110.,18.,73.5));
#98759=CARTESIAN_POINT('',(101.762546306575,23.6695993375792,73.5));
#98760=CARTESIAN_POINT('Origin',(102.233436854001,23.6427384220077,81.));
#98761=CARTESIAN_POINT('',(102.233436854001,23.6427384220077,81.));
#98762=CARTESIAN_POINT('Origin',(101.93162832147,24.4182457460812,81.));
#98763=CARTESIAN_POINT('',(102.062377423568,24.0822814662025,73.5));
#98764=CARTESIAN_POINT('Origin',(103.211774900609,24.7882250993908,81.));
#98765=CARTESIAN_POINT('',(103.211774900609,24.7882250993908,81.));
#98766=CARTESIAN_POINT('',(102.750883770178,24.8884188233975,73.5));
#98767=CARTESIAN_POINT('Origin',(103.034998205313,25.6013978977554,81.));
#98768=CARTESIAN_POINT('',(103.111581176602,25.2491162298216,73.5));
#98769=CARTESIAN_POINT('Origin',(110.,18.,73.5));
#98770=CARTESIAN_POINT('',(103.917718533797,25.9376225764324,73.5));
#98771=CARTESIAN_POINT('Origin',(110.,18.,73.5));
#98772=CARTESIAN_POINT('Origin',(104.309869548856,26.5973784055936,81.));
#98773=CARTESIAN_POINT('',(104.357261577992,25.7665631459995,81.));
#98774=CARTESIAN_POINT('',(104.330400662421,26.237453693425,73.5));
#98775=CARTESIAN_POINT('Origin',(104.357261577992,25.7665631459995,81.));
#98776=CARTESIAN_POINT('Origin',(110.,18.,73.5));
#98777=CARTESIAN_POINT('',(105.234319253049,26.7913757181765,73.5));
#98778=CARTESIAN_POINT('Origin',(105.6416912025,26.5536626322083,81.));
#98779=CARTESIAN_POINT('',(105.6416912025,26.5536626322083,81.));
#98780=CARTESIAN_POINT('Origin',(105.724850788567,27.381662924023,81.));
#98781=CARTESIAN_POINT('',(105.688824500252,27.0229577085549,73.5));
#98782=CARTESIAN_POINT('Origin',(107.033436854,27.1301425564335,81.));
#98783=CARTESIAN_POINT('',(107.033436854,27.1301425564335,81.));
#98784=CARTESIAN_POINT('',(106.668266848679,27.4286560128359,73.5));
#98785=CARTESIAN_POINT('Origin',(107.245100390271,27.9349397653088,81.));
#98786=CARTESIAN_POINT('',(107.153403786858,27.5862865594204,73.5));
#98787=CARTESIAN_POINT('Origin',(110.,18.,73.5));
#98788=CARTESIAN_POINT('',(108.184252771882,27.833771504544,73.5));
#98789=CARTESIAN_POINT('Origin',(110.,18.,73.5));
#98790=CARTESIAN_POINT('Origin',(108.833184763353,28.243585417398,81.));
#98791=CARTESIAN_POINT('',(108.498229135614,27.4818080697133,81.));
#98792=CARTESIAN_POINT('',(108.688075719542,27.9135692201318,73.5));
#98793=CARTESIAN_POINT('Origin',(108.498229135614,27.4818080697133,81.));
#98794=CARTESIAN_POINT('Origin',(110.,18.,73.5));
#98795=CARTESIAN_POINT('',(109.744948417961,27.9967469053937,73.5));
#98796=CARTESIAN_POINT('Origin',(110.,27.6,81.));
#98797=CARTESIAN_POINT('',(110.,27.6,81.));
#98798=CARTESIAN_POINT('Origin',(110.45,28.3,81.));
#98799=CARTESIAN_POINT('',(110.255051582039,27.9967469053937,73.5));
#98800=CARTESIAN_POINT('Origin',(111.501770864386,27.4818080697133,81.));
#98801=CARTESIAN_POINT('',(111.501770864386,27.4818080697133,81.));
#98802=CARTESIAN_POINT('',(111.311924280458,27.9135692201318,73.5));
#98803=CARTESIAN_POINT('Origin',(112.055734743182,28.1027943988618,81.));
#98804=CARTESIAN_POINT('',(111.815747228118,27.833771504544,73.5));
#98805=CARTESIAN_POINT('Origin',(110.,18.,73.5));
#98806=CARTESIAN_POINT('',(112.846596213142,27.5862865594204,73.5));
#98807=CARTESIAN_POINT('Origin',(110.,18.,73.5));
#98808=CARTESIAN_POINT('Origin',(113.610850474395,27.6568244703713,81.));
#98809=CARTESIAN_POINT('',(112.966563146,27.1301425564335,81.));
#98810=CARTESIAN_POINT('',(113.331733151321,27.4286560128359,73.5));
#98811=CARTESIAN_POINT('Origin',(112.966563146,27.1301425564335,81.));
#98812=CARTESIAN_POINT('Origin',(110.,18.,73.5));
#98813=CARTESIAN_POINT('',(114.311175499748,27.0229577085549,73.5));
#98814=CARTESIAN_POINT('Origin',(114.3583087975,26.5536626322083,81.));
#98815=CARTESIAN_POINT('',(114.3583087975,26.5536626322083,81.));
#98816=CARTESIAN_POINT('Origin',(115.077055083202,26.9730714742574,81.));
#98817=CARTESIAN_POINT('',(114.765680746951,26.7913757181765,73.5));
#98818=CARTESIAN_POINT('Origin',(115.642738422008,25.7665631459995,81.));
#98819=CARTESIAN_POINT('',(115.642738422008,25.7665631459995,81.));
#98820=CARTESIAN_POINT('',(115.669599337579,26.237453693425,73.5));
#98821=CARTESIAN_POINT('Origin',(116.418245746081,26.0683716785304,81.));
#98822=CARTESIAN_POINT('',(116.082281466203,25.9376225764324,73.5));
#98823=CARTESIAN_POINT('Origin',(110.,18.,73.5));
#98824=CARTESIAN_POINT('',(116.888418823398,25.2491162298216,73.5));
#98825=CARTESIAN_POINT('Origin',(110.,18.,73.5));
#98826=CARTESIAN_POINT('Origin',(117.601397897755,24.9650017946875,81.));
#98827=CARTESIAN_POINT('',(116.788225099391,24.7882250993908,81.));
#98828=CARTESIAN_POINT('',(117.249116229822,24.8884188233975,73.5));
#98829=CARTESIAN_POINT('Origin',(116.788225099391,24.7882250993908,81.));
#98830=CARTESIAN_POINT('Origin',(110.,18.,73.5));
#98831=CARTESIAN_POINT('',(117.937622576432,24.0822814662025,73.5));
#98832=CARTESIAN_POINT('Origin',(117.766563145999,23.6427384220077,81.));
#98833=CARTESIAN_POINT('',(117.766563145999,23.6427384220077,81.));
#98834=CARTESIAN_POINT('Origin',(118.597378405594,23.6901304511437,81.));
#98835=CARTESIAN_POINT('',(118.237453693425,23.6695993375792,73.5));
#98836=CARTESIAN_POINT('Origin',(118.553662632208,22.3583087974996,81.));
#98837=CARTESIAN_POINT('',(118.553662632208,22.3583087974996,81.));
#98838=CARTESIAN_POINT('',(118.791375718177,22.7656807469507,73.5));
#98839=CARTESIAN_POINT('Origin',(119.381662924023,22.2751492114326,81.));
#98840=CARTESIAN_POINT('',(119.022957708555,22.3111754997483,73.5));
#98841=CARTESIAN_POINT('Origin',(110.,18.,73.5));
#98842=CARTESIAN_POINT('',(119.428656012836,21.3317331513213,73.5));
#98843=CARTESIAN_POINT('Origin',(110.,18.,73.5));
#98844=CARTESIAN_POINT('Origin',(119.934939765309,20.7548996097291,81.));
#98845=CARTESIAN_POINT('',(119.130142556433,20.9665631459995,81.));
#98846=CARTESIAN_POINT('',(119.58628655942,20.8465962131424,73.5));
#98847=CARTESIAN_POINT('Origin',(119.130142556433,20.9665631459995,81.));
#98848=CARTESIAN_POINT('Origin',(110.,18.,73.5));
#98849=CARTESIAN_POINT('',(119.833771504544,19.815747228118,73.5));
#98850=CARTESIAN_POINT('Origin',(119.481808069713,19.5017708643862,81.));
#98851=CARTESIAN_POINT('',(119.481808069713,19.5017708643862,81.));
#98852=CARTESIAN_POINT('Origin',(120.243585417398,19.1668152366466,81.));
#98853=CARTESIAN_POINT('',(119.913569220132,19.3119242804578,73.5));
#98854=CARTESIAN_POINT('Origin',(119.6,18.,81.));
#98855=CARTESIAN_POINT('',(119.6,18.,81.));
#98856=CARTESIAN_POINT('',(119.996746905394,18.2550515820388,73.5));
#98857=CARTESIAN_POINT('Origin',(120.3,17.55,81.));
#98858=CARTESIAN_POINT('Origin',(110.,18.,49.85));
#98859=CARTESIAN_POINT('',(107.49,18.,50.));
#98860=CARTESIAN_POINT('Origin',(110.,18.,50.));
#98861=CARTESIAN_POINT('',(107.19,18.,49.7));
#98862=CARTESIAN_POINT('',(107.34,18.,49.85));
#98863=CARTESIAN_POINT('Origin',(110.,18.,49.7));
#98864=CARTESIAN_POINT('Origin',(113.7,18.,49.7));
#98865=CARTESIAN_POINT('',(106.3,18.,49.7));
#98866=CARTESIAN_POINT('Origin',(110.,18.,49.7));
#98867=CARTESIAN_POINT('Origin',(110.,18.,49.85));
#98868=CARTESIAN_POINT('',(106.,18.,50.));
#98869=CARTESIAN_POINT('Origin',(110.,18.,50.));
#98870=CARTESIAN_POINT('',(106.15,18.,49.85));
#98871=CARTESIAN_POINT('Origin',(110.,18.,54.8));
#98872=CARTESIAN_POINT('',(106.,18.,59.6));
#98873=CARTESIAN_POINT('Origin',(110.,18.,59.6));
#98874=CARTESIAN_POINT('',(106.,18.,54.8));
#98875=CARTESIAN_POINT('Origin',(110.,18.,59.8));
#98876=CARTESIAN_POINT('',(105.6,18.,60.));
#98877=CARTESIAN_POINT('Origin',(110.,18.,60.));
#98878=CARTESIAN_POINT('',(105.8,18.,59.8));
#98879=CARTESIAN_POINT('Origin',(116.,18.,60.));
#98880=CARTESIAN_POINT('',(104.,18.,60.));
#98881=CARTESIAN_POINT('Origin',(110.,18.,60.));
#98882=CARTESIAN_POINT('Origin',(110.,18.,62.8));
#98883=CARTESIAN_POINT('',(104.,18.,65.6));
#98884=CARTESIAN_POINT('Origin',(110.,18.,65.6));
#98885=CARTESIAN_POINT('',(104.,18.,62.8));
#98886=CARTESIAN_POINT('Origin',(110.,18.,65.8));
#98887=CARTESIAN_POINT('',(103.6,18.,66.));
#98888=CARTESIAN_POINT('Origin',(110.,18.,66.));
#98889=CARTESIAN_POINT('',(103.8,18.,65.8));
#98890=CARTESIAN_POINT('Origin',(119.2,18.,66.));
#98891=CARTESIAN_POINT('Origin',(110.,18.,73.5));
#98892=CARTESIAN_POINT('Origin',(117.4,18.,81.));
#98893=CARTESIAN_POINT('',(102.6,18.,81.));
#98894=CARTESIAN_POINT('Origin',(110.,18.,81.));
#98895=CARTESIAN_POINT('Origin',(110.,18.,80.8));
#98896=CARTESIAN_POINT('',(103.,18.,80.6));
#98897=CARTESIAN_POINT('',(102.8,18.,80.8));
#98898=CARTESIAN_POINT('Origin',(110.,18.,80.6));
#98899=CARTESIAN_POINT('Origin',(110.,18.,80.6));
#98900=CARTESIAN_POINT('Origin',(110.,18.,78.85));
#98901=CARTESIAN_POINT('',(110.,18.,79.6));
#98902=CARTESIAN_POINT('',(107.49,18.,78.1));
#98903=CARTESIAN_POINT('',(108.745,18.,78.85));
#98904=CARTESIAN_POINT('Origin',(110.,18.,78.1));
#98905=CARTESIAN_POINT('Origin',(110.,18.,64.05));
#98906=CARTESIAN_POINT('',(107.49,18.,64.05));
#98907=CARTESIAN_POINT('',(0.,0.,0.));
#98908=CARTESIAN_POINT('Origin',(110.,18.,40.65));
#98909=CARTESIAN_POINT('',(107.49,18.,40.8));
#98910=CARTESIAN_POINT('Origin',(110.,18.,40.8));
#98911=CARTESIAN_POINT('',(107.19,18.,40.5));
#98912=CARTESIAN_POINT('',(107.34,18.,40.65));
#98913=CARTESIAN_POINT('Origin',(110.,18.,40.5));
#98914=CARTESIAN_POINT('Origin',(114.5,18.,40.5));
#98915=CARTESIAN_POINT('',(105.5,18.,40.5));
#98916=CARTESIAN_POINT('Origin',(110.,18.,40.5));
#98917=CARTESIAN_POINT('Origin',(110.,18.,40.65));
#98918=CARTESIAN_POINT('',(105.2,18.,40.8));
#98919=CARTESIAN_POINT('Origin',(110.,18.,40.8));
#98920=CARTESIAN_POINT('',(105.35,18.,40.65));
#98921=CARTESIAN_POINT('Origin',(110.,18.,44.65));
#98922=CARTESIAN_POINT('',(105.2,18.,48.5));
#98923=CARTESIAN_POINT('Origin',(110.,18.,48.5));
#98924=CARTESIAN_POINT('',(105.2,18.,44.65));
#98925=CARTESIAN_POINT('Origin',(115.7,18.,48.5));
#98926=CARTESIAN_POINT('',(104.3,18.,48.5));
#98927=CARTESIAN_POINT('Origin',(110.,18.,48.5));
#98928=CARTESIAN_POINT('Origin',(110.,18.,48.65));
#98929=CARTESIAN_POINT('',(104.,18.,48.8));
#98930=CARTESIAN_POINT('Origin',(110.,18.,48.8));
#98931=CARTESIAN_POINT('',(104.15,18.,48.65));
#98932=CARTESIAN_POINT('Origin',(110.,18.,49.15));
#98933=CARTESIAN_POINT('',(104.,18.,49.5));
#98934=CARTESIAN_POINT('Origin',(110.,18.,49.5));
#98935=CARTESIAN_POINT('',(104.,18.,49.15));
#98936=CARTESIAN_POINT('Origin',(112.81,18.,49.5));
#98937=CARTESIAN_POINT('',(107.19,18.,49.5));
#98938=CARTESIAN_POINT('Origin',(110.,18.,49.5));
#98939=CARTESIAN_POINT('Origin',(110.,18.,49.35));
#98940=CARTESIAN_POINT('',(107.49,18.,49.2));
#98941=CARTESIAN_POINT('',(107.34,18.,49.35));
#98942=CARTESIAN_POINT('Origin',(110.,18.,49.2));
#98943=CARTESIAN_POINT('Origin',(110.,18.,45.));
#98944=CARTESIAN_POINT('',(107.49,18.,45.));
#98945=CARTESIAN_POINT('',(0.,0.,0.));
#98946=CARTESIAN_POINT('Origin',(214.,14.3,28.5));
#98947=CARTESIAN_POINT('',(211.2,14.45,28.5));
#98948=CARTESIAN_POINT('Origin',(214.,14.45,28.5));
#98949=CARTESIAN_POINT('',(211.5,14.15,28.5));
#98950=CARTESIAN_POINT('',(211.35,14.3,28.5));
#98951=CARTESIAN_POINT('Origin',(214.,14.15,28.5));
#98952=CARTESIAN_POINT('Origin',(214.,14.45,28.5));
#98953=CARTESIAN_POINT('',(211.5,11.5,28.5));
#98954=CARTESIAN_POINT('',(211.5,14.45,28.5));
#98955=CARTESIAN_POINT('Origin',(214.,11.5,28.5));
#98956=CARTESIAN_POINT('Origin',(218.,14.45,25.5));
#98957=CARTESIAN_POINT('',(218.,14.45,25.5));
#98958=CARTESIAN_POINT('',(207.955857948402,14.45,25.5));
#98959=CARTESIAN_POINT('',(218.,14.45,25.5));
#98960=CARTESIAN_POINT('',(207.955857948402,14.45,31.5));
#98961=CARTESIAN_POINT('',(207.955857948402,14.45,25.5));
#98962=CARTESIAN_POINT('',(218.,14.45,31.5));
#98963=CARTESIAN_POINT('',(218.,14.45,31.5));
#98964=CARTESIAN_POINT('',(218.,14.45,25.5));
#98965=CARTESIAN_POINT('Origin',(6.,14.3,28.5));
#98966=CARTESIAN_POINT('',(3.2,14.45,28.5));
#98967=CARTESIAN_POINT('Origin',(6.,14.45,28.5));
#98968=CARTESIAN_POINT('',(3.5,14.15,28.5));
#98969=CARTESIAN_POINT('',(3.35,14.3,28.5));
#98970=CARTESIAN_POINT('Origin',(6.,14.15,28.5));
#98971=CARTESIAN_POINT('Origin',(6.,14.45,28.5));
#98972=CARTESIAN_POINT('',(3.5,11.5,28.5));
#98973=CARTESIAN_POINT('',(3.5,14.45,28.5));
#98974=CARTESIAN_POINT('Origin',(6.,11.5,28.5));
#98975=CARTESIAN_POINT('Origin',(12.0441420515979,14.45,25.5));
#98976=CARTESIAN_POINT('',(12.0441420515979,14.45,25.5));
#98977=CARTESIAN_POINT('',(2.,14.45,25.5));
#98978=CARTESIAN_POINT('',(12.0441420515979,14.45,25.5));
#98979=CARTESIAN_POINT('',(2.,14.45,31.5));
#98980=CARTESIAN_POINT('',(2.,14.45,25.5));
#98981=CARTESIAN_POINT('',(12.0441420515979,14.45,31.5));
#98982=CARTESIAN_POINT('',(12.0441420515979,14.45,31.5));
#98983=CARTESIAN_POINT('',(12.0441420515979,14.45,25.5));
#98984=CARTESIAN_POINT('Origin',(6.,11.5,28.5));
#98985=CARTESIAN_POINT('',(4.55,11.5,28.5));
#98986=CARTESIAN_POINT('Origin',(6.,11.5,28.5));
#98987=CARTESIAN_POINT('Origin',(214.,11.5,28.5));
#98988=CARTESIAN_POINT('',(212.55,11.5,28.5));
#98989=CARTESIAN_POINT('Origin',(214.,11.5,28.5));
#98990=CARTESIAN_POINT('Origin',(6.,14.45,28.5));
#98991=CARTESIAN_POINT('',(4.55,9.5,28.5));
#98992=CARTESIAN_POINT('',(4.55,14.45,28.5));
#98993=CARTESIAN_POINT('Origin',(6.,9.5,28.5));
#98994=CARTESIAN_POINT('Origin',(214.,14.45,28.5));
#98995=CARTESIAN_POINT('',(212.55,9.5,28.5));
#98996=CARTESIAN_POINT('',(212.55,14.45,28.5));
#98997=CARTESIAN_POINT('Origin',(214.,9.5,28.5));
#98998=CARTESIAN_POINT('Origin',(56.,9.65,31.35));
#98999=CARTESIAN_POINT('',(218.,9.5,31.2));
#99000=CARTESIAN_POINT('',(218.,9.8,31.5));
#99001=CARTESIAN_POINT('',(218.,8.15,29.85));
#99002=CARTESIAN_POINT('',(2.,9.8,31.5));
#99003=CARTESIAN_POINT('',(56.,9.8,31.5));
#99004=CARTESIAN_POINT('',(2.,9.5,31.2));
#99005=CARTESIAN_POINT('',(2.,9.38750000000001,31.0875));
#99006=CARTESIAN_POINT('',(56.,9.5,31.2));
#99007=CARTESIAN_POINT('Origin',(218.,9.5,25.5));
#99008=CARTESIAN_POINT('',(218.,9.5,25.8));
#99009=CARTESIAN_POINT('',(218.,9.5,25.5));
#99010=CARTESIAN_POINT('',(218.,9.8,25.5));
#99011=CARTESIAN_POINT('',(218.,9.65,25.65));
#99012=CARTESIAN_POINT('',(218.,9.5,25.5));
#99013=CARTESIAN_POINT('',(218.,9.5,31.5));
#99014=CARTESIAN_POINT('Origin',(2.,9.5,25.5));
#99015=CARTESIAN_POINT('',(2.,9.5,25.8));
#99016=CARTESIAN_POINT('',(2.,9.5,25.5));
#99017=CARTESIAN_POINT('',(56.,9.5,25.8));
#99018=CARTESIAN_POINT('Origin',(56.,9.65,25.65));
#99019=CARTESIAN_POINT('',(2.,9.8,25.5));
#99020=CARTESIAN_POINT('',(2.,10.8875,24.4125));
#99021=CARTESIAN_POINT('',(56.,9.8,25.5));
#99022=CARTESIAN_POINT('Origin',(12.4354100534341,13.375,25.5));
#99023=CARTESIAN_POINT('',(12.4354100534341,13.375,25.5));
#99024=CARTESIAN_POINT('',(12.4354100534341,13.375,25.5));
#99025=CARTESIAN_POINT('',(12.4354100534341,13.375,31.5));
#99026=CARTESIAN_POINT('',(12.4354100534341,13.375,31.5));
#99027=CARTESIAN_POINT('',(12.4354100534341,13.375,25.5));
#99028=CARTESIAN_POINT('Origin',(12.7858454239988,13.375,25.5));
#99029=CARTESIAN_POINT('',(12.7858454239988,13.375,25.5));
#99030=CARTESIAN_POINT('',(12.7858454239988,13.375,25.5));
#99031=CARTESIAN_POINT('',(12.7858454239988,13.375,31.5));
#99032=CARTESIAN_POINT('',(12.7858454239988,13.375,31.5));
#99033=CARTESIAN_POINT('',(12.7858454239988,13.375,25.5));
#99034=CARTESIAN_POINT('Origin',(13.1771134258349,14.45,25.5));
#99035=CARTESIAN_POINT('',(13.1771134258349,14.45,25.5));
#99036=CARTESIAN_POINT('',(13.1771134258349,14.45,25.5));
#99037=CARTESIAN_POINT('',(13.1771134258349,14.45,31.5));
#99038=CARTESIAN_POINT('',(13.1771134258349,14.45,31.5));
#99039=CARTESIAN_POINT('',(13.1771134258349,14.45,25.5));
#99040=CARTESIAN_POINT('Origin',(13.6149383783928,14.45,25.5));
#99041=CARTESIAN_POINT('',(13.6149383783928,14.45,25.5));
#99042=CARTESIAN_POINT('',(13.6149383783928,14.45,25.5));
#99043=CARTESIAN_POINT('',(13.6149383783928,14.45,31.5));
#99044=CARTESIAN_POINT('',(13.6149383783928,14.45,31.5));
#99045=CARTESIAN_POINT('',(13.6149383783928,14.45,25.5));
#99046=CARTESIAN_POINT('Origin',(14.006206380229,13.375,25.5));
#99047=CARTESIAN_POINT('',(14.006206380229,13.375,25.5));
#99048=CARTESIAN_POINT('',(14.006206380229,13.375,25.5));
#99049=CARTESIAN_POINT('',(14.006206380229,13.375,31.5));
#99050=CARTESIAN_POINT('',(14.006206380229,13.375,31.5));
#99051=CARTESIAN_POINT('',(14.006206380229,13.375,25.5));
#99052=CARTESIAN_POINT('Origin',(14.3566417507937,13.375,25.5));
#99053=CARTESIAN_POINT('',(14.3566417507937,13.375,25.5));
#99054=CARTESIAN_POINT('',(14.3566417507937,13.375,25.5));
#99055=CARTESIAN_POINT('',(14.3566417507937,13.375,31.5));
#99056=CARTESIAN_POINT('',(14.3566417507937,13.375,31.5));
#99057=CARTESIAN_POINT('',(14.3566417507937,13.375,25.5));
#99058=CARTESIAN_POINT('Origin',(14.7479097526298,14.45,25.5));
#99059=CARTESIAN_POINT('',(14.7479097526298,14.45,25.5));
#99060=CARTESIAN_POINT('',(14.7479097526298,14.45,25.5));
#99061=CARTESIAN_POINT('',(14.7479097526298,14.45,31.5));
#99062=CARTESIAN_POINT('',(14.7479097526298,14.45,31.5));
#99063=CARTESIAN_POINT('',(14.7479097526298,14.45,25.5));
#99064=CARTESIAN_POINT('Origin',(15.1857347051877,14.45,25.5));
#99065=CARTESIAN_POINT('',(15.1857347051877,14.45,25.5));
#99066=CARTESIAN_POINT('',(15.1857347051877,14.45,25.5));
#99067=CARTESIAN_POINT('',(15.1857347051877,14.45,31.5));
#99068=CARTESIAN_POINT('',(15.1857347051877,14.45,31.5));
#99069=CARTESIAN_POINT('',(15.1857347051877,14.45,25.5));
#99070=CARTESIAN_POINT('Origin',(15.5770027070239,13.375,25.5));
#99071=CARTESIAN_POINT('',(15.5770027070239,13.375,25.5));
#99072=CARTESIAN_POINT('',(15.5770027070239,13.375,25.5));
#99073=CARTESIAN_POINT('',(15.5770027070239,13.375,31.5));
#99074=CARTESIAN_POINT('',(15.5770027070239,13.375,31.5));
#99075=CARTESIAN_POINT('',(15.5770027070239,13.375,25.5));
#99076=CARTESIAN_POINT('Origin',(15.9274380775886,13.375,25.5));
#99077=CARTESIAN_POINT('',(15.9274380775886,13.375,25.5));
#99078=CARTESIAN_POINT('',(15.9274380775886,13.375,25.5));
#99079=CARTESIAN_POINT('',(15.9274380775886,13.375,31.5));
#99080=CARTESIAN_POINT('',(15.9274380775886,13.375,31.5));
#99081=CARTESIAN_POINT('',(15.9274380775886,13.375,25.5));
#99082=CARTESIAN_POINT('Origin',(16.3187060794247,14.45,25.5));
#99083=CARTESIAN_POINT('',(16.3187060794247,14.45,25.5));
#99084=CARTESIAN_POINT('',(16.3187060794247,14.45,25.5));
#99085=CARTESIAN_POINT('',(16.3187060794247,14.45,31.5));
#99086=CARTESIAN_POINT('',(16.3187060794247,14.45,31.5));
#99087=CARTESIAN_POINT('',(16.3187060794247,14.45,25.5));
#99088=CARTESIAN_POINT('Origin',(16.7565310319826,14.45,25.5));
#99089=CARTESIAN_POINT('',(16.7565310319826,14.45,25.5));
#99090=CARTESIAN_POINT('',(16.7565310319826,14.45,25.5));
#99091=CARTESIAN_POINT('',(16.7565310319826,14.45,31.5));
#99092=CARTESIAN_POINT('',(16.7565310319826,14.45,31.5));
#99093=CARTESIAN_POINT('',(16.7565310319826,14.45,25.5));
#99094=CARTESIAN_POINT('Origin',(17.1477990338188,13.375,25.5));
#99095=CARTESIAN_POINT('',(17.1477990338188,13.375,25.5));
#99096=CARTESIAN_POINT('',(17.1477990338188,13.375,25.5));
#99097=CARTESIAN_POINT('',(17.1477990338188,13.375,31.5));
#99098=CARTESIAN_POINT('',(17.1477990338188,13.375,31.5));
#99099=CARTESIAN_POINT('',(17.1477990338188,13.375,25.5));
#99100=CARTESIAN_POINT('Origin',(17.4982344043835,13.375,25.5));
#99101=CARTESIAN_POINT('',(17.4982344043835,13.375,25.5));
#99102=CARTESIAN_POINT('',(17.4982344043835,13.375,25.5));
#99103=CARTESIAN_POINT('',(17.4982344043835,13.375,31.5));
#99104=CARTESIAN_POINT('',(17.4982344043835,13.375,31.5));
#99105=CARTESIAN_POINT('',(17.4982344043835,13.375,25.5));
#99106=CARTESIAN_POINT('Origin',(17.8895024062196,14.45,25.5));
#99107=CARTESIAN_POINT('',(17.8895024062196,14.45,25.5));
#99108=CARTESIAN_POINT('',(17.8895024062196,14.45,25.5));
#99109=CARTESIAN_POINT('',(17.8895024062196,14.45,31.5));
#99110=CARTESIAN_POINT('',(17.8895024062196,14.45,31.5));
#99111=CARTESIAN_POINT('',(17.8895024062196,14.45,25.5));
#99112=CARTESIAN_POINT('Origin',(18.3273273587775,14.45,25.5));
#99113=CARTESIAN_POINT('',(18.3273273587775,14.45,25.5));
#99114=CARTESIAN_POINT('',(18.3273273587775,14.45,25.5));
#99115=CARTESIAN_POINT('',(18.3273273587775,14.45,31.5));
#99116=CARTESIAN_POINT('',(18.3273273587775,14.45,31.5));
#99117=CARTESIAN_POINT('',(18.3273273587775,14.45,25.5));
#99118=CARTESIAN_POINT('Origin',(18.7185953606136,13.375,25.5));
#99119=CARTESIAN_POINT('',(18.7185953606136,13.375,25.5));
#99120=CARTESIAN_POINT('',(18.7185953606136,13.375,25.5));
#99121=CARTESIAN_POINT('',(18.7185953606136,13.375,31.5));
#99122=CARTESIAN_POINT('',(18.7185953606136,13.375,31.5));
#99123=CARTESIAN_POINT('',(18.7185953606136,13.375,25.5));
#99124=CARTESIAN_POINT('Origin',(19.0690307311783,13.375,25.5));
#99125=CARTESIAN_POINT('',(19.0690307311783,13.375,25.5));
#99126=CARTESIAN_POINT('',(19.0690307311783,13.375,25.5));
#99127=CARTESIAN_POINT('',(19.0690307311783,13.375,31.5));
#99128=CARTESIAN_POINT('',(19.0690307311783,13.375,31.5));
#99129=CARTESIAN_POINT('',(19.0690307311783,13.375,25.5));
#99130=CARTESIAN_POINT('Origin',(19.4602987330145,14.45,25.5));
#99131=CARTESIAN_POINT('',(19.4602987330145,14.45,25.5));
#99132=CARTESIAN_POINT('',(19.4602987330145,14.45,25.5));
#99133=CARTESIAN_POINT('',(19.4602987330145,14.45,31.5));
#99134=CARTESIAN_POINT('',(19.4602987330145,14.45,31.5));
#99135=CARTESIAN_POINT('',(19.4602987330145,14.45,25.5));
#99136=CARTESIAN_POINT('Origin',(19.8981236855724,14.45,25.5));
#99137=CARTESIAN_POINT('',(19.8981236855724,14.45,25.5));
#99138=CARTESIAN_POINT('',(19.8981236855724,14.45,25.5));
#99139=CARTESIAN_POINT('',(19.8981236855724,14.45,31.5));
#99140=CARTESIAN_POINT('',(19.8981236855724,14.45,31.5));
#99141=CARTESIAN_POINT('',(19.8981236855724,14.45,25.5));
#99142=CARTESIAN_POINT('Origin',(20.2893916874086,13.375,25.5));
#99143=CARTESIAN_POINT('',(20.2893916874086,13.375,25.5));
#99144=CARTESIAN_POINT('',(20.2893916874086,13.375,25.5));
#99145=CARTESIAN_POINT('',(20.2893916874086,13.375,31.5));
#99146=CARTESIAN_POINT('',(20.2893916874086,13.375,31.5));
#99147=CARTESIAN_POINT('',(20.2893916874086,13.375,25.5));
#99148=CARTESIAN_POINT('Origin',(20.6398270579732,13.375,25.5));
#99149=CARTESIAN_POINT('',(20.6398270579732,13.375,25.5));
#99150=CARTESIAN_POINT('',(20.6398270579732,13.375,25.5));
#99151=CARTESIAN_POINT('',(20.6398270579732,13.375,31.5));
#99152=CARTESIAN_POINT('',(20.6398270579732,13.375,31.5));
#99153=CARTESIAN_POINT('',(20.6398270579732,13.375,25.5));
#99154=CARTESIAN_POINT('Origin',(21.0310950598094,14.45,25.5));
#99155=CARTESIAN_POINT('',(21.0310950598094,14.45,25.5));
#99156=CARTESIAN_POINT('',(21.0310950598094,14.45,25.5));
#99157=CARTESIAN_POINT('',(21.0310950598094,14.45,31.5));
#99158=CARTESIAN_POINT('',(21.0310950598094,14.45,31.5));
#99159=CARTESIAN_POINT('',(21.0310950598094,14.45,25.5));
#99160=CARTESIAN_POINT('Origin',(21.4689200123673,14.45,25.5));
#99161=CARTESIAN_POINT('',(21.4689200123673,14.45,25.5));
#99162=CARTESIAN_POINT('',(21.4689200123673,14.45,25.5));
#99163=CARTESIAN_POINT('',(21.4689200123673,14.45,31.5));
#99164=CARTESIAN_POINT('',(21.4689200123673,14.45,31.5));
#99165=CARTESIAN_POINT('',(21.4689200123673,14.45,25.5));
#99166=CARTESIAN_POINT('Origin',(21.8601880142034,13.375,25.5));
#99167=CARTESIAN_POINT('',(21.8601880142034,13.375,25.5));
#99168=CARTESIAN_POINT('',(21.8601880142034,13.375,25.5));
#99169=CARTESIAN_POINT('',(21.8601880142034,13.375,31.5));
#99170=CARTESIAN_POINT('',(21.8601880142034,13.375,31.5));
#99171=CARTESIAN_POINT('',(21.8601880142034,13.375,25.5));
#99172=CARTESIAN_POINT('Origin',(22.2106233847681,13.375,25.5));
#99173=CARTESIAN_POINT('',(22.2106233847681,13.375,25.5));
#99174=CARTESIAN_POINT('',(22.2106233847681,13.375,25.5));
#99175=CARTESIAN_POINT('',(22.2106233847681,13.375,31.5));
#99176=CARTESIAN_POINT('',(22.2106233847681,13.375,31.5));
#99177=CARTESIAN_POINT('',(22.2106233847681,13.375,25.5));
#99178=CARTESIAN_POINT('Origin',(22.6018913866043,14.45,25.5));
#99179=CARTESIAN_POINT('',(22.6018913866043,14.45,25.5));
#99180=CARTESIAN_POINT('',(22.6018913866043,14.45,25.5));
#99181=CARTESIAN_POINT('',(22.6018913866043,14.45,31.5));
#99182=CARTESIAN_POINT('',(22.6018913866043,14.45,31.5));
#99183=CARTESIAN_POINT('',(22.6018913866043,14.45,25.5));
#99184=CARTESIAN_POINT('Origin',(23.0397163391622,14.45,25.5));
#99185=CARTESIAN_POINT('',(23.0397163391622,14.45,25.5));
#99186=CARTESIAN_POINT('',(23.0397163391622,14.45,25.5));
#99187=CARTESIAN_POINT('',(23.0397163391622,14.45,31.5));
#99188=CARTESIAN_POINT('',(23.0397163391622,14.45,31.5));
#99189=CARTESIAN_POINT('',(23.0397163391622,14.45,25.5));
#99190=CARTESIAN_POINT('Origin',(23.4309843409983,13.375,25.5));
#99191=CARTESIAN_POINT('',(23.4309843409983,13.375,25.5));
#99192=CARTESIAN_POINT('',(23.4309843409983,13.375,25.5));
#99193=CARTESIAN_POINT('',(23.4309843409983,13.375,31.5));
#99194=CARTESIAN_POINT('',(23.4309843409983,13.375,31.5));
#99195=CARTESIAN_POINT('',(23.4309843409983,13.375,25.5));
#99196=CARTESIAN_POINT('Origin',(23.781419711563,13.375,25.5));
#99197=CARTESIAN_POINT('',(23.781419711563,13.375,25.5));
#99198=CARTESIAN_POINT('',(23.781419711563,13.375,25.5));
#99199=CARTESIAN_POINT('',(23.781419711563,13.375,31.5));
#99200=CARTESIAN_POINT('',(23.781419711563,13.375,31.5));
#99201=CARTESIAN_POINT('',(23.781419711563,13.375,25.5));
#99202=CARTESIAN_POINT('Origin',(24.1726877133992,14.45,25.5));
#99203=CARTESIAN_POINT('',(24.1726877133992,14.45,25.5));
#99204=CARTESIAN_POINT('',(24.1726877133992,14.45,25.5));
#99205=CARTESIAN_POINT('',(24.1726877133992,14.45,31.5));
#99206=CARTESIAN_POINT('',(24.1726877133992,14.45,31.5));
#99207=CARTESIAN_POINT('',(24.1726877133992,14.45,25.5));
#99208=CARTESIAN_POINT('Origin',(24.6105126659571,14.45,25.5));
#99209=CARTESIAN_POINT('',(24.6105126659571,14.45,25.5));
#99210=CARTESIAN_POINT('',(24.6105126659571,14.45,25.5));
#99211=CARTESIAN_POINT('',(24.6105126659571,14.45,31.5));
#99212=CARTESIAN_POINT('',(24.6105126659571,14.45,31.5));
#99213=CARTESIAN_POINT('',(24.6105126659571,14.45,25.5));
#99214=CARTESIAN_POINT('Origin',(25.0017806677932,13.375,25.5));
#99215=CARTESIAN_POINT('',(25.0017806677932,13.375,25.5));
#99216=CARTESIAN_POINT('',(25.0017806677932,13.375,25.5));
#99217=CARTESIAN_POINT('',(25.0017806677932,13.375,31.5));
#99218=CARTESIAN_POINT('',(25.0017806677932,13.375,31.5));
#99219=CARTESIAN_POINT('',(25.0017806677932,13.375,25.5));
#99220=CARTESIAN_POINT('Origin',(25.3522160383579,13.375,25.5));
#99221=CARTESIAN_POINT('',(25.3522160383579,13.375,25.5));
#99222=CARTESIAN_POINT('',(25.3522160383579,13.375,25.5));
#99223=CARTESIAN_POINT('',(25.3522160383579,13.375,31.5));
#99224=CARTESIAN_POINT('',(25.3522160383579,13.375,31.5));
#99225=CARTESIAN_POINT('',(25.3522160383579,13.375,25.5));
#99226=CARTESIAN_POINT('Origin',(25.7434840401941,14.45,25.5));
#99227=CARTESIAN_POINT('',(25.7434840401941,14.45,25.5));
#99228=CARTESIAN_POINT('',(25.7434840401941,14.45,25.5));
#99229=CARTESIAN_POINT('',(25.7434840401941,14.45,31.5));
#99230=CARTESIAN_POINT('',(25.7434840401941,14.45,31.5));
#99231=CARTESIAN_POINT('',(25.7434840401941,14.45,25.5));
#99232=CARTESIAN_POINT('Origin',(26.181308992752,14.45,25.5));
#99233=CARTESIAN_POINT('',(26.181308992752,14.45,25.5));
#99234=CARTESIAN_POINT('',(26.181308992752,14.45,25.5));
#99235=CARTESIAN_POINT('',(26.181308992752,14.45,31.5));
#99236=CARTESIAN_POINT('',(26.181308992752,14.45,31.5));
#99237=CARTESIAN_POINT('',(26.181308992752,14.45,25.5));
#99238=CARTESIAN_POINT('Origin',(26.5725769945881,13.375,25.5));
#99239=CARTESIAN_POINT('',(26.5725769945881,13.375,25.5));
#99240=CARTESIAN_POINT('',(26.5725769945881,13.375,25.5));
#99241=CARTESIAN_POINT('',(26.5725769945881,13.375,31.5));
#99242=CARTESIAN_POINT('',(26.5725769945881,13.375,31.5));
#99243=CARTESIAN_POINT('',(26.5725769945881,13.375,25.5));
#99244=CARTESIAN_POINT('Origin',(26.9230123651528,13.375,25.5));
#99245=CARTESIAN_POINT('',(26.9230123651528,13.375,25.5));
#99246=CARTESIAN_POINT('',(26.9230123651528,13.375,25.5));
#99247=CARTESIAN_POINT('',(26.9230123651528,13.375,31.5));
#99248=CARTESIAN_POINT('',(26.9230123651528,13.375,31.5));
#99249=CARTESIAN_POINT('',(26.9230123651528,13.375,25.5));
#99250=CARTESIAN_POINT('Origin',(27.314280366989,14.45,25.5));
#99251=CARTESIAN_POINT('',(27.314280366989,14.45,25.5));
#99252=CARTESIAN_POINT('',(27.314280366989,14.45,25.5));
#99253=CARTESIAN_POINT('',(27.314280366989,14.45,31.5));
#99254=CARTESIAN_POINT('',(27.314280366989,14.45,31.5));
#99255=CARTESIAN_POINT('',(27.314280366989,14.45,25.5));
#99256=CARTESIAN_POINT('Origin',(27.7521053195469,14.45,25.5));
#99257=CARTESIAN_POINT('',(27.7521053195469,14.45,25.5));
#99258=CARTESIAN_POINT('',(27.7521053195469,14.45,25.5));
#99259=CARTESIAN_POINT('',(27.7521053195469,14.45,31.5));
#99260=CARTESIAN_POINT('',(27.7521053195469,14.45,31.5));
#99261=CARTESIAN_POINT('',(27.7521053195469,14.45,25.5));
#99262=CARTESIAN_POINT('Origin',(28.143373321383,13.375,25.5));
#99263=CARTESIAN_POINT('',(28.143373321383,13.375,25.5));
#99264=CARTESIAN_POINT('',(28.143373321383,13.375,25.5));
#99265=CARTESIAN_POINT('',(28.143373321383,13.375,31.5));
#99266=CARTESIAN_POINT('',(28.143373321383,13.375,31.5));
#99267=CARTESIAN_POINT('',(28.143373321383,13.375,25.5));
#99268=CARTESIAN_POINT('Origin',(28.4938086919477,13.375,25.5));
#99269=CARTESIAN_POINT('',(28.4938086919477,13.375,25.5));
#99270=CARTESIAN_POINT('',(28.4938086919477,13.375,25.5));
#99271=CARTESIAN_POINT('',(28.4938086919477,13.375,31.5));
#99272=CARTESIAN_POINT('',(28.4938086919477,13.375,31.5));
#99273=CARTESIAN_POINT('',(28.4938086919477,13.375,25.5));
#99274=CARTESIAN_POINT('Origin',(28.8850766937839,14.45,25.5));
#99275=CARTESIAN_POINT('',(28.8850766937839,14.45,25.5));
#99276=CARTESIAN_POINT('',(28.8850766937839,14.45,25.5));
#99277=CARTESIAN_POINT('',(28.8850766937839,14.45,31.5));
#99278=CARTESIAN_POINT('',(28.8850766937839,14.45,31.5));
#99279=CARTESIAN_POINT('',(28.8850766937839,14.45,25.5));
#99280=CARTESIAN_POINT('Origin',(29.3229016463418,14.45,25.5));
#99281=CARTESIAN_POINT('',(29.3229016463418,14.45,25.5));
#99282=CARTESIAN_POINT('',(29.3229016463418,14.45,25.5));
#99283=CARTESIAN_POINT('',(29.3229016463418,14.45,31.5));
#99284=CARTESIAN_POINT('',(29.3229016463418,14.45,31.5));
#99285=CARTESIAN_POINT('',(29.3229016463418,14.45,25.5));
#99286=CARTESIAN_POINT('Origin',(29.7141696481779,13.375,25.5));
#99287=CARTESIAN_POINT('',(29.7141696481779,13.375,25.5));
#99288=CARTESIAN_POINT('',(29.7141696481779,13.375,25.5));
#99289=CARTESIAN_POINT('',(29.7141696481779,13.375,31.5));
#99290=CARTESIAN_POINT('',(29.7141696481779,13.375,31.5));
#99291=CARTESIAN_POINT('',(29.7141696481779,13.375,25.5));
#99292=CARTESIAN_POINT('Origin',(30.0646050187426,13.375,25.5));
#99293=CARTESIAN_POINT('',(30.0646050187426,13.375,25.5));
#99294=CARTESIAN_POINT('',(30.0646050187426,13.375,25.5));
#99295=CARTESIAN_POINT('',(30.0646050187426,13.375,31.5));
#99296=CARTESIAN_POINT('',(30.0646050187426,13.375,31.5));
#99297=CARTESIAN_POINT('',(30.0646050187426,13.375,25.5));
#99298=CARTESIAN_POINT('Origin',(30.4558730205788,14.45,25.5));
#99299=CARTESIAN_POINT('',(30.4558730205788,14.45,25.5));
#99300=CARTESIAN_POINT('',(30.4558730205788,14.45,25.5));
#99301=CARTESIAN_POINT('',(30.4558730205788,14.45,31.5));
#99302=CARTESIAN_POINT('',(30.4558730205788,14.45,31.5));
#99303=CARTESIAN_POINT('',(30.4558730205788,14.45,25.5));
#99304=CARTESIAN_POINT('Origin',(30.8936979731367,14.45,25.5));
#99305=CARTESIAN_POINT('',(30.8936979731367,14.45,25.5));
#99306=CARTESIAN_POINT('',(30.8936979731367,14.45,25.5));
#99307=CARTESIAN_POINT('',(30.8936979731367,14.45,31.5));
#99308=CARTESIAN_POINT('',(30.8936979731367,14.45,31.5));
#99309=CARTESIAN_POINT('',(30.8936979731367,14.45,25.5));
#99310=CARTESIAN_POINT('Origin',(31.2849659749728,13.375,25.5));
#99311=CARTESIAN_POINT('',(31.2849659749728,13.375,25.5));
#99312=CARTESIAN_POINT('',(31.2849659749728,13.375,25.5));
#99313=CARTESIAN_POINT('',(31.2849659749728,13.375,31.5));
#99314=CARTESIAN_POINT('',(31.2849659749728,13.375,31.5));
#99315=CARTESIAN_POINT('',(31.2849659749728,13.375,25.5));
#99316=CARTESIAN_POINT('Origin',(31.6354013455375,13.375,25.5));
#99317=CARTESIAN_POINT('',(31.6354013455375,13.375,25.5));
#99318=CARTESIAN_POINT('',(31.6354013455375,13.375,25.5));
#99319=CARTESIAN_POINT('',(31.6354013455375,13.375,31.5));
#99320=CARTESIAN_POINT('',(31.6354013455375,13.375,31.5));
#99321=CARTESIAN_POINT('',(31.6354013455375,13.375,25.5));
#99322=CARTESIAN_POINT('Origin',(32.0266693473737,14.45,25.5));
#99323=CARTESIAN_POINT('',(32.0266693473737,14.45,25.5));
#99324=CARTESIAN_POINT('',(32.0266693473737,14.45,25.5));
#99325=CARTESIAN_POINT('',(32.0266693473737,14.45,31.5));
#99326=CARTESIAN_POINT('',(32.0266693473737,14.45,31.5));
#99327=CARTESIAN_POINT('',(32.0266693473737,14.45,25.5));
#99328=CARTESIAN_POINT('Origin',(32.4644942999316,14.45,25.5));
#99329=CARTESIAN_POINT('',(32.4644942999316,14.45,25.5));
#99330=CARTESIAN_POINT('',(32.4644942999316,14.45,25.5));
#99331=CARTESIAN_POINT('',(32.4644942999316,14.45,31.5));
#99332=CARTESIAN_POINT('',(32.4644942999316,14.45,31.5));
#99333=CARTESIAN_POINT('',(32.4644942999316,14.45,25.5));
#99334=CARTESIAN_POINT('Origin',(32.8557623017677,13.375,25.5));
#99335=CARTESIAN_POINT('',(32.8557623017677,13.375,25.5));
#99336=CARTESIAN_POINT('',(32.8557623017677,13.375,25.5));
#99337=CARTESIAN_POINT('',(32.8557623017677,13.375,31.5));
#99338=CARTESIAN_POINT('',(32.8557623017677,13.375,31.5));
#99339=CARTESIAN_POINT('',(32.8557623017677,13.375,25.5));
#99340=CARTESIAN_POINT('Origin',(33.2061976723324,13.375,25.5));
#99341=CARTESIAN_POINT('',(33.2061976723324,13.375,25.5));
#99342=CARTESIAN_POINT('',(33.2061976723324,13.375,25.5));
#99343=CARTESIAN_POINT('',(33.2061976723324,13.375,31.5));
#99344=CARTESIAN_POINT('',(33.2061976723324,13.375,31.5));
#99345=CARTESIAN_POINT('',(33.2061976723324,13.375,25.5));
#99346=CARTESIAN_POINT('Origin',(33.5974656741686,14.45,25.5));
#99347=CARTESIAN_POINT('',(33.5974656741686,14.45,25.5));
#99348=CARTESIAN_POINT('',(33.5974656741686,14.45,25.5));
#99349=CARTESIAN_POINT('',(33.5974656741686,14.45,31.5));
#99350=CARTESIAN_POINT('',(33.5974656741686,14.45,31.5));
#99351=CARTESIAN_POINT('',(33.5974656741686,14.45,25.5));
#99352=CARTESIAN_POINT('Origin',(34.0352906267265,14.45,25.5));
#99353=CARTESIAN_POINT('',(34.0352906267265,14.45,25.5));
#99354=CARTESIAN_POINT('',(34.0352906267265,14.45,25.5));
#99355=CARTESIAN_POINT('',(34.0352906267265,14.45,31.5));
#99356=CARTESIAN_POINT('',(34.0352906267265,14.45,31.5));
#99357=CARTESIAN_POINT('',(34.0352906267265,14.45,25.5));
#99358=CARTESIAN_POINT('Origin',(34.4265586285626,13.375,25.5));
#99359=CARTESIAN_POINT('',(34.4265586285626,13.375,25.5));
#99360=CARTESIAN_POINT('',(34.4265586285626,13.375,25.5));
#99361=CARTESIAN_POINT('',(34.4265586285626,13.375,31.5));
#99362=CARTESIAN_POINT('',(34.4265586285626,13.375,31.5));
#99363=CARTESIAN_POINT('',(34.4265586285626,13.375,25.5));
#99364=CARTESIAN_POINT('Origin',(34.7769939991273,13.375,25.5));
#99365=CARTESIAN_POINT('',(34.7769939991273,13.375,25.5));
#99366=CARTESIAN_POINT('',(34.7769939991273,13.375,25.5));
#99367=CARTESIAN_POINT('',(34.7769939991273,13.375,31.5));
#99368=CARTESIAN_POINT('',(34.7769939991273,13.375,31.5));
#99369=CARTESIAN_POINT('',(34.7769939991273,13.375,25.5));
#99370=CARTESIAN_POINT('Origin',(35.1682620009635,14.45,25.5));
#99371=CARTESIAN_POINT('',(35.1682620009635,14.45,25.5));
#99372=CARTESIAN_POINT('',(35.1682620009635,14.45,25.5));
#99373=CARTESIAN_POINT('',(35.1682620009635,14.45,31.5));
#99374=CARTESIAN_POINT('',(35.1682620009635,14.45,31.5));
#99375=CARTESIAN_POINT('',(35.1682620009635,14.45,25.5));
#99376=CARTESIAN_POINT('Origin',(35.6060869535213,14.45,25.5));
#99377=CARTESIAN_POINT('',(35.6060869535213,14.45,25.5));
#99378=CARTESIAN_POINT('',(35.6060869535213,14.45,25.5));
#99379=CARTESIAN_POINT('',(35.6060869535213,14.45,31.5));
#99380=CARTESIAN_POINT('',(35.6060869535213,14.45,31.5));
#99381=CARTESIAN_POINT('',(35.6060869535213,14.45,25.5));
#99382=CARTESIAN_POINT('Origin',(35.9973549553575,13.375,25.5));
#99383=CARTESIAN_POINT('',(35.9973549553575,13.375,25.5));
#99384=CARTESIAN_POINT('',(35.9973549553575,13.375,25.5));
#99385=CARTESIAN_POINT('',(35.9973549553575,13.375,31.5));
#99386=CARTESIAN_POINT('',(35.9973549553575,13.375,31.5));
#99387=CARTESIAN_POINT('',(35.9973549553575,13.375,25.5));
#99388=CARTESIAN_POINT('Origin',(36.3477903259222,13.375,25.5));
#99389=CARTESIAN_POINT('',(36.3477903259222,13.375,25.5));
#99390=CARTESIAN_POINT('',(36.3477903259222,13.375,25.5));
#99391=CARTESIAN_POINT('',(36.3477903259222,13.375,31.5));
#99392=CARTESIAN_POINT('',(36.3477903259222,13.375,31.5));
#99393=CARTESIAN_POINT('',(36.3477903259222,13.375,25.5));
#99394=CARTESIAN_POINT('Origin',(36.7390583277584,14.45,25.5));
#99395=CARTESIAN_POINT('',(36.7390583277584,14.45,25.5));
#99396=CARTESIAN_POINT('',(36.7390583277584,14.45,25.5));
#99397=CARTESIAN_POINT('',(36.7390583277584,14.45,31.5));
#99398=CARTESIAN_POINT('',(36.7390583277584,14.45,31.5));
#99399=CARTESIAN_POINT('',(36.7390583277584,14.45,25.5));
#99400=CARTESIAN_POINT('Origin',(37.1768832803162,14.45,25.5));
#99401=CARTESIAN_POINT('',(37.1768832803162,14.45,25.5));
#99402=CARTESIAN_POINT('',(37.1768832803162,14.45,25.5));
#99403=CARTESIAN_POINT('',(37.1768832803162,14.45,31.5));
#99404=CARTESIAN_POINT('',(37.1768832803162,14.45,31.5));
#99405=CARTESIAN_POINT('',(37.1768832803162,14.45,25.5));
#99406=CARTESIAN_POINT('Origin',(37.5681512821524,13.375,25.5));
#99407=CARTESIAN_POINT('',(37.5681512821524,13.375,25.5));
#99408=CARTESIAN_POINT('',(37.5681512821524,13.375,25.5));
#99409=CARTESIAN_POINT('',(37.5681512821524,13.375,31.5));
#99410=CARTESIAN_POINT('',(37.5681512821524,13.375,31.5));
#99411=CARTESIAN_POINT('',(37.5681512821524,13.375,25.5));
#99412=CARTESIAN_POINT('Origin',(37.9185866527171,13.375,25.5));
#99413=CARTESIAN_POINT('',(37.9185866527171,13.375,25.5));
#99414=CARTESIAN_POINT('',(37.9185866527171,13.375,25.5));
#99415=CARTESIAN_POINT('',(37.9185866527171,13.375,31.5));
#99416=CARTESIAN_POINT('',(37.9185866527171,13.375,31.5));
#99417=CARTESIAN_POINT('',(37.9185866527171,13.375,25.5));
#99418=CARTESIAN_POINT('Origin',(38.3098546545533,14.45,25.5));
#99419=CARTESIAN_POINT('',(38.3098546545533,14.45,25.5));
#99420=CARTESIAN_POINT('',(38.3098546545533,14.45,25.5));
#99421=CARTESIAN_POINT('',(38.3098546545533,14.45,31.5));
#99422=CARTESIAN_POINT('',(38.3098546545533,14.45,31.5));
#99423=CARTESIAN_POINT('',(38.3098546545533,14.45,25.5));
#99424=CARTESIAN_POINT('Origin',(38.7476796071111,14.45,25.5));
#99425=CARTESIAN_POINT('',(38.7476796071111,14.45,25.5));
#99426=CARTESIAN_POINT('',(38.7476796071111,14.45,25.5));
#99427=CARTESIAN_POINT('',(38.7476796071111,14.45,31.5));
#99428=CARTESIAN_POINT('',(38.7476796071111,14.45,31.5));
#99429=CARTESIAN_POINT('',(38.7476796071111,14.45,25.5));
#99430=CARTESIAN_POINT('Origin',(39.1389476089473,13.375,25.5));
#99431=CARTESIAN_POINT('',(39.1389476089473,13.375,25.5));
#99432=CARTESIAN_POINT('',(39.1389476089473,13.375,25.5));
#99433=CARTESIAN_POINT('',(39.1389476089473,13.375,31.5));
#99434=CARTESIAN_POINT('',(39.1389476089473,13.375,31.5));
#99435=CARTESIAN_POINT('',(39.1389476089473,13.375,25.5));
#99436=CARTESIAN_POINT('Origin',(39.489382979512,13.375,25.5));
#99437=CARTESIAN_POINT('',(39.489382979512,13.375,25.5));
#99438=CARTESIAN_POINT('',(39.489382979512,13.375,25.5));
#99439=CARTESIAN_POINT('',(39.489382979512,13.375,31.5));
#99440=CARTESIAN_POINT('',(39.489382979512,13.375,31.5));
#99441=CARTESIAN_POINT('',(39.489382979512,13.375,25.5));
#99442=CARTESIAN_POINT('Origin',(39.8806509813482,14.45,25.5));
#99443=CARTESIAN_POINT('',(39.8806509813482,14.45,25.5));
#99444=CARTESIAN_POINT('',(39.8806509813482,14.45,25.5));
#99445=CARTESIAN_POINT('',(39.8806509813482,14.45,31.5));
#99446=CARTESIAN_POINT('',(39.8806509813482,14.45,31.5));
#99447=CARTESIAN_POINT('',(39.8806509813482,14.45,25.5));
#99448=CARTESIAN_POINT('Origin',(40.318475933906,14.45,25.5));
#99449=CARTESIAN_POINT('',(40.318475933906,14.45,25.5));
#99450=CARTESIAN_POINT('',(40.318475933906,14.45,25.5));
#99451=CARTESIAN_POINT('',(40.318475933906,14.45,31.5));
#99452=CARTESIAN_POINT('',(40.318475933906,14.45,31.5));
#99453=CARTESIAN_POINT('',(40.318475933906,14.45,25.5));
#99454=CARTESIAN_POINT('Origin',(40.7097439357422,13.375,25.5));
#99455=CARTESIAN_POINT('',(40.7097439357422,13.375,25.5));
#99456=CARTESIAN_POINT('',(40.7097439357422,13.375,25.5));
#99457=CARTESIAN_POINT('',(40.7097439357422,13.375,31.5));
#99458=CARTESIAN_POINT('',(40.7097439357422,13.375,31.5));
#99459=CARTESIAN_POINT('',(40.7097439357422,13.375,25.5));
#99460=CARTESIAN_POINT('Origin',(41.0601793063069,13.375,25.5));
#99461=CARTESIAN_POINT('',(41.0601793063069,13.375,25.5));
#99462=CARTESIAN_POINT('',(41.0601793063069,13.375,25.5));
#99463=CARTESIAN_POINT('',(41.0601793063069,13.375,31.5));
#99464=CARTESIAN_POINT('',(41.0601793063069,13.375,31.5));
#99465=CARTESIAN_POINT('',(41.0601793063069,13.375,25.5));
#99466=CARTESIAN_POINT('Origin',(41.4514473081431,14.45,25.5));
#99467=CARTESIAN_POINT('',(41.4514473081431,14.45,25.5));
#99468=CARTESIAN_POINT('',(41.4514473081431,14.45,25.5));
#99469=CARTESIAN_POINT('',(41.4514473081431,14.45,31.5));
#99470=CARTESIAN_POINT('',(41.4514473081431,14.45,31.5));
#99471=CARTESIAN_POINT('',(41.4514473081431,14.45,25.5));
#99472=CARTESIAN_POINT('Origin',(41.8892722607009,14.45,25.5));
#99473=CARTESIAN_POINT('',(41.8892722607009,14.45,25.5));
#99474=CARTESIAN_POINT('',(41.8892722607009,14.45,25.5));
#99475=CARTESIAN_POINT('',(41.8892722607009,14.45,31.5));
#99476=CARTESIAN_POINT('',(41.8892722607009,14.45,31.5));
#99477=CARTESIAN_POINT('',(41.8892722607009,14.45,25.5));
#99478=CARTESIAN_POINT('Origin',(42.2805402625371,13.375,25.5));
#99479=CARTESIAN_POINT('',(42.2805402625371,13.375,25.5));
#99480=CARTESIAN_POINT('',(42.2805402625371,13.375,25.5));
#99481=CARTESIAN_POINT('',(42.2805402625371,13.375,31.5));
#99482=CARTESIAN_POINT('',(42.2805402625371,13.375,31.5));
#99483=CARTESIAN_POINT('',(42.2805402625371,13.375,25.5));
#99484=CARTESIAN_POINT('Origin',(42.6309756331018,13.375,25.5));
#99485=CARTESIAN_POINT('',(42.6309756331018,13.375,25.5));
#99486=CARTESIAN_POINT('',(42.6309756331018,13.375,25.5));
#99487=CARTESIAN_POINT('',(42.6309756331018,13.375,31.5));
#99488=CARTESIAN_POINT('',(42.6309756331018,13.375,31.5));
#99489=CARTESIAN_POINT('',(42.6309756331018,13.375,25.5));
#99490=CARTESIAN_POINT('Origin',(43.022243634938,14.45,25.5));
#99491=CARTESIAN_POINT('',(43.022243634938,14.45,25.5));
#99492=CARTESIAN_POINT('',(43.022243634938,14.45,25.5));
#99493=CARTESIAN_POINT('',(43.022243634938,14.45,31.5));
#99494=CARTESIAN_POINT('',(43.022243634938,14.45,31.5));
#99495=CARTESIAN_POINT('',(43.022243634938,14.45,25.5));
#99496=CARTESIAN_POINT('Origin',(43.4600685874958,14.45,25.5));
#99497=CARTESIAN_POINT('',(43.4600685874958,14.45,25.5));
#99498=CARTESIAN_POINT('',(43.4600685874958,14.45,25.5));
#99499=CARTESIAN_POINT('',(43.4600685874958,14.45,31.5));
#99500=CARTESIAN_POINT('',(43.4600685874958,14.45,31.5));
#99501=CARTESIAN_POINT('',(43.4600685874958,14.45,25.5));
#99502=CARTESIAN_POINT('Origin',(43.851336589332,13.375,25.5));
#99503=CARTESIAN_POINT('',(43.851336589332,13.375,25.5));
#99504=CARTESIAN_POINT('',(43.851336589332,13.375,25.5));
#99505=CARTESIAN_POINT('',(43.851336589332,13.375,31.5));
#99506=CARTESIAN_POINT('',(43.851336589332,13.375,31.5));
#99507=CARTESIAN_POINT('',(43.851336589332,13.375,25.5));
#99508=CARTESIAN_POINT('Origin',(44.2017719598967,13.375,25.5));
#99509=CARTESIAN_POINT('',(44.2017719598967,13.375,25.5));
#99510=CARTESIAN_POINT('',(44.2017719598967,13.375,25.5));
#99511=CARTESIAN_POINT('',(44.2017719598967,13.375,31.5));
#99512=CARTESIAN_POINT('',(44.2017719598967,13.375,31.5));
#99513=CARTESIAN_POINT('',(44.2017719598967,13.375,25.5));
#99514=CARTESIAN_POINT('Origin',(44.5930399617329,14.45,25.5));
#99515=CARTESIAN_POINT('',(44.5930399617329,14.45,25.5));
#99516=CARTESIAN_POINT('',(44.5930399617329,14.45,25.5));
#99517=CARTESIAN_POINT('',(44.5930399617329,14.45,31.5));
#99518=CARTESIAN_POINT('',(44.5930399617329,14.45,31.5));
#99519=CARTESIAN_POINT('',(44.5930399617329,14.45,25.5));
#99520=CARTESIAN_POINT('Origin',(45.0308649142907,14.45,25.5));
#99521=CARTESIAN_POINT('',(45.0308649142907,14.45,25.5));
#99522=CARTESIAN_POINT('',(45.0308649142907,14.45,25.5));
#99523=CARTESIAN_POINT('',(45.0308649142907,14.45,31.5));
#99524=CARTESIAN_POINT('',(45.0308649142907,14.45,31.5));
#99525=CARTESIAN_POINT('',(45.0308649142907,14.45,25.5));
#99526=CARTESIAN_POINT('Origin',(45.4221329161269,13.375,25.5));
#99527=CARTESIAN_POINT('',(45.4221329161269,13.375,25.5));
#99528=CARTESIAN_POINT('',(45.4221329161269,13.375,25.5));
#99529=CARTESIAN_POINT('',(45.4221329161269,13.375,31.5));
#99530=CARTESIAN_POINT('',(45.4221329161269,13.375,31.5));
#99531=CARTESIAN_POINT('',(45.4221329161269,13.375,25.5));
#99532=CARTESIAN_POINT('Origin',(45.7725682866916,13.375,25.5));
#99533=CARTESIAN_POINT('',(45.7725682866916,13.375,25.5));
#99534=CARTESIAN_POINT('',(45.7725682866916,13.375,25.5));
#99535=CARTESIAN_POINT('',(45.7725682866916,13.375,31.5));
#99536=CARTESIAN_POINT('',(45.7725682866916,13.375,31.5));
#99537=CARTESIAN_POINT('',(45.7725682866916,13.375,25.5));
#99538=CARTESIAN_POINT('Origin',(46.1638362885278,14.45,25.5));
#99539=CARTESIAN_POINT('',(46.1638362885278,14.45,25.5));
#99540=CARTESIAN_POINT('',(46.1638362885278,14.45,25.5));
#99541=CARTESIAN_POINT('',(46.1638362885278,14.45,31.5));
#99542=CARTESIAN_POINT('',(46.1638362885278,14.45,31.5));
#99543=CARTESIAN_POINT('',(46.1638362885278,14.45,25.5));
#99544=CARTESIAN_POINT('Origin',(46.6016612410856,14.45,25.5));
#99545=CARTESIAN_POINT('',(46.6016612410856,14.45,25.5));
#99546=CARTESIAN_POINT('',(46.6016612410856,14.45,25.5));
#99547=CARTESIAN_POINT('',(46.6016612410856,14.45,31.5));
#99548=CARTESIAN_POINT('',(46.6016612410856,14.45,31.5));
#99549=CARTESIAN_POINT('',(46.6016612410856,14.45,25.5));
#99550=CARTESIAN_POINT('Origin',(46.9929292429218,13.375,25.5));
#99551=CARTESIAN_POINT('',(46.9929292429218,13.375,25.5));
#99552=CARTESIAN_POINT('',(46.9929292429218,13.375,25.5));
#99553=CARTESIAN_POINT('',(46.9929292429218,13.375,31.5));
#99554=CARTESIAN_POINT('',(46.9929292429218,13.375,31.5));
#99555=CARTESIAN_POINT('',(46.9929292429218,13.375,25.5));
#99556=CARTESIAN_POINT('Origin',(47.3433646134865,13.375,25.5));
#99557=CARTESIAN_POINT('',(47.3433646134865,13.375,25.5));
#99558=CARTESIAN_POINT('',(47.3433646134865,13.375,25.5));
#99559=CARTESIAN_POINT('',(47.3433646134865,13.375,31.5));
#99560=CARTESIAN_POINT('',(47.3433646134865,13.375,31.5));
#99561=CARTESIAN_POINT('',(47.3433646134865,13.375,25.5));
#99562=CARTESIAN_POINT('Origin',(47.7346326153227,14.45,25.5));
#99563=CARTESIAN_POINT('',(47.7346326153227,14.45,25.5));
#99564=CARTESIAN_POINT('',(47.7346326153227,14.45,25.5));
#99565=CARTESIAN_POINT('',(47.7346326153227,14.45,31.5));
#99566=CARTESIAN_POINT('',(47.7346326153227,14.45,31.5));
#99567=CARTESIAN_POINT('',(47.7346326153227,14.45,25.5));
#99568=CARTESIAN_POINT('Origin',(48.1724575678805,14.45,25.5));
#99569=CARTESIAN_POINT('',(48.1724575678805,14.45,25.5));
#99570=CARTESIAN_POINT('',(48.1724575678805,14.45,25.5));
#99571=CARTESIAN_POINT('',(48.1724575678805,14.45,31.5));
#99572=CARTESIAN_POINT('',(48.1724575678805,14.45,31.5));
#99573=CARTESIAN_POINT('',(48.1724575678805,14.45,25.5));
#99574=CARTESIAN_POINT('Origin',(48.5637255697167,13.375,25.5));
#99575=CARTESIAN_POINT('',(48.5637255697167,13.375,25.5));
#99576=CARTESIAN_POINT('',(48.5637255697167,13.375,25.5));
#99577=CARTESIAN_POINT('',(48.5637255697167,13.375,31.5));
#99578=CARTESIAN_POINT('',(48.5637255697167,13.375,31.5));
#99579=CARTESIAN_POINT('',(48.5637255697167,13.375,25.5));
#99580=CARTESIAN_POINT('Origin',(48.9141609402814,13.375,25.5));
#99581=CARTESIAN_POINT('',(48.9141609402814,13.375,25.5));
#99582=CARTESIAN_POINT('',(48.9141609402814,13.375,25.5));
#99583=CARTESIAN_POINT('',(48.9141609402814,13.375,31.5));
#99584=CARTESIAN_POINT('',(48.9141609402814,13.375,31.5));
#99585=CARTESIAN_POINT('',(48.9141609402814,13.375,25.5));
#99586=CARTESIAN_POINT('Origin',(49.3054289421176,14.45,25.5));
#99587=CARTESIAN_POINT('',(49.3054289421176,14.45,25.5));
#99588=CARTESIAN_POINT('',(49.3054289421176,14.45,25.5));
#99589=CARTESIAN_POINT('',(49.3054289421176,14.45,31.5));
#99590=CARTESIAN_POINT('',(49.3054289421176,14.45,31.5));
#99591=CARTESIAN_POINT('',(49.3054289421176,14.45,25.5));
#99592=CARTESIAN_POINT('Origin',(49.7432538946754,14.45,25.5));
#99593=CARTESIAN_POINT('',(49.7432538946754,14.45,25.5));
#99594=CARTESIAN_POINT('',(49.7432538946754,14.45,25.5));
#99595=CARTESIAN_POINT('',(49.7432538946754,14.45,31.5));
#99596=CARTESIAN_POINT('',(49.7432538946754,14.45,31.5));
#99597=CARTESIAN_POINT('',(49.7432538946754,14.45,25.5));
#99598=CARTESIAN_POINT('Origin',(50.1345218965116,13.375,25.5));
#99599=CARTESIAN_POINT('',(50.1345218965116,13.375,25.5));
#99600=CARTESIAN_POINT('',(50.1345218965116,13.375,25.5));
#99601=CARTESIAN_POINT('',(50.1345218965116,13.375,31.5));
#99602=CARTESIAN_POINT('',(50.1345218965116,13.375,31.5));
#99603=CARTESIAN_POINT('',(50.1345218965116,13.375,25.5));
#99604=CARTESIAN_POINT('Origin',(50.4849572670763,13.375,25.5));
#99605=CARTESIAN_POINT('',(50.4849572670763,13.375,25.5));
#99606=CARTESIAN_POINT('',(50.4849572670763,13.375,25.5));
#99607=CARTESIAN_POINT('',(50.4849572670763,13.375,31.5));
#99608=CARTESIAN_POINT('',(50.4849572670763,13.375,31.5));
#99609=CARTESIAN_POINT('',(50.4849572670763,13.375,25.5));
#99610=CARTESIAN_POINT('Origin',(50.8762252689124,14.45,25.5));
#99611=CARTESIAN_POINT('',(50.8762252689124,14.45,25.5));
#99612=CARTESIAN_POINT('',(50.8762252689124,14.45,25.5));
#99613=CARTESIAN_POINT('',(50.8762252689124,14.45,31.5));
#99614=CARTESIAN_POINT('',(50.8762252689124,14.45,31.5));
#99615=CARTESIAN_POINT('',(50.8762252689124,14.45,25.5));
#99616=CARTESIAN_POINT('Origin',(51.3140502214703,14.45,25.5));
#99617=CARTESIAN_POINT('',(51.3140502214703,14.45,25.5));
#99618=CARTESIAN_POINT('',(51.3140502214703,14.45,25.5));
#99619=CARTESIAN_POINT('',(51.3140502214703,14.45,31.5));
#99620=CARTESIAN_POINT('',(51.3140502214703,14.45,31.5));
#99621=CARTESIAN_POINT('',(51.3140502214703,14.45,25.5));
#99622=CARTESIAN_POINT('Origin',(51.7053182233065,13.375,25.5));
#99623=CARTESIAN_POINT('',(51.7053182233065,13.375,25.5));
#99624=CARTESIAN_POINT('',(51.7053182233065,13.375,25.5));
#99625=CARTESIAN_POINT('',(51.7053182233065,13.375,31.5));
#99626=CARTESIAN_POINT('',(51.7053182233065,13.375,31.5));
#99627=CARTESIAN_POINT('',(51.7053182233065,13.375,25.5));
#99628=CARTESIAN_POINT('Origin',(52.0557535938712,13.375,25.5));
#99629=CARTESIAN_POINT('',(52.0557535938712,13.375,25.5));
#99630=CARTESIAN_POINT('',(52.0557535938712,13.375,25.5));
#99631=CARTESIAN_POINT('',(52.0557535938712,13.375,31.5));
#99632=CARTESIAN_POINT('',(52.0557535938712,13.375,31.5));
#99633=CARTESIAN_POINT('',(52.0557535938712,13.375,25.5));
#99634=CARTESIAN_POINT('Origin',(52.4470215957073,14.45,25.5));
#99635=CARTESIAN_POINT('',(52.4470215957073,14.45,25.5));
#99636=CARTESIAN_POINT('',(52.4470215957073,14.45,25.5));
#99637=CARTESIAN_POINT('',(52.4470215957073,14.45,31.5));
#99638=CARTESIAN_POINT('',(52.4470215957073,14.45,31.5));
#99639=CARTESIAN_POINT('',(52.4470215957073,14.45,25.5));
#99640=CARTESIAN_POINT('Origin',(52.8848465482652,14.45,25.5));
#99641=CARTESIAN_POINT('',(52.8848465482652,14.45,25.5));
#99642=CARTESIAN_POINT('',(52.8848465482652,14.45,25.5));
#99643=CARTESIAN_POINT('',(52.8848465482652,14.45,31.5));
#99644=CARTESIAN_POINT('',(52.8848465482652,14.45,31.5));
#99645=CARTESIAN_POINT('',(52.8848465482652,14.45,25.5));
#99646=CARTESIAN_POINT('Origin',(53.2761145501014,13.375,25.5));
#99647=CARTESIAN_POINT('',(53.2761145501014,13.375,25.5));
#99648=CARTESIAN_POINT('',(53.2761145501014,13.375,25.5));
#99649=CARTESIAN_POINT('',(53.2761145501014,13.375,31.5));
#99650=CARTESIAN_POINT('',(53.2761145501014,13.375,31.5));
#99651=CARTESIAN_POINT('',(53.2761145501014,13.375,25.5));
#99652=CARTESIAN_POINT('Origin',(53.6265499206661,13.375,25.5));
#99653=CARTESIAN_POINT('',(53.6265499206661,13.375,25.5));
#99654=CARTESIAN_POINT('',(53.6265499206661,13.375,25.5));
#99655=CARTESIAN_POINT('',(53.6265499206661,13.375,31.5));
#99656=CARTESIAN_POINT('',(53.6265499206661,13.375,31.5));
#99657=CARTESIAN_POINT('',(53.6265499206661,13.375,25.5));
#99658=CARTESIAN_POINT('Origin',(54.0178179225022,14.45,25.5));
#99659=CARTESIAN_POINT('',(54.0178179225022,14.45,25.5));
#99660=CARTESIAN_POINT('',(54.0178179225022,14.45,25.5));
#99661=CARTESIAN_POINT('',(54.0178179225022,14.45,31.5));
#99662=CARTESIAN_POINT('',(54.0178179225022,14.45,31.5));
#99663=CARTESIAN_POINT('',(54.0178179225022,14.45,25.5));
#99664=CARTESIAN_POINT('Origin',(54.4556428750601,14.45,25.5));
#99665=CARTESIAN_POINT('',(54.4556428750601,14.45,25.5));
#99666=CARTESIAN_POINT('',(54.4556428750601,14.45,25.5));
#99667=CARTESIAN_POINT('',(54.4556428750601,14.45,31.5));
#99668=CARTESIAN_POINT('',(54.4556428750601,14.45,31.5));
#99669=CARTESIAN_POINT('',(54.4556428750601,14.45,25.5));
#99670=CARTESIAN_POINT('Origin',(54.8469108768963,13.375,25.5));
#99671=CARTESIAN_POINT('',(54.8469108768963,13.375,25.5));
#99672=CARTESIAN_POINT('',(54.8469108768963,13.375,25.5));
#99673=CARTESIAN_POINT('',(54.8469108768963,13.375,31.5));
#99674=CARTESIAN_POINT('',(54.8469108768963,13.375,31.5));
#99675=CARTESIAN_POINT('',(54.8469108768963,13.375,25.5));
#99676=CARTESIAN_POINT('Origin',(55.197346247461,13.375,25.5));
#99677=CARTESIAN_POINT('',(55.197346247461,13.375,25.5));
#99678=CARTESIAN_POINT('',(55.197346247461,13.375,25.5));
#99679=CARTESIAN_POINT('',(55.197346247461,13.375,31.5));
#99680=CARTESIAN_POINT('',(55.197346247461,13.375,31.5));
#99681=CARTESIAN_POINT('',(55.197346247461,13.375,25.5));
#99682=CARTESIAN_POINT('Origin',(55.5886142492971,14.45,25.5));
#99683=CARTESIAN_POINT('',(55.5886142492971,14.45,25.5));
#99684=CARTESIAN_POINT('',(55.5886142492971,14.45,25.5));
#99685=CARTESIAN_POINT('',(55.5886142492971,14.45,31.5));
#99686=CARTESIAN_POINT('',(55.5886142492971,14.45,31.5));
#99687=CARTESIAN_POINT('',(55.5886142492971,14.45,25.5));
#99688=CARTESIAN_POINT('Origin',(56.026439201855,14.45,25.5));
#99689=CARTESIAN_POINT('',(56.026439201855,14.45,25.5));
#99690=CARTESIAN_POINT('',(56.026439201855,14.45,25.5));
#99691=CARTESIAN_POINT('',(56.026439201855,14.45,31.5));
#99692=CARTESIAN_POINT('',(56.026439201855,14.45,31.5));
#99693=CARTESIAN_POINT('',(56.026439201855,14.45,25.5));
#99694=CARTESIAN_POINT('Origin',(56.4177072036912,13.375,25.5));
#99695=CARTESIAN_POINT('',(56.4177072036912,13.375,25.5));
#99696=CARTESIAN_POINT('',(56.4177072036912,13.375,25.5));
#99697=CARTESIAN_POINT('',(56.4177072036912,13.375,31.5));
#99698=CARTESIAN_POINT('',(56.4177072036912,13.375,31.5));
#99699=CARTESIAN_POINT('',(56.4177072036912,13.375,25.5));
#99700=CARTESIAN_POINT('Origin',(56.7681425742559,13.375,25.5));
#99701=CARTESIAN_POINT('',(56.7681425742559,13.375,25.5));
#99702=CARTESIAN_POINT('',(56.7681425742559,13.375,25.5));
#99703=CARTESIAN_POINT('',(56.7681425742559,13.375,31.5));
#99704=CARTESIAN_POINT('',(56.7681425742559,13.375,31.5));
#99705=CARTESIAN_POINT('',(56.7681425742559,13.375,25.5));
#99706=CARTESIAN_POINT('Origin',(57.159410576092,14.45,25.5));
#99707=CARTESIAN_POINT('',(57.159410576092,14.45,25.5));
#99708=CARTESIAN_POINT('',(57.159410576092,14.45,25.5));
#99709=CARTESIAN_POINT('',(57.159410576092,14.45,31.5));
#99710=CARTESIAN_POINT('',(57.159410576092,14.45,31.5));
#99711=CARTESIAN_POINT('',(57.159410576092,14.45,25.5));
#99712=CARTESIAN_POINT('Origin',(57.5972355286499,14.45,25.5));
#99713=CARTESIAN_POINT('',(57.5972355286499,14.45,25.5));
#99714=CARTESIAN_POINT('',(57.5972355286499,14.45,25.5));
#99715=CARTESIAN_POINT('',(57.5972355286499,14.45,31.5));
#99716=CARTESIAN_POINT('',(57.5972355286499,14.45,31.5));
#99717=CARTESIAN_POINT('',(57.5972355286499,14.45,25.5));
#99718=CARTESIAN_POINT('Origin',(57.9885035304861,13.375,25.5));
#99719=CARTESIAN_POINT('',(57.9885035304861,13.375,25.5));
#99720=CARTESIAN_POINT('',(57.9885035304861,13.375,25.5));
#99721=CARTESIAN_POINT('',(57.9885035304861,13.375,31.5));
#99722=CARTESIAN_POINT('',(57.9885035304861,13.375,31.5));
#99723=CARTESIAN_POINT('',(57.9885035304861,13.375,25.5));
#99724=CARTESIAN_POINT('Origin',(58.3389389010508,13.375,25.5));
#99725=CARTESIAN_POINT('',(58.3389389010508,13.375,25.5));
#99726=CARTESIAN_POINT('',(58.3389389010508,13.375,25.5));
#99727=CARTESIAN_POINT('',(58.3389389010508,13.375,31.5));
#99728=CARTESIAN_POINT('',(58.3389389010508,13.375,31.5));
#99729=CARTESIAN_POINT('',(58.3389389010508,13.375,25.5));
#99730=CARTESIAN_POINT('Origin',(58.7302069028869,14.45,25.5));
#99731=CARTESIAN_POINT('',(58.7302069028869,14.45,25.5));
#99732=CARTESIAN_POINT('',(58.7302069028869,14.45,25.5));
#99733=CARTESIAN_POINT('',(58.7302069028869,14.45,31.5));
#99734=CARTESIAN_POINT('',(58.7302069028869,14.45,31.5));
#99735=CARTESIAN_POINT('',(58.7302069028869,14.45,25.5));
#99736=CARTESIAN_POINT('Origin',(59.1680318554448,14.45,25.5));
#99737=CARTESIAN_POINT('',(59.1680318554448,14.45,25.5));
#99738=CARTESIAN_POINT('',(59.1680318554448,14.45,25.5));
#99739=CARTESIAN_POINT('',(59.1680318554448,14.45,31.5));
#99740=CARTESIAN_POINT('',(59.1680318554448,14.45,31.5));
#99741=CARTESIAN_POINT('',(59.1680318554448,14.45,25.5));
#99742=CARTESIAN_POINT('Origin',(59.559299857281,13.375,25.5));
#99743=CARTESIAN_POINT('',(59.559299857281,13.375,25.5));
#99744=CARTESIAN_POINT('',(59.559299857281,13.375,25.5));
#99745=CARTESIAN_POINT('',(59.559299857281,13.375,31.5));
#99746=CARTESIAN_POINT('',(59.559299857281,13.375,31.5));
#99747=CARTESIAN_POINT('',(59.559299857281,13.375,25.5));
#99748=CARTESIAN_POINT('Origin',(59.9097352278457,13.375,25.5));
#99749=CARTESIAN_POINT('',(59.9097352278457,13.375,25.5));
#99750=CARTESIAN_POINT('',(59.9097352278457,13.375,25.5));
#99751=CARTESIAN_POINT('',(59.9097352278457,13.375,31.5));
#99752=CARTESIAN_POINT('',(59.9097352278457,13.375,31.5));
#99753=CARTESIAN_POINT('',(59.9097352278457,13.375,25.5));
#99754=CARTESIAN_POINT('Origin',(60.3010032296818,14.45,25.5));
#99755=CARTESIAN_POINT('',(60.3010032296818,14.45,25.5));
#99756=CARTESIAN_POINT('',(60.3010032296818,14.45,25.5));
#99757=CARTESIAN_POINT('',(60.3010032296818,14.45,31.5));
#99758=CARTESIAN_POINT('',(60.3010032296818,14.45,31.5));
#99759=CARTESIAN_POINT('',(60.3010032296818,14.45,25.5));
#99760=CARTESIAN_POINT('Origin',(60.7388281822397,14.45,25.5));
#99761=CARTESIAN_POINT('',(60.7388281822397,14.45,25.5));
#99762=CARTESIAN_POINT('',(60.7388281822397,14.45,25.5));
#99763=CARTESIAN_POINT('',(60.7388281822397,14.45,31.5));
#99764=CARTESIAN_POINT('',(60.7388281822397,14.45,31.5));
#99765=CARTESIAN_POINT('',(60.7388281822397,14.45,25.5));
#99766=CARTESIAN_POINT('Origin',(61.1300961840759,13.375,25.5));
#99767=CARTESIAN_POINT('',(61.1300961840759,13.375,25.5));
#99768=CARTESIAN_POINT('',(61.1300961840759,13.375,25.5));
#99769=CARTESIAN_POINT('',(61.1300961840759,13.375,31.5));
#99770=CARTESIAN_POINT('',(61.1300961840759,13.375,31.5));
#99771=CARTESIAN_POINT('',(61.1300961840759,13.375,25.5));
#99772=CARTESIAN_POINT('Origin',(61.4805315546406,13.375,25.5));
#99773=CARTESIAN_POINT('',(61.4805315546406,13.375,25.5));
#99774=CARTESIAN_POINT('',(61.4805315546406,13.375,25.5));
#99775=CARTESIAN_POINT('',(61.4805315546406,13.375,31.5));
#99776=CARTESIAN_POINT('',(61.4805315546406,13.375,31.5));
#99777=CARTESIAN_POINT('',(61.4805315546406,13.375,25.5));
#99778=CARTESIAN_POINT('Origin',(61.8717995564767,14.45,25.5));
#99779=CARTESIAN_POINT('',(61.8717995564767,14.45,25.5));
#99780=CARTESIAN_POINT('',(61.8717995564767,14.45,25.5));
#99781=CARTESIAN_POINT('',(61.8717995564767,14.45,31.5));
#99782=CARTESIAN_POINT('',(61.8717995564767,14.45,31.5));
#99783=CARTESIAN_POINT('',(61.8717995564767,14.45,25.5));
#99784=CARTESIAN_POINT('Origin',(62.3096245090346,14.45,25.5));
#99785=CARTESIAN_POINT('',(62.3096245090346,14.45,25.5));
#99786=CARTESIAN_POINT('',(62.3096245090346,14.45,25.5));
#99787=CARTESIAN_POINT('',(62.3096245090346,14.45,31.5));
#99788=CARTESIAN_POINT('',(62.3096245090346,14.45,31.5));
#99789=CARTESIAN_POINT('',(62.3096245090346,14.45,25.5));
#99790=CARTESIAN_POINT('Origin',(62.7008925108708,13.375,25.5));
#99791=CARTESIAN_POINT('',(62.7008925108708,13.375,25.5));
#99792=CARTESIAN_POINT('',(62.7008925108708,13.375,25.5));
#99793=CARTESIAN_POINT('',(62.7008925108708,13.375,31.5));
#99794=CARTESIAN_POINT('',(62.7008925108708,13.375,31.5));
#99795=CARTESIAN_POINT('',(62.7008925108708,13.375,25.5));
#99796=CARTESIAN_POINT('Origin',(63.0513278814355,13.375,25.5));
#99797=CARTESIAN_POINT('',(63.0513278814355,13.375,25.5));
#99798=CARTESIAN_POINT('',(63.0513278814355,13.375,25.5));
#99799=CARTESIAN_POINT('',(63.0513278814355,13.375,31.5));
#99800=CARTESIAN_POINT('',(63.0513278814355,13.375,31.5));
#99801=CARTESIAN_POINT('',(63.0513278814355,13.375,25.5));
#99802=CARTESIAN_POINT('Origin',(63.4425958832716,14.45,25.5));
#99803=CARTESIAN_POINT('',(63.4425958832716,14.45,25.5));
#99804=CARTESIAN_POINT('',(63.4425958832716,14.45,25.5));
#99805=CARTESIAN_POINT('',(63.4425958832716,14.45,31.5));
#99806=CARTESIAN_POINT('',(63.4425958832716,14.45,31.5));
#99807=CARTESIAN_POINT('',(63.4425958832716,14.45,25.5));
#99808=CARTESIAN_POINT('Origin',(63.8804208358295,14.45,25.5));
#99809=CARTESIAN_POINT('',(63.8804208358295,14.45,25.5));
#99810=CARTESIAN_POINT('',(63.8804208358295,14.45,25.5));
#99811=CARTESIAN_POINT('',(63.8804208358295,14.45,31.5));
#99812=CARTESIAN_POINT('',(63.8804208358295,14.45,31.5));
#99813=CARTESIAN_POINT('',(63.8804208358295,14.45,25.5));
#99814=CARTESIAN_POINT('Origin',(64.2716888376656,13.375,25.5));
#99815=CARTESIAN_POINT('',(64.2716888376656,13.375,25.5));
#99816=CARTESIAN_POINT('',(64.2716888376656,13.375,25.5));
#99817=CARTESIAN_POINT('',(64.2716888376656,13.375,31.5));
#99818=CARTESIAN_POINT('',(64.2716888376656,13.375,31.5));
#99819=CARTESIAN_POINT('',(64.2716888376656,13.375,25.5));
#99820=CARTESIAN_POINT('Origin',(64.6221242082303,13.375,25.5));
#99821=CARTESIAN_POINT('',(64.6221242082303,13.375,25.5));
#99822=CARTESIAN_POINT('',(64.6221242082303,13.375,25.5));
#99823=CARTESIAN_POINT('',(64.6221242082303,13.375,31.5));
#99824=CARTESIAN_POINT('',(64.6221242082303,13.375,31.5));
#99825=CARTESIAN_POINT('',(64.6221242082303,13.375,25.5));
#99826=CARTESIAN_POINT('Origin',(65.0133922100665,14.45,25.5));
#99827=CARTESIAN_POINT('',(65.0133922100665,14.45,25.5));
#99828=CARTESIAN_POINT('',(65.0133922100665,14.45,25.5));
#99829=CARTESIAN_POINT('',(65.0133922100665,14.45,31.5));
#99830=CARTESIAN_POINT('',(65.0133922100665,14.45,31.5));
#99831=CARTESIAN_POINT('',(65.0133922100665,14.45,25.5));
#99832=CARTESIAN_POINT('Origin',(65.4512171626244,14.45,25.5));
#99833=CARTESIAN_POINT('',(65.4512171626244,14.45,25.5));
#99834=CARTESIAN_POINT('',(65.4512171626244,14.45,25.5));
#99835=CARTESIAN_POINT('',(65.4512171626244,14.45,31.5));
#99836=CARTESIAN_POINT('',(65.4512171626244,14.45,31.5));
#99837=CARTESIAN_POINT('',(65.4512171626244,14.45,25.5));
#99838=CARTESIAN_POINT('Origin',(65.8424851644606,13.375,25.5));
#99839=CARTESIAN_POINT('',(65.8424851644606,13.375,25.5));
#99840=CARTESIAN_POINT('',(65.8424851644606,13.375,25.5));
#99841=CARTESIAN_POINT('',(65.8424851644606,13.375,31.5));
#99842=CARTESIAN_POINT('',(65.8424851644606,13.375,31.5));
#99843=CARTESIAN_POINT('',(65.8424851644606,13.375,25.5));
#99844=CARTESIAN_POINT('Origin',(66.1929205350253,13.375,25.5));
#99845=CARTESIAN_POINT('',(66.1929205350253,13.375,25.5));
#99846=CARTESIAN_POINT('',(66.1929205350253,13.375,25.5));
#99847=CARTESIAN_POINT('',(66.1929205350253,13.375,31.5));
#99848=CARTESIAN_POINT('',(66.1929205350253,13.375,31.5));
#99849=CARTESIAN_POINT('',(66.1929205350253,13.375,25.5));
#99850=CARTESIAN_POINT('Origin',(66.5841885368614,14.45,25.5));
#99851=CARTESIAN_POINT('',(66.5841885368614,14.45,25.5));
#99852=CARTESIAN_POINT('',(66.5841885368614,14.45,25.5));
#99853=CARTESIAN_POINT('',(66.5841885368614,14.45,31.5));
#99854=CARTESIAN_POINT('',(66.5841885368614,14.45,31.5));
#99855=CARTESIAN_POINT('',(66.5841885368614,14.45,25.5));
#99856=CARTESIAN_POINT('Origin',(67.0220134894193,14.45,25.5));
#99857=CARTESIAN_POINT('',(67.0220134894193,14.45,25.5));
#99858=CARTESIAN_POINT('',(67.0220134894193,14.45,25.5));
#99859=CARTESIAN_POINT('',(67.0220134894193,14.45,31.5));
#99860=CARTESIAN_POINT('',(67.0220134894193,14.45,31.5));
#99861=CARTESIAN_POINT('',(67.0220134894193,14.45,25.5));
#99862=CARTESIAN_POINT('Origin',(67.4132814912554,13.375,25.5));
#99863=CARTESIAN_POINT('',(67.4132814912554,13.375,25.5));
#99864=CARTESIAN_POINT('',(67.4132814912554,13.375,25.5));
#99865=CARTESIAN_POINT('',(67.4132814912554,13.375,31.5));
#99866=CARTESIAN_POINT('',(67.4132814912554,13.375,31.5));
#99867=CARTESIAN_POINT('',(67.4132814912554,13.375,25.5));
#99868=CARTESIAN_POINT('Origin',(67.7637168618201,13.375,25.5));
#99869=CARTESIAN_POINT('',(67.7637168618201,13.375,25.5));
#99870=CARTESIAN_POINT('',(67.7637168618201,13.375,25.5));
#99871=CARTESIAN_POINT('',(67.7637168618201,13.375,31.5));
#99872=CARTESIAN_POINT('',(67.7637168618201,13.375,31.5));
#99873=CARTESIAN_POINT('',(67.7637168618201,13.375,25.5));
#99874=CARTESIAN_POINT('Origin',(68.1549848636563,14.45,25.5));
#99875=CARTESIAN_POINT('',(68.1549848636563,14.45,25.5));
#99876=CARTESIAN_POINT('',(68.1549848636563,14.45,25.5));
#99877=CARTESIAN_POINT('',(68.1549848636563,14.45,31.5));
#99878=CARTESIAN_POINT('',(68.1549848636563,14.45,31.5));
#99879=CARTESIAN_POINT('',(68.1549848636563,14.45,25.5));
#99880=CARTESIAN_POINT('Origin',(68.5928098162142,14.45,25.5));
#99881=CARTESIAN_POINT('',(68.5928098162142,14.45,25.5));
#99882=CARTESIAN_POINT('',(68.5928098162142,14.45,25.5));
#99883=CARTESIAN_POINT('',(68.5928098162142,14.45,31.5));
#99884=CARTESIAN_POINT('',(68.5928098162142,14.45,31.5));
#99885=CARTESIAN_POINT('',(68.5928098162142,14.45,25.5));
#99886=CARTESIAN_POINT('Origin',(68.9840778180503,13.375,25.5));
#99887=CARTESIAN_POINT('',(68.9840778180503,13.375,25.5));
#99888=CARTESIAN_POINT('',(68.9840778180503,13.375,25.5));
#99889=CARTESIAN_POINT('',(68.9840778180503,13.375,31.5));
#99890=CARTESIAN_POINT('',(68.9840778180503,13.375,31.5));
#99891=CARTESIAN_POINT('',(68.9840778180503,13.375,25.5));
#99892=CARTESIAN_POINT('Origin',(69.334513188615,13.375,25.5));
#99893=CARTESIAN_POINT('',(69.334513188615,13.375,25.5));
#99894=CARTESIAN_POINT('',(69.334513188615,13.375,25.5));
#99895=CARTESIAN_POINT('',(69.334513188615,13.375,31.5));
#99896=CARTESIAN_POINT('',(69.334513188615,13.375,31.5));
#99897=CARTESIAN_POINT('',(69.334513188615,13.375,25.5));
#99898=CARTESIAN_POINT('Origin',(69.7257811904512,14.45,25.5));
#99899=CARTESIAN_POINT('',(69.7257811904512,14.45,25.5));
#99900=CARTESIAN_POINT('',(69.7257811904512,14.45,25.5));
#99901=CARTESIAN_POINT('',(69.7257811904512,14.45,31.5));
#99902=CARTESIAN_POINT('',(69.7257811904512,14.45,31.5));
#99903=CARTESIAN_POINT('',(69.7257811904512,14.45,25.5));
#99904=CARTESIAN_POINT('Origin',(70.1636061430091,14.45,25.5));
#99905=CARTESIAN_POINT('',(70.1636061430091,14.45,25.5));
#99906=CARTESIAN_POINT('',(70.1636061430091,14.45,25.5));
#99907=CARTESIAN_POINT('',(70.1636061430091,14.45,31.5));
#99908=CARTESIAN_POINT('',(70.1636061430091,14.45,31.5));
#99909=CARTESIAN_POINT('',(70.1636061430091,14.45,25.5));
#99910=CARTESIAN_POINT('Origin',(70.5548741448452,13.375,25.5));
#99911=CARTESIAN_POINT('',(70.5548741448452,13.375,25.5));
#99912=CARTESIAN_POINT('',(70.5548741448452,13.375,25.5));
#99913=CARTESIAN_POINT('',(70.5548741448452,13.375,31.5));
#99914=CARTESIAN_POINT('',(70.5548741448452,13.375,31.5));
#99915=CARTESIAN_POINT('',(70.5548741448452,13.375,25.5));
#99916=CARTESIAN_POINT('Origin',(70.9053095154099,13.375,25.5));
#99917=CARTESIAN_POINT('',(70.9053095154099,13.375,25.5));
#99918=CARTESIAN_POINT('',(70.9053095154099,13.375,25.5));
#99919=CARTESIAN_POINT('',(70.9053095154099,13.375,31.5));
#99920=CARTESIAN_POINT('',(70.9053095154099,13.375,31.5));
#99921=CARTESIAN_POINT('',(70.9053095154099,13.375,25.5));
#99922=CARTESIAN_POINT('Origin',(71.2965775172461,14.45,25.5));
#99923=CARTESIAN_POINT('',(71.2965775172461,14.45,25.5));
#99924=CARTESIAN_POINT('',(71.2965775172461,14.45,25.5));
#99925=CARTESIAN_POINT('',(71.2965775172461,14.45,31.5));
#99926=CARTESIAN_POINT('',(71.2965775172461,14.45,31.5));
#99927=CARTESIAN_POINT('',(71.2965775172461,14.45,25.5));
#99928=CARTESIAN_POINT('Origin',(71.734402469804,14.45,25.5));
#99929=CARTESIAN_POINT('',(71.734402469804,14.45,25.5));
#99930=CARTESIAN_POINT('',(71.734402469804,14.45,25.5));
#99931=CARTESIAN_POINT('',(71.734402469804,14.45,31.5));
#99932=CARTESIAN_POINT('',(71.734402469804,14.45,31.5));
#99933=CARTESIAN_POINT('',(71.734402469804,14.45,25.5));
#99934=CARTESIAN_POINT('Origin',(72.1256704716401,13.375,25.5));
#99935=CARTESIAN_POINT('',(72.1256704716401,13.375,25.5));
#99936=CARTESIAN_POINT('',(72.1256704716401,13.375,25.5));
#99937=CARTESIAN_POINT('',(72.1256704716401,13.375,31.5));
#99938=CARTESIAN_POINT('',(72.1256704716401,13.375,31.5));
#99939=CARTESIAN_POINT('',(72.1256704716401,13.375,25.5));
#99940=CARTESIAN_POINT('Origin',(72.4761058422048,13.375,25.5));
#99941=CARTESIAN_POINT('',(72.4761058422048,13.375,25.5));
#99942=CARTESIAN_POINT('',(72.4761058422048,13.375,25.5));
#99943=CARTESIAN_POINT('',(72.4761058422048,13.375,31.5));
#99944=CARTESIAN_POINT('',(72.4761058422048,13.375,31.5));
#99945=CARTESIAN_POINT('',(72.4761058422048,13.375,25.5));
#99946=CARTESIAN_POINT('Origin',(72.867373844041,14.45,25.5));
#99947=CARTESIAN_POINT('',(72.867373844041,14.45,25.5));
#99948=CARTESIAN_POINT('',(72.867373844041,14.45,25.5));
#99949=CARTESIAN_POINT('',(72.867373844041,14.45,31.5));
#99950=CARTESIAN_POINT('',(72.867373844041,14.45,31.5));
#99951=CARTESIAN_POINT('',(72.867373844041,14.45,25.5));
#99952=CARTESIAN_POINT('Origin',(73.3051987965989,14.45,25.5));
#99953=CARTESIAN_POINT('',(73.3051987965989,14.45,25.5));
#99954=CARTESIAN_POINT('',(73.3051987965989,14.45,25.5));
#99955=CARTESIAN_POINT('',(73.3051987965989,14.45,31.5));
#99956=CARTESIAN_POINT('',(73.3051987965989,14.45,31.5));
#99957=CARTESIAN_POINT('',(73.3051987965989,14.45,25.5));
#99958=CARTESIAN_POINT('Origin',(73.696466798435,13.375,25.5));
#99959=CARTESIAN_POINT('',(73.696466798435,13.375,25.5));
#99960=CARTESIAN_POINT('',(73.696466798435,13.375,25.5));
#99961=CARTESIAN_POINT('',(73.696466798435,13.375,31.5));
#99962=CARTESIAN_POINT('',(73.696466798435,13.375,31.5));
#99963=CARTESIAN_POINT('',(73.696466798435,13.375,25.5));
#99964=CARTESIAN_POINT('Origin',(74.0469021689997,13.375,25.5));
#99965=CARTESIAN_POINT('',(74.0469021689997,13.375,25.5));
#99966=CARTESIAN_POINT('',(74.0469021689997,13.375,25.5));
#99967=CARTESIAN_POINT('',(74.0469021689997,13.375,31.5));
#99968=CARTESIAN_POINT('',(74.0469021689997,13.375,31.5));
#99969=CARTESIAN_POINT('',(74.0469021689997,13.375,25.5));
#99970=CARTESIAN_POINT('Origin',(74.4381701708359,14.45,25.5));
#99971=CARTESIAN_POINT('',(74.4381701708359,14.45,25.5));
#99972=CARTESIAN_POINT('',(74.4381701708359,14.45,25.5));
#99973=CARTESIAN_POINT('',(74.4381701708359,14.45,31.5));
#99974=CARTESIAN_POINT('',(74.4381701708359,14.45,31.5));
#99975=CARTESIAN_POINT('',(74.4381701708359,14.45,25.5));
#99976=CARTESIAN_POINT('Origin',(74.8759951233938,14.45,25.5));
#99977=CARTESIAN_POINT('',(74.8759951233938,14.45,25.5));
#99978=CARTESIAN_POINT('',(74.8759951233938,14.45,25.5));
#99979=CARTESIAN_POINT('',(74.8759951233938,14.45,31.5));
#99980=CARTESIAN_POINT('',(74.8759951233938,14.45,31.5));
#99981=CARTESIAN_POINT('',(74.8759951233938,14.45,25.5));
#99982=CARTESIAN_POINT('Origin',(75.2672631252299,13.375,25.5));
#99983=CARTESIAN_POINT('',(75.2672631252299,13.375,25.5));
#99984=CARTESIAN_POINT('',(75.2672631252299,13.375,25.5));
#99985=CARTESIAN_POINT('',(75.2672631252299,13.375,31.5));
#99986=CARTESIAN_POINT('',(75.2672631252299,13.375,31.5));
#99987=CARTESIAN_POINT('',(75.2672631252299,13.375,25.5));
#99988=CARTESIAN_POINT('Origin',(75.6176984957946,13.375,25.5));
#99989=CARTESIAN_POINT('',(75.6176984957946,13.375,25.5));
#99990=CARTESIAN_POINT('',(75.6176984957946,13.375,25.5));
#99991=CARTESIAN_POINT('',(75.6176984957946,13.375,31.5));
#99992=CARTESIAN_POINT('',(75.6176984957946,13.375,31.5));
#99993=CARTESIAN_POINT('',(75.6176984957946,13.375,25.5));
#99994=CARTESIAN_POINT('Origin',(76.0089664976308,14.45,25.5));
#99995=CARTESIAN_POINT('',(76.0089664976308,14.45,25.5));
#99996=CARTESIAN_POINT('',(76.0089664976308,14.45,25.5));
#99997=CARTESIAN_POINT('',(76.0089664976308,14.45,31.5));
#99998=CARTESIAN_POINT('',(76.0089664976308,14.45,31.5));
#99999=CARTESIAN_POINT('',(76.0089664976308,14.45,25.5));
#100000=CARTESIAN_POINT('Origin',(76.4467914501887,14.45,25.5));
#100001=CARTESIAN_POINT('',(76.4467914501887,14.45,25.5));
#100002=CARTESIAN_POINT('',(76.4467914501887,14.45,25.5));
#100003=CARTESIAN_POINT('',(76.4467914501887,14.45,31.5));
#100004=CARTESIAN_POINT('',(76.4467914501887,14.45,31.5));
#100005=CARTESIAN_POINT('',(76.4467914501887,14.45,25.5));
#100006=CARTESIAN_POINT('Origin',(76.8380594520248,13.375,25.5));
#100007=CARTESIAN_POINT('',(76.8380594520248,13.375,25.5));
#100008=CARTESIAN_POINT('',(76.8380594520248,13.375,25.5));
#100009=CARTESIAN_POINT('',(76.8380594520248,13.375,31.5));
#100010=CARTESIAN_POINT('',(76.8380594520248,13.375,31.5));
#100011=CARTESIAN_POINT('',(76.8380594520248,13.375,25.5));
#100012=CARTESIAN_POINT('Origin',(77.1884948225895,13.375,25.5));
#100013=CARTESIAN_POINT('',(77.1884948225895,13.375,25.5));
#100014=CARTESIAN_POINT('',(77.1884948225895,13.375,25.5));
#100015=CARTESIAN_POINT('',(77.1884948225895,13.375,31.5));
#100016=CARTESIAN_POINT('',(77.1884948225895,13.375,31.5));
#100017=CARTESIAN_POINT('',(77.1884948225895,13.375,25.5));
#100018=CARTESIAN_POINT('Origin',(77.5797628244257,14.45,25.5));
#100019=CARTESIAN_POINT('',(77.5797628244257,14.45,25.5));
#100020=CARTESIAN_POINT('',(77.5797628244257,14.45,25.5));
#100021=CARTESIAN_POINT('',(77.5797628244257,14.45,31.5));
#100022=CARTESIAN_POINT('',(77.5797628244257,14.45,31.5));
#100023=CARTESIAN_POINT('',(77.5797628244257,14.45,25.5));
#100024=CARTESIAN_POINT('Origin',(78.0175877769835,14.45,25.5));
#100025=CARTESIAN_POINT('',(78.0175877769835,14.45,25.5));
#100026=CARTESIAN_POINT('',(78.0175877769835,14.45,25.5));
#100027=CARTESIAN_POINT('',(78.0175877769835,14.45,31.5));
#100028=CARTESIAN_POINT('',(78.0175877769835,14.45,31.5));
#100029=CARTESIAN_POINT('',(78.0175877769835,14.45,25.5));
#100030=CARTESIAN_POINT('Origin',(78.4088557788197,13.375,25.5));
#100031=CARTESIAN_POINT('',(78.4088557788197,13.375,25.5));
#100032=CARTESIAN_POINT('',(78.4088557788197,13.375,25.5));
#100033=CARTESIAN_POINT('',(78.4088557788197,13.375,31.5));
#100034=CARTESIAN_POINT('',(78.4088557788197,13.375,31.5));
#100035=CARTESIAN_POINT('',(78.4088557788197,13.375,25.5));
#100036=CARTESIAN_POINT('Origin',(78.7592911493844,13.375,25.5));
#100037=CARTESIAN_POINT('',(78.7592911493844,13.375,25.5));
#100038=CARTESIAN_POINT('',(78.7592911493844,13.375,25.5));
#100039=CARTESIAN_POINT('',(78.7592911493844,13.375,31.5));
#100040=CARTESIAN_POINT('',(78.7592911493844,13.375,31.5));
#100041=CARTESIAN_POINT('',(78.7592911493844,13.375,25.5));
#100042=CARTESIAN_POINT('Origin',(79.1505591512206,14.45,25.5));
#100043=CARTESIAN_POINT('',(79.1505591512206,14.45,25.5));
#100044=CARTESIAN_POINT('',(79.1505591512206,14.45,25.5));
#100045=CARTESIAN_POINT('',(79.1505591512206,14.45,31.5));
#100046=CARTESIAN_POINT('',(79.1505591512206,14.45,31.5));
#100047=CARTESIAN_POINT('',(79.1505591512206,14.45,25.5));
#100048=CARTESIAN_POINT('Origin',(79.5883841037785,14.45,25.5));
#100049=CARTESIAN_POINT('',(79.5883841037785,14.45,25.5));
#100050=CARTESIAN_POINT('',(79.5883841037785,14.45,25.5));
#100051=CARTESIAN_POINT('',(79.5883841037785,14.45,31.5));
#100052=CARTESIAN_POINT('',(79.5883841037785,14.45,31.5));
#100053=CARTESIAN_POINT('',(79.5883841037785,14.45,25.5));
#100054=CARTESIAN_POINT('Origin',(79.9796521056146,13.375,25.5));
#100055=CARTESIAN_POINT('',(79.9796521056146,13.375,25.5));
#100056=CARTESIAN_POINT('',(79.9796521056146,13.375,25.5));
#100057=CARTESIAN_POINT('',(79.9796521056146,13.375,31.5));
#100058=CARTESIAN_POINT('',(79.9796521056146,13.375,31.5));
#100059=CARTESIAN_POINT('',(79.9796521056146,13.375,25.5));
#100060=CARTESIAN_POINT('Origin',(80.3300874761793,13.375,25.5));
#100061=CARTESIAN_POINT('',(80.3300874761793,13.375,25.5));
#100062=CARTESIAN_POINT('',(80.3300874761793,13.375,25.5));
#100063=CARTESIAN_POINT('',(80.3300874761793,13.375,31.5));
#100064=CARTESIAN_POINT('',(80.3300874761793,13.375,31.5));
#100065=CARTESIAN_POINT('',(80.3300874761793,13.375,25.5));
#100066=CARTESIAN_POINT('Origin',(80.7213554780155,14.45,25.5));
#100067=CARTESIAN_POINT('',(80.7213554780155,14.45,25.5));
#100068=CARTESIAN_POINT('',(80.7213554780155,14.45,25.5));
#100069=CARTESIAN_POINT('',(80.7213554780155,14.45,31.5));
#100070=CARTESIAN_POINT('',(80.7213554780155,14.45,31.5));
#100071=CARTESIAN_POINT('',(80.7213554780155,14.45,25.5));
#100072=CARTESIAN_POINT('Origin',(81.1591804305733,14.45,25.5));
#100073=CARTESIAN_POINT('',(81.1591804305733,14.45,25.5));
#100074=CARTESIAN_POINT('',(81.1591804305733,14.45,25.5));
#100075=CARTESIAN_POINT('',(81.1591804305733,14.45,31.5));
#100076=CARTESIAN_POINT('',(81.1591804305733,14.45,31.5));
#100077=CARTESIAN_POINT('',(81.1591804305733,14.45,25.5));
#100078=CARTESIAN_POINT('Origin',(81.5504484324095,13.375,25.5));
#100079=CARTESIAN_POINT('',(81.5504484324095,13.375,25.5));
#100080=CARTESIAN_POINT('',(81.5504484324095,13.375,25.5));
#100081=CARTESIAN_POINT('',(81.5504484324095,13.375,31.5));
#100082=CARTESIAN_POINT('',(81.5504484324095,13.375,31.5));
#100083=CARTESIAN_POINT('',(81.5504484324095,13.375,25.5));
#100084=CARTESIAN_POINT('Origin',(81.9008838029742,13.375,25.5));
#100085=CARTESIAN_POINT('',(81.9008838029742,13.375,25.5));
#100086=CARTESIAN_POINT('',(81.9008838029742,13.375,25.5));
#100087=CARTESIAN_POINT('',(81.9008838029742,13.375,31.5));
#100088=CARTESIAN_POINT('',(81.9008838029742,13.375,31.5));
#100089=CARTESIAN_POINT('',(81.9008838029742,13.375,25.5));
#100090=CARTESIAN_POINT('Origin',(82.2921518048104,14.45,25.5));
#100091=CARTESIAN_POINT('',(82.2921518048104,14.45,25.5));
#100092=CARTESIAN_POINT('',(82.2921518048104,14.45,25.5));
#100093=CARTESIAN_POINT('',(82.2921518048104,14.45,31.5));
#100094=CARTESIAN_POINT('',(82.2921518048104,14.45,31.5));
#100095=CARTESIAN_POINT('',(82.2921518048104,14.45,25.5));
#100096=CARTESIAN_POINT('Origin',(82.7299767573682,14.45,25.5));
#100097=CARTESIAN_POINT('',(82.7299767573682,14.45,25.5));
#100098=CARTESIAN_POINT('',(82.7299767573682,14.45,25.5));
#100099=CARTESIAN_POINT('',(82.7299767573682,14.45,31.5));
#100100=CARTESIAN_POINT('',(82.7299767573682,14.45,31.5));
#100101=CARTESIAN_POINT('',(82.7299767573682,14.45,25.5));
#100102=CARTESIAN_POINT('Origin',(83.1212447592044,13.375,25.5));
#100103=CARTESIAN_POINT('',(83.1212447592044,13.375,25.5));
#100104=CARTESIAN_POINT('',(83.1212447592044,13.375,25.5));
#100105=CARTESIAN_POINT('',(83.1212447592044,13.375,31.5));
#100106=CARTESIAN_POINT('',(83.1212447592044,13.375,31.5));
#100107=CARTESIAN_POINT('',(83.1212447592044,13.375,25.5));
#100108=CARTESIAN_POINT('Origin',(83.4716801297691,13.375,25.5));
#100109=CARTESIAN_POINT('',(83.4716801297691,13.375,25.5));
#100110=CARTESIAN_POINT('',(83.4716801297691,13.375,25.5));
#100111=CARTESIAN_POINT('',(83.4716801297691,13.375,31.5));
#100112=CARTESIAN_POINT('',(83.4716801297691,13.375,31.5));
#100113=CARTESIAN_POINT('',(83.4716801297691,13.375,25.5));
#100114=CARTESIAN_POINT('Origin',(83.8629481316053,14.45,25.5));
#100115=CARTESIAN_POINT('',(83.8629481316053,14.45,25.5));
#100116=CARTESIAN_POINT('',(83.8629481316053,14.45,25.5));
#100117=CARTESIAN_POINT('',(83.8629481316053,14.45,31.5));
#100118=CARTESIAN_POINT('',(83.8629481316053,14.45,31.5));
#100119=CARTESIAN_POINT('',(83.8629481316053,14.45,25.5));
#100120=CARTESIAN_POINT('Origin',(84.3007730841631,14.45,25.5));
#100121=CARTESIAN_POINT('',(84.3007730841631,14.45,25.5));
#100122=CARTESIAN_POINT('',(84.3007730841631,14.45,25.5));
#100123=CARTESIAN_POINT('',(84.3007730841631,14.45,31.5));
#100124=CARTESIAN_POINT('',(84.3007730841631,14.45,31.5));
#100125=CARTESIAN_POINT('',(84.3007730841631,14.45,25.5));
#100126=CARTESIAN_POINT('Origin',(84.6920410859993,13.375,25.5));
#100127=CARTESIAN_POINT('',(84.6920410859993,13.375,25.5));
#100128=CARTESIAN_POINT('',(84.6920410859993,13.375,25.5));
#100129=CARTESIAN_POINT('',(84.6920410859993,13.375,31.5));
#100130=CARTESIAN_POINT('',(84.6920410859993,13.375,31.5));
#100131=CARTESIAN_POINT('',(84.6920410859993,13.375,25.5));
#100132=CARTESIAN_POINT('Origin',(85.042476456564,13.375,25.5));
#100133=CARTESIAN_POINT('',(85.042476456564,13.375,25.5));
#100134=CARTESIAN_POINT('',(85.042476456564,13.375,25.5));
#100135=CARTESIAN_POINT('',(85.042476456564,13.375,31.5));
#100136=CARTESIAN_POINT('',(85.042476456564,13.375,31.5));
#100137=CARTESIAN_POINT('',(85.042476456564,13.375,25.5));
#100138=CARTESIAN_POINT('Origin',(85.4337444584002,14.45,25.5));
#100139=CARTESIAN_POINT('',(85.4337444584002,14.45,25.5));
#100140=CARTESIAN_POINT('',(85.4337444584002,14.45,25.5));
#100141=CARTESIAN_POINT('',(85.4337444584002,14.45,31.5));
#100142=CARTESIAN_POINT('',(85.4337444584002,14.45,31.5));
#100143=CARTESIAN_POINT('',(85.4337444584002,14.45,25.5));
#100144=CARTESIAN_POINT('Origin',(85.871569410958,14.45,25.5));
#100145=CARTESIAN_POINT('',(85.871569410958,14.45,25.5));
#100146=CARTESIAN_POINT('',(85.871569410958,14.45,25.5));
#100147=CARTESIAN_POINT('',(85.871569410958,14.45,31.5));
#100148=CARTESIAN_POINT('',(85.871569410958,14.45,31.5));
#100149=CARTESIAN_POINT('',(85.871569410958,14.45,25.5));
#100150=CARTESIAN_POINT('Origin',(86.2628374127942,13.375,25.5));
#100151=CARTESIAN_POINT('',(86.2628374127942,13.375,25.5));
#100152=CARTESIAN_POINT('',(86.2628374127942,13.375,25.5));
#100153=CARTESIAN_POINT('',(86.2628374127942,13.375,31.5));
#100154=CARTESIAN_POINT('',(86.2628374127942,13.375,31.5));
#100155=CARTESIAN_POINT('',(86.2628374127942,13.375,25.5));
#100156=CARTESIAN_POINT('Origin',(86.6132727833589,13.375,25.5));
#100157=CARTESIAN_POINT('',(86.6132727833589,13.375,25.5));
#100158=CARTESIAN_POINT('',(86.6132727833589,13.375,25.5));
#100159=CARTESIAN_POINT('',(86.6132727833589,13.375,31.5));
#100160=CARTESIAN_POINT('',(86.6132727833589,13.375,31.5));
#100161=CARTESIAN_POINT('',(86.6132727833589,13.375,25.5));
#100162=CARTESIAN_POINT('Origin',(87.0045407851951,14.45,25.5));
#100163=CARTESIAN_POINT('',(87.0045407851951,14.45,25.5));
#100164=CARTESIAN_POINT('',(87.0045407851951,14.45,25.5));
#100165=CARTESIAN_POINT('',(87.0045407851951,14.45,31.5));
#100166=CARTESIAN_POINT('',(87.0045407851951,14.45,31.5));
#100167=CARTESIAN_POINT('',(87.0045407851951,14.45,25.5));
#100168=CARTESIAN_POINT('Origin',(87.4423657377529,14.45,25.5));
#100169=CARTESIAN_POINT('',(87.4423657377529,14.45,25.5));
#100170=CARTESIAN_POINT('',(87.4423657377529,14.45,25.5));
#100171=CARTESIAN_POINT('',(87.4423657377529,14.45,31.5));
#100172=CARTESIAN_POINT('',(87.4423657377529,14.45,31.5));
#100173=CARTESIAN_POINT('',(87.4423657377529,14.45,25.5));
#100174=CARTESIAN_POINT('Origin',(87.8336337395891,13.375,25.5));
#100175=CARTESIAN_POINT('',(87.8336337395891,13.375,25.5));
#100176=CARTESIAN_POINT('',(87.8336337395891,13.375,25.5));
#100177=CARTESIAN_POINT('',(87.8336337395891,13.375,31.5));
#100178=CARTESIAN_POINT('',(87.8336337395891,13.375,31.5));
#100179=CARTESIAN_POINT('',(87.8336337395891,13.375,25.5));
#100180=CARTESIAN_POINT('Origin',(88.1840691101538,13.375,25.5));
#100181=CARTESIAN_POINT('',(88.1840691101538,13.375,25.5));
#100182=CARTESIAN_POINT('',(88.1840691101538,13.375,25.5));
#100183=CARTESIAN_POINT('',(88.1840691101538,13.375,31.5));
#100184=CARTESIAN_POINT('',(88.1840691101538,13.375,31.5));
#100185=CARTESIAN_POINT('',(88.1840691101538,13.375,25.5));
#100186=CARTESIAN_POINT('Origin',(88.57533711199,14.45,25.5));
#100187=CARTESIAN_POINT('',(88.57533711199,14.45,25.5));
#100188=CARTESIAN_POINT('',(88.57533711199,14.45,25.5));
#100189=CARTESIAN_POINT('',(88.57533711199,14.45,31.5));
#100190=CARTESIAN_POINT('',(88.57533711199,14.45,31.5));
#100191=CARTESIAN_POINT('',(88.57533711199,14.45,25.5));
#100192=CARTESIAN_POINT('Origin',(89.0131620645478,14.45,25.5));
#100193=CARTESIAN_POINT('',(89.0131620645478,14.45,25.5));
#100194=CARTESIAN_POINT('',(89.0131620645478,14.45,25.5));
#100195=CARTESIAN_POINT('',(89.0131620645478,14.45,31.5));
#100196=CARTESIAN_POINT('',(89.0131620645478,14.45,31.5));
#100197=CARTESIAN_POINT('',(89.0131620645478,14.45,25.5));
#100198=CARTESIAN_POINT('Origin',(89.404430066384,13.375,25.5));
#100199=CARTESIAN_POINT('',(89.404430066384,13.375,25.5));
#100200=CARTESIAN_POINT('',(89.404430066384,13.375,25.5));
#100201=CARTESIAN_POINT('',(89.404430066384,13.375,31.5));
#100202=CARTESIAN_POINT('',(89.404430066384,13.375,31.5));
#100203=CARTESIAN_POINT('',(89.404430066384,13.375,25.5));
#100204=CARTESIAN_POINT('Origin',(89.7548654369487,13.375,25.5));
#100205=CARTESIAN_POINT('',(89.7548654369487,13.375,25.5));
#100206=CARTESIAN_POINT('',(89.7548654369487,13.375,25.5));
#100207=CARTESIAN_POINT('',(89.7548654369487,13.375,31.5));
#100208=CARTESIAN_POINT('',(89.7548654369487,13.375,31.5));
#100209=CARTESIAN_POINT('',(89.7548654369487,13.375,25.5));
#100210=CARTESIAN_POINT('Origin',(90.1461334387849,14.45,25.5));
#100211=CARTESIAN_POINT('',(90.1461334387849,14.45,25.5));
#100212=CARTESIAN_POINT('',(90.1461334387849,14.45,25.5));
#100213=CARTESIAN_POINT('',(90.1461334387849,14.45,31.5));
#100214=CARTESIAN_POINT('',(90.1461334387849,14.45,31.5));
#100215=CARTESIAN_POINT('',(90.1461334387849,14.45,25.5));
#100216=CARTESIAN_POINT('Origin',(90.5839583913427,14.45,25.5));
#100217=CARTESIAN_POINT('',(90.5839583913427,14.45,25.5));
#100218=CARTESIAN_POINT('',(90.5839583913427,14.45,25.5));
#100219=CARTESIAN_POINT('',(90.5839583913427,14.45,31.5));
#100220=CARTESIAN_POINT('',(90.5839583913427,14.45,31.5));
#100221=CARTESIAN_POINT('',(90.5839583913427,14.45,25.5));
#100222=CARTESIAN_POINT('Origin',(90.9752263931789,13.375,25.5));
#100223=CARTESIAN_POINT('',(90.9752263931789,13.375,25.5));
#100224=CARTESIAN_POINT('',(90.9752263931789,13.375,25.5));
#100225=CARTESIAN_POINT('',(90.9752263931789,13.375,31.5));
#100226=CARTESIAN_POINT('',(90.9752263931789,13.375,31.5));
#100227=CARTESIAN_POINT('',(90.9752263931789,13.375,25.5));
#100228=CARTESIAN_POINT('Origin',(91.3256617637436,13.375,25.5));
#100229=CARTESIAN_POINT('',(91.3256617637436,13.375,25.5));
#100230=CARTESIAN_POINT('',(91.3256617637436,13.375,25.5));
#100231=CARTESIAN_POINT('',(91.3256617637436,13.375,31.5));
#100232=CARTESIAN_POINT('',(91.3256617637436,13.375,31.5));
#100233=CARTESIAN_POINT('',(91.3256617637436,13.375,25.5));
#100234=CARTESIAN_POINT('Origin',(91.7169297655798,14.45,25.5));
#100235=CARTESIAN_POINT('',(91.7169297655798,14.45,25.5));
#100236=CARTESIAN_POINT('',(91.7169297655798,14.45,25.5));
#100237=CARTESIAN_POINT('',(91.7169297655798,14.45,31.5));
#100238=CARTESIAN_POINT('',(91.7169297655798,14.45,31.5));
#100239=CARTESIAN_POINT('',(91.7169297655798,14.45,25.5));
#100240=CARTESIAN_POINT('Origin',(92.1547547181376,14.45,25.5));
#100241=CARTESIAN_POINT('',(92.1547547181376,14.45,25.5));
#100242=CARTESIAN_POINT('',(92.1547547181376,14.45,25.5));
#100243=CARTESIAN_POINT('',(92.1547547181376,14.45,31.5));
#100244=CARTESIAN_POINT('',(92.1547547181376,14.45,31.5));
#100245=CARTESIAN_POINT('',(92.1547547181376,14.45,25.5));
#100246=CARTESIAN_POINT('Origin',(92.5460227199738,13.375,25.5));
#100247=CARTESIAN_POINT('',(92.5460227199738,13.375,25.5));
#100248=CARTESIAN_POINT('',(92.5460227199738,13.375,25.5));
#100249=CARTESIAN_POINT('',(92.5460227199738,13.375,31.5));
#100250=CARTESIAN_POINT('',(92.5460227199738,13.375,31.5));
#100251=CARTESIAN_POINT('',(92.5460227199738,13.375,25.5));
#100252=CARTESIAN_POINT('Origin',(92.8964580905385,13.375,25.5));
#100253=CARTESIAN_POINT('',(92.8964580905385,13.375,25.5));
#100254=CARTESIAN_POINT('',(92.8964580905385,13.375,25.5));
#100255=CARTESIAN_POINT('',(92.8964580905385,13.375,31.5));
#100256=CARTESIAN_POINT('',(92.8964580905385,13.375,31.5));
#100257=CARTESIAN_POINT('',(92.8964580905385,13.375,25.5));
#100258=CARTESIAN_POINT('Origin',(93.2877260923746,14.45,25.5));
#100259=CARTESIAN_POINT('',(93.2877260923746,14.45,25.5));
#100260=CARTESIAN_POINT('',(93.2877260923746,14.45,25.5));
#100261=CARTESIAN_POINT('',(93.2877260923746,14.45,31.5));
#100262=CARTESIAN_POINT('',(93.2877260923746,14.45,31.5));
#100263=CARTESIAN_POINT('',(93.2877260923746,14.45,25.5));
#100264=CARTESIAN_POINT('Origin',(93.7255510449325,14.45,25.5));
#100265=CARTESIAN_POINT('',(93.7255510449325,14.45,25.5));
#100266=CARTESIAN_POINT('',(93.7255510449325,14.45,25.5));
#100267=CARTESIAN_POINT('',(93.7255510449325,14.45,31.5));
#100268=CARTESIAN_POINT('',(93.7255510449325,14.45,31.5));
#100269=CARTESIAN_POINT('',(93.7255510449325,14.45,25.5));
#100270=CARTESIAN_POINT('Origin',(94.1168190467687,13.375,25.5));
#100271=CARTESIAN_POINT('',(94.1168190467687,13.375,25.5));
#100272=CARTESIAN_POINT('',(94.1168190467687,13.375,25.5));
#100273=CARTESIAN_POINT('',(94.1168190467687,13.375,31.5));
#100274=CARTESIAN_POINT('',(94.1168190467687,13.375,31.5));
#100275=CARTESIAN_POINT('',(94.1168190467687,13.375,25.5));
#100276=CARTESIAN_POINT('Origin',(94.4672544173334,13.375,25.5));
#100277=CARTESIAN_POINT('',(94.4672544173334,13.375,25.5));
#100278=CARTESIAN_POINT('',(94.4672544173334,13.375,25.5));
#100279=CARTESIAN_POINT('',(94.4672544173334,13.375,31.5));
#100280=CARTESIAN_POINT('',(94.4672544173334,13.375,31.5));
#100281=CARTESIAN_POINT('',(94.4672544173334,13.375,25.5));
#100282=CARTESIAN_POINT('Origin',(94.8585224191696,14.45,25.5));
#100283=CARTESIAN_POINT('',(94.8585224191696,14.45,25.5));
#100284=CARTESIAN_POINT('',(94.8585224191696,14.45,25.5));
#100285=CARTESIAN_POINT('',(94.8585224191696,14.45,31.5));
#100286=CARTESIAN_POINT('',(94.8585224191696,14.45,31.5));
#100287=CARTESIAN_POINT('',(94.8585224191696,14.45,25.5));
#100288=CARTESIAN_POINT('Origin',(95.2963473717274,14.45,25.5));
#100289=CARTESIAN_POINT('',(95.2963473717274,14.45,25.5));
#100290=CARTESIAN_POINT('',(95.2963473717274,14.45,25.5));
#100291=CARTESIAN_POINT('',(95.2963473717274,14.45,31.5));
#100292=CARTESIAN_POINT('',(95.2963473717274,14.45,31.5));
#100293=CARTESIAN_POINT('',(95.2963473717274,14.45,25.5));
#100294=CARTESIAN_POINT('Origin',(95.6876153735636,13.375,25.5));
#100295=CARTESIAN_POINT('',(95.6876153735636,13.375,25.5));
#100296=CARTESIAN_POINT('',(95.6876153735636,13.375,25.5));
#100297=CARTESIAN_POINT('',(95.6876153735636,13.375,31.5));
#100298=CARTESIAN_POINT('',(95.6876153735636,13.375,31.5));
#100299=CARTESIAN_POINT('',(95.6876153735636,13.375,25.5));
#100300=CARTESIAN_POINT('Origin',(96.0380507441283,13.375,25.5));
#100301=CARTESIAN_POINT('',(96.0380507441283,13.375,25.5));
#100302=CARTESIAN_POINT('',(96.0380507441283,13.375,25.5));
#100303=CARTESIAN_POINT('',(96.0380507441283,13.375,31.5));
#100304=CARTESIAN_POINT('',(96.0380507441283,13.375,31.5));
#100305=CARTESIAN_POINT('',(96.0380507441283,13.375,25.5));
#100306=CARTESIAN_POINT('Origin',(96.4293187459645,14.45,25.5));
#100307=CARTESIAN_POINT('',(96.4293187459645,14.45,25.5));
#100308=CARTESIAN_POINT('',(96.4293187459645,14.45,25.5));
#100309=CARTESIAN_POINT('',(96.4293187459645,14.45,31.5));
#100310=CARTESIAN_POINT('',(96.4293187459645,14.45,31.5));
#100311=CARTESIAN_POINT('',(96.4293187459645,14.45,25.5));
#100312=CARTESIAN_POINT('Origin',(96.8671436985223,14.45,25.5));
#100313=CARTESIAN_POINT('',(96.8671436985223,14.45,25.5));
#100314=CARTESIAN_POINT('',(96.8671436985223,14.45,25.5));
#100315=CARTESIAN_POINT('',(96.8671436985223,14.45,31.5));
#100316=CARTESIAN_POINT('',(96.8671436985223,14.45,31.5));
#100317=CARTESIAN_POINT('',(96.8671436985223,14.45,25.5));
#100318=CARTESIAN_POINT('Origin',(97.2584117003585,13.375,25.5));
#100319=CARTESIAN_POINT('',(97.2584117003585,13.375,25.5));
#100320=CARTESIAN_POINT('',(97.2584117003585,13.375,25.5));
#100321=CARTESIAN_POINT('',(97.2584117003585,13.375,31.5));
#100322=CARTESIAN_POINT('',(97.2584117003585,13.375,31.5));
#100323=CARTESIAN_POINT('',(97.2584117003585,13.375,25.5));
#100324=CARTESIAN_POINT('Origin',(97.6088470709232,13.375,25.5));
#100325=CARTESIAN_POINT('',(97.6088470709232,13.375,25.5));
#100326=CARTESIAN_POINT('',(97.6088470709232,13.375,25.5));
#100327=CARTESIAN_POINT('',(97.6088470709232,13.375,31.5));
#100328=CARTESIAN_POINT('',(97.6088470709232,13.375,31.5));
#100329=CARTESIAN_POINT('',(97.6088470709232,13.375,25.5));
#100330=CARTESIAN_POINT('Origin',(98.0001150727593,14.45,25.5));
#100331=CARTESIAN_POINT('',(98.0001150727593,14.45,25.5));
#100332=CARTESIAN_POINT('',(98.0001150727593,14.45,25.5));
#100333=CARTESIAN_POINT('',(98.0001150727593,14.45,31.5));
#100334=CARTESIAN_POINT('',(98.0001150727593,14.45,31.5));
#100335=CARTESIAN_POINT('',(98.0001150727593,14.45,25.5));
#100336=CARTESIAN_POINT('Origin',(98.4379400253172,14.45,25.5));
#100337=CARTESIAN_POINT('',(98.4379400253172,14.45,25.5));
#100338=CARTESIAN_POINT('',(98.4379400253172,14.45,25.5));
#100339=CARTESIAN_POINT('',(98.4379400253172,14.45,31.5));
#100340=CARTESIAN_POINT('',(98.4379400253172,14.45,31.5));
#100341=CARTESIAN_POINT('',(98.4379400253172,14.45,25.5));
#100342=CARTESIAN_POINT('Origin',(98.8292080271534,13.375,25.5));
#100343=CARTESIAN_POINT('',(98.8292080271534,13.375,25.5));
#100344=CARTESIAN_POINT('',(98.8292080271534,13.375,25.5));
#100345=CARTESIAN_POINT('',(98.8292080271534,13.375,31.5));
#100346=CARTESIAN_POINT('',(98.8292080271534,13.375,31.5));
#100347=CARTESIAN_POINT('',(98.8292080271534,13.375,25.5));
#100348=CARTESIAN_POINT('Origin',(99.1796433977181,13.375,25.5));
#100349=CARTESIAN_POINT('',(99.1796433977181,13.375,25.5));
#100350=CARTESIAN_POINT('',(99.1796433977181,13.375,25.5));
#100351=CARTESIAN_POINT('',(99.1796433977181,13.375,31.5));
#100352=CARTESIAN_POINT('',(99.1796433977181,13.375,31.5));
#100353=CARTESIAN_POINT('',(99.1796433977181,13.375,25.5));
#100354=CARTESIAN_POINT('Origin',(99.5709113995542,14.45,25.5));
#100355=CARTESIAN_POINT('',(99.5709113995542,14.45,25.5));
#100356=CARTESIAN_POINT('',(99.5709113995542,14.45,25.5));
#100357=CARTESIAN_POINT('',(99.5709113995542,14.45,31.5));
#100358=CARTESIAN_POINT('',(99.5709113995542,14.45,31.5));
#100359=CARTESIAN_POINT('',(99.5709113995542,14.45,25.5));
#100360=CARTESIAN_POINT('Origin',(100.008736352112,14.45,25.5));
#100361=CARTESIAN_POINT('',(100.008736352112,14.45,25.5));
#100362=CARTESIAN_POINT('',(100.008736352112,14.45,25.5));
#100363=CARTESIAN_POINT('',(100.008736352112,14.45,31.5));
#100364=CARTESIAN_POINT('',(100.008736352112,14.45,31.5));
#100365=CARTESIAN_POINT('',(100.008736352112,14.45,25.5));
#100366=CARTESIAN_POINT('Origin',(100.400004353948,13.375,25.5));
#100367=CARTESIAN_POINT('',(100.400004353948,13.375,25.5));
#100368=CARTESIAN_POINT('',(100.400004353948,13.375,25.5));
#100369=CARTESIAN_POINT('',(100.400004353948,13.375,31.5));
#100370=CARTESIAN_POINT('',(100.400004353948,13.375,31.5));
#100371=CARTESIAN_POINT('',(100.400004353948,13.375,25.5));
#100372=CARTESIAN_POINT('Origin',(100.750439724513,13.375,25.5));
#100373=CARTESIAN_POINT('',(100.750439724513,13.375,25.5));
#100374=CARTESIAN_POINT('',(100.750439724513,13.375,25.5));
#100375=CARTESIAN_POINT('',(100.750439724513,13.375,31.5));
#100376=CARTESIAN_POINT('',(100.750439724513,13.375,31.5));
#100377=CARTESIAN_POINT('',(100.750439724513,13.375,25.5));
#100378=CARTESIAN_POINT('Origin',(101.141707726349,14.45,25.5));
#100379=CARTESIAN_POINT('',(101.141707726349,14.45,25.5));
#100380=CARTESIAN_POINT('',(101.141707726349,14.45,25.5));
#100381=CARTESIAN_POINT('',(101.141707726349,14.45,31.5));
#100382=CARTESIAN_POINT('',(101.141707726349,14.45,31.5));
#100383=CARTESIAN_POINT('',(101.141707726349,14.45,25.5));
#100384=CARTESIAN_POINT('Origin',(101.579532678907,14.45,25.5));
#100385=CARTESIAN_POINT('',(101.579532678907,14.45,25.5));
#100386=CARTESIAN_POINT('',(101.579532678907,14.45,25.5));
#100387=CARTESIAN_POINT('',(101.579532678907,14.45,31.5));
#100388=CARTESIAN_POINT('',(101.579532678907,14.45,31.5));
#100389=CARTESIAN_POINT('',(101.579532678907,14.45,25.5));
#100390=CARTESIAN_POINT('Origin',(101.970800680743,13.375,25.5));
#100391=CARTESIAN_POINT('',(101.970800680743,13.375,25.5));
#100392=CARTESIAN_POINT('',(101.970800680743,13.375,25.5));
#100393=CARTESIAN_POINT('',(101.970800680743,13.375,31.5));
#100394=CARTESIAN_POINT('',(101.970800680743,13.375,31.5));
#100395=CARTESIAN_POINT('',(101.970800680743,13.375,25.5));
#100396=CARTESIAN_POINT('Origin',(102.321236051308,13.375,25.5));
#100397=CARTESIAN_POINT('',(102.321236051308,13.375,25.5));
#100398=CARTESIAN_POINT('',(102.321236051308,13.375,25.5));
#100399=CARTESIAN_POINT('',(102.321236051308,13.375,31.5));
#100400=CARTESIAN_POINT('',(102.321236051308,13.375,31.5));
#100401=CARTESIAN_POINT('',(102.321236051308,13.375,25.5));
#100402=CARTESIAN_POINT('Origin',(102.712504053144,14.45,25.5));
#100403=CARTESIAN_POINT('',(102.712504053144,14.45,25.5));
#100404=CARTESIAN_POINT('',(102.712504053144,14.45,25.5));
#100405=CARTESIAN_POINT('',(102.712504053144,14.45,31.5));
#100406=CARTESIAN_POINT('',(102.712504053144,14.45,31.5));
#100407=CARTESIAN_POINT('',(102.712504053144,14.45,25.5));
#100408=CARTESIAN_POINT('Origin',(103.150329005702,14.45,25.5));
#100409=CARTESIAN_POINT('',(103.150329005702,14.45,25.5));
#100410=CARTESIAN_POINT('',(103.150329005702,14.45,25.5));
#100411=CARTESIAN_POINT('',(103.150329005702,14.45,31.5));
#100412=CARTESIAN_POINT('',(103.150329005702,14.45,31.5));
#100413=CARTESIAN_POINT('',(103.150329005702,14.45,25.5));
#100414=CARTESIAN_POINT('Origin',(103.541597007538,13.375,25.5));
#100415=CARTESIAN_POINT('',(103.541597007538,13.375,25.5));
#100416=CARTESIAN_POINT('',(103.541597007538,13.375,25.5));
#100417=CARTESIAN_POINT('',(103.541597007538,13.375,31.5));
#100418=CARTESIAN_POINT('',(103.541597007538,13.375,31.5));
#100419=CARTESIAN_POINT('',(103.541597007538,13.375,25.5));
#100420=CARTESIAN_POINT('Origin',(103.892032378103,13.375,25.5));
#100421=CARTESIAN_POINT('',(103.892032378103,13.375,25.5));
#100422=CARTESIAN_POINT('',(103.892032378103,13.375,25.5));
#100423=CARTESIAN_POINT('',(103.892032378103,13.375,31.5));
#100424=CARTESIAN_POINT('',(103.892032378103,13.375,31.5));
#100425=CARTESIAN_POINT('',(103.892032378103,13.375,25.5));
#100426=CARTESIAN_POINT('Origin',(104.283300379939,14.45,25.5));
#100427=CARTESIAN_POINT('',(104.283300379939,14.45,25.5));
#100428=CARTESIAN_POINT('',(104.283300379939,14.45,25.5));
#100429=CARTESIAN_POINT('',(104.283300379939,14.45,31.5));
#100430=CARTESIAN_POINT('',(104.283300379939,14.45,31.5));
#100431=CARTESIAN_POINT('',(104.283300379939,14.45,25.5));
#100432=CARTESIAN_POINT('Origin',(104.721125332497,14.45,25.5));
#100433=CARTESIAN_POINT('',(104.721125332497,14.45,25.5));
#100434=CARTESIAN_POINT('',(104.721125332497,14.45,25.5));
#100435=CARTESIAN_POINT('',(104.721125332497,14.45,31.5));
#100436=CARTESIAN_POINT('',(104.721125332497,14.45,31.5));
#100437=CARTESIAN_POINT('',(104.721125332497,14.45,25.5));
#100438=CARTESIAN_POINT('Origin',(105.112393334333,13.375,25.5));
#100439=CARTESIAN_POINT('',(105.112393334333,13.375,25.5));
#100440=CARTESIAN_POINT('',(105.112393334333,13.375,25.5));
#100441=CARTESIAN_POINT('',(105.112393334333,13.375,31.5));
#100442=CARTESIAN_POINT('',(105.112393334333,13.375,31.5));
#100443=CARTESIAN_POINT('',(105.112393334333,13.375,25.5));
#100444=CARTESIAN_POINT('Origin',(105.462828704898,13.375,25.5));
#100445=CARTESIAN_POINT('',(105.462828704898,13.375,25.5));
#100446=CARTESIAN_POINT('',(105.462828704898,13.375,25.5));
#100447=CARTESIAN_POINT('',(105.462828704898,13.375,31.5));
#100448=CARTESIAN_POINT('',(105.462828704898,13.375,31.5));
#100449=CARTESIAN_POINT('',(105.462828704898,13.375,25.5));
#100450=CARTESIAN_POINT('Origin',(105.854096706734,14.45,25.5));
#100451=CARTESIAN_POINT('',(105.854096706734,14.45,25.5));
#100452=CARTESIAN_POINT('',(105.854096706734,14.45,25.5));
#100453=CARTESIAN_POINT('',(105.854096706734,14.45,31.5));
#100454=CARTESIAN_POINT('',(105.854096706734,14.45,31.5));
#100455=CARTESIAN_POINT('',(105.854096706734,14.45,25.5));
#100456=CARTESIAN_POINT('Origin',(106.291921659292,14.45,25.5));
#100457=CARTESIAN_POINT('',(106.291921659292,14.45,25.5));
#100458=CARTESIAN_POINT('',(106.291921659292,14.45,25.5));
#100459=CARTESIAN_POINT('',(106.291921659292,14.45,31.5));
#100460=CARTESIAN_POINT('',(106.291921659292,14.45,31.5));
#100461=CARTESIAN_POINT('',(106.291921659292,14.45,25.5));
#100462=CARTESIAN_POINT('Origin',(106.683189661128,13.375,25.5));
#100463=CARTESIAN_POINT('',(106.683189661128,13.375,25.5));
#100464=CARTESIAN_POINT('',(106.683189661128,13.375,25.5));
#100465=CARTESIAN_POINT('',(106.683189661128,13.375,31.5));
#100466=CARTESIAN_POINT('',(106.683189661128,13.375,31.5));
#100467=CARTESIAN_POINT('',(106.683189661128,13.375,25.5));
#100468=CARTESIAN_POINT('Origin',(107.033625031693,13.375,25.5));
#100469=CARTESIAN_POINT('',(107.033625031693,13.375,25.5));
#100470=CARTESIAN_POINT('',(107.033625031693,13.375,25.5));
#100471=CARTESIAN_POINT('',(107.033625031693,13.375,31.5));
#100472=CARTESIAN_POINT('',(107.033625031693,13.375,31.5));
#100473=CARTESIAN_POINT('',(107.033625031693,13.375,25.5));
#100474=CARTESIAN_POINT('Origin',(107.424893033529,14.45,25.5));
#100475=CARTESIAN_POINT('',(107.424893033529,14.45,25.5));
#100476=CARTESIAN_POINT('',(107.424893033529,14.45,25.5));
#100477=CARTESIAN_POINT('',(107.424893033529,14.45,31.5));
#100478=CARTESIAN_POINT('',(107.424893033529,14.45,31.5));
#100479=CARTESIAN_POINT('',(107.424893033529,14.45,25.5));
#100480=CARTESIAN_POINT('Origin',(107.862717986087,14.45,25.5));
#100481=CARTESIAN_POINT('',(107.862717986087,14.45,25.5));
#100482=CARTESIAN_POINT('',(107.862717986087,14.45,25.5));
#100483=CARTESIAN_POINT('',(107.862717986087,14.45,31.5));
#100484=CARTESIAN_POINT('',(107.862717986087,14.45,31.5));
#100485=CARTESIAN_POINT('',(107.862717986087,14.45,25.5));
#100486=CARTESIAN_POINT('Origin',(108.253985987923,13.375,25.5));
#100487=CARTESIAN_POINT('',(108.253985987923,13.375,25.5));
#100488=CARTESIAN_POINT('',(108.253985987923,13.375,25.5));
#100489=CARTESIAN_POINT('',(108.253985987923,13.375,31.5));
#100490=CARTESIAN_POINT('',(108.253985987923,13.375,31.5));
#100491=CARTESIAN_POINT('',(108.253985987923,13.375,25.5));
#100492=CARTESIAN_POINT('Origin',(108.604421358487,13.375,25.5));
#100493=CARTESIAN_POINT('',(108.604421358487,13.375,25.5));
#100494=CARTESIAN_POINT('',(108.604421358487,13.375,25.5));
#100495=CARTESIAN_POINT('',(108.604421358487,13.375,31.5));
#100496=CARTESIAN_POINT('',(108.604421358487,13.375,31.5));
#100497=CARTESIAN_POINT('',(108.604421358487,13.375,25.5));
#100498=CARTESIAN_POINT('Origin',(108.995689360324,14.45,25.5));
#100499=CARTESIAN_POINT('',(108.995689360324,14.45,25.5));
#100500=CARTESIAN_POINT('',(108.995689360324,14.45,25.5));
#100501=CARTESIAN_POINT('',(108.995689360324,14.45,31.5));
#100502=CARTESIAN_POINT('',(108.995689360324,14.45,31.5));
#100503=CARTESIAN_POINT('',(108.995689360324,14.45,25.5));
#100504=CARTESIAN_POINT('Origin',(109.433514312881,14.45,25.5));
#100505=CARTESIAN_POINT('',(109.433514312881,14.45,25.5));
#100506=CARTESIAN_POINT('',(109.433514312881,14.45,25.5));
#100507=CARTESIAN_POINT('',(109.433514312881,14.45,31.5));
#100508=CARTESIAN_POINT('',(109.433514312881,14.45,31.5));
#100509=CARTESIAN_POINT('',(109.433514312881,14.45,25.5));
#100510=CARTESIAN_POINT('Origin',(109.824782314718,13.375,25.5));
#100511=CARTESIAN_POINT('',(109.824782314718,13.375,25.5));
#100512=CARTESIAN_POINT('',(109.824782314718,13.375,25.5));
#100513=CARTESIAN_POINT('',(109.824782314718,13.375,31.5));
#100514=CARTESIAN_POINT('',(109.824782314718,13.375,31.5));
#100515=CARTESIAN_POINT('',(109.824782314718,13.375,25.5));
#100516=CARTESIAN_POINT('Origin',(110.175217685282,13.375,25.5));
#100517=CARTESIAN_POINT('',(110.175217685282,13.375,25.5));
#100518=CARTESIAN_POINT('',(110.175217685282,13.375,25.5));
#100519=CARTESIAN_POINT('',(110.175217685282,13.375,31.5));
#100520=CARTESIAN_POINT('',(110.175217685282,13.375,31.5));
#100521=CARTESIAN_POINT('',(110.175217685282,13.375,25.5));
#100522=CARTESIAN_POINT('Origin',(110.566485687119,14.45,25.5));
#100523=CARTESIAN_POINT('',(110.566485687119,14.45,25.5));
#100524=CARTESIAN_POINT('',(110.566485687119,14.45,25.5));
#100525=CARTESIAN_POINT('',(110.566485687119,14.45,31.5));
#100526=CARTESIAN_POINT('',(110.566485687119,14.45,31.5));
#100527=CARTESIAN_POINT('',(110.566485687119,14.45,25.5));
#100528=CARTESIAN_POINT('Origin',(111.004310639676,14.45,25.5));
#100529=CARTESIAN_POINT('',(111.004310639676,14.45,25.5));
#100530=CARTESIAN_POINT('',(111.004310639676,14.45,25.5));
#100531=CARTESIAN_POINT('',(111.004310639676,14.45,31.5));
#100532=CARTESIAN_POINT('',(111.004310639676,14.45,31.5));
#100533=CARTESIAN_POINT('',(111.004310639676,14.45,25.5));
#100534=CARTESIAN_POINT('Origin',(111.395578641513,13.375,25.5));
#100535=CARTESIAN_POINT('',(111.395578641513,13.375,25.5));
#100536=CARTESIAN_POINT('',(111.395578641513,13.375,25.5));
#100537=CARTESIAN_POINT('',(111.395578641513,13.375,31.5));
#100538=CARTESIAN_POINT('',(111.395578641513,13.375,31.5));
#100539=CARTESIAN_POINT('',(111.395578641513,13.375,25.5));
#100540=CARTESIAN_POINT('Origin',(111.746014012077,13.375,25.5));
#100541=CARTESIAN_POINT('',(111.746014012077,13.375,25.5));
#100542=CARTESIAN_POINT('',(111.746014012077,13.375,25.5));
#100543=CARTESIAN_POINT('',(111.746014012077,13.375,31.5));
#100544=CARTESIAN_POINT('',(111.746014012077,13.375,31.5));
#100545=CARTESIAN_POINT('',(111.746014012077,13.375,25.5));
#100546=CARTESIAN_POINT('Origin',(112.137282013913,14.45,25.5));
#100547=CARTESIAN_POINT('',(112.137282013913,14.45,25.5));
#100548=CARTESIAN_POINT('',(112.137282013913,14.45,25.5));
#100549=CARTESIAN_POINT('',(112.137282013913,14.45,31.5));
#100550=CARTESIAN_POINT('',(112.137282013913,14.45,31.5));
#100551=CARTESIAN_POINT('',(112.137282013913,14.45,25.5));
#100552=CARTESIAN_POINT('Origin',(112.575106966471,14.45,25.5));
#100553=CARTESIAN_POINT('',(112.575106966471,14.45,25.5));
#100554=CARTESIAN_POINT('',(112.575106966471,14.45,25.5));
#100555=CARTESIAN_POINT('',(112.575106966471,14.45,31.5));
#100556=CARTESIAN_POINT('',(112.575106966471,14.45,31.5));
#100557=CARTESIAN_POINT('',(112.575106966471,14.45,25.5));
#100558=CARTESIAN_POINT('Origin',(112.966374968307,13.375,25.5));
#100559=CARTESIAN_POINT('',(112.966374968307,13.375,25.5));
#100560=CARTESIAN_POINT('',(112.966374968307,13.375,25.5));
#100561=CARTESIAN_POINT('',(112.966374968307,13.375,31.5));
#100562=CARTESIAN_POINT('',(112.966374968307,13.375,31.5));
#100563=CARTESIAN_POINT('',(112.966374968307,13.375,25.5));
#100564=CARTESIAN_POINT('Origin',(113.316810338872,13.375,25.5));
#100565=CARTESIAN_POINT('',(113.316810338872,13.375,25.5));
#100566=CARTESIAN_POINT('',(113.316810338872,13.375,25.5));
#100567=CARTESIAN_POINT('',(113.316810338872,13.375,31.5));
#100568=CARTESIAN_POINT('',(113.316810338872,13.375,31.5));
#100569=CARTESIAN_POINT('',(113.316810338872,13.375,25.5));
#100570=CARTESIAN_POINT('Origin',(113.708078340708,14.45,25.5));
#100571=CARTESIAN_POINT('',(113.708078340708,14.45,25.5));
#100572=CARTESIAN_POINT('',(113.708078340708,14.45,25.5));
#100573=CARTESIAN_POINT('',(113.708078340708,14.45,31.5));
#100574=CARTESIAN_POINT('',(113.708078340708,14.45,31.5));
#100575=CARTESIAN_POINT('',(113.708078340708,14.45,25.5));
#100576=CARTESIAN_POINT('Origin',(114.145903293266,14.45,25.5));
#100577=CARTESIAN_POINT('',(114.145903293266,14.45,25.5));
#100578=CARTESIAN_POINT('',(114.145903293266,14.45,25.5));
#100579=CARTESIAN_POINT('',(114.145903293266,14.45,31.5));
#100580=CARTESIAN_POINT('',(114.145903293266,14.45,31.5));
#100581=CARTESIAN_POINT('',(114.145903293266,14.45,25.5));
#100582=CARTESIAN_POINT('Origin',(114.537171295102,13.375,25.5));
#100583=CARTESIAN_POINT('',(114.537171295102,13.375,25.5));
#100584=CARTESIAN_POINT('',(114.537171295102,13.375,25.5));
#100585=CARTESIAN_POINT('',(114.537171295102,13.375,31.5));
#100586=CARTESIAN_POINT('',(114.537171295102,13.375,31.5));
#100587=CARTESIAN_POINT('',(114.537171295102,13.375,25.5));
#100588=CARTESIAN_POINT('Origin',(114.887606665667,13.375,25.5));
#100589=CARTESIAN_POINT('',(114.887606665667,13.375,25.5));
#100590=CARTESIAN_POINT('',(114.887606665667,13.375,25.5));
#100591=CARTESIAN_POINT('',(114.887606665667,13.375,31.5));
#100592=CARTESIAN_POINT('',(114.887606665667,13.375,31.5));
#100593=CARTESIAN_POINT('',(114.887606665667,13.375,25.5));
#100594=CARTESIAN_POINT('Origin',(115.278874667503,14.45,25.5));
#100595=CARTESIAN_POINT('',(115.278874667503,14.45,25.5));
#100596=CARTESIAN_POINT('',(115.278874667503,14.45,25.5));
#100597=CARTESIAN_POINT('',(115.278874667503,14.45,31.5));
#100598=CARTESIAN_POINT('',(115.278874667503,14.45,31.5));
#100599=CARTESIAN_POINT('',(115.278874667503,14.45,25.5));
#100600=CARTESIAN_POINT('Origin',(115.716699620061,14.45,25.5));
#100601=CARTESIAN_POINT('',(115.716699620061,14.45,25.5));
#100602=CARTESIAN_POINT('',(115.716699620061,14.45,25.5));
#100603=CARTESIAN_POINT('',(115.716699620061,14.45,31.5));
#100604=CARTESIAN_POINT('',(115.716699620061,14.45,31.5));
#100605=CARTESIAN_POINT('',(115.716699620061,14.45,25.5));
#100606=CARTESIAN_POINT('Origin',(116.107967621897,13.375,25.5));
#100607=CARTESIAN_POINT('',(116.107967621897,13.375,25.5));
#100608=CARTESIAN_POINT('',(116.107967621897,13.375,25.5));
#100609=CARTESIAN_POINT('',(116.107967621897,13.375,31.5));
#100610=CARTESIAN_POINT('',(116.107967621897,13.375,31.5));
#100611=CARTESIAN_POINT('',(116.107967621897,13.375,25.5));
#100612=CARTESIAN_POINT('Origin',(116.458402992462,13.375,25.5));
#100613=CARTESIAN_POINT('',(116.458402992462,13.375,25.5));
#100614=CARTESIAN_POINT('',(116.458402992462,13.375,25.5));
#100615=CARTESIAN_POINT('',(116.458402992462,13.375,31.5));
#100616=CARTESIAN_POINT('',(116.458402992462,13.375,31.5));
#100617=CARTESIAN_POINT('',(116.458402992462,13.375,25.5));
#100618=CARTESIAN_POINT('Origin',(116.849670994298,14.45,25.5));
#100619=CARTESIAN_POINT('',(116.849670994298,14.45,25.5));
#100620=CARTESIAN_POINT('',(116.849670994298,14.45,25.5));
#100621=CARTESIAN_POINT('',(116.849670994298,14.45,31.5));
#100622=CARTESIAN_POINT('',(116.849670994298,14.45,31.5));
#100623=CARTESIAN_POINT('',(116.849670994298,14.45,25.5));
#100624=CARTESIAN_POINT('Origin',(117.287495946856,14.45,25.5));
#100625=CARTESIAN_POINT('',(117.287495946856,14.45,25.5));
#100626=CARTESIAN_POINT('',(117.287495946856,14.45,25.5));
#100627=CARTESIAN_POINT('',(117.287495946856,14.45,31.5));
#100628=CARTESIAN_POINT('',(117.287495946856,14.45,31.5));
#100629=CARTESIAN_POINT('',(117.287495946856,14.45,25.5));
#100630=CARTESIAN_POINT('Origin',(117.678763948692,13.375,25.5));
#100631=CARTESIAN_POINT('',(117.678763948692,13.375,25.5));
#100632=CARTESIAN_POINT('',(117.678763948692,13.375,25.5));
#100633=CARTESIAN_POINT('',(117.678763948692,13.375,31.5));
#100634=CARTESIAN_POINT('',(117.678763948692,13.375,31.5));
#100635=CARTESIAN_POINT('',(117.678763948692,13.375,25.5));
#100636=CARTESIAN_POINT('Origin',(118.029199319257,13.375,25.5));
#100637=CARTESIAN_POINT('',(118.029199319257,13.375,25.5));
#100638=CARTESIAN_POINT('',(118.029199319257,13.375,25.5));
#100639=CARTESIAN_POINT('',(118.029199319257,13.375,31.5));
#100640=CARTESIAN_POINT('',(118.029199319257,13.375,31.5));
#100641=CARTESIAN_POINT('',(118.029199319257,13.375,25.5));
#100642=CARTESIAN_POINT('Origin',(118.420467321093,14.45,25.5));
#100643=CARTESIAN_POINT('',(118.420467321093,14.45,25.5));
#100644=CARTESIAN_POINT('',(118.420467321093,14.45,25.5));
#100645=CARTESIAN_POINT('',(118.420467321093,14.45,31.5));
#100646=CARTESIAN_POINT('',(118.420467321093,14.45,31.5));
#100647=CARTESIAN_POINT('',(118.420467321093,14.45,25.5));
#100648=CARTESIAN_POINT('Origin',(118.858292273651,14.45,25.5));
#100649=CARTESIAN_POINT('',(118.858292273651,14.45,25.5));
#100650=CARTESIAN_POINT('',(118.858292273651,14.45,25.5));
#100651=CARTESIAN_POINT('',(118.858292273651,14.45,31.5));
#100652=CARTESIAN_POINT('',(118.858292273651,14.45,31.5));
#100653=CARTESIAN_POINT('',(118.858292273651,14.45,25.5));
#100654=CARTESIAN_POINT('Origin',(119.249560275487,13.375,25.5));
#100655=CARTESIAN_POINT('',(119.249560275487,13.375,25.5));
#100656=CARTESIAN_POINT('',(119.249560275487,13.375,25.5));
#100657=CARTESIAN_POINT('',(119.249560275487,13.375,31.5));
#100658=CARTESIAN_POINT('',(119.249560275487,13.375,31.5));
#100659=CARTESIAN_POINT('',(119.249560275487,13.375,25.5));
#100660=CARTESIAN_POINT('Origin',(119.599995646052,13.375,25.5));
#100661=CARTESIAN_POINT('',(119.599995646052,13.375,25.5));
#100662=CARTESIAN_POINT('',(119.599995646052,13.375,25.5));
#100663=CARTESIAN_POINT('',(119.599995646052,13.375,31.5));
#100664=CARTESIAN_POINT('',(119.599995646052,13.375,31.5));
#100665=CARTESIAN_POINT('',(119.599995646052,13.375,25.5));
#100666=CARTESIAN_POINT('Origin',(119.991263647888,14.45,25.5));
#100667=CARTESIAN_POINT('',(119.991263647888,14.45,25.5));
#100668=CARTESIAN_POINT('',(119.991263647888,14.45,25.5));
#100669=CARTESIAN_POINT('',(119.991263647888,14.45,31.5));
#100670=CARTESIAN_POINT('',(119.991263647888,14.45,31.5));
#100671=CARTESIAN_POINT('',(119.991263647888,14.45,25.5));
#100672=CARTESIAN_POINT('Origin',(120.429088600446,14.45,25.5));
#100673=CARTESIAN_POINT('',(120.429088600446,14.45,25.5));
#100674=CARTESIAN_POINT('',(120.429088600446,14.45,25.5));
#100675=CARTESIAN_POINT('',(120.429088600446,14.45,31.5));
#100676=CARTESIAN_POINT('',(120.429088600446,14.45,31.5));
#100677=CARTESIAN_POINT('',(120.429088600446,14.45,25.5));
#100678=CARTESIAN_POINT('Origin',(120.820356602282,13.375,25.5));
#100679=CARTESIAN_POINT('',(120.820356602282,13.375,25.5));
#100680=CARTESIAN_POINT('',(120.820356602282,13.375,25.5));
#100681=CARTESIAN_POINT('',(120.820356602282,13.375,31.5));
#100682=CARTESIAN_POINT('',(120.820356602282,13.375,31.5));
#100683=CARTESIAN_POINT('',(120.820356602282,13.375,25.5));
#100684=CARTESIAN_POINT('Origin',(121.170791972847,13.375,25.5));
#100685=CARTESIAN_POINT('',(121.170791972847,13.375,25.5));
#100686=CARTESIAN_POINT('',(121.170791972847,13.375,25.5));
#100687=CARTESIAN_POINT('',(121.170791972847,13.375,31.5));
#100688=CARTESIAN_POINT('',(121.170791972847,13.375,31.5));
#100689=CARTESIAN_POINT('',(121.170791972847,13.375,25.5));
#100690=CARTESIAN_POINT('Origin',(121.562059974683,14.45,25.5));
#100691=CARTESIAN_POINT('',(121.562059974683,14.45,25.5));
#100692=CARTESIAN_POINT('',(121.562059974683,14.45,25.5));
#100693=CARTESIAN_POINT('',(121.562059974683,14.45,31.5));
#100694=CARTESIAN_POINT('',(121.562059974683,14.45,31.5));
#100695=CARTESIAN_POINT('',(121.562059974683,14.45,25.5));
#100696=CARTESIAN_POINT('Origin',(121.999884927241,14.45,25.5));
#100697=CARTESIAN_POINT('',(121.999884927241,14.45,25.5));
#100698=CARTESIAN_POINT('',(121.999884927241,14.45,25.5));
#100699=CARTESIAN_POINT('',(121.999884927241,14.45,31.5));
#100700=CARTESIAN_POINT('',(121.999884927241,14.45,31.5));
#100701=CARTESIAN_POINT('',(121.999884927241,14.45,25.5));
#100702=CARTESIAN_POINT('Origin',(122.391152929077,13.375,25.5));
#100703=CARTESIAN_POINT('',(122.391152929077,13.375,25.5));
#100704=CARTESIAN_POINT('',(122.391152929077,13.375,25.5));
#100705=CARTESIAN_POINT('',(122.391152929077,13.375,31.5));
#100706=CARTESIAN_POINT('',(122.391152929077,13.375,31.5));
#100707=CARTESIAN_POINT('',(122.391152929077,13.375,25.5));
#100708=CARTESIAN_POINT('Origin',(122.741588299642,13.375,25.5));
#100709=CARTESIAN_POINT('',(122.741588299642,13.375,25.5));
#100710=CARTESIAN_POINT('',(122.741588299642,13.375,25.5));
#100711=CARTESIAN_POINT('',(122.741588299642,13.375,31.5));
#100712=CARTESIAN_POINT('',(122.741588299642,13.375,31.5));
#100713=CARTESIAN_POINT('',(122.741588299642,13.375,25.5));
#100714=CARTESIAN_POINT('Origin',(123.132856301478,14.45,25.5));
#100715=CARTESIAN_POINT('',(123.132856301478,14.45,25.5));
#100716=CARTESIAN_POINT('',(123.132856301478,14.45,25.5));
#100717=CARTESIAN_POINT('',(123.132856301478,14.45,31.5));
#100718=CARTESIAN_POINT('',(123.132856301478,14.45,31.5));
#100719=CARTESIAN_POINT('',(123.132856301478,14.45,25.5));
#100720=CARTESIAN_POINT('Origin',(123.570681254036,14.45,25.5));
#100721=CARTESIAN_POINT('',(123.570681254036,14.45,25.5));
#100722=CARTESIAN_POINT('',(123.570681254036,14.45,25.5));
#100723=CARTESIAN_POINT('',(123.570681254036,14.45,31.5));
#100724=CARTESIAN_POINT('',(123.570681254036,14.45,31.5));
#100725=CARTESIAN_POINT('',(123.570681254036,14.45,25.5));
#100726=CARTESIAN_POINT('Origin',(123.961949255872,13.375,25.5));
#100727=CARTESIAN_POINT('',(123.961949255872,13.375,25.5));
#100728=CARTESIAN_POINT('',(123.961949255872,13.375,25.5));
#100729=CARTESIAN_POINT('',(123.961949255872,13.375,31.5));
#100730=CARTESIAN_POINT('',(123.961949255872,13.375,31.5));
#100731=CARTESIAN_POINT('',(123.961949255872,13.375,25.5));
#100732=CARTESIAN_POINT('Origin',(124.312384626436,13.375,25.5));
#100733=CARTESIAN_POINT('',(124.312384626436,13.375,25.5));
#100734=CARTESIAN_POINT('',(124.312384626436,13.375,25.5));
#100735=CARTESIAN_POINT('',(124.312384626436,13.375,31.5));
#100736=CARTESIAN_POINT('',(124.312384626436,13.375,31.5));
#100737=CARTESIAN_POINT('',(124.312384626436,13.375,25.5));
#100738=CARTESIAN_POINT('Origin',(124.703652628273,14.45,25.5));
#100739=CARTESIAN_POINT('',(124.703652628273,14.45,25.5));
#100740=CARTESIAN_POINT('',(124.703652628273,14.45,25.5));
#100741=CARTESIAN_POINT('',(124.703652628273,14.45,31.5));
#100742=CARTESIAN_POINT('',(124.703652628273,14.45,31.5));
#100743=CARTESIAN_POINT('',(124.703652628273,14.45,25.5));
#100744=CARTESIAN_POINT('Origin',(125.14147758083,14.45,25.5));
#100745=CARTESIAN_POINT('',(125.14147758083,14.45,25.5));
#100746=CARTESIAN_POINT('',(125.14147758083,14.45,25.5));
#100747=CARTESIAN_POINT('',(125.14147758083,14.45,31.5));
#100748=CARTESIAN_POINT('',(125.14147758083,14.45,31.5));
#100749=CARTESIAN_POINT('',(125.14147758083,14.45,25.5));
#100750=CARTESIAN_POINT('Origin',(125.532745582667,13.375,25.5));
#100751=CARTESIAN_POINT('',(125.532745582667,13.375,25.5));
#100752=CARTESIAN_POINT('',(125.532745582667,13.375,25.5));
#100753=CARTESIAN_POINT('',(125.532745582667,13.375,31.5));
#100754=CARTESIAN_POINT('',(125.532745582667,13.375,31.5));
#100755=CARTESIAN_POINT('',(125.532745582667,13.375,25.5));
#100756=CARTESIAN_POINT('Origin',(125.883180953231,13.375,25.5));
#100757=CARTESIAN_POINT('',(125.883180953231,13.375,25.5));
#100758=CARTESIAN_POINT('',(125.883180953231,13.375,25.5));
#100759=CARTESIAN_POINT('',(125.883180953231,13.375,31.5));
#100760=CARTESIAN_POINT('',(125.883180953231,13.375,31.5));
#100761=CARTESIAN_POINT('',(125.883180953231,13.375,25.5));
#100762=CARTESIAN_POINT('Origin',(126.274448955067,14.45,25.5));
#100763=CARTESIAN_POINT('',(126.274448955067,14.45,25.5));
#100764=CARTESIAN_POINT('',(126.274448955067,14.45,25.5));
#100765=CARTESIAN_POINT('',(126.274448955067,14.45,31.5));
#100766=CARTESIAN_POINT('',(126.274448955067,14.45,31.5));
#100767=CARTESIAN_POINT('',(126.274448955067,14.45,25.5));
#100768=CARTESIAN_POINT('Origin',(126.712273907625,14.45,25.5));
#100769=CARTESIAN_POINT('',(126.712273907625,14.45,25.5));
#100770=CARTESIAN_POINT('',(126.712273907625,14.45,25.5));
#100771=CARTESIAN_POINT('',(126.712273907625,14.45,31.5));
#100772=CARTESIAN_POINT('',(126.712273907625,14.45,31.5));
#100773=CARTESIAN_POINT('',(126.712273907625,14.45,25.5));
#100774=CARTESIAN_POINT('Origin',(127.103541909462,13.375,25.5));
#100775=CARTESIAN_POINT('',(127.103541909462,13.375,25.5));
#100776=CARTESIAN_POINT('',(127.103541909462,13.375,25.5));
#100777=CARTESIAN_POINT('',(127.103541909462,13.375,31.5));
#100778=CARTESIAN_POINT('',(127.103541909462,13.375,31.5));
#100779=CARTESIAN_POINT('',(127.103541909462,13.375,25.5));
#100780=CARTESIAN_POINT('Origin',(127.453977280026,13.375,25.5));
#100781=CARTESIAN_POINT('',(127.453977280026,13.375,25.5));
#100782=CARTESIAN_POINT('',(127.453977280026,13.375,25.5));
#100783=CARTESIAN_POINT('',(127.453977280026,13.375,31.5));
#100784=CARTESIAN_POINT('',(127.453977280026,13.375,31.5));
#100785=CARTESIAN_POINT('',(127.453977280026,13.375,25.5));
#100786=CARTESIAN_POINT('Origin',(127.845245281862,14.45,25.5));
#100787=CARTESIAN_POINT('',(127.845245281862,14.45,25.5));
#100788=CARTESIAN_POINT('',(127.845245281862,14.45,25.5));
#100789=CARTESIAN_POINT('',(127.845245281862,14.45,31.5));
#100790=CARTESIAN_POINT('',(127.845245281862,14.45,31.5));
#100791=CARTESIAN_POINT('',(127.845245281862,14.45,25.5));
#100792=CARTESIAN_POINT('Origin',(128.28307023442,14.45,25.5));
#100793=CARTESIAN_POINT('',(128.28307023442,14.45,25.5));
#100794=CARTESIAN_POINT('',(128.28307023442,14.45,25.5));
#100795=CARTESIAN_POINT('',(128.28307023442,14.45,31.5));
#100796=CARTESIAN_POINT('',(128.28307023442,14.45,31.5));
#100797=CARTESIAN_POINT('',(128.28307023442,14.45,25.5));
#100798=CARTESIAN_POINT('Origin',(128.674338236256,13.375,25.5));
#100799=CARTESIAN_POINT('',(128.674338236256,13.375,25.5));
#100800=CARTESIAN_POINT('',(128.674338236256,13.375,25.5));
#100801=CARTESIAN_POINT('',(128.674338236256,13.375,31.5));
#100802=CARTESIAN_POINT('',(128.674338236256,13.375,31.5));
#100803=CARTESIAN_POINT('',(128.674338236256,13.375,25.5));
#100804=CARTESIAN_POINT('Origin',(129.024773606821,13.375,25.5));
#100805=CARTESIAN_POINT('',(129.024773606821,13.375,25.5));
#100806=CARTESIAN_POINT('',(129.024773606821,13.375,25.5));
#100807=CARTESIAN_POINT('',(129.024773606821,13.375,31.5));
#100808=CARTESIAN_POINT('',(129.024773606821,13.375,31.5));
#100809=CARTESIAN_POINT('',(129.024773606821,13.375,25.5));
#100810=CARTESIAN_POINT('Origin',(129.416041608657,14.45,25.5));
#100811=CARTESIAN_POINT('',(129.416041608657,14.45,25.5));
#100812=CARTESIAN_POINT('',(129.416041608657,14.45,25.5));
#100813=CARTESIAN_POINT('',(129.416041608657,14.45,31.5));
#100814=CARTESIAN_POINT('',(129.416041608657,14.45,31.5));
#100815=CARTESIAN_POINT('',(129.416041608657,14.45,25.5));
#100816=CARTESIAN_POINT('Origin',(129.853866561215,14.45,25.5));
#100817=CARTESIAN_POINT('',(129.853866561215,14.45,25.5));
#100818=CARTESIAN_POINT('',(129.853866561215,14.45,25.5));
#100819=CARTESIAN_POINT('',(129.853866561215,14.45,31.5));
#100820=CARTESIAN_POINT('',(129.853866561215,14.45,31.5));
#100821=CARTESIAN_POINT('',(129.853866561215,14.45,25.5));
#100822=CARTESIAN_POINT('Origin',(130.245134563051,13.375,25.5));
#100823=CARTESIAN_POINT('',(130.245134563051,13.375,25.5));
#100824=CARTESIAN_POINT('',(130.245134563051,13.375,25.5));
#100825=CARTESIAN_POINT('',(130.245134563051,13.375,31.5));
#100826=CARTESIAN_POINT('',(130.245134563051,13.375,31.5));
#100827=CARTESIAN_POINT('',(130.245134563051,13.375,25.5));
#100828=CARTESIAN_POINT('Origin',(130.595569933616,13.375,25.5));
#100829=CARTESIAN_POINT('',(130.595569933616,13.375,25.5));
#100830=CARTESIAN_POINT('',(130.595569933616,13.375,25.5));
#100831=CARTESIAN_POINT('',(130.595569933616,13.375,31.5));
#100832=CARTESIAN_POINT('',(130.595569933616,13.375,31.5));
#100833=CARTESIAN_POINT('',(130.595569933616,13.375,25.5));
#100834=CARTESIAN_POINT('Origin',(130.986837935452,14.45,25.5));
#100835=CARTESIAN_POINT('',(130.986837935452,14.45,25.5));
#100836=CARTESIAN_POINT('',(130.986837935452,14.45,25.5));
#100837=CARTESIAN_POINT('',(130.986837935452,14.45,31.5));
#100838=CARTESIAN_POINT('',(130.986837935452,14.45,31.5));
#100839=CARTESIAN_POINT('',(130.986837935452,14.45,25.5));
#100840=CARTESIAN_POINT('Origin',(131.42466288801,14.45,25.5));
#100841=CARTESIAN_POINT('',(131.42466288801,14.45,25.5));
#100842=CARTESIAN_POINT('',(131.42466288801,14.45,25.5));
#100843=CARTESIAN_POINT('',(131.42466288801,14.45,31.5));
#100844=CARTESIAN_POINT('',(131.42466288801,14.45,31.5));
#100845=CARTESIAN_POINT('',(131.42466288801,14.45,25.5));
#100846=CARTESIAN_POINT('Origin',(131.815930889846,13.375,25.5));
#100847=CARTESIAN_POINT('',(131.815930889846,13.375,25.5));
#100848=CARTESIAN_POINT('',(131.815930889846,13.375,25.5));
#100849=CARTESIAN_POINT('',(131.815930889846,13.375,31.5));
#100850=CARTESIAN_POINT('',(131.815930889846,13.375,31.5));
#100851=CARTESIAN_POINT('',(131.815930889846,13.375,25.5));
#100852=CARTESIAN_POINT('Origin',(132.166366260411,13.375,25.5));
#100853=CARTESIAN_POINT('',(132.166366260411,13.375,25.5));
#100854=CARTESIAN_POINT('',(132.166366260411,13.375,25.5));
#100855=CARTESIAN_POINT('',(132.166366260411,13.375,31.5));
#100856=CARTESIAN_POINT('',(132.166366260411,13.375,31.5));
#100857=CARTESIAN_POINT('',(132.166366260411,13.375,25.5));
#100858=CARTESIAN_POINT('Origin',(132.557634262247,14.45,25.5));
#100859=CARTESIAN_POINT('',(132.557634262247,14.45,25.5));
#100860=CARTESIAN_POINT('',(132.557634262247,14.45,25.5));
#100861=CARTESIAN_POINT('',(132.557634262247,14.45,31.5));
#100862=CARTESIAN_POINT('',(132.557634262247,14.45,31.5));
#100863=CARTESIAN_POINT('',(132.557634262247,14.45,25.5));
#100864=CARTESIAN_POINT('Origin',(132.995459214805,14.45,25.5));
#100865=CARTESIAN_POINT('',(132.995459214805,14.45,25.5));
#100866=CARTESIAN_POINT('',(132.995459214805,14.45,25.5));
#100867=CARTESIAN_POINT('',(132.995459214805,14.45,31.5));
#100868=CARTESIAN_POINT('',(132.995459214805,14.45,31.5));
#100869=CARTESIAN_POINT('',(132.995459214805,14.45,25.5));
#100870=CARTESIAN_POINT('Origin',(133.386727216641,13.375,25.5));
#100871=CARTESIAN_POINT('',(133.386727216641,13.375,25.5));
#100872=CARTESIAN_POINT('',(133.386727216641,13.375,25.5));
#100873=CARTESIAN_POINT('',(133.386727216641,13.375,31.5));
#100874=CARTESIAN_POINT('',(133.386727216641,13.375,31.5));
#100875=CARTESIAN_POINT('',(133.386727216641,13.375,25.5));
#100876=CARTESIAN_POINT('Origin',(133.737162587206,13.375,25.5));
#100877=CARTESIAN_POINT('',(133.737162587206,13.375,25.5));
#100878=CARTESIAN_POINT('',(133.737162587206,13.375,25.5));
#100879=CARTESIAN_POINT('',(133.737162587206,13.375,31.5));
#100880=CARTESIAN_POINT('',(133.737162587206,13.375,31.5));
#100881=CARTESIAN_POINT('',(133.737162587206,13.375,25.5));
#100882=CARTESIAN_POINT('Origin',(134.128430589042,14.45,25.5));
#100883=CARTESIAN_POINT('',(134.128430589042,14.45,25.5));
#100884=CARTESIAN_POINT('',(134.128430589042,14.45,25.5));
#100885=CARTESIAN_POINT('',(134.128430589042,14.45,31.5));
#100886=CARTESIAN_POINT('',(134.128430589042,14.45,31.5));
#100887=CARTESIAN_POINT('',(134.128430589042,14.45,25.5));
#100888=CARTESIAN_POINT('Origin',(134.5662555416,14.45,25.5));
#100889=CARTESIAN_POINT('',(134.5662555416,14.45,25.5));
#100890=CARTESIAN_POINT('',(134.5662555416,14.45,25.5));
#100891=CARTESIAN_POINT('',(134.5662555416,14.45,31.5));
#100892=CARTESIAN_POINT('',(134.5662555416,14.45,31.5));
#100893=CARTESIAN_POINT('',(134.5662555416,14.45,25.5));
#100894=CARTESIAN_POINT('Origin',(134.957523543436,13.375,25.5));
#100895=CARTESIAN_POINT('',(134.957523543436,13.375,25.5));
#100896=CARTESIAN_POINT('',(134.957523543436,13.375,25.5));
#100897=CARTESIAN_POINT('',(134.957523543436,13.375,31.5));
#100898=CARTESIAN_POINT('',(134.957523543436,13.375,31.5));
#100899=CARTESIAN_POINT('',(134.957523543436,13.375,25.5));
#100900=CARTESIAN_POINT('Origin',(135.307958914001,13.375,25.5));
#100901=CARTESIAN_POINT('',(135.307958914001,13.375,25.5));
#100902=CARTESIAN_POINT('',(135.307958914001,13.375,25.5));
#100903=CARTESIAN_POINT('',(135.307958914001,13.375,31.5));
#100904=CARTESIAN_POINT('',(135.307958914001,13.375,31.5));
#100905=CARTESIAN_POINT('',(135.307958914001,13.375,25.5));
#100906=CARTESIAN_POINT('Origin',(135.699226915837,14.45,25.5));
#100907=CARTESIAN_POINT('',(135.699226915837,14.45,25.5));
#100908=CARTESIAN_POINT('',(135.699226915837,14.45,25.5));
#100909=CARTESIAN_POINT('',(135.699226915837,14.45,31.5));
#100910=CARTESIAN_POINT('',(135.699226915837,14.45,31.5));
#100911=CARTESIAN_POINT('',(135.699226915837,14.45,25.5));
#100912=CARTESIAN_POINT('Origin',(136.137051868395,14.45,25.5));
#100913=CARTESIAN_POINT('',(136.137051868395,14.45,25.5));
#100914=CARTESIAN_POINT('',(136.137051868395,14.45,25.5));
#100915=CARTESIAN_POINT('',(136.137051868395,14.45,31.5));
#100916=CARTESIAN_POINT('',(136.137051868395,14.45,31.5));
#100917=CARTESIAN_POINT('',(136.137051868395,14.45,25.5));
#100918=CARTESIAN_POINT('Origin',(136.528319870231,13.375,25.5));
#100919=CARTESIAN_POINT('',(136.528319870231,13.375,25.5));
#100920=CARTESIAN_POINT('',(136.528319870231,13.375,25.5));
#100921=CARTESIAN_POINT('',(136.528319870231,13.375,31.5));
#100922=CARTESIAN_POINT('',(136.528319870231,13.375,31.5));
#100923=CARTESIAN_POINT('',(136.528319870231,13.375,25.5));
#100924=CARTESIAN_POINT('Origin',(136.878755240796,13.375,25.5));
#100925=CARTESIAN_POINT('',(136.878755240796,13.375,25.5));
#100926=CARTESIAN_POINT('',(136.878755240796,13.375,25.5));
#100927=CARTESIAN_POINT('',(136.878755240796,13.375,31.5));
#100928=CARTESIAN_POINT('',(136.878755240796,13.375,31.5));
#100929=CARTESIAN_POINT('',(136.878755240796,13.375,25.5));
#100930=CARTESIAN_POINT('Origin',(137.270023242632,14.45,25.5));
#100931=CARTESIAN_POINT('',(137.270023242632,14.45,25.5));
#100932=CARTESIAN_POINT('',(137.270023242632,14.45,25.5));
#100933=CARTESIAN_POINT('',(137.270023242632,14.45,31.5));
#100934=CARTESIAN_POINT('',(137.270023242632,14.45,31.5));
#100935=CARTESIAN_POINT('',(137.270023242632,14.45,25.5));
#100936=CARTESIAN_POINT('Origin',(137.70784819519,14.45,25.5));
#100937=CARTESIAN_POINT('',(137.70784819519,14.45,25.5));
#100938=CARTESIAN_POINT('',(137.70784819519,14.45,25.5));
#100939=CARTESIAN_POINT('',(137.70784819519,14.45,31.5));
#100940=CARTESIAN_POINT('',(137.70784819519,14.45,31.5));
#100941=CARTESIAN_POINT('',(137.70784819519,14.45,25.5));
#100942=CARTESIAN_POINT('Origin',(138.099116197026,13.375,25.5));
#100943=CARTESIAN_POINT('',(138.099116197026,13.375,25.5));
#100944=CARTESIAN_POINT('',(138.099116197026,13.375,25.5));
#100945=CARTESIAN_POINT('',(138.099116197026,13.375,31.5));
#100946=CARTESIAN_POINT('',(138.099116197026,13.375,31.5));
#100947=CARTESIAN_POINT('',(138.099116197026,13.375,25.5));
#100948=CARTESIAN_POINT('Origin',(138.44955156759,13.375,25.5));
#100949=CARTESIAN_POINT('',(138.44955156759,13.375,25.5));
#100950=CARTESIAN_POINT('',(138.44955156759,13.375,25.5));
#100951=CARTESIAN_POINT('',(138.44955156759,13.375,31.5));
#100952=CARTESIAN_POINT('',(138.44955156759,13.375,31.5));
#100953=CARTESIAN_POINT('',(138.44955156759,13.375,25.5));
#100954=CARTESIAN_POINT('Origin',(138.840819569427,14.45,25.5));
#100955=CARTESIAN_POINT('',(138.840819569427,14.45,25.5));
#100956=CARTESIAN_POINT('',(138.840819569427,14.45,25.5));
#100957=CARTESIAN_POINT('',(138.840819569427,14.45,31.5));
#100958=CARTESIAN_POINT('',(138.840819569427,14.45,31.5));
#100959=CARTESIAN_POINT('',(138.840819569427,14.45,25.5));
#100960=CARTESIAN_POINT('Origin',(139.278644521985,14.45,25.5));
#100961=CARTESIAN_POINT('',(139.278644521985,14.45,25.5));
#100962=CARTESIAN_POINT('',(139.278644521985,14.45,25.5));
#100963=CARTESIAN_POINT('',(139.278644521985,14.45,31.5));
#100964=CARTESIAN_POINT('',(139.278644521985,14.45,31.5));
#100965=CARTESIAN_POINT('',(139.278644521985,14.45,25.5));
#100966=CARTESIAN_POINT('Origin',(139.669912523821,13.375,25.5));
#100967=CARTESIAN_POINT('',(139.669912523821,13.375,25.5));
#100968=CARTESIAN_POINT('',(139.669912523821,13.375,25.5));
#100969=CARTESIAN_POINT('',(139.669912523821,13.375,31.5));
#100970=CARTESIAN_POINT('',(139.669912523821,13.375,31.5));
#100971=CARTESIAN_POINT('',(139.669912523821,13.375,25.5));
#100972=CARTESIAN_POINT('Origin',(140.020347894385,13.375,25.5));
#100973=CARTESIAN_POINT('',(140.020347894385,13.375,25.5));
#100974=CARTESIAN_POINT('',(140.020347894385,13.375,25.5));
#100975=CARTESIAN_POINT('',(140.020347894385,13.375,31.5));
#100976=CARTESIAN_POINT('',(140.020347894385,13.375,31.5));
#100977=CARTESIAN_POINT('',(140.020347894385,13.375,25.5));
#100978=CARTESIAN_POINT('Origin',(140.411615896222,14.45,25.5));
#100979=CARTESIAN_POINT('',(140.411615896222,14.45,25.5));
#100980=CARTESIAN_POINT('',(140.411615896222,14.45,25.5));
#100981=CARTESIAN_POINT('',(140.411615896222,14.45,31.5));
#100982=CARTESIAN_POINT('',(140.411615896222,14.45,31.5));
#100983=CARTESIAN_POINT('',(140.411615896222,14.45,25.5));
#100984=CARTESIAN_POINT('Origin',(140.849440848779,14.45,25.5));
#100985=CARTESIAN_POINT('',(140.849440848779,14.45,25.5));
#100986=CARTESIAN_POINT('',(140.849440848779,14.45,25.5));
#100987=CARTESIAN_POINT('',(140.849440848779,14.45,31.5));
#100988=CARTESIAN_POINT('',(140.849440848779,14.45,31.5));
#100989=CARTESIAN_POINT('',(140.849440848779,14.45,25.5));
#100990=CARTESIAN_POINT('Origin',(141.240708850616,13.375,25.5));
#100991=CARTESIAN_POINT('',(141.240708850616,13.375,25.5));
#100992=CARTESIAN_POINT('',(141.240708850616,13.375,25.5));
#100993=CARTESIAN_POINT('',(141.240708850616,13.375,31.5));
#100994=CARTESIAN_POINT('',(141.240708850616,13.375,31.5));
#100995=CARTESIAN_POINT('',(141.240708850616,13.375,25.5));
#100996=CARTESIAN_POINT('Origin',(141.59114422118,13.375,25.5));
#100997=CARTESIAN_POINT('',(141.59114422118,13.375,25.5));
#100998=CARTESIAN_POINT('',(141.59114422118,13.375,25.5));
#100999=CARTESIAN_POINT('',(141.59114422118,13.375,31.5));
#101000=CARTESIAN_POINT('',(141.59114422118,13.375,31.5));
#101001=CARTESIAN_POINT('',(141.59114422118,13.375,25.5));
#101002=CARTESIAN_POINT('Origin',(141.982412223016,14.45,25.5));
#101003=CARTESIAN_POINT('',(141.982412223016,14.45,25.5));
#101004=CARTESIAN_POINT('',(141.982412223016,14.45,25.5));
#101005=CARTESIAN_POINT('',(141.982412223016,14.45,31.5));
#101006=CARTESIAN_POINT('',(141.982412223016,14.45,31.5));
#101007=CARTESIAN_POINT('',(141.982412223016,14.45,25.5));
#101008=CARTESIAN_POINT('Origin',(142.420237175574,14.45,25.5));
#101009=CARTESIAN_POINT('',(142.420237175574,14.45,25.5));
#101010=CARTESIAN_POINT('',(142.420237175574,14.45,25.5));
#101011=CARTESIAN_POINT('',(142.420237175574,14.45,31.5));
#101012=CARTESIAN_POINT('',(142.420237175574,14.45,31.5));
#101013=CARTESIAN_POINT('',(142.420237175574,14.45,25.5));
#101014=CARTESIAN_POINT('Origin',(142.81150517741,13.375,25.5));
#101015=CARTESIAN_POINT('',(142.81150517741,13.375,25.5));
#101016=CARTESIAN_POINT('',(142.81150517741,13.375,25.5));
#101017=CARTESIAN_POINT('',(142.81150517741,13.375,31.5));
#101018=CARTESIAN_POINT('',(142.81150517741,13.375,31.5));
#101019=CARTESIAN_POINT('',(142.81150517741,13.375,25.5));
#101020=CARTESIAN_POINT('Origin',(143.161940547975,13.375,25.5));
#101021=CARTESIAN_POINT('',(143.161940547975,13.375,25.5));
#101022=CARTESIAN_POINT('',(143.161940547975,13.375,25.5));
#101023=CARTESIAN_POINT('',(143.161940547975,13.375,31.5));
#101024=CARTESIAN_POINT('',(143.161940547975,13.375,31.5));
#101025=CARTESIAN_POINT('',(143.161940547975,13.375,25.5));
#101026=CARTESIAN_POINT('Origin',(143.553208549811,14.45,25.5));
#101027=CARTESIAN_POINT('',(143.553208549811,14.45,25.5));
#101028=CARTESIAN_POINT('',(143.553208549811,14.45,25.5));
#101029=CARTESIAN_POINT('',(143.553208549811,14.45,31.5));
#101030=CARTESIAN_POINT('',(143.553208549811,14.45,31.5));
#101031=CARTESIAN_POINT('',(143.553208549811,14.45,25.5));
#101032=CARTESIAN_POINT('Origin',(143.991033502369,14.45,25.5));
#101033=CARTESIAN_POINT('',(143.991033502369,14.45,25.5));
#101034=CARTESIAN_POINT('',(143.991033502369,14.45,25.5));
#101035=CARTESIAN_POINT('',(143.991033502369,14.45,31.5));
#101036=CARTESIAN_POINT('',(143.991033502369,14.45,31.5));
#101037=CARTESIAN_POINT('',(143.991033502369,14.45,25.5));
#101038=CARTESIAN_POINT('Origin',(144.382301504205,13.375,25.5));
#101039=CARTESIAN_POINT('',(144.382301504205,13.375,25.5));
#101040=CARTESIAN_POINT('',(144.382301504205,13.375,25.5));
#101041=CARTESIAN_POINT('',(144.382301504205,13.375,31.5));
#101042=CARTESIAN_POINT('',(144.382301504205,13.375,31.5));
#101043=CARTESIAN_POINT('',(144.382301504205,13.375,25.5));
#101044=CARTESIAN_POINT('Origin',(144.73273687477,13.375,25.5));
#101045=CARTESIAN_POINT('',(144.73273687477,13.375,25.5));
#101046=CARTESIAN_POINT('',(144.73273687477,13.375,25.5));
#101047=CARTESIAN_POINT('',(144.73273687477,13.375,31.5));
#101048=CARTESIAN_POINT('',(144.73273687477,13.375,31.5));
#101049=CARTESIAN_POINT('',(144.73273687477,13.375,25.5));
#101050=CARTESIAN_POINT('Origin',(145.124004876606,14.45,25.5));
#101051=CARTESIAN_POINT('',(145.124004876606,14.45,25.5));
#101052=CARTESIAN_POINT('',(145.124004876606,14.45,25.5));
#101053=CARTESIAN_POINT('',(145.124004876606,14.45,31.5));
#101054=CARTESIAN_POINT('',(145.124004876606,14.45,31.5));
#101055=CARTESIAN_POINT('',(145.124004876606,14.45,25.5));
#101056=CARTESIAN_POINT('Origin',(145.561829829164,14.45,25.5));
#101057=CARTESIAN_POINT('',(145.561829829164,14.45,25.5));
#101058=CARTESIAN_POINT('',(145.561829829164,14.45,25.5));
#101059=CARTESIAN_POINT('',(145.561829829164,14.45,31.5));
#101060=CARTESIAN_POINT('',(145.561829829164,14.45,31.5));
#101061=CARTESIAN_POINT('',(145.561829829164,14.45,25.5));
#101062=CARTESIAN_POINT('Origin',(145.953097831,13.375,25.5));
#101063=CARTESIAN_POINT('',(145.953097831,13.375,25.5));
#101064=CARTESIAN_POINT('',(145.953097831,13.375,25.5));
#101065=CARTESIAN_POINT('',(145.953097831,13.375,31.5));
#101066=CARTESIAN_POINT('',(145.953097831,13.375,31.5));
#101067=CARTESIAN_POINT('',(145.953097831,13.375,25.5));
#101068=CARTESIAN_POINT('Origin',(146.303533201565,13.375,25.5));
#101069=CARTESIAN_POINT('',(146.303533201565,13.375,25.5));
#101070=CARTESIAN_POINT('',(146.303533201565,13.375,25.5));
#101071=CARTESIAN_POINT('',(146.303533201565,13.375,31.5));
#101072=CARTESIAN_POINT('',(146.303533201565,13.375,31.5));
#101073=CARTESIAN_POINT('',(146.303533201565,13.375,25.5));
#101074=CARTESIAN_POINT('Origin',(146.694801203401,14.45,25.5));
#101075=CARTESIAN_POINT('',(146.694801203401,14.45,25.5));
#101076=CARTESIAN_POINT('',(146.694801203401,14.45,25.5));
#101077=CARTESIAN_POINT('',(146.694801203401,14.45,31.5));
#101078=CARTESIAN_POINT('',(146.694801203401,14.45,31.5));
#101079=CARTESIAN_POINT('',(146.694801203401,14.45,25.5));
#101080=CARTESIAN_POINT('Origin',(147.132626155959,14.45,25.5));
#101081=CARTESIAN_POINT('',(147.132626155959,14.45,25.5));
#101082=CARTESIAN_POINT('',(147.132626155959,14.45,25.5));
#101083=CARTESIAN_POINT('',(147.132626155959,14.45,31.5));
#101084=CARTESIAN_POINT('',(147.132626155959,14.45,31.5));
#101085=CARTESIAN_POINT('',(147.132626155959,14.45,25.5));
#101086=CARTESIAN_POINT('Origin',(147.523894157795,13.375,25.5));
#101087=CARTESIAN_POINT('',(147.523894157795,13.375,25.5));
#101088=CARTESIAN_POINT('',(147.523894157795,13.375,25.5));
#101089=CARTESIAN_POINT('',(147.523894157795,13.375,31.5));
#101090=CARTESIAN_POINT('',(147.523894157795,13.375,31.5));
#101091=CARTESIAN_POINT('',(147.523894157795,13.375,25.5));
#101092=CARTESIAN_POINT('Origin',(147.87432952836,13.375,25.5));
#101093=CARTESIAN_POINT('',(147.87432952836,13.375,25.5));
#101094=CARTESIAN_POINT('',(147.87432952836,13.375,25.5));
#101095=CARTESIAN_POINT('',(147.87432952836,13.375,31.5));
#101096=CARTESIAN_POINT('',(147.87432952836,13.375,31.5));
#101097=CARTESIAN_POINT('',(147.87432952836,13.375,25.5));
#101098=CARTESIAN_POINT('Origin',(148.265597530196,14.45,25.5));
#101099=CARTESIAN_POINT('',(148.265597530196,14.45,25.5));
#101100=CARTESIAN_POINT('',(148.265597530196,14.45,25.5));
#101101=CARTESIAN_POINT('',(148.265597530196,14.45,31.5));
#101102=CARTESIAN_POINT('',(148.265597530196,14.45,31.5));
#101103=CARTESIAN_POINT('',(148.265597530196,14.45,25.5));
#101104=CARTESIAN_POINT('Origin',(148.703422482754,14.45,25.5));
#101105=CARTESIAN_POINT('',(148.703422482754,14.45,25.5));
#101106=CARTESIAN_POINT('',(148.703422482754,14.45,25.5));
#101107=CARTESIAN_POINT('',(148.703422482754,14.45,31.5));
#101108=CARTESIAN_POINT('',(148.703422482754,14.45,31.5));
#101109=CARTESIAN_POINT('',(148.703422482754,14.45,25.5));
#101110=CARTESIAN_POINT('Origin',(149.09469048459,13.375,25.5));
#101111=CARTESIAN_POINT('',(149.09469048459,13.375,25.5));
#101112=CARTESIAN_POINT('',(149.09469048459,13.375,25.5));
#101113=CARTESIAN_POINT('',(149.09469048459,13.375,31.5));
#101114=CARTESIAN_POINT('',(149.09469048459,13.375,31.5));
#101115=CARTESIAN_POINT('',(149.09469048459,13.375,25.5));
#101116=CARTESIAN_POINT('Origin',(149.445125855155,13.375,25.5));
#101117=CARTESIAN_POINT('',(149.445125855155,13.375,25.5));
#101118=CARTESIAN_POINT('',(149.445125855155,13.375,25.5));
#101119=CARTESIAN_POINT('',(149.445125855155,13.375,31.5));
#101120=CARTESIAN_POINT('',(149.445125855155,13.375,31.5));
#101121=CARTESIAN_POINT('',(149.445125855155,13.375,25.5));
#101122=CARTESIAN_POINT('Origin',(149.836393856991,14.45,25.5));
#101123=CARTESIAN_POINT('',(149.836393856991,14.45,25.5));
#101124=CARTESIAN_POINT('',(149.836393856991,14.45,25.5));
#101125=CARTESIAN_POINT('',(149.836393856991,14.45,31.5));
#101126=CARTESIAN_POINT('',(149.836393856991,14.45,31.5));
#101127=CARTESIAN_POINT('',(149.836393856991,14.45,25.5));
#101128=CARTESIAN_POINT('Origin',(150.274218809549,14.45,25.5));
#101129=CARTESIAN_POINT('',(150.274218809549,14.45,25.5));
#101130=CARTESIAN_POINT('',(150.274218809549,14.45,25.5));
#101131=CARTESIAN_POINT('',(150.274218809549,14.45,31.5));
#101132=CARTESIAN_POINT('',(150.274218809549,14.45,31.5));
#101133=CARTESIAN_POINT('',(150.274218809549,14.45,25.5));
#101134=CARTESIAN_POINT('Origin',(150.665486811385,13.375,25.5));
#101135=CARTESIAN_POINT('',(150.665486811385,13.375,25.5));
#101136=CARTESIAN_POINT('',(150.665486811385,13.375,25.5));
#101137=CARTESIAN_POINT('',(150.665486811385,13.375,31.5));
#101138=CARTESIAN_POINT('',(150.665486811385,13.375,31.5));
#101139=CARTESIAN_POINT('',(150.665486811385,13.375,25.5));
#101140=CARTESIAN_POINT('Origin',(151.01592218195,13.375,25.5));
#101141=CARTESIAN_POINT('',(151.01592218195,13.375,25.5));
#101142=CARTESIAN_POINT('',(151.01592218195,13.375,25.5));
#101143=CARTESIAN_POINT('',(151.01592218195,13.375,31.5));
#101144=CARTESIAN_POINT('',(151.01592218195,13.375,31.5));
#101145=CARTESIAN_POINT('',(151.01592218195,13.375,25.5));
#101146=CARTESIAN_POINT('Origin',(151.407190183786,14.45,25.5));
#101147=CARTESIAN_POINT('',(151.407190183786,14.45,25.5));
#101148=CARTESIAN_POINT('',(151.407190183786,14.45,25.5));
#101149=CARTESIAN_POINT('',(151.407190183786,14.45,31.5));
#101150=CARTESIAN_POINT('',(151.407190183786,14.45,31.5));
#101151=CARTESIAN_POINT('',(151.407190183786,14.45,25.5));
#101152=CARTESIAN_POINT('Origin',(151.845015136344,14.45,25.5));
#101153=CARTESIAN_POINT('',(151.845015136344,14.45,25.5));
#101154=CARTESIAN_POINT('',(151.845015136344,14.45,25.5));
#101155=CARTESIAN_POINT('',(151.845015136344,14.45,31.5));
#101156=CARTESIAN_POINT('',(151.845015136344,14.45,31.5));
#101157=CARTESIAN_POINT('',(151.845015136344,14.45,25.5));
#101158=CARTESIAN_POINT('Origin',(152.23628313818,13.375,25.5));
#101159=CARTESIAN_POINT('',(152.23628313818,13.375,25.5));
#101160=CARTESIAN_POINT('',(152.23628313818,13.375,25.5));
#101161=CARTESIAN_POINT('',(152.23628313818,13.375,31.5));
#101162=CARTESIAN_POINT('',(152.23628313818,13.375,31.5));
#101163=CARTESIAN_POINT('',(152.23628313818,13.375,25.5));
#101164=CARTESIAN_POINT('Origin',(152.586718508745,13.375,25.5));
#101165=CARTESIAN_POINT('',(152.586718508745,13.375,25.5));
#101166=CARTESIAN_POINT('',(152.586718508745,13.375,25.5));
#101167=CARTESIAN_POINT('',(152.586718508745,13.375,31.5));
#101168=CARTESIAN_POINT('',(152.586718508745,13.375,31.5));
#101169=CARTESIAN_POINT('',(152.586718508745,13.375,25.5));
#101170=CARTESIAN_POINT('Origin',(152.977986510581,14.45,25.5));
#101171=CARTESIAN_POINT('',(152.977986510581,14.45,25.5));
#101172=CARTESIAN_POINT('',(152.977986510581,14.45,25.5));
#101173=CARTESIAN_POINT('',(152.977986510581,14.45,31.5));
#101174=CARTESIAN_POINT('',(152.977986510581,14.45,31.5));
#101175=CARTESIAN_POINT('',(152.977986510581,14.45,25.5));
#101176=CARTESIAN_POINT('Origin',(153.415811463139,14.45,25.5));
#101177=CARTESIAN_POINT('',(153.415811463139,14.45,25.5));
#101178=CARTESIAN_POINT('',(153.415811463139,14.45,25.5));
#101179=CARTESIAN_POINT('',(153.415811463139,14.45,31.5));
#101180=CARTESIAN_POINT('',(153.415811463139,14.45,31.5));
#101181=CARTESIAN_POINT('',(153.415811463139,14.45,25.5));
#101182=CARTESIAN_POINT('Origin',(153.807079464975,13.375,25.5));
#101183=CARTESIAN_POINT('',(153.807079464975,13.375,25.5));
#101184=CARTESIAN_POINT('',(153.807079464975,13.375,25.5));
#101185=CARTESIAN_POINT('',(153.807079464975,13.375,31.5));
#101186=CARTESIAN_POINT('',(153.807079464975,13.375,31.5));
#101187=CARTESIAN_POINT('',(153.807079464975,13.375,25.5));
#101188=CARTESIAN_POINT('Origin',(154.157514835539,13.375,25.5));
#101189=CARTESIAN_POINT('',(154.157514835539,13.375,25.5));
#101190=CARTESIAN_POINT('',(154.157514835539,13.375,25.5));
#101191=CARTESIAN_POINT('',(154.157514835539,13.375,31.5));
#101192=CARTESIAN_POINT('',(154.157514835539,13.375,31.5));
#101193=CARTESIAN_POINT('',(154.157514835539,13.375,25.5));
#101194=CARTESIAN_POINT('Origin',(154.548782837376,14.45,25.5));
#101195=CARTESIAN_POINT('',(154.548782837376,14.45,25.5));
#101196=CARTESIAN_POINT('',(154.548782837376,14.45,25.5));
#101197=CARTESIAN_POINT('',(154.548782837376,14.45,31.5));
#101198=CARTESIAN_POINT('',(154.548782837376,14.45,31.5));
#101199=CARTESIAN_POINT('',(154.548782837376,14.45,25.5));
#101200=CARTESIAN_POINT('Origin',(154.986607789934,14.45,25.5));
#101201=CARTESIAN_POINT('',(154.986607789934,14.45,25.5));
#101202=CARTESIAN_POINT('',(154.986607789934,14.45,25.5));
#101203=CARTESIAN_POINT('',(154.986607789934,14.45,31.5));
#101204=CARTESIAN_POINT('',(154.986607789934,14.45,31.5));
#101205=CARTESIAN_POINT('',(154.986607789934,14.45,25.5));
#101206=CARTESIAN_POINT('Origin',(155.37787579177,13.375,25.5));
#101207=CARTESIAN_POINT('',(155.37787579177,13.375,25.5));
#101208=CARTESIAN_POINT('',(155.37787579177,13.375,25.5));
#101209=CARTESIAN_POINT('',(155.37787579177,13.375,31.5));
#101210=CARTESIAN_POINT('',(155.37787579177,13.375,31.5));
#101211=CARTESIAN_POINT('',(155.37787579177,13.375,25.5));
#101212=CARTESIAN_POINT('Origin',(155.728311162334,13.375,25.5));
#101213=CARTESIAN_POINT('',(155.728311162334,13.375,25.5));
#101214=CARTESIAN_POINT('',(155.728311162334,13.375,25.5));
#101215=CARTESIAN_POINT('',(155.728311162334,13.375,31.5));
#101216=CARTESIAN_POINT('',(155.728311162334,13.375,31.5));
#101217=CARTESIAN_POINT('',(155.728311162334,13.375,25.5));
#101218=CARTESIAN_POINT('Origin',(156.119579164171,14.45,25.5));
#101219=CARTESIAN_POINT('',(156.119579164171,14.45,25.5));
#101220=CARTESIAN_POINT('',(156.119579164171,14.45,25.5));
#101221=CARTESIAN_POINT('',(156.119579164171,14.45,31.5));
#101222=CARTESIAN_POINT('',(156.119579164171,14.45,31.5));
#101223=CARTESIAN_POINT('',(156.119579164171,14.45,25.5));
#101224=CARTESIAN_POINT('Origin',(156.557404116728,14.45,25.5));
#101225=CARTESIAN_POINT('',(156.557404116728,14.45,25.5));
#101226=CARTESIAN_POINT('',(156.557404116728,14.45,25.5));
#101227=CARTESIAN_POINT('',(156.557404116728,14.45,31.5));
#101228=CARTESIAN_POINT('',(156.557404116728,14.45,31.5));
#101229=CARTESIAN_POINT('',(156.557404116728,14.45,25.5));
#101230=CARTESIAN_POINT('Origin',(156.948672118565,13.375,25.5));
#101231=CARTESIAN_POINT('',(156.948672118565,13.375,25.5));
#101232=CARTESIAN_POINT('',(156.948672118565,13.375,25.5));
#101233=CARTESIAN_POINT('',(156.948672118565,13.375,31.5));
#101234=CARTESIAN_POINT('',(156.948672118565,13.375,31.5));
#101235=CARTESIAN_POINT('',(156.948672118565,13.375,25.5));
#101236=CARTESIAN_POINT('Origin',(157.299107489129,13.375,25.5));
#101237=CARTESIAN_POINT('',(157.299107489129,13.375,25.5));
#101238=CARTESIAN_POINT('',(157.299107489129,13.375,25.5));
#101239=CARTESIAN_POINT('',(157.299107489129,13.375,31.5));
#101240=CARTESIAN_POINT('',(157.299107489129,13.375,31.5));
#101241=CARTESIAN_POINT('',(157.299107489129,13.375,25.5));
#101242=CARTESIAN_POINT('Origin',(157.690375490965,14.45,25.5));
#101243=CARTESIAN_POINT('',(157.690375490965,14.45,25.5));
#101244=CARTESIAN_POINT('',(157.690375490965,14.45,25.5));
#101245=CARTESIAN_POINT('',(157.690375490965,14.45,31.5));
#101246=CARTESIAN_POINT('',(157.690375490965,14.45,31.5));
#101247=CARTESIAN_POINT('',(157.690375490965,14.45,25.5));
#101248=CARTESIAN_POINT('Origin',(158.128200443523,14.45,25.5));
#101249=CARTESIAN_POINT('',(158.128200443523,14.45,25.5));
#101250=CARTESIAN_POINT('',(158.128200443523,14.45,25.5));
#101251=CARTESIAN_POINT('',(158.128200443523,14.45,31.5));
#101252=CARTESIAN_POINT('',(158.128200443523,14.45,31.5));
#101253=CARTESIAN_POINT('',(158.128200443523,14.45,25.5));
#101254=CARTESIAN_POINT('Origin',(158.519468445359,13.375,25.5));
#101255=CARTESIAN_POINT('',(158.519468445359,13.375,25.5));
#101256=CARTESIAN_POINT('',(158.519468445359,13.375,25.5));
#101257=CARTESIAN_POINT('',(158.519468445359,13.375,31.5));
#101258=CARTESIAN_POINT('',(158.519468445359,13.375,31.5));
#101259=CARTESIAN_POINT('',(158.519468445359,13.375,25.5));
#101260=CARTESIAN_POINT('Origin',(158.869903815924,13.375,25.5));
#101261=CARTESIAN_POINT('',(158.869903815924,13.375,25.5));
#101262=CARTESIAN_POINT('',(158.869903815924,13.375,25.5));
#101263=CARTESIAN_POINT('',(158.869903815924,13.375,31.5));
#101264=CARTESIAN_POINT('',(158.869903815924,13.375,31.5));
#101265=CARTESIAN_POINT('',(158.869903815924,13.375,25.5));
#101266=CARTESIAN_POINT('Origin',(159.26117181776,14.45,25.5));
#101267=CARTESIAN_POINT('',(159.26117181776,14.45,25.5));
#101268=CARTESIAN_POINT('',(159.26117181776,14.45,25.5));
#101269=CARTESIAN_POINT('',(159.26117181776,14.45,31.5));
#101270=CARTESIAN_POINT('',(159.26117181776,14.45,31.5));
#101271=CARTESIAN_POINT('',(159.26117181776,14.45,25.5));
#101272=CARTESIAN_POINT('Origin',(159.698996770318,14.45,25.5));
#101273=CARTESIAN_POINT('',(159.698996770318,14.45,25.5));
#101274=CARTESIAN_POINT('',(159.698996770318,14.45,25.5));
#101275=CARTESIAN_POINT('',(159.698996770318,14.45,31.5));
#101276=CARTESIAN_POINT('',(159.698996770318,14.45,31.5));
#101277=CARTESIAN_POINT('',(159.698996770318,14.45,25.5));
#101278=CARTESIAN_POINT('Origin',(160.090264772154,13.375,25.5));
#101279=CARTESIAN_POINT('',(160.090264772154,13.375,25.5));
#101280=CARTESIAN_POINT('',(160.090264772154,13.375,25.5));
#101281=CARTESIAN_POINT('',(160.090264772154,13.375,31.5));
#101282=CARTESIAN_POINT('',(160.090264772154,13.375,31.5));
#101283=CARTESIAN_POINT('',(160.090264772154,13.375,25.5));
#101284=CARTESIAN_POINT('Origin',(160.440700142719,13.375,25.5));
#101285=CARTESIAN_POINT('',(160.440700142719,13.375,25.5));
#101286=CARTESIAN_POINT('',(160.440700142719,13.375,25.5));
#101287=CARTESIAN_POINT('',(160.440700142719,13.375,31.5));
#101288=CARTESIAN_POINT('',(160.440700142719,13.375,31.5));
#101289=CARTESIAN_POINT('',(160.440700142719,13.375,25.5));
#101290=CARTESIAN_POINT('Origin',(160.831968144555,14.45,25.5));
#101291=CARTESIAN_POINT('',(160.831968144555,14.45,25.5));
#101292=CARTESIAN_POINT('',(160.831968144555,14.45,25.5));
#101293=CARTESIAN_POINT('',(160.831968144555,14.45,31.5));
#101294=CARTESIAN_POINT('',(160.831968144555,14.45,31.5));
#101295=CARTESIAN_POINT('',(160.831968144555,14.45,25.5));
#101296=CARTESIAN_POINT('Origin',(161.269793097113,14.45,25.5));
#101297=CARTESIAN_POINT('',(161.269793097113,14.45,25.5));
#101298=CARTESIAN_POINT('',(161.269793097113,14.45,25.5));
#101299=CARTESIAN_POINT('',(161.269793097113,14.45,31.5));
#101300=CARTESIAN_POINT('',(161.269793097113,14.45,31.5));
#101301=CARTESIAN_POINT('',(161.269793097113,14.45,25.5));
#101302=CARTESIAN_POINT('Origin',(161.661061098949,13.375,25.5));
#101303=CARTESIAN_POINT('',(161.661061098949,13.375,25.5));
#101304=CARTESIAN_POINT('',(161.661061098949,13.375,25.5));
#101305=CARTESIAN_POINT('',(161.661061098949,13.375,31.5));
#101306=CARTESIAN_POINT('',(161.661061098949,13.375,31.5));
#101307=CARTESIAN_POINT('',(161.661061098949,13.375,25.5));
#101308=CARTESIAN_POINT('Origin',(162.011496469514,13.375,25.5));
#101309=CARTESIAN_POINT('',(162.011496469514,13.375,25.5));
#101310=CARTESIAN_POINT('',(162.011496469514,13.375,25.5));
#101311=CARTESIAN_POINT('',(162.011496469514,13.375,31.5));
#101312=CARTESIAN_POINT('',(162.011496469514,13.375,31.5));
#101313=CARTESIAN_POINT('',(162.011496469514,13.375,25.5));
#101314=CARTESIAN_POINT('Origin',(162.40276447135,14.45,25.5));
#101315=CARTESIAN_POINT('',(162.40276447135,14.45,25.5));
#101316=CARTESIAN_POINT('',(162.40276447135,14.45,25.5));
#101317=CARTESIAN_POINT('',(162.40276447135,14.45,31.5));
#101318=CARTESIAN_POINT('',(162.40276447135,14.45,31.5));
#101319=CARTESIAN_POINT('',(162.40276447135,14.45,25.5));
#101320=CARTESIAN_POINT('Origin',(162.840589423908,14.45,25.5));
#101321=CARTESIAN_POINT('',(162.840589423908,14.45,25.5));
#101322=CARTESIAN_POINT('',(162.840589423908,14.45,25.5));
#101323=CARTESIAN_POINT('',(162.840589423908,14.45,31.5));
#101324=CARTESIAN_POINT('',(162.840589423908,14.45,31.5));
#101325=CARTESIAN_POINT('',(162.840589423908,14.45,25.5));
#101326=CARTESIAN_POINT('Origin',(163.231857425744,13.375,25.5));
#101327=CARTESIAN_POINT('',(163.231857425744,13.375,25.5));
#101328=CARTESIAN_POINT('',(163.231857425744,13.375,25.5));
#101329=CARTESIAN_POINT('',(163.231857425744,13.375,31.5));
#101330=CARTESIAN_POINT('',(163.231857425744,13.375,31.5));
#101331=CARTESIAN_POINT('',(163.231857425744,13.375,25.5));
#101332=CARTESIAN_POINT('Origin',(163.582292796309,13.375,25.5));
#101333=CARTESIAN_POINT('',(163.582292796309,13.375,25.5));
#101334=CARTESIAN_POINT('',(163.582292796309,13.375,25.5));
#101335=CARTESIAN_POINT('',(163.582292796309,13.375,31.5));
#101336=CARTESIAN_POINT('',(163.582292796309,13.375,31.5));
#101337=CARTESIAN_POINT('',(163.582292796309,13.375,25.5));
#101338=CARTESIAN_POINT('Origin',(163.973560798145,14.45,25.5));
#101339=CARTESIAN_POINT('',(163.973560798145,14.45,25.5));
#101340=CARTESIAN_POINT('',(163.973560798145,14.45,25.5));
#101341=CARTESIAN_POINT('',(163.973560798145,14.45,31.5));
#101342=CARTESIAN_POINT('',(163.973560798145,14.45,31.5));
#101343=CARTESIAN_POINT('',(163.973560798145,14.45,25.5));
#101344=CARTESIAN_POINT('Origin',(164.411385750703,14.45,25.5));
#101345=CARTESIAN_POINT('',(164.411385750703,14.45,25.5));
#101346=CARTESIAN_POINT('',(164.411385750703,14.45,25.5));
#101347=CARTESIAN_POINT('',(164.411385750703,14.45,31.5));
#101348=CARTESIAN_POINT('',(164.411385750703,14.45,31.5));
#101349=CARTESIAN_POINT('',(164.411385750703,14.45,25.5));
#101350=CARTESIAN_POINT('Origin',(164.802653752539,13.375,25.5));
#101351=CARTESIAN_POINT('',(164.802653752539,13.375,25.5));
#101352=CARTESIAN_POINT('',(164.802653752539,13.375,25.5));
#101353=CARTESIAN_POINT('',(164.802653752539,13.375,31.5));
#101354=CARTESIAN_POINT('',(164.802653752539,13.375,31.5));
#101355=CARTESIAN_POINT('',(164.802653752539,13.375,25.5));
#101356=CARTESIAN_POINT('Origin',(165.153089123104,13.375,25.5));
#101357=CARTESIAN_POINT('',(165.153089123104,13.375,25.5));
#101358=CARTESIAN_POINT('',(165.153089123104,13.375,25.5));
#101359=CARTESIAN_POINT('',(165.153089123104,13.375,31.5));
#101360=CARTESIAN_POINT('',(165.153089123104,13.375,31.5));
#101361=CARTESIAN_POINT('',(165.153089123104,13.375,25.5));
#101362=CARTESIAN_POINT('Origin',(165.54435712494,14.45,25.5));
#101363=CARTESIAN_POINT('',(165.54435712494,14.45,25.5));
#101364=CARTESIAN_POINT('',(165.54435712494,14.45,25.5));
#101365=CARTESIAN_POINT('',(165.54435712494,14.45,31.5));
#101366=CARTESIAN_POINT('',(165.54435712494,14.45,31.5));
#101367=CARTESIAN_POINT('',(165.54435712494,14.45,25.5));
#101368=CARTESIAN_POINT('Origin',(165.982182077498,14.45,25.5));
#101369=CARTESIAN_POINT('',(165.982182077498,14.45,25.5));
#101370=CARTESIAN_POINT('',(165.982182077498,14.45,25.5));
#101371=CARTESIAN_POINT('',(165.982182077498,14.45,31.5));
#101372=CARTESIAN_POINT('',(165.982182077498,14.45,31.5));
#101373=CARTESIAN_POINT('',(165.982182077498,14.45,25.5));
#101374=CARTESIAN_POINT('Origin',(166.373450079334,13.375,25.5));
#101375=CARTESIAN_POINT('',(166.373450079334,13.375,25.5));
#101376=CARTESIAN_POINT('',(166.373450079334,13.375,25.5));
#101377=CARTESIAN_POINT('',(166.373450079334,13.375,31.5));
#101378=CARTESIAN_POINT('',(166.373450079334,13.375,31.5));
#101379=CARTESIAN_POINT('',(166.373450079334,13.375,25.5));
#101380=CARTESIAN_POINT('Origin',(166.723885449899,13.375,25.5));
#101381=CARTESIAN_POINT('',(166.723885449899,13.375,25.5));
#101382=CARTESIAN_POINT('',(166.723885449899,13.375,25.5));
#101383=CARTESIAN_POINT('',(166.723885449899,13.375,31.5));
#101384=CARTESIAN_POINT('',(166.723885449899,13.375,31.5));
#101385=CARTESIAN_POINT('',(166.723885449899,13.375,25.5));
#101386=CARTESIAN_POINT('Origin',(167.115153451735,14.45,25.5));
#101387=CARTESIAN_POINT('',(167.115153451735,14.45,25.5));
#101388=CARTESIAN_POINT('',(167.115153451735,14.45,25.5));
#101389=CARTESIAN_POINT('',(167.115153451735,14.45,31.5));
#101390=CARTESIAN_POINT('',(167.115153451735,14.45,31.5));
#101391=CARTESIAN_POINT('',(167.115153451735,14.45,25.5));
#101392=CARTESIAN_POINT('Origin',(167.552978404293,14.45,25.5));
#101393=CARTESIAN_POINT('',(167.552978404293,14.45,25.5));
#101394=CARTESIAN_POINT('',(167.552978404293,14.45,25.5));
#101395=CARTESIAN_POINT('',(167.552978404293,14.45,31.5));
#101396=CARTESIAN_POINT('',(167.552978404293,14.45,31.5));
#101397=CARTESIAN_POINT('',(167.552978404293,14.45,25.5));
#101398=CARTESIAN_POINT('Origin',(167.944246406129,13.375,25.5));
#101399=CARTESIAN_POINT('',(167.944246406129,13.375,25.5));
#101400=CARTESIAN_POINT('',(167.944246406129,13.375,25.5));
#101401=CARTESIAN_POINT('',(167.944246406129,13.375,31.5));
#101402=CARTESIAN_POINT('',(167.944246406129,13.375,31.5));
#101403=CARTESIAN_POINT('',(167.944246406129,13.375,25.5));
#101404=CARTESIAN_POINT('Origin',(168.294681776694,13.375,25.5));
#101405=CARTESIAN_POINT('',(168.294681776694,13.375,25.5));
#101406=CARTESIAN_POINT('',(168.294681776694,13.375,25.5));
#101407=CARTESIAN_POINT('',(168.294681776694,13.375,31.5));
#101408=CARTESIAN_POINT('',(168.294681776694,13.375,31.5));
#101409=CARTESIAN_POINT('',(168.294681776694,13.375,25.5));
#101410=CARTESIAN_POINT('Origin',(168.68594977853,14.45,25.5));
#101411=CARTESIAN_POINT('',(168.68594977853,14.45,25.5));
#101412=CARTESIAN_POINT('',(168.68594977853,14.45,25.5));
#101413=CARTESIAN_POINT('',(168.68594977853,14.45,31.5));
#101414=CARTESIAN_POINT('',(168.68594977853,14.45,31.5));
#101415=CARTESIAN_POINT('',(168.68594977853,14.45,25.5));
#101416=CARTESIAN_POINT('Origin',(169.123774731088,14.45,25.5));
#101417=CARTESIAN_POINT('',(169.123774731088,14.45,25.5));
#101418=CARTESIAN_POINT('',(169.123774731088,14.45,25.5));
#101419=CARTESIAN_POINT('',(169.123774731088,14.45,31.5));
#101420=CARTESIAN_POINT('',(169.123774731088,14.45,31.5));
#101421=CARTESIAN_POINT('',(169.123774731088,14.45,25.5));
#101422=CARTESIAN_POINT('Origin',(169.515042732924,13.375,25.5));
#101423=CARTESIAN_POINT('',(169.515042732924,13.375,25.5));
#101424=CARTESIAN_POINT('',(169.515042732924,13.375,25.5));
#101425=CARTESIAN_POINT('',(169.515042732924,13.375,31.5));
#101426=CARTESIAN_POINT('',(169.515042732924,13.375,31.5));
#101427=CARTESIAN_POINT('',(169.515042732924,13.375,25.5));
#101428=CARTESIAN_POINT('Origin',(169.865478103488,13.375,25.5));
#101429=CARTESIAN_POINT('',(169.865478103488,13.375,25.5));
#101430=CARTESIAN_POINT('',(169.865478103488,13.375,25.5));
#101431=CARTESIAN_POINT('',(169.865478103488,13.375,31.5));
#101432=CARTESIAN_POINT('',(169.865478103488,13.375,31.5));
#101433=CARTESIAN_POINT('',(169.865478103488,13.375,25.5));
#101434=CARTESIAN_POINT('Origin',(170.256746105325,14.45,25.5));
#101435=CARTESIAN_POINT('',(170.256746105325,14.45,25.5));
#101436=CARTESIAN_POINT('',(170.256746105325,14.45,25.5));
#101437=CARTESIAN_POINT('',(170.256746105325,14.45,31.5));
#101438=CARTESIAN_POINT('',(170.256746105325,14.45,31.5));
#101439=CARTESIAN_POINT('',(170.256746105325,14.45,25.5));
#101440=CARTESIAN_POINT('Origin',(170.694571057882,14.45,25.5));
#101441=CARTESIAN_POINT('',(170.694571057882,14.45,25.5));
#101442=CARTESIAN_POINT('',(170.694571057882,14.45,25.5));
#101443=CARTESIAN_POINT('',(170.694571057882,14.45,31.5));
#101444=CARTESIAN_POINT('',(170.694571057882,14.45,31.5));
#101445=CARTESIAN_POINT('',(170.694571057882,14.45,25.5));
#101446=CARTESIAN_POINT('Origin',(171.085839059719,13.375,25.5));
#101447=CARTESIAN_POINT('',(171.085839059719,13.375,25.5));
#101448=CARTESIAN_POINT('',(171.085839059719,13.375,25.5));
#101449=CARTESIAN_POINT('',(171.085839059719,13.375,31.5));
#101450=CARTESIAN_POINT('',(171.085839059719,13.375,31.5));
#101451=CARTESIAN_POINT('',(171.085839059719,13.375,25.5));
#101452=CARTESIAN_POINT('Origin',(171.436274430283,13.375,25.5));
#101453=CARTESIAN_POINT('',(171.436274430283,13.375,25.5));
#101454=CARTESIAN_POINT('',(171.436274430283,13.375,25.5));
#101455=CARTESIAN_POINT('',(171.436274430283,13.375,31.5));
#101456=CARTESIAN_POINT('',(171.436274430283,13.375,31.5));
#101457=CARTESIAN_POINT('',(171.436274430283,13.375,25.5));
#101458=CARTESIAN_POINT('Origin',(171.827542432119,14.45,25.5));
#101459=CARTESIAN_POINT('',(171.827542432119,14.45,25.5));
#101460=CARTESIAN_POINT('',(171.827542432119,14.45,25.5));
#101461=CARTESIAN_POINT('',(171.827542432119,14.45,31.5));
#101462=CARTESIAN_POINT('',(171.827542432119,14.45,31.5));
#101463=CARTESIAN_POINT('',(171.827542432119,14.45,25.5));
#101464=CARTESIAN_POINT('Origin',(172.265367384677,14.45,25.5));
#101465=CARTESIAN_POINT('',(172.265367384677,14.45,25.5));
#101466=CARTESIAN_POINT('',(172.265367384677,14.45,25.5));
#101467=CARTESIAN_POINT('',(172.265367384677,14.45,31.5));
#101468=CARTESIAN_POINT('',(172.265367384677,14.45,31.5));
#101469=CARTESIAN_POINT('',(172.265367384677,14.45,25.5));
#101470=CARTESIAN_POINT('Origin',(172.656635386514,13.375,25.5));
#101471=CARTESIAN_POINT('',(172.656635386514,13.375,25.5));
#101472=CARTESIAN_POINT('',(172.656635386514,13.375,25.5));
#101473=CARTESIAN_POINT('',(172.656635386514,13.375,31.5));
#101474=CARTESIAN_POINT('',(172.656635386514,13.375,31.5));
#101475=CARTESIAN_POINT('',(172.656635386514,13.375,25.5));
#101476=CARTESIAN_POINT('Origin',(173.007070757078,13.375,25.5));
#101477=CARTESIAN_POINT('',(173.007070757078,13.375,25.5));
#101478=CARTESIAN_POINT('',(173.007070757078,13.375,25.5));
#101479=CARTESIAN_POINT('',(173.007070757078,13.375,31.5));
#101480=CARTESIAN_POINT('',(173.007070757078,13.375,31.5));
#101481=CARTESIAN_POINT('',(173.007070757078,13.375,25.5));
#101482=CARTESIAN_POINT('Origin',(173.398338758914,14.45,25.5));
#101483=CARTESIAN_POINT('',(173.398338758914,14.45,25.5));
#101484=CARTESIAN_POINT('',(173.398338758914,14.45,25.5));
#101485=CARTESIAN_POINT('',(173.398338758914,14.45,31.5));
#101486=CARTESIAN_POINT('',(173.398338758914,14.45,31.5));
#101487=CARTESIAN_POINT('',(173.398338758914,14.45,25.5));
#101488=CARTESIAN_POINT('Origin',(173.836163711472,14.45,25.5));
#101489=CARTESIAN_POINT('',(173.836163711472,14.45,25.5));
#101490=CARTESIAN_POINT('',(173.836163711472,14.45,25.5));
#101491=CARTESIAN_POINT('',(173.836163711472,14.45,31.5));
#101492=CARTESIAN_POINT('',(173.836163711472,14.45,31.5));
#101493=CARTESIAN_POINT('',(173.836163711472,14.45,25.5));
#101494=CARTESIAN_POINT('Origin',(174.227431713308,13.375,25.5));
#101495=CARTESIAN_POINT('',(174.227431713308,13.375,25.5));
#101496=CARTESIAN_POINT('',(174.227431713308,13.375,25.5));
#101497=CARTESIAN_POINT('',(174.227431713308,13.375,31.5));
#101498=CARTESIAN_POINT('',(174.227431713308,13.375,31.5));
#101499=CARTESIAN_POINT('',(174.227431713308,13.375,25.5));
#101500=CARTESIAN_POINT('Origin',(174.577867083873,13.375,25.5));
#101501=CARTESIAN_POINT('',(174.577867083873,13.375,25.5));
#101502=CARTESIAN_POINT('',(174.577867083873,13.375,25.5));
#101503=CARTESIAN_POINT('',(174.577867083873,13.375,31.5));
#101504=CARTESIAN_POINT('',(174.577867083873,13.375,31.5));
#101505=CARTESIAN_POINT('',(174.577867083873,13.375,25.5));
#101506=CARTESIAN_POINT('Origin',(174.969135085709,14.45,25.5));
#101507=CARTESIAN_POINT('',(174.969135085709,14.45,25.5));
#101508=CARTESIAN_POINT('',(174.969135085709,14.45,25.5));
#101509=CARTESIAN_POINT('',(174.969135085709,14.45,31.5));
#101510=CARTESIAN_POINT('',(174.969135085709,14.45,31.5));
#101511=CARTESIAN_POINT('',(174.969135085709,14.45,25.5));
#101512=CARTESIAN_POINT('Origin',(175.406960038267,14.45,25.5));
#101513=CARTESIAN_POINT('',(175.406960038267,14.45,25.5));
#101514=CARTESIAN_POINT('',(175.406960038267,14.45,25.5));
#101515=CARTESIAN_POINT('',(175.406960038267,14.45,31.5));
#101516=CARTESIAN_POINT('',(175.406960038267,14.45,31.5));
#101517=CARTESIAN_POINT('',(175.406960038267,14.45,25.5));
#101518=CARTESIAN_POINT('Origin',(175.798228040103,13.375,25.5));
#101519=CARTESIAN_POINT('',(175.798228040103,13.375,25.5));
#101520=CARTESIAN_POINT('',(175.798228040103,13.375,25.5));
#101521=CARTESIAN_POINT('',(175.798228040103,13.375,31.5));
#101522=CARTESIAN_POINT('',(175.798228040103,13.375,31.5));
#101523=CARTESIAN_POINT('',(175.798228040103,13.375,25.5));
#101524=CARTESIAN_POINT('Origin',(176.148663410668,13.375,25.5));
#101525=CARTESIAN_POINT('',(176.148663410668,13.375,25.5));
#101526=CARTESIAN_POINT('',(176.148663410668,13.375,25.5));
#101527=CARTESIAN_POINT('',(176.148663410668,13.375,31.5));
#101528=CARTESIAN_POINT('',(176.148663410668,13.375,31.5));
#101529=CARTESIAN_POINT('',(176.148663410668,13.375,25.5));
#101530=CARTESIAN_POINT('Origin',(176.539931412504,14.45,25.5));
#101531=CARTESIAN_POINT('',(176.539931412504,14.45,25.5));
#101532=CARTESIAN_POINT('',(176.539931412504,14.45,25.5));
#101533=CARTESIAN_POINT('',(176.539931412504,14.45,31.5));
#101534=CARTESIAN_POINT('',(176.539931412504,14.45,31.5));
#101535=CARTESIAN_POINT('',(176.539931412504,14.45,25.5));
#101536=CARTESIAN_POINT('Origin',(176.977756365062,14.45,25.5));
#101537=CARTESIAN_POINT('',(176.977756365062,14.45,25.5));
#101538=CARTESIAN_POINT('',(176.977756365062,14.45,25.5));
#101539=CARTESIAN_POINT('',(176.977756365062,14.45,31.5));
#101540=CARTESIAN_POINT('',(176.977756365062,14.45,31.5));
#101541=CARTESIAN_POINT('',(176.977756365062,14.45,25.5));
#101542=CARTESIAN_POINT('Origin',(177.369024366898,13.375,25.5));
#101543=CARTESIAN_POINT('',(177.369024366898,13.375,25.5));
#101544=CARTESIAN_POINT('',(177.369024366898,13.375,25.5));
#101545=CARTESIAN_POINT('',(177.369024366898,13.375,31.5));
#101546=CARTESIAN_POINT('',(177.369024366898,13.375,31.5));
#101547=CARTESIAN_POINT('',(177.369024366898,13.375,25.5));
#101548=CARTESIAN_POINT('Origin',(177.719459737463,13.375,25.5));
#101549=CARTESIAN_POINT('',(177.719459737463,13.375,25.5));
#101550=CARTESIAN_POINT('',(177.719459737463,13.375,25.5));
#101551=CARTESIAN_POINT('',(177.719459737463,13.375,31.5));
#101552=CARTESIAN_POINT('',(177.719459737463,13.375,31.5));
#101553=CARTESIAN_POINT('',(177.719459737463,13.375,25.5));
#101554=CARTESIAN_POINT('Origin',(178.110727739299,14.45,25.5));
#101555=CARTESIAN_POINT('',(178.110727739299,14.45,25.5));
#101556=CARTESIAN_POINT('',(178.110727739299,14.45,25.5));
#101557=CARTESIAN_POINT('',(178.110727739299,14.45,31.5));
#101558=CARTESIAN_POINT('',(178.110727739299,14.45,31.5));
#101559=CARTESIAN_POINT('',(178.110727739299,14.45,25.5));
#101560=CARTESIAN_POINT('Origin',(178.548552691857,14.45,25.5));
#101561=CARTESIAN_POINT('',(178.548552691857,14.45,25.5));
#101562=CARTESIAN_POINT('',(178.548552691857,14.45,25.5));
#101563=CARTESIAN_POINT('',(178.548552691857,14.45,31.5));
#101564=CARTESIAN_POINT('',(178.548552691857,14.45,31.5));
#101565=CARTESIAN_POINT('',(178.548552691857,14.45,25.5));
#101566=CARTESIAN_POINT('Origin',(178.939820693693,13.375,25.5));
#101567=CARTESIAN_POINT('',(178.939820693693,13.375,25.5));
#101568=CARTESIAN_POINT('',(178.939820693693,13.375,25.5));
#101569=CARTESIAN_POINT('',(178.939820693693,13.375,31.5));
#101570=CARTESIAN_POINT('',(178.939820693693,13.375,31.5));
#101571=CARTESIAN_POINT('',(178.939820693693,13.375,25.5));
#101572=CARTESIAN_POINT('Origin',(179.290256064258,13.375,25.5));
#101573=CARTESIAN_POINT('',(179.290256064258,13.375,25.5));
#101574=CARTESIAN_POINT('',(179.290256064258,13.375,25.5));
#101575=CARTESIAN_POINT('',(179.290256064258,13.375,31.5));
#101576=CARTESIAN_POINT('',(179.290256064258,13.375,31.5));
#101577=CARTESIAN_POINT('',(179.290256064258,13.375,25.5));
#101578=CARTESIAN_POINT('Origin',(179.681524066094,14.45,25.5));
#101579=CARTESIAN_POINT('',(179.681524066094,14.45,25.5));
#101580=CARTESIAN_POINT('',(179.681524066094,14.45,25.5));
#101581=CARTESIAN_POINT('',(179.681524066094,14.45,31.5));
#101582=CARTESIAN_POINT('',(179.681524066094,14.45,31.5));
#101583=CARTESIAN_POINT('',(179.681524066094,14.45,25.5));
#101584=CARTESIAN_POINT('Origin',(180.119349018652,14.45,25.5));
#101585=CARTESIAN_POINT('',(180.119349018652,14.45,25.5));
#101586=CARTESIAN_POINT('',(180.119349018652,14.45,25.5));
#101587=CARTESIAN_POINT('',(180.119349018652,14.45,31.5));
#101588=CARTESIAN_POINT('',(180.119349018652,14.45,31.5));
#101589=CARTESIAN_POINT('',(180.119349018652,14.45,25.5));
#101590=CARTESIAN_POINT('Origin',(180.510617020488,13.375,25.5));
#101591=CARTESIAN_POINT('',(180.510617020488,13.375,25.5));
#101592=CARTESIAN_POINT('',(180.510617020488,13.375,25.5));
#101593=CARTESIAN_POINT('',(180.510617020488,13.375,31.5));
#101594=CARTESIAN_POINT('',(180.510617020488,13.375,31.5));
#101595=CARTESIAN_POINT('',(180.510617020488,13.375,25.5));
#101596=CARTESIAN_POINT('Origin',(180.861052391053,13.375,25.5));
#101597=CARTESIAN_POINT('',(180.861052391053,13.375,25.5));
#101598=CARTESIAN_POINT('',(180.861052391053,13.375,25.5));
#101599=CARTESIAN_POINT('',(180.861052391053,13.375,31.5));
#101600=CARTESIAN_POINT('',(180.861052391053,13.375,31.5));
#101601=CARTESIAN_POINT('',(180.861052391053,13.375,25.5));
#101602=CARTESIAN_POINT('Origin',(181.252320392889,14.45,25.5));
#101603=CARTESIAN_POINT('',(181.252320392889,14.45,25.5));
#101604=CARTESIAN_POINT('',(181.252320392889,14.45,25.5));
#101605=CARTESIAN_POINT('',(181.252320392889,14.45,31.5));
#101606=CARTESIAN_POINT('',(181.252320392889,14.45,31.5));
#101607=CARTESIAN_POINT('',(181.252320392889,14.45,25.5));
#101608=CARTESIAN_POINT('Origin',(181.690145345447,14.45,25.5));
#101609=CARTESIAN_POINT('',(181.690145345447,14.45,25.5));
#101610=CARTESIAN_POINT('',(181.690145345447,14.45,25.5));
#101611=CARTESIAN_POINT('',(181.690145345447,14.45,31.5));
#101612=CARTESIAN_POINT('',(181.690145345447,14.45,31.5));
#101613=CARTESIAN_POINT('',(181.690145345447,14.45,25.5));
#101614=CARTESIAN_POINT('Origin',(182.081413347283,13.375,25.5));
#101615=CARTESIAN_POINT('',(182.081413347283,13.375,25.5));
#101616=CARTESIAN_POINT('',(182.081413347283,13.375,25.5));
#101617=CARTESIAN_POINT('',(182.081413347283,13.375,31.5));
#101618=CARTESIAN_POINT('',(182.081413347283,13.375,31.5));
#101619=CARTESIAN_POINT('',(182.081413347283,13.375,25.5));
#101620=CARTESIAN_POINT('Origin',(182.431848717848,13.375,25.5));
#101621=CARTESIAN_POINT('',(182.431848717848,13.375,25.5));
#101622=CARTESIAN_POINT('',(182.431848717848,13.375,25.5));
#101623=CARTESIAN_POINT('',(182.431848717848,13.375,31.5));
#101624=CARTESIAN_POINT('',(182.431848717848,13.375,31.5));
#101625=CARTESIAN_POINT('',(182.431848717848,13.375,25.5));
#101626=CARTESIAN_POINT('Origin',(182.823116719684,14.45,25.5));
#101627=CARTESIAN_POINT('',(182.823116719684,14.45,25.5));
#101628=CARTESIAN_POINT('',(182.823116719684,14.45,25.5));
#101629=CARTESIAN_POINT('',(182.823116719684,14.45,31.5));
#101630=CARTESIAN_POINT('',(182.823116719684,14.45,31.5));
#101631=CARTESIAN_POINT('',(182.823116719684,14.45,25.5));
#101632=CARTESIAN_POINT('Origin',(183.260941672242,14.45,25.5));
#101633=CARTESIAN_POINT('',(183.260941672242,14.45,25.5));
#101634=CARTESIAN_POINT('',(183.260941672242,14.45,25.5));
#101635=CARTESIAN_POINT('',(183.260941672242,14.45,31.5));
#101636=CARTESIAN_POINT('',(183.260941672242,14.45,31.5));
#101637=CARTESIAN_POINT('',(183.260941672242,14.45,25.5));
#101638=CARTESIAN_POINT('Origin',(183.652209674078,13.375,25.5));
#101639=CARTESIAN_POINT('',(183.652209674078,13.375,25.5));
#101640=CARTESIAN_POINT('',(183.652209674078,13.375,25.5));
#101641=CARTESIAN_POINT('',(183.652209674078,13.375,31.5));
#101642=CARTESIAN_POINT('',(183.652209674078,13.375,31.5));
#101643=CARTESIAN_POINT('',(183.652209674078,13.375,25.5));
#101644=CARTESIAN_POINT('Origin',(184.002645044642,13.375,25.5));
#101645=CARTESIAN_POINT('',(184.002645044642,13.375,25.5));
#101646=CARTESIAN_POINT('',(184.002645044642,13.375,25.5));
#101647=CARTESIAN_POINT('',(184.002645044642,13.375,31.5));
#101648=CARTESIAN_POINT('',(184.002645044642,13.375,31.5));
#101649=CARTESIAN_POINT('',(184.002645044642,13.375,25.5));
#101650=CARTESIAN_POINT('Origin',(184.393913046479,14.45,25.5));
#101651=CARTESIAN_POINT('',(184.393913046479,14.45,25.5));
#101652=CARTESIAN_POINT('',(184.393913046479,14.45,25.5));
#101653=CARTESIAN_POINT('',(184.393913046479,14.45,31.5));
#101654=CARTESIAN_POINT('',(184.393913046479,14.45,31.5));
#101655=CARTESIAN_POINT('',(184.393913046479,14.45,25.5));
#101656=CARTESIAN_POINT('Origin',(184.831737999037,14.45,25.5));
#101657=CARTESIAN_POINT('',(184.831737999037,14.45,25.5));
#101658=CARTESIAN_POINT('',(184.831737999037,14.45,25.5));
#101659=CARTESIAN_POINT('',(184.831737999037,14.45,31.5));
#101660=CARTESIAN_POINT('',(184.831737999037,14.45,31.5));
#101661=CARTESIAN_POINT('',(184.831737999037,14.45,25.5));
#101662=CARTESIAN_POINT('Origin',(185.223006000873,13.375,25.5));
#101663=CARTESIAN_POINT('',(185.223006000873,13.375,25.5));
#101664=CARTESIAN_POINT('',(185.223006000873,13.375,25.5));
#101665=CARTESIAN_POINT('',(185.223006000873,13.375,31.5));
#101666=CARTESIAN_POINT('',(185.223006000873,13.375,31.5));
#101667=CARTESIAN_POINT('',(185.223006000873,13.375,25.5));
#101668=CARTESIAN_POINT('Origin',(185.573441371437,13.375,25.5));
#101669=CARTESIAN_POINT('',(185.573441371437,13.375,25.5));
#101670=CARTESIAN_POINT('',(185.573441371437,13.375,25.5));
#101671=CARTESIAN_POINT('',(185.573441371437,13.375,31.5));
#101672=CARTESIAN_POINT('',(185.573441371437,13.375,31.5));
#101673=CARTESIAN_POINT('',(185.573441371437,13.375,25.5));
#101674=CARTESIAN_POINT('Origin',(185.964709373274,14.45,25.5));
#101675=CARTESIAN_POINT('',(185.964709373274,14.45,25.5));
#101676=CARTESIAN_POINT('',(185.964709373274,14.45,25.5));
#101677=CARTESIAN_POINT('',(185.964709373274,14.45,31.5));
#101678=CARTESIAN_POINT('',(185.964709373274,14.45,31.5));
#101679=CARTESIAN_POINT('',(185.964709373274,14.45,25.5));
#101680=CARTESIAN_POINT('Origin',(186.402534325831,14.45,25.5));
#101681=CARTESIAN_POINT('',(186.402534325831,14.45,25.5));
#101682=CARTESIAN_POINT('',(186.402534325831,14.45,25.5));
#101683=CARTESIAN_POINT('',(186.402534325831,14.45,31.5));
#101684=CARTESIAN_POINT('',(186.402534325831,14.45,31.5));
#101685=CARTESIAN_POINT('',(186.402534325831,14.45,25.5));
#101686=CARTESIAN_POINT('Origin',(186.793802327668,13.375,25.5));
#101687=CARTESIAN_POINT('',(186.793802327668,13.375,25.5));
#101688=CARTESIAN_POINT('',(186.793802327668,13.375,25.5));
#101689=CARTESIAN_POINT('',(186.793802327668,13.375,31.5));
#101690=CARTESIAN_POINT('',(186.793802327668,13.375,31.5));
#101691=CARTESIAN_POINT('',(186.793802327668,13.375,25.5));
#101692=CARTESIAN_POINT('Origin',(187.144237698232,13.375,25.5));
#101693=CARTESIAN_POINT('',(187.144237698232,13.375,25.5));
#101694=CARTESIAN_POINT('',(187.144237698232,13.375,25.5));
#101695=CARTESIAN_POINT('',(187.144237698232,13.375,31.5));
#101696=CARTESIAN_POINT('',(187.144237698232,13.375,31.5));
#101697=CARTESIAN_POINT('',(187.144237698232,13.375,25.5));
#101698=CARTESIAN_POINT('Origin',(187.535505700068,14.45,25.5));
#101699=CARTESIAN_POINT('',(187.535505700068,14.45,25.5));
#101700=CARTESIAN_POINT('',(187.535505700068,14.45,25.5));
#101701=CARTESIAN_POINT('',(187.535505700068,14.45,31.5));
#101702=CARTESIAN_POINT('',(187.535505700068,14.45,31.5));
#101703=CARTESIAN_POINT('',(187.535505700068,14.45,25.5));
#101704=CARTESIAN_POINT('Origin',(187.973330652626,14.45,25.5));
#101705=CARTESIAN_POINT('',(187.973330652626,14.45,25.5));
#101706=CARTESIAN_POINT('',(187.973330652626,14.45,25.5));
#101707=CARTESIAN_POINT('',(187.973330652626,14.45,31.5));
#101708=CARTESIAN_POINT('',(187.973330652626,14.45,31.5));
#101709=CARTESIAN_POINT('',(187.973330652626,14.45,25.5));
#101710=CARTESIAN_POINT('Origin',(188.364598654462,13.375,25.5));
#101711=CARTESIAN_POINT('',(188.364598654462,13.375,25.5));
#101712=CARTESIAN_POINT('',(188.364598654462,13.375,25.5));
#101713=CARTESIAN_POINT('',(188.364598654462,13.375,31.5));
#101714=CARTESIAN_POINT('',(188.364598654462,13.375,31.5));
#101715=CARTESIAN_POINT('',(188.364598654462,13.375,25.5));
#101716=CARTESIAN_POINT('Origin',(188.715034025027,13.375,25.5));
#101717=CARTESIAN_POINT('',(188.715034025027,13.375,25.5));
#101718=CARTESIAN_POINT('',(188.715034025027,13.375,25.5));
#101719=CARTESIAN_POINT('',(188.715034025027,13.375,31.5));
#101720=CARTESIAN_POINT('',(188.715034025027,13.375,31.5));
#101721=CARTESIAN_POINT('',(188.715034025027,13.375,25.5));
#101722=CARTESIAN_POINT('Origin',(189.106302026863,14.45,25.5));
#101723=CARTESIAN_POINT('',(189.106302026863,14.45,25.5));
#101724=CARTESIAN_POINT('',(189.106302026863,14.45,25.5));
#101725=CARTESIAN_POINT('',(189.106302026863,14.45,31.5));
#101726=CARTESIAN_POINT('',(189.106302026863,14.45,31.5));
#101727=CARTESIAN_POINT('',(189.106302026863,14.45,25.5));
#101728=CARTESIAN_POINT('Origin',(189.544126979421,14.45,25.5));
#101729=CARTESIAN_POINT('',(189.544126979421,14.45,25.5));
#101730=CARTESIAN_POINT('',(189.544126979421,14.45,25.5));
#101731=CARTESIAN_POINT('',(189.544126979421,14.45,31.5));
#101732=CARTESIAN_POINT('',(189.544126979421,14.45,31.5));
#101733=CARTESIAN_POINT('',(189.544126979421,14.45,25.5));
#101734=CARTESIAN_POINT('Origin',(189.935394981257,13.375,25.5));
#101735=CARTESIAN_POINT('',(189.935394981257,13.375,25.5));
#101736=CARTESIAN_POINT('',(189.935394981257,13.375,25.5));
#101737=CARTESIAN_POINT('',(189.935394981257,13.375,31.5));
#101738=CARTESIAN_POINT('',(189.935394981257,13.375,31.5));
#101739=CARTESIAN_POINT('',(189.935394981257,13.375,25.5));
#101740=CARTESIAN_POINT('Origin',(190.285830351822,13.375,25.5));
#101741=CARTESIAN_POINT('',(190.285830351822,13.375,25.5));
#101742=CARTESIAN_POINT('',(190.285830351822,13.375,25.5));
#101743=CARTESIAN_POINT('',(190.285830351822,13.375,31.5));
#101744=CARTESIAN_POINT('',(190.285830351822,13.375,31.5));
#101745=CARTESIAN_POINT('',(190.285830351822,13.375,25.5));
#101746=CARTESIAN_POINT('Origin',(190.677098353658,14.45,25.5));
#101747=CARTESIAN_POINT('',(190.677098353658,14.45,25.5));
#101748=CARTESIAN_POINT('',(190.677098353658,14.45,25.5));
#101749=CARTESIAN_POINT('',(190.677098353658,14.45,31.5));
#101750=CARTESIAN_POINT('',(190.677098353658,14.45,31.5));
#101751=CARTESIAN_POINT('',(190.677098353658,14.45,25.5));
#101752=CARTESIAN_POINT('Origin',(191.114923306216,14.45,25.5));
#101753=CARTESIAN_POINT('',(191.114923306216,14.45,25.5));
#101754=CARTESIAN_POINT('',(191.114923306216,14.45,25.5));
#101755=CARTESIAN_POINT('',(191.114923306216,14.45,31.5));
#101756=CARTESIAN_POINT('',(191.114923306216,14.45,31.5));
#101757=CARTESIAN_POINT('',(191.114923306216,14.45,25.5));
#101758=CARTESIAN_POINT('Origin',(191.506191308052,13.375,25.5));
#101759=CARTESIAN_POINT('',(191.506191308052,13.375,25.5));
#101760=CARTESIAN_POINT('',(191.506191308052,13.375,25.5));
#101761=CARTESIAN_POINT('',(191.506191308052,13.375,31.5));
#101762=CARTESIAN_POINT('',(191.506191308052,13.375,31.5));
#101763=CARTESIAN_POINT('',(191.506191308052,13.375,25.5));
#101764=CARTESIAN_POINT('Origin',(191.856626678617,13.375,25.5));
#101765=CARTESIAN_POINT('',(191.856626678617,13.375,25.5));
#101766=CARTESIAN_POINT('',(191.856626678617,13.375,25.5));
#101767=CARTESIAN_POINT('',(191.856626678617,13.375,31.5));
#101768=CARTESIAN_POINT('',(191.856626678617,13.375,31.5));
#101769=CARTESIAN_POINT('',(191.856626678617,13.375,25.5));
#101770=CARTESIAN_POINT('Origin',(192.247894680453,14.45,25.5));
#101771=CARTESIAN_POINT('',(192.247894680453,14.45,25.5));
#101772=CARTESIAN_POINT('',(192.247894680453,14.45,25.5));
#101773=CARTESIAN_POINT('',(192.247894680453,14.45,31.5));
#101774=CARTESIAN_POINT('',(192.247894680453,14.45,31.5));
#101775=CARTESIAN_POINT('',(192.247894680453,14.45,25.5));
#101776=CARTESIAN_POINT('Origin',(192.685719633011,14.45,25.5));
#101777=CARTESIAN_POINT('',(192.685719633011,14.45,25.5));
#101778=CARTESIAN_POINT('',(192.685719633011,14.45,25.5));
#101779=CARTESIAN_POINT('',(192.685719633011,14.45,31.5));
#101780=CARTESIAN_POINT('',(192.685719633011,14.45,31.5));
#101781=CARTESIAN_POINT('',(192.685719633011,14.45,25.5));
#101782=CARTESIAN_POINT('Origin',(193.076987634847,13.375,25.5));
#101783=CARTESIAN_POINT('',(193.076987634847,13.375,25.5));
#101784=CARTESIAN_POINT('',(193.076987634847,13.375,25.5));
#101785=CARTESIAN_POINT('',(193.076987634847,13.375,31.5));
#101786=CARTESIAN_POINT('',(193.076987634847,13.375,31.5));
#101787=CARTESIAN_POINT('',(193.076987634847,13.375,25.5));
#101788=CARTESIAN_POINT('Origin',(193.427423005412,13.375,25.5));
#101789=CARTESIAN_POINT('',(193.427423005412,13.375,25.5));
#101790=CARTESIAN_POINT('',(193.427423005412,13.375,25.5));
#101791=CARTESIAN_POINT('',(193.427423005412,13.375,31.5));
#101792=CARTESIAN_POINT('',(193.427423005412,13.375,31.5));
#101793=CARTESIAN_POINT('',(193.427423005412,13.375,25.5));
#101794=CARTESIAN_POINT('Origin',(193.818691007248,14.45,25.5));
#101795=CARTESIAN_POINT('',(193.818691007248,14.45,25.5));
#101796=CARTESIAN_POINT('',(193.818691007248,14.45,25.5));
#101797=CARTESIAN_POINT('',(193.818691007248,14.45,31.5));
#101798=CARTESIAN_POINT('',(193.818691007248,14.45,31.5));
#101799=CARTESIAN_POINT('',(193.818691007248,14.45,25.5));
#101800=CARTESIAN_POINT('Origin',(194.256515959806,14.45,25.5));
#101801=CARTESIAN_POINT('',(194.256515959806,14.45,25.5));
#101802=CARTESIAN_POINT('',(194.256515959806,14.45,25.5));
#101803=CARTESIAN_POINT('',(194.256515959806,14.45,31.5));
#101804=CARTESIAN_POINT('',(194.256515959806,14.45,31.5));
#101805=CARTESIAN_POINT('',(194.256515959806,14.45,25.5));
#101806=CARTESIAN_POINT('Origin',(194.647783961642,13.375,25.5));
#101807=CARTESIAN_POINT('',(194.647783961642,13.375,25.5));
#101808=CARTESIAN_POINT('',(194.647783961642,13.375,25.5));
#101809=CARTESIAN_POINT('',(194.647783961642,13.375,31.5));
#101810=CARTESIAN_POINT('',(194.647783961642,13.375,31.5));
#101811=CARTESIAN_POINT('',(194.647783961642,13.375,25.5));
#101812=CARTESIAN_POINT('Origin',(194.998219332207,13.375,25.5));
#101813=CARTESIAN_POINT('',(194.998219332207,13.375,25.5));
#101814=CARTESIAN_POINT('',(194.998219332207,13.375,25.5));
#101815=CARTESIAN_POINT('',(194.998219332207,13.375,31.5));
#101816=CARTESIAN_POINT('',(194.998219332207,13.375,31.5));
#101817=CARTESIAN_POINT('',(194.998219332207,13.375,25.5));
#101818=CARTESIAN_POINT('Origin',(195.389487334043,14.45,25.5));
#101819=CARTESIAN_POINT('',(195.389487334043,14.45,25.5));
#101820=CARTESIAN_POINT('',(195.389487334043,14.45,25.5));
#101821=CARTESIAN_POINT('',(195.389487334043,14.45,31.5));
#101822=CARTESIAN_POINT('',(195.389487334043,14.45,31.5));
#101823=CARTESIAN_POINT('',(195.389487334043,14.45,25.5));
#101824=CARTESIAN_POINT('Origin',(195.827312286601,14.45,25.5));
#101825=CARTESIAN_POINT('',(195.827312286601,14.45,25.5));
#101826=CARTESIAN_POINT('',(195.827312286601,14.45,25.5));
#101827=CARTESIAN_POINT('',(195.827312286601,14.45,31.5));
#101828=CARTESIAN_POINT('',(195.827312286601,14.45,31.5));
#101829=CARTESIAN_POINT('',(195.827312286601,14.45,25.5));
#101830=CARTESIAN_POINT('Origin',(196.218580288437,13.375,25.5));
#101831=CARTESIAN_POINT('',(196.218580288437,13.375,25.5));
#101832=CARTESIAN_POINT('',(196.218580288437,13.375,25.5));
#101833=CARTESIAN_POINT('',(196.218580288437,13.375,31.5));
#101834=CARTESIAN_POINT('',(196.218580288437,13.375,31.5));
#101835=CARTESIAN_POINT('',(196.218580288437,13.375,25.5));
#101836=CARTESIAN_POINT('Origin',(196.569015659002,13.375,25.5));
#101837=CARTESIAN_POINT('',(196.569015659002,13.375,25.5));
#101838=CARTESIAN_POINT('',(196.569015659002,13.375,25.5));
#101839=CARTESIAN_POINT('',(196.569015659002,13.375,31.5));
#101840=CARTESIAN_POINT('',(196.569015659002,13.375,31.5));
#101841=CARTESIAN_POINT('',(196.569015659002,13.375,25.5));
#101842=CARTESIAN_POINT('Origin',(196.960283660838,14.45,25.5));
#101843=CARTESIAN_POINT('',(196.960283660838,14.45,25.5));
#101844=CARTESIAN_POINT('',(196.960283660838,14.45,25.5));
#101845=CARTESIAN_POINT('',(196.960283660838,14.45,31.5));
#101846=CARTESIAN_POINT('',(196.960283660838,14.45,31.5));
#101847=CARTESIAN_POINT('',(196.960283660838,14.45,25.5));
#101848=CARTESIAN_POINT('Origin',(197.398108613396,14.45,25.5));
#101849=CARTESIAN_POINT('',(197.398108613396,14.45,25.5));
#101850=CARTESIAN_POINT('',(197.398108613396,14.45,25.5));
#101851=CARTESIAN_POINT('',(197.398108613396,14.45,31.5));
#101852=CARTESIAN_POINT('',(197.398108613396,14.45,31.5));
#101853=CARTESIAN_POINT('',(197.398108613396,14.45,25.5));
#101854=CARTESIAN_POINT('Origin',(197.789376615232,13.375,25.5));
#101855=CARTESIAN_POINT('',(197.789376615232,13.375,25.5));
#101856=CARTESIAN_POINT('',(197.789376615232,13.375,25.5));
#101857=CARTESIAN_POINT('',(197.789376615232,13.375,31.5));
#101858=CARTESIAN_POINT('',(197.789376615232,13.375,31.5));
#101859=CARTESIAN_POINT('',(197.789376615232,13.375,25.5));
#101860=CARTESIAN_POINT('Origin',(198.139811985797,13.375,25.5));
#101861=CARTESIAN_POINT('',(198.139811985797,13.375,25.5));
#101862=CARTESIAN_POINT('',(198.139811985797,13.375,25.5));
#101863=CARTESIAN_POINT('',(198.139811985797,13.375,31.5));
#101864=CARTESIAN_POINT('',(198.139811985797,13.375,31.5));
#101865=CARTESIAN_POINT('',(198.139811985797,13.375,25.5));
#101866=CARTESIAN_POINT('Origin',(198.531079987633,14.45,25.5));
#101867=CARTESIAN_POINT('',(198.531079987633,14.45,25.5));
#101868=CARTESIAN_POINT('',(198.531079987633,14.45,25.5));
#101869=CARTESIAN_POINT('',(198.531079987633,14.45,31.5));
#101870=CARTESIAN_POINT('',(198.531079987633,14.45,31.5));
#101871=CARTESIAN_POINT('',(198.531079987633,14.45,25.5));
#101872=CARTESIAN_POINT('Origin',(198.968904940191,14.45,25.5));
#101873=CARTESIAN_POINT('',(198.968904940191,14.45,25.5));
#101874=CARTESIAN_POINT('',(198.968904940191,14.45,25.5));
#101875=CARTESIAN_POINT('',(198.968904940191,14.45,31.5));
#101876=CARTESIAN_POINT('',(198.968904940191,14.45,31.5));
#101877=CARTESIAN_POINT('',(198.968904940191,14.45,25.5));
#101878=CARTESIAN_POINT('Origin',(199.360172942027,13.375,25.5));
#101879=CARTESIAN_POINT('',(199.360172942027,13.375,25.5));
#101880=CARTESIAN_POINT('',(199.360172942027,13.375,25.5));
#101881=CARTESIAN_POINT('',(199.360172942027,13.375,31.5));
#101882=CARTESIAN_POINT('',(199.360172942027,13.375,31.5));
#101883=CARTESIAN_POINT('',(199.360172942027,13.375,25.5));
#101884=CARTESIAN_POINT('Origin',(199.710608312591,13.375,25.5));
#101885=CARTESIAN_POINT('',(199.710608312591,13.375,25.5));
#101886=CARTESIAN_POINT('',(199.710608312591,13.375,25.5));
#101887=CARTESIAN_POINT('',(199.710608312591,13.375,31.5));
#101888=CARTESIAN_POINT('',(199.710608312591,13.375,31.5));
#101889=CARTESIAN_POINT('',(199.710608312591,13.375,25.5));
#101890=CARTESIAN_POINT('Origin',(200.101876314428,14.45,25.5));
#101891=CARTESIAN_POINT('',(200.101876314428,14.45,25.5));
#101892=CARTESIAN_POINT('',(200.101876314428,14.45,25.5));
#101893=CARTESIAN_POINT('',(200.101876314428,14.45,31.5));
#101894=CARTESIAN_POINT('',(200.101876314428,14.45,31.5));
#101895=CARTESIAN_POINT('',(200.101876314428,14.45,25.5));
#101896=CARTESIAN_POINT('Origin',(200.539701266986,14.45,25.5));
#101897=CARTESIAN_POINT('',(200.539701266986,14.45,25.5));
#101898=CARTESIAN_POINT('',(200.539701266986,14.45,25.5));
#101899=CARTESIAN_POINT('',(200.539701266986,14.45,31.5));
#101900=CARTESIAN_POINT('',(200.539701266986,14.45,31.5));
#101901=CARTESIAN_POINT('',(200.539701266986,14.45,25.5));
#101902=CARTESIAN_POINT('Origin',(200.930969268822,13.375,25.5));
#101903=CARTESIAN_POINT('',(200.930969268822,13.375,25.5));
#101904=CARTESIAN_POINT('',(200.930969268822,13.375,25.5));
#101905=CARTESIAN_POINT('',(200.930969268822,13.375,31.5));
#101906=CARTESIAN_POINT('',(200.930969268822,13.375,31.5));
#101907=CARTESIAN_POINT('',(200.930969268822,13.375,25.5));
#101908=CARTESIAN_POINT('Origin',(201.281404639386,13.375,25.5));
#101909=CARTESIAN_POINT('',(201.281404639386,13.375,25.5));
#101910=CARTESIAN_POINT('',(201.281404639386,13.375,25.5));
#101911=CARTESIAN_POINT('',(201.281404639386,13.375,31.5));
#101912=CARTESIAN_POINT('',(201.281404639386,13.375,31.5));
#101913=CARTESIAN_POINT('',(201.281404639386,13.375,25.5));
#101914=CARTESIAN_POINT('Origin',(201.672672641223,14.45,25.5));
#101915=CARTESIAN_POINT('',(201.672672641223,14.45,25.5));
#101916=CARTESIAN_POINT('',(201.672672641223,14.45,25.5));
#101917=CARTESIAN_POINT('',(201.672672641223,14.45,31.5));
#101918=CARTESIAN_POINT('',(201.672672641223,14.45,31.5));
#101919=CARTESIAN_POINT('',(201.672672641223,14.45,25.5));
#101920=CARTESIAN_POINT('Origin',(202.11049759378,14.45,25.5));
#101921=CARTESIAN_POINT('',(202.11049759378,14.45,25.5));
#101922=CARTESIAN_POINT('',(202.11049759378,14.45,25.5));
#101923=CARTESIAN_POINT('',(202.11049759378,14.45,31.5));
#101924=CARTESIAN_POINT('',(202.11049759378,14.45,31.5));
#101925=CARTESIAN_POINT('',(202.11049759378,14.45,25.5));
#101926=CARTESIAN_POINT('Origin',(202.501765595617,13.375,25.5));
#101927=CARTESIAN_POINT('',(202.501765595617,13.375,25.5));
#101928=CARTESIAN_POINT('',(202.501765595617,13.375,25.5));
#101929=CARTESIAN_POINT('',(202.501765595617,13.375,31.5));
#101930=CARTESIAN_POINT('',(202.501765595617,13.375,31.5));
#101931=CARTESIAN_POINT('',(202.501765595617,13.375,25.5));
#101932=CARTESIAN_POINT('Origin',(202.852200966181,13.375,25.5));
#101933=CARTESIAN_POINT('',(202.852200966181,13.375,25.5));
#101934=CARTESIAN_POINT('',(202.852200966181,13.375,25.5));
#101935=CARTESIAN_POINT('',(202.852200966181,13.375,31.5));
#101936=CARTESIAN_POINT('',(202.852200966181,13.375,31.5));
#101937=CARTESIAN_POINT('',(202.852200966181,13.375,25.5));
#101938=CARTESIAN_POINT('Origin',(203.243468968017,14.45,25.5));
#101939=CARTESIAN_POINT('',(203.243468968017,14.45,25.5));
#101940=CARTESIAN_POINT('',(203.243468968017,14.45,25.5));
#101941=CARTESIAN_POINT('',(203.243468968017,14.45,31.5));
#101942=CARTESIAN_POINT('',(203.243468968017,14.45,31.5));
#101943=CARTESIAN_POINT('',(203.243468968017,14.45,25.5));
#101944=CARTESIAN_POINT('Origin',(203.681293920575,14.45,25.5));
#101945=CARTESIAN_POINT('',(203.681293920575,14.45,25.5));
#101946=CARTESIAN_POINT('',(203.681293920575,14.45,25.5));
#101947=CARTESIAN_POINT('',(203.681293920575,14.45,31.5));
#101948=CARTESIAN_POINT('',(203.681293920575,14.45,31.5));
#101949=CARTESIAN_POINT('',(203.681293920575,14.45,25.5));
#101950=CARTESIAN_POINT('Origin',(204.072561922411,13.375,25.5));
#101951=CARTESIAN_POINT('',(204.072561922411,13.375,25.5));
#101952=CARTESIAN_POINT('',(204.072561922411,13.375,25.5));
#101953=CARTESIAN_POINT('',(204.072561922411,13.375,31.5));
#101954=CARTESIAN_POINT('',(204.072561922411,13.375,31.5));
#101955=CARTESIAN_POINT('',(204.072561922411,13.375,25.5));
#101956=CARTESIAN_POINT('Origin',(204.422997292976,13.375,25.5));
#101957=CARTESIAN_POINT('',(204.422997292976,13.375,25.5));
#101958=CARTESIAN_POINT('',(204.422997292976,13.375,25.5));
#101959=CARTESIAN_POINT('',(204.422997292976,13.375,31.5));
#101960=CARTESIAN_POINT('',(204.422997292976,13.375,31.5));
#101961=CARTESIAN_POINT('',(204.422997292976,13.375,25.5));
#101962=CARTESIAN_POINT('Origin',(204.814265294812,14.45,25.5));
#101963=CARTESIAN_POINT('',(204.814265294812,14.45,25.5));
#101964=CARTESIAN_POINT('',(204.814265294812,14.45,25.5));
#101965=CARTESIAN_POINT('',(204.814265294812,14.45,31.5));
#101966=CARTESIAN_POINT('',(204.814265294812,14.45,31.5));
#101967=CARTESIAN_POINT('',(204.814265294812,14.45,25.5));
#101968=CARTESIAN_POINT('Origin',(205.25209024737,14.45,25.5));
#101969=CARTESIAN_POINT('',(205.25209024737,14.45,25.5));
#101970=CARTESIAN_POINT('',(205.25209024737,14.45,25.5));
#101971=CARTESIAN_POINT('',(205.25209024737,14.45,31.5));
#101972=CARTESIAN_POINT('',(205.25209024737,14.45,31.5));
#101973=CARTESIAN_POINT('',(205.25209024737,14.45,25.5));
#101974=CARTESIAN_POINT('Origin',(205.643358249206,13.375,25.5));
#101975=CARTESIAN_POINT('',(205.643358249206,13.375,25.5));
#101976=CARTESIAN_POINT('',(205.643358249206,13.375,25.5));
#101977=CARTESIAN_POINT('',(205.643358249206,13.375,31.5));
#101978=CARTESIAN_POINT('',(205.643358249206,13.375,31.5));
#101979=CARTESIAN_POINT('',(205.643358249206,13.375,25.5));
#101980=CARTESIAN_POINT('Origin',(205.993793619771,13.375,25.5));
#101981=CARTESIAN_POINT('',(205.993793619771,13.375,25.5));
#101982=CARTESIAN_POINT('',(205.993793619771,13.375,25.5));
#101983=CARTESIAN_POINT('',(205.993793619771,13.375,31.5));
#101984=CARTESIAN_POINT('',(205.993793619771,13.375,31.5));
#101985=CARTESIAN_POINT('',(205.993793619771,13.375,25.5));
#101986=CARTESIAN_POINT('Origin',(206.385061621607,14.45,25.5));
#101987=CARTESIAN_POINT('',(206.385061621607,14.45,25.5));
#101988=CARTESIAN_POINT('',(206.385061621607,14.45,25.5));
#101989=CARTESIAN_POINT('',(206.385061621607,14.45,31.5));
#101990=CARTESIAN_POINT('',(206.385061621607,14.45,31.5));
#101991=CARTESIAN_POINT('',(206.385061621607,14.45,25.5));
#101992=CARTESIAN_POINT('Origin',(206.822886574165,14.45,25.5));
#101993=CARTESIAN_POINT('',(206.822886574165,14.45,25.5));
#101994=CARTESIAN_POINT('',(206.822886574165,14.45,25.5));
#101995=CARTESIAN_POINT('',(206.822886574165,14.45,31.5));
#101996=CARTESIAN_POINT('',(206.822886574165,14.45,31.5));
#101997=CARTESIAN_POINT('',(206.822886574165,14.45,25.5));
#101998=CARTESIAN_POINT('Origin',(207.214154576001,13.375,25.5));
#101999=CARTESIAN_POINT('',(207.214154576001,13.375,25.5));
#102000=CARTESIAN_POINT('',(207.214154576001,13.375,25.5));
#102001=CARTESIAN_POINT('',(207.214154576001,13.375,31.5));
#102002=CARTESIAN_POINT('',(207.214154576001,13.375,31.5));
#102003=CARTESIAN_POINT('',(207.214154576001,13.375,25.5));
#102004=CARTESIAN_POINT('Origin',(207.564589946566,13.375,25.5));
#102005=CARTESIAN_POINT('',(207.564589946566,13.375,25.5));
#102006=CARTESIAN_POINT('',(207.564589946566,13.375,25.5));
#102007=CARTESIAN_POINT('',(207.564589946566,13.375,31.5));
#102008=CARTESIAN_POINT('',(207.564589946566,13.375,31.5));
#102009=CARTESIAN_POINT('',(207.564589946566,13.375,25.5));
#102010=CARTESIAN_POINT('Origin',(207.955857948402,14.45,25.5));
#102011=CARTESIAN_POINT('',(207.955857948402,14.45,25.5));
#102012=CARTESIAN_POINT('',(207.955857948402,14.45,31.5));
#102013=CARTESIAN_POINT('Origin',(2.,14.45,25.5));
#102014=CARTESIAN_POINT('',(2.,14.45,31.5));
#102015=CARTESIAN_POINT('',(2.,14.45,25.5));
#102016=CARTESIAN_POINT('Origin',(110.,11.975,31.5));
#102017=CARTESIAN_POINT('Origin',(110.,11.975,25.5));
#102018=CARTESIAN_POINT('',(0.,0.,0.));
#102019=CARTESIAN_POINT('Origin',(107.825160250462,5.69826049129303,6.4));
#102020=CARTESIAN_POINT('',(107.557248030597,6.1204252013845,6.4));
#102021=CARTESIAN_POINT('',(108.022872954966,6.15750953753911,6.4));
#102022=CARTESIAN_POINT('Origin',(107.825160250462,5.69826049129303,6.4));
#102023=CARTESIAN_POINT('',(108.022872954966,6.15750953753911,8.4));
#102024=CARTESIAN_POINT('',(108.022872954966,6.15750953753911,6.4));
#102025=CARTESIAN_POINT('',(107.557248030597,6.1204252013845,8.4));
#102026=CARTESIAN_POINT('Origin',(107.825160250462,5.69826049129303,8.4));
#102027=CARTESIAN_POINT('',(107.557248030597,6.1204252013845,6.4));
#102028=CARTESIAN_POINT('Origin',(110.,10.75,6.4));
#102029=CARTESIAN_POINT('',(105.002771567388,10.9164571785702,6.4));
#102030=CARTESIAN_POINT('Origin',(110.,10.75,6.4));
#102031=CARTESIAN_POINT('',(105.002771567388,10.9164571785702,8.4));
#102032=CARTESIAN_POINT('',(105.002771567388,10.9164571785702,6.4));
#102033=CARTESIAN_POINT('Origin',(110.,10.75,8.4));
#102034=CARTESIAN_POINT('Origin',(104.503048724127,10.9331028964272,6.4));
#102035=CARTESIAN_POINT('',(104.770960943993,10.5109381863358,6.4));
#102036=CARTESIAN_POINT('Origin',(104.503048724127,10.9331028964272,6.4));
#102037=CARTESIAN_POINT('',(104.770960943993,10.5109381863358,8.4));
#102038=CARTESIAN_POINT('',(104.770960943993,10.5109381863358,6.4));
#102039=CARTESIAN_POINT('Origin',(104.503048724127,10.9331028964272,8.4));
#102040=CARTESIAN_POINT('Origin',(105.000867940784,10.6568407035301,6.4));
#102041=CARTESIAN_POINT('',(95.6068564566982,4.69525649247563,6.4));
#102042=CARTESIAN_POINT('',(95.6068564566982,4.69525649247563,6.4));
#102043=CARTESIAN_POINT('',(95.6068564566982,4.69525649247563,7.33954966094489));
#102044=CARTESIAN_POINT('',(95.6068564566982,4.69525649247563,6.4));
#102045=CARTESIAN_POINT('',(96.0290211667896,4.96316871234137,7.81341546108985));
#102046=CARTESIAN_POINT('',(98.0390228445825,6.23874670017144,10.0695752740066));
#102047=CARTESIAN_POINT('',(96.0290211667896,4.96316871234136,8.4));
#102048=CARTESIAN_POINT('',(96.0290211667896,4.96316871234137,6.4));
#102049=CARTESIAN_POINT('',(95.6068564566982,4.69525649247563,8.4));
#102050=CARTESIAN_POINT('Origin',(96.2969333866554,4.5410040022499,6.4));
#102051=CARTESIAN_POINT('',(95.8747686765639,4.27309178238416,8.4));
#102052=CARTESIAN_POINT('Origin',(96.2969333866554,4.5410040022499,8.4));
#102053=CARTESIAN_POINT('',(95.8747686765639,4.27309178238416,7.64027218795995));
#102054=CARTESIAN_POINT('Origin',(96.2969333866554,4.5410040022499,8.11413798810492));
#102055=CARTESIAN_POINT('',(95.8747686765639,4.27309178238416,6.4));
#102056=CARTESIAN_POINT('Origin',(95.6068564566982,4.69525649247563,6.4));
#102057=CARTESIAN_POINT('',(95.7511326297006,4.46791221986573,7.50149485088472));
#102058=CARTESIAN_POINT('',(95.8150253859024,4.36723272524474,7.57321233772642));
#102059=CARTESIAN_POINT('',(95.7511326297006,4.46791221986573,6.4));
#102060=CARTESIAN_POINT('',(98.3931435433018,0.304743507524373,6.4));
#102061=CARTESIAN_POINT('',(95.7511326297006,4.46791221986573,5.2163000524998));
#102062=CARTESIAN_POINT('Origin',(95.6068564566982,4.69525649247563,6.4));
#102063=CARTESIAN_POINT('',(96.2533349608981,3.67656309191811,8.06520020999922));
#102064=CARTESIAN_POINT('',(95.8150253859024,4.36723272524474,7.57321233772642));
#102065=CARTESIAN_POINT('',(97.7466650391019,1.32343690808192,6.73479979000078));
#102066=CARTESIAN_POINT('',(96.4723671690011,3.33142143066498,7.87006549336387));
#102067=CARTESIAN_POINT('',(97.4483935532906,1.79344046148143,6.4));
#102068=CARTESIAN_POINT('',(95.0971229410666,5.49847294134964,3.76077719575972));
#102069=CARTESIAN_POINT('',(98.1252313234361,0.726908217615838,6.4));
#102070=CARTESIAN_POINT('',(98.3931435433018,0.304743507524373,6.4));
#102071=CARTESIAN_POINT('',(98.1252313234361,0.726908217615838,8.4));
#102072=CARTESIAN_POINT('',(98.1252313234361,0.726908217615836,6.4));
#102073=CARTESIAN_POINT('',(98.3931435433018,0.304743507524373,8.4));
#102074=CARTESIAN_POINT('Origin',(98.5473960335276,0.99482043748158,6.4));
#102075=CARTESIAN_POINT('',(98.8153082533933,0.572655727390118,8.4));
#102076=CARTESIAN_POINT('Origin',(98.5473960335276,0.99482043748158,8.4));
#102077=CARTESIAN_POINT('',(98.8153082533933,0.572655727390118,6.4));
#102078=CARTESIAN_POINT('Origin',(98.5473960335276,0.99482043748158,6.4));
#102079=CARTESIAN_POINT('',(98.8153082533933,0.572655727390115,6.4));
#102080=CARTESIAN_POINT('Origin',(105.303428228349,8.02737175376219,6.4));
#102081=CARTESIAN_POINT('',(97.4483935532906,3.7,6.4));
#102082=CARTESIAN_POINT('',(97.4483935532906,5.86368587688109,6.4));
#102083=CARTESIAN_POINT('',(95.3289679196091,3.7,6.4));
#102084=CARTESIAN_POINT('',(99.6517141141745,3.7,6.4));
#102085=CARTESIAN_POINT('Origin',(95.3289679196091,4.2,6.4));
#102086=CARTESIAN_POINT('',(111.393143543302,8.55474350752437,6.4));
#102087=CARTESIAN_POINT('',(107.85,10.75,6.4));
#102088=CARTESIAN_POINT('Origin',(110.,10.75,6.4));
#102089=CARTESIAN_POINT('Origin',(95.3289679196091,4.2,5.2163000524998));
#102090=CARTESIAN_POINT('',(95.3289679196091,3.7,7.02762905073977));
#102091=CARTESIAN_POINT('Origin',(95.3289679196091,4.2,7.02762905073977));
#102092=CARTESIAN_POINT('',(95.3289679196091,3.7,5.2163000524998));
#102093=CARTESIAN_POINT('Origin',(91.7466650391019,3.7,0.));
#102094=CARTESIAN_POINT('',(97.7466650391019,0.6,6.73479979000078));
#102095=CARTESIAN_POINT('',(97.7466650391019,3.7,6.73479979000078));
#102096=CARTESIAN_POINT('',(91.7466650391019,0.6,0.));
#102097=CARTESIAN_POINT('',(97.7466650391019,0.6,6.73479979000078));
#102098=CARTESIAN_POINT('',(91.7466650391019,3.7,0.));
#102099=CARTESIAN_POINT('',(91.7466650391019,3.7,0.));
#102100=CARTESIAN_POINT('',(97.7466650391019,3.7,6.73479979000078));
#102101=CARTESIAN_POINT('Origin',(97.7466650391019,3.7,6.73479979000078));
#102102=CARTESIAN_POINT('',(96.2533349608981,0.6,8.06520020999922));
#102103=CARTESIAN_POINT('',(96.2533349608981,3.7,8.06520020999922));
#102104=CARTESIAN_POINT('',(96.2533349608981,0.6,8.06520020999922));
#102105=CARTESIAN_POINT('Origin',(96.2533349608981,3.7,8.06520020999922));
#102106=CARTESIAN_POINT('',(90.2533349608981,3.7,1.33040041999844));
#102107=CARTESIAN_POINT('',(90.2533349608981,3.7,1.33040041999844));
#102108=CARTESIAN_POINT('',(90.2533349608981,0.6,1.33040041999844));
#102109=CARTESIAN_POINT('',(90.2533349608981,3.7,1.33040041999844));
#102110=CARTESIAN_POINT('',(90.2533349608981,0.6,1.33040041999844));
#102111=CARTESIAN_POINT('Origin',(90.2533349608981,3.7,1.33040041999844));
#102112=CARTESIAN_POINT('',(91.7466650391019,3.7,0.));
#102113=CARTESIAN_POINT('',(91.7466650391019,0.6,0.));
#102114=CARTESIAN_POINT('Origin',(94.,3.7,4.03260010499961));
#102115=CARTESIAN_POINT('Origin',(94.,0.6,4.03260010499961));
#102116=CARTESIAN_POINT('Origin',(110.,10.75,6.4));
#102117=CARTESIAN_POINT('',(107.85,10.75,8.4));
#102118=CARTESIAN_POINT('',(107.85,10.75,6.4));
#102119=CARTESIAN_POINT('Origin',(110.,10.75,8.4));
#102120=CARTESIAN_POINT('Origin',(98.3931435433018,0.304743507524372,6.4));
#102121=CARTESIAN_POINT('',(111.393143543302,8.55474350752437,8.4));
#102122=CARTESIAN_POINT('Origin',(105.303428228349,8.02737175376219,8.4));
#102123=CARTESIAN_POINT('',(0.,0.,0.));
#102124=CARTESIAN_POINT('Origin',(116.37,9.4,49.7));
#102125=CARTESIAN_POINT('',(116.37,8.6,49.7));
#102126=CARTESIAN_POINT('',(116.37,8.6,49.6));
#102127=CARTESIAN_POINT('',(116.37,8.6,49.1));
#102128=CARTESIAN_POINT('',(116.37,9.4,49.7));
#102129=CARTESIAN_POINT('',(116.37,9.8,49.7));
#102130=CARTESIAN_POINT('',(116.37,9.4,49.6));
#102131=CARTESIAN_POINT('',(116.37,9.4,49.7));
#102132=CARTESIAN_POINT('',(116.37,8.5,49.6));
#102133=CARTESIAN_POINT('Origin',(116.3,8.95,49.6));
#102134=CARTESIAN_POINT('',(116.23,8.6,49.6));
#102135=CARTESIAN_POINT('',(107.65,8.6,49.6));
#102136=CARTESIAN_POINT('',(116.23,9.4,49.6));
#102137=CARTESIAN_POINT('',(116.37,9.4,49.6));
#102138=CARTESIAN_POINT('',(116.23,9.4,49.6));
#102139=CARTESIAN_POINT('Origin',(116.23,9.4,49.7));
#102140=CARTESIAN_POINT('',(116.23,9.4,49.7));
#102141=CARTESIAN_POINT('',(113.115,9.4,49.7));
#102142=CARTESIAN_POINT('',(116.23,9.4,49.7));
#102143=CARTESIAN_POINT('Origin',(116.23,8.5,49.7));
#102144=CARTESIAN_POINT('',(116.23,8.6,49.7));
#102145=CARTESIAN_POINT('',(116.23,8.6,49.1));
#102146=CARTESIAN_POINT('',(116.23,9.35,49.7));
#102147=CARTESIAN_POINT('Origin',(114.57,9.8,49.7));
#102148=CARTESIAN_POINT('',(114.57,8.6,49.7));
#102149=CARTESIAN_POINT('',(114.57,8.6,49.6));
#102150=CARTESIAN_POINT('',(114.57,8.6,49.1));
#102151=CARTESIAN_POINT('',(114.57,9.8,49.7));
#102152=CARTESIAN_POINT('',(114.57,10.,49.7));
#102153=CARTESIAN_POINT('',(114.57,9.8,49.6));
#102154=CARTESIAN_POINT('',(114.57,9.8,49.7));
#102155=CARTESIAN_POINT('',(114.57,8.5,49.6));
#102156=CARTESIAN_POINT('Origin',(114.5,9.15,49.6));
#102157=CARTESIAN_POINT('',(114.43,8.6,49.6));
#102158=CARTESIAN_POINT('',(106.75,8.6,49.6));
#102159=CARTESIAN_POINT('',(114.43,9.8,49.6));
#102160=CARTESIAN_POINT('',(114.57,9.8,49.6));
#102161=CARTESIAN_POINT('',(114.43,9.8,49.6));
#102162=CARTESIAN_POINT('Origin',(114.43,9.8,49.7));
#102163=CARTESIAN_POINT('',(114.43,9.8,49.7));
#102164=CARTESIAN_POINT('',(112.215,9.8,49.7));
#102165=CARTESIAN_POINT('',(114.43,9.8,49.7));
#102166=CARTESIAN_POINT('Origin',(114.43,8.5,49.7));
#102167=CARTESIAN_POINT('',(114.43,8.6,49.7));
#102168=CARTESIAN_POINT('',(114.43,8.6,49.1));
#102169=CARTESIAN_POINT('',(114.43,9.35,49.7));
#102170=CARTESIAN_POINT('Origin',(112.77,9.4,49.7));
#102171=CARTESIAN_POINT('',(112.77,8.6,49.7));
#102172=CARTESIAN_POINT('',(112.77,8.6,49.6));
#102173=CARTESIAN_POINT('',(112.77,8.6,49.1));
#102174=CARTESIAN_POINT('',(112.77,9.4,49.7));
#102175=CARTESIAN_POINT('',(112.77,9.8,49.7));
#102176=CARTESIAN_POINT('',(112.77,9.4,49.6));
#102177=CARTESIAN_POINT('',(112.77,9.4,49.7));
#102178=CARTESIAN_POINT('',(112.77,8.5,49.6));
#102179=CARTESIAN_POINT('Origin',(112.7,8.95,49.6));
#102180=CARTESIAN_POINT('',(112.63,8.6,49.6));
#102181=CARTESIAN_POINT('',(105.85,8.6,49.6));
#102182=CARTESIAN_POINT('',(112.63,9.4,49.6));
#102183=CARTESIAN_POINT('',(112.77,9.4,49.6));
#102184=CARTESIAN_POINT('',(112.63,9.4,49.6));
#102185=CARTESIAN_POINT('Origin',(112.63,9.4,49.7));
#102186=CARTESIAN_POINT('',(112.63,9.4,49.7));
#102187=CARTESIAN_POINT('',(111.315,9.4,49.7));
#102188=CARTESIAN_POINT('',(112.63,9.4,49.7));
#102189=CARTESIAN_POINT('Origin',(112.63,8.5,49.7));
#102190=CARTESIAN_POINT('',(112.63,8.6,49.7));
#102191=CARTESIAN_POINT('',(112.63,8.6,49.1));
#102192=CARTESIAN_POINT('',(112.63,9.35,49.7));
#102193=CARTESIAN_POINT('Origin',(110.97,9.4,49.7));
#102194=CARTESIAN_POINT('',(110.97,8.6,49.7));
#102195=CARTESIAN_POINT('',(110.97,8.6,49.6));
#102196=CARTESIAN_POINT('',(110.97,8.6,49.1));
#102197=CARTESIAN_POINT('',(110.97,9.4,49.7));
#102198=CARTESIAN_POINT('',(110.97,9.8,49.7));
#102199=CARTESIAN_POINT('',(110.97,9.4,49.6));
#102200=CARTESIAN_POINT('',(110.97,9.4,49.7));
#102201=CARTESIAN_POINT('',(110.97,8.5,49.6));
#102202=CARTESIAN_POINT('Origin',(110.9,8.95,49.6));
#102203=CARTESIAN_POINT('',(110.83,8.6,49.6));
#102204=CARTESIAN_POINT('',(104.95,8.6,49.6));
#102205=CARTESIAN_POINT('',(110.83,9.4,49.6));
#102206=CARTESIAN_POINT('',(110.97,9.4,49.6));
#102207=CARTESIAN_POINT('',(110.83,9.4,49.6));
#102208=CARTESIAN_POINT('Origin',(110.83,9.4,49.7));
#102209=CARTESIAN_POINT('',(110.83,9.4,49.7));
#102210=CARTESIAN_POINT('',(110.415,9.4,49.7));
#102211=CARTESIAN_POINT('',(110.83,9.4,49.7));
#102212=CARTESIAN_POINT('Origin',(110.83,8.5,49.7));
#102213=CARTESIAN_POINT('',(110.83,8.6,49.7));
#102214=CARTESIAN_POINT('',(110.83,8.6,49.1));
#102215=CARTESIAN_POINT('',(110.83,9.35,49.7));
#102216=CARTESIAN_POINT('Origin',(110.07,10.2,49.7));
#102217=CARTESIAN_POINT('',(110.07,8.6,49.7));
#102218=CARTESIAN_POINT('',(110.07,8.6,49.6));
#102219=CARTESIAN_POINT('',(110.07,8.6,49.1));
#102220=CARTESIAN_POINT('',(110.07,10.2,49.7));
#102221=CARTESIAN_POINT('',(110.07,10.2,49.7));
#102222=CARTESIAN_POINT('',(110.07,10.2,49.6));
#102223=CARTESIAN_POINT('',(110.07,10.2,49.7));
#102224=CARTESIAN_POINT('',(110.07,8.5,49.6));
#102225=CARTESIAN_POINT('Origin',(110.,9.35,49.6));
#102226=CARTESIAN_POINT('',(109.93,8.6,49.6));
#102227=CARTESIAN_POINT('',(104.5,8.6,49.6));
#102228=CARTESIAN_POINT('',(109.93,10.2,49.6));
#102229=CARTESIAN_POINT('',(110.07,10.2,49.6));
#102230=CARTESIAN_POINT('',(109.93,10.2,49.6));
#102231=CARTESIAN_POINT('Origin',(109.93,10.2,49.7));
#102232=CARTESIAN_POINT('',(109.93,10.2,49.7));
#102233=CARTESIAN_POINT('',(109.965,10.2,49.7));
#102234=CARTESIAN_POINT('',(109.93,10.2,49.7));
#102235=CARTESIAN_POINT('Origin',(109.93,8.5,49.7));
#102236=CARTESIAN_POINT('',(109.93,8.6,49.7));
#102237=CARTESIAN_POINT('',(109.93,8.6,49.1));
#102238=CARTESIAN_POINT('',(109.93,9.35,49.7));
#102239=CARTESIAN_POINT('Origin',(108.27,9.4,49.7));
#102240=CARTESIAN_POINT('',(108.27,8.6,49.7));
#102241=CARTESIAN_POINT('',(108.27,8.6,49.6));
#102242=CARTESIAN_POINT('',(108.27,8.6,49.1));
#102243=CARTESIAN_POINT('',(108.27,9.4,49.7));
#102244=CARTESIAN_POINT('',(108.27,9.8,49.7));
#102245=CARTESIAN_POINT('',(108.27,9.4,49.6));
#102246=CARTESIAN_POINT('',(108.27,9.4,49.7));
#102247=CARTESIAN_POINT('',(108.27,8.5,49.6));
#102248=CARTESIAN_POINT('Origin',(108.2,8.95,49.6));
#102249=CARTESIAN_POINT('',(108.13,8.6,49.6));
#102250=CARTESIAN_POINT('',(103.6,8.6,49.6));
#102251=CARTESIAN_POINT('',(108.13,9.4,49.6));
#102252=CARTESIAN_POINT('',(108.27,9.4,49.6));
#102253=CARTESIAN_POINT('',(108.13,9.4,49.6));
#102254=CARTESIAN_POINT('Origin',(108.13,9.4,49.7));
#102255=CARTESIAN_POINT('',(108.13,9.4,49.7));
#102256=CARTESIAN_POINT('',(109.065,9.4,49.7));
#102257=CARTESIAN_POINT('',(108.13,9.4,49.7));
#102258=CARTESIAN_POINT('Origin',(108.13,8.5,49.7));
#102259=CARTESIAN_POINT('',(108.13,8.6,49.7));
#102260=CARTESIAN_POINT('',(108.13,8.6,49.1));
#102261=CARTESIAN_POINT('',(108.13,9.35,49.7));
#102262=CARTESIAN_POINT('Origin',(106.47,9.4,49.7));
#102263=CARTESIAN_POINT('',(106.47,8.6,49.7));
#102264=CARTESIAN_POINT('',(106.47,8.6,49.6));
#102265=CARTESIAN_POINT('',(106.47,8.6,49.1));
#102266=CARTESIAN_POINT('',(106.47,9.4,49.7));
#102267=CARTESIAN_POINT('',(106.47,9.8,49.7));
#102268=CARTESIAN_POINT('',(106.47,9.4,49.6));
#102269=CARTESIAN_POINT('',(106.47,9.4,49.7));
#102270=CARTESIAN_POINT('',(106.47,8.5,49.6));
#102271=CARTESIAN_POINT('Origin',(106.4,8.95,49.6));
#102272=CARTESIAN_POINT('',(106.33,8.6,49.6));
#102273=CARTESIAN_POINT('',(102.7,8.6,49.6));
#102274=CARTESIAN_POINT('',(106.33,9.4,49.6));
#102275=CARTESIAN_POINT('',(106.47,9.4,49.6));
#102276=CARTESIAN_POINT('',(106.33,9.4,49.6));
#102277=CARTESIAN_POINT('Origin',(106.33,9.4,49.7));
#102278=CARTESIAN_POINT('',(106.33,9.4,49.7));
#102279=CARTESIAN_POINT('',(108.165,9.4,49.7));
#102280=CARTESIAN_POINT('',(106.33,9.4,49.7));
#102281=CARTESIAN_POINT('Origin',(106.33,8.5,49.7));
#102282=CARTESIAN_POINT('',(106.33,8.6,49.7));
#102283=CARTESIAN_POINT('',(106.33,8.6,49.1));
#102284=CARTESIAN_POINT('',(106.33,9.35,49.7));
#102285=CARTESIAN_POINT('Origin',(104.67,9.4,49.7));
#102286=CARTESIAN_POINT('',(104.67,8.6,49.7));
#102287=CARTESIAN_POINT('',(104.67,8.6,49.6));
#102288=CARTESIAN_POINT('',(104.67,8.6,49.1));
#102289=CARTESIAN_POINT('',(104.67,9.4,49.7));
#102290=CARTESIAN_POINT('',(104.67,9.8,49.7));
#102291=CARTESIAN_POINT('',(104.67,9.4,49.6));
#102292=CARTESIAN_POINT('',(104.67,9.4,49.7));
#102293=CARTESIAN_POINT('',(104.67,8.5,49.6));
#102294=CARTESIAN_POINT('Origin',(104.6,8.95,49.6));
#102295=CARTESIAN_POINT('',(104.53,8.6,49.6));
#102296=CARTESIAN_POINT('',(101.8,8.6,49.6));
#102297=CARTESIAN_POINT('',(104.53,9.4,49.6));
#102298=CARTESIAN_POINT('',(104.67,9.4,49.6));
#102299=CARTESIAN_POINT('',(104.53,9.4,49.6));
#102300=CARTESIAN_POINT('Origin',(104.53,9.4,49.7));
#102301=CARTESIAN_POINT('',(104.53,9.4,49.7));
#102302=CARTESIAN_POINT('',(107.265,9.4,49.7));
#102303=CARTESIAN_POINT('',(104.53,9.4,49.7));
#102304=CARTESIAN_POINT('Origin',(104.53,8.5,49.7));
#102305=CARTESIAN_POINT('',(104.53,8.6,49.7));
#102306=CARTESIAN_POINT('',(104.53,8.6,49.1));
#102307=CARTESIAN_POINT('',(104.53,9.35,49.7));
#102308=CARTESIAN_POINT('Origin',(102.87,9.4,49.7));
#102309=CARTESIAN_POINT('',(102.87,8.88352744046827,49.6));
#102310=CARTESIAN_POINT('',(102.87,8.74291386665029,49.7));
#102311=CARTESIAN_POINT('Ctrl Pts',(102.87,8.88352744046827,49.6));
#102312=CARTESIAN_POINT('Ctrl Pts',(102.87,8.81502339168512,49.6474651054947));
#102313=CARTESIAN_POINT('Ctrl Pts',(102.87,8.74291386665029,49.7));
#102314=CARTESIAN_POINT('',(102.87,8.6,49.6));
#102315=CARTESIAN_POINT('',(102.87,8.5,49.6));
#102316=CARTESIAN_POINT('',(102.87,8.6,49.7));
#102317=CARTESIAN_POINT('',(102.87,8.6,49.1));
#102318=CARTESIAN_POINT('',(102.87,9.8,49.7));
#102319=CARTESIAN_POINT('Origin',(102.73,8.5,49.7));
#102320=CARTESIAN_POINT('',(102.73,8.62294578406448,49.7));
#102321=CARTESIAN_POINT('',(102.73,8.75186326612437,49.6));
#102322=CARTESIAN_POINT('Ctrl Pts',(102.73,8.62294578406448,49.7));
#102323=CARTESIAN_POINT('Ctrl Pts',(102.73,8.68905731332551,49.6478692670285));
#102324=CARTESIAN_POINT('Ctrl Pts',(102.73,8.75186326612437,49.6));
#102325=CARTESIAN_POINT('',(102.73,8.6,49.7));
#102326=CARTESIAN_POINT('',(102.73,9.35,49.7));
#102327=CARTESIAN_POINT('',(102.73,8.6,49.6));
#102328=CARTESIAN_POINT('',(102.73,8.6,49.1));
#102329=CARTESIAN_POINT('',(102.73,9.4,49.6));
#102330=CARTESIAN_POINT('Origin',(102.8,8.95,49.6));
#102331=CARTESIAN_POINT('Origin',(101.5,10.2,49.6));
#102332=CARTESIAN_POINT('',(100.9,8.6,49.6));
#102333=CARTESIAN_POINT('Origin',(103.77,9.4,49.7));
#102334=CARTESIAN_POINT('',(103.77,8.6,49.7));
#102335=CARTESIAN_POINT('',(103.77,8.6,49.6));
#102336=CARTESIAN_POINT('',(103.77,8.6,49.1));
#102337=CARTESIAN_POINT('',(103.77,9.4,49.7));
#102338=CARTESIAN_POINT('',(103.77,9.8,49.7));
#102339=CARTESIAN_POINT('',(103.77,9.4,49.6));
#102340=CARTESIAN_POINT('',(103.77,9.4,49.7));
#102341=CARTESIAN_POINT('',(103.77,8.5,49.6));
#102342=CARTESIAN_POINT('Origin',(103.7,8.95,49.6));
#102343=CARTESIAN_POINT('',(103.63,8.6,49.6));
#102344=CARTESIAN_POINT('',(101.35,8.6,49.6));
#102345=CARTESIAN_POINT('',(103.63,9.4,49.6));
#102346=CARTESIAN_POINT('',(103.77,9.4,49.6));
#102347=CARTESIAN_POINT('',(103.63,9.4,49.6));
#102348=CARTESIAN_POINT('Origin',(103.63,9.4,49.7));
#102349=CARTESIAN_POINT('',(103.63,9.4,49.7));
#102350=CARTESIAN_POINT('',(106.815,9.4,49.7));
#102351=CARTESIAN_POINT('',(103.63,9.4,49.7));
#102352=CARTESIAN_POINT('Origin',(103.63,8.5,49.7));
#102353=CARTESIAN_POINT('',(103.63,8.6,49.7));
#102354=CARTESIAN_POINT('',(103.63,8.6,49.1));
#102355=CARTESIAN_POINT('',(103.63,9.35,49.7));
#102356=CARTESIAN_POINT('Origin',(105.57,9.8,49.7));
#102357=CARTESIAN_POINT('',(105.57,8.6,49.7));
#102358=CARTESIAN_POINT('',(105.57,8.6,49.6));
#102359=CARTESIAN_POINT('',(105.57,8.6,49.1));
#102360=CARTESIAN_POINT('',(105.57,9.8,49.7));
#102361=CARTESIAN_POINT('',(105.57,10.,49.7));
#102362=CARTESIAN_POINT('',(105.57,9.8,49.6));
#102363=CARTESIAN_POINT('',(105.57,9.8,49.7));
#102364=CARTESIAN_POINT('',(105.57,8.5,49.6));
#102365=CARTESIAN_POINT('Origin',(105.5,9.15,49.6));
#102366=CARTESIAN_POINT('',(105.43,8.6,49.6));
#102367=CARTESIAN_POINT('',(102.25,8.6,49.6));
#102368=CARTESIAN_POINT('',(105.43,9.8,49.6));
#102369=CARTESIAN_POINT('',(105.57,9.8,49.6));
#102370=CARTESIAN_POINT('',(105.43,9.8,49.6));
#102371=CARTESIAN_POINT('Origin',(105.43,9.8,49.7));
#102372=CARTESIAN_POINT('',(105.43,9.8,49.7));
#102373=CARTESIAN_POINT('',(107.715,9.8,49.7));
#102374=CARTESIAN_POINT('',(105.43,9.8,49.7));
#102375=CARTESIAN_POINT('Origin',(105.43,8.5,49.7));
#102376=CARTESIAN_POINT('',(105.43,8.6,49.7));
#102377=CARTESIAN_POINT('',(105.43,8.6,49.1));
#102378=CARTESIAN_POINT('',(105.43,9.35,49.7));
#102379=CARTESIAN_POINT('Origin',(107.37,9.4,49.7));
#102380=CARTESIAN_POINT('',(107.37,8.6,49.7));
#102381=CARTESIAN_POINT('',(107.37,8.6,49.6));
#102382=CARTESIAN_POINT('',(107.37,8.6,49.1));
#102383=CARTESIAN_POINT('',(107.37,9.4,49.7));
#102384=CARTESIAN_POINT('',(107.37,9.8,49.7));
#102385=CARTESIAN_POINT('',(107.37,9.4,49.6));
#102386=CARTESIAN_POINT('',(107.37,9.4,49.7));
#102387=CARTESIAN_POINT('',(107.37,8.5,49.6));
#102388=CARTESIAN_POINT('Origin',(107.3,8.95,49.6));
#102389=CARTESIAN_POINT('',(107.23,8.6,49.6));
#102390=CARTESIAN_POINT('',(103.15,8.6,49.6));
#102391=CARTESIAN_POINT('',(107.23,9.4,49.6));
#102392=CARTESIAN_POINT('',(107.37,9.4,49.6));
#102393=CARTESIAN_POINT('',(107.23,9.4,49.6));
#102394=CARTESIAN_POINT('Origin',(107.23,9.4,49.7));
#102395=CARTESIAN_POINT('',(107.23,9.4,49.7));
#102396=CARTESIAN_POINT('',(108.615,9.4,49.7));
#102397=CARTESIAN_POINT('',(107.23,9.4,49.7));
#102398=CARTESIAN_POINT('Origin',(107.23,8.5,49.7));
#102399=CARTESIAN_POINT('',(107.23,8.6,49.7));
#102400=CARTESIAN_POINT('',(107.23,8.6,49.1));
#102401=CARTESIAN_POINT('',(107.23,9.35,49.7));
#102402=CARTESIAN_POINT('Origin',(109.17,9.4,49.7));
#102403=CARTESIAN_POINT('',(109.17,8.6,49.7));
#102404=CARTESIAN_POINT('',(109.17,8.6,49.6));
#102405=CARTESIAN_POINT('',(109.17,8.6,49.1));
#102406=CARTESIAN_POINT('',(109.17,9.4,49.7));
#102407=CARTESIAN_POINT('',(109.17,9.8,49.7));
#102408=CARTESIAN_POINT('',(109.17,9.4,49.6));
#102409=CARTESIAN_POINT('',(109.17,9.4,49.7));
#102410=CARTESIAN_POINT('',(109.17,8.5,49.6));
#102411=CARTESIAN_POINT('Origin',(109.1,8.95,49.6));
#102412=CARTESIAN_POINT('',(109.03,8.6,49.6));
#102413=CARTESIAN_POINT('',(104.05,8.6,49.6));
#102414=CARTESIAN_POINT('',(109.03,9.4,49.6));
#102415=CARTESIAN_POINT('',(109.17,9.4,49.6));
#102416=CARTESIAN_POINT('',(109.03,9.4,49.6));
#102417=CARTESIAN_POINT('Origin',(109.03,9.4,49.7));
#102418=CARTESIAN_POINT('',(109.03,9.4,49.7));
#102419=CARTESIAN_POINT('',(109.515,9.4,49.7));
#102420=CARTESIAN_POINT('',(109.03,9.4,49.7));
#102421=CARTESIAN_POINT('Origin',(109.03,8.5,49.7));
#102422=CARTESIAN_POINT('',(109.03,8.6,49.7));
#102423=CARTESIAN_POINT('',(109.03,8.6,49.1));
#102424=CARTESIAN_POINT('',(109.03,9.35,49.7));
#102425=CARTESIAN_POINT('Origin',(111.87,9.4,49.7));
#102426=CARTESIAN_POINT('',(111.87,8.6,49.7));
#102427=CARTESIAN_POINT('',(111.87,8.6,49.6));
#102428=CARTESIAN_POINT('',(111.87,8.6,49.1));
#102429=CARTESIAN_POINT('',(111.87,9.4,49.7));
#102430=CARTESIAN_POINT('',(111.87,9.8,49.7));
#102431=CARTESIAN_POINT('',(111.87,9.4,49.6));
#102432=CARTESIAN_POINT('',(111.87,9.4,49.7));
#102433=CARTESIAN_POINT('',(111.87,8.5,49.6));
#102434=CARTESIAN_POINT('Origin',(111.8,8.95,49.6));
#102435=CARTESIAN_POINT('',(111.73,8.6,49.6));
#102436=CARTESIAN_POINT('',(105.4,8.6,49.6));
#102437=CARTESIAN_POINT('',(111.73,9.4,49.6));
#102438=CARTESIAN_POINT('',(111.87,9.4,49.6));
#102439=CARTESIAN_POINT('',(111.73,9.4,49.6));
#102440=CARTESIAN_POINT('Origin',(111.73,9.4,49.7));
#102441=CARTESIAN_POINT('',(111.73,9.4,49.7));
#102442=CARTESIAN_POINT('',(110.865,9.4,49.7));
#102443=CARTESIAN_POINT('',(111.73,9.4,49.7));
#102444=CARTESIAN_POINT('Origin',(111.73,8.5,49.7));
#102445=CARTESIAN_POINT('',(111.73,8.6,49.7));
#102446=CARTESIAN_POINT('',(111.73,8.6,49.1));
#102447=CARTESIAN_POINT('',(111.73,9.35,49.7));
#102448=CARTESIAN_POINT('Origin',(113.67,9.4,49.7));
#102449=CARTESIAN_POINT('',(113.67,8.6,49.7));
#102450=CARTESIAN_POINT('',(113.67,8.6,49.6));
#102451=CARTESIAN_POINT('',(113.67,8.6,49.1));
#102452=CARTESIAN_POINT('',(113.67,9.4,49.7));
#102453=CARTESIAN_POINT('',(113.67,9.8,49.7));
#102454=CARTESIAN_POINT('',(113.67,9.4,49.6));
#102455=CARTESIAN_POINT('',(113.67,9.4,49.7));
#102456=CARTESIAN_POINT('',(113.67,8.5,49.6));
#102457=CARTESIAN_POINT('Origin',(113.6,8.95,49.6));
#102458=CARTESIAN_POINT('',(113.53,8.6,49.6));
#102459=CARTESIAN_POINT('',(106.3,8.6,49.6));
#102460=CARTESIAN_POINT('',(113.53,9.4,49.6));
#102461=CARTESIAN_POINT('',(113.67,9.4,49.6));
#102462=CARTESIAN_POINT('',(113.53,9.4,49.6));
#102463=CARTESIAN_POINT('Origin',(113.53,9.4,49.7));
#102464=CARTESIAN_POINT('',(113.53,9.4,49.7));
#102465=CARTESIAN_POINT('',(111.765,9.4,49.7));
#102466=CARTESIAN_POINT('',(113.53,9.4,49.7));
#102467=CARTESIAN_POINT('Origin',(113.53,8.5,49.7));
#102468=CARTESIAN_POINT('',(113.53,8.6,49.7));
#102469=CARTESIAN_POINT('',(113.53,8.6,49.1));
#102470=CARTESIAN_POINT('',(113.53,9.35,49.7));
#102471=CARTESIAN_POINT('Origin',(115.47,9.4,49.7));
#102472=CARTESIAN_POINT('',(115.47,8.6,49.7));
#102473=CARTESIAN_POINT('',(115.47,8.6,49.6));
#102474=CARTESIAN_POINT('',(115.47,8.6,49.1));
#102475=CARTESIAN_POINT('',(115.47,9.4,49.7));
#102476=CARTESIAN_POINT('',(115.47,9.8,49.7));
#102477=CARTESIAN_POINT('',(115.47,9.4,49.6));
#102478=CARTESIAN_POINT('',(115.47,9.4,49.7));
#102479=CARTESIAN_POINT('',(115.47,8.5,49.6));
#102480=CARTESIAN_POINT('Origin',(115.4,8.95,49.6));
#102481=CARTESIAN_POINT('',(115.33,8.6,49.6));
#102482=CARTESIAN_POINT('',(107.2,8.6,49.6));
#102483=CARTESIAN_POINT('',(115.33,9.4,49.6));
#102484=CARTESIAN_POINT('',(115.47,9.4,49.6));
#102485=CARTESIAN_POINT('',(115.33,9.4,49.6));
#102486=CARTESIAN_POINT('Origin',(115.33,9.4,49.7));
#102487=CARTESIAN_POINT('',(115.33,9.4,49.7));
#102488=CARTESIAN_POINT('',(112.665,9.4,49.7));
#102489=CARTESIAN_POINT('',(115.33,9.4,49.7));
#102490=CARTESIAN_POINT('Origin',(115.33,8.5,49.7));
#102491=CARTESIAN_POINT('',(115.33,8.6,49.7));
#102492=CARTESIAN_POINT('',(115.33,8.6,49.1));
#102493=CARTESIAN_POINT('',(115.33,9.35,49.7));
#102494=CARTESIAN_POINT('Origin',(117.27,9.4,49.7));
#102495=CARTESIAN_POINT('',(117.27,8.75186326612437,49.6));
#102496=CARTESIAN_POINT('',(117.27,8.62294578406447,49.7));
#102497=CARTESIAN_POINT('Ctrl Pts',(117.27,8.75186326612437,49.6));
#102498=CARTESIAN_POINT('Ctrl Pts',(117.27,8.68905731332593,49.6478692670281));
#102499=CARTESIAN_POINT('Ctrl Pts',(117.27,8.62294578406447,49.7));
#102500=CARTESIAN_POINT('',(117.27,8.6,49.6));
#102501=CARTESIAN_POINT('',(117.27,8.5,49.6));
#102502=CARTESIAN_POINT('',(117.27,8.6,49.7));
#102503=CARTESIAN_POINT('',(117.27,8.6,49.1));
#102504=CARTESIAN_POINT('',(117.27,9.8,49.7));
#102505=CARTESIAN_POINT('Origin',(117.13,8.5,49.7));
#102506=CARTESIAN_POINT('',(117.13,8.74291386665028,49.7));
#102507=CARTESIAN_POINT('',(117.13,8.88352744046827,49.6));
#102508=CARTESIAN_POINT('Ctrl Pts',(117.13,8.74291386665028,49.7));
#102509=CARTESIAN_POINT('Ctrl Pts',(117.13,8.81502339168516,49.6474651054946));
#102510=CARTESIAN_POINT('Ctrl Pts',(117.13,8.88352744046827,49.6));
#102511=CARTESIAN_POINT('',(117.13,8.6,49.7));
#102512=CARTESIAN_POINT('',(117.13,9.35,49.7));
#102513=CARTESIAN_POINT('',(117.13,8.6,49.6));
#102514=CARTESIAN_POINT('',(117.13,8.6,49.1));
#102515=CARTESIAN_POINT('',(117.13,9.4,49.6));
#102516=CARTESIAN_POINT('Origin',(117.2,8.95,49.6));
#102517=CARTESIAN_POINT('Origin',(118.5,10.2,49.6));
#102518=CARTESIAN_POINT('',(108.1,8.6,49.6));
#102519=CARTESIAN_POINT('Origin',(110.,10.2,49.7));
#102520=CARTESIAN_POINT('',(117.3,8.6,49.7));
#102521=CARTESIAN_POINT('',(99.,8.6,49.7));
#102522=CARTESIAN_POINT('Origin',(118.5,10.2,49.7));
#102523=CARTESIAN_POINT('Origin',(110.,10.2,49.7));
#102524=CARTESIAN_POINT('',(102.7,8.6,49.7));
#102525=CARTESIAN_POINT('Origin',(101.5,10.2,49.7));
#102526=CARTESIAN_POINT('',(99.,8.6,49.7));
#102527=CARTESIAN_POINT('Origin',(99.,8.6,48.5));
#102528=CARTESIAN_POINT('',(99.,8.6,49.7));
#102529=CARTESIAN_POINT('',(99.,8.6,49.7));
#102530=CARTESIAN_POINT('',(99.,8.6,49.7));
#102531=CARTESIAN_POINT('',(99.,8.6,49.7));
#102532=CARTESIAN_POINT('',(99.,8.6,49.7));
#102533=CARTESIAN_POINT('',(99.,8.6,49.7));
#102534=CARTESIAN_POINT('',(99.,8.6,49.7));
#102535=CARTESIAN_POINT('',(99.,8.6,49.7));
#102536=CARTESIAN_POINT('',(99.,8.6,49.7));
#102537=CARTESIAN_POINT('',(99.,8.6,49.7));
#102538=CARTESIAN_POINT('',(99.,8.6,49.7));
#102539=CARTESIAN_POINT('',(99.,8.6,49.7));
#102540=CARTESIAN_POINT('',(99.,8.6,49.7));
#102541=CARTESIAN_POINT('',(99.,8.6,49.7));
#102542=CARTESIAN_POINT('',(99.,8.6,49.7));
#102543=CARTESIAN_POINT('',(100.3,8.6,49.7));
#102544=CARTESIAN_POINT('Ctrl Pts',(102.7,8.6,49.7));
#102545=CARTESIAN_POINT('Ctrl Pts',(101.5,8.6,48.98));
#102546=CARTESIAN_POINT('Ctrl Pts',(100.3,8.6,49.7));
#102547=CARTESIAN_POINT('',(99.,8.6,49.7));
#102548=CARTESIAN_POINT('',(99.,8.6,49.7));
#102549=CARTESIAN_POINT('',(99.,8.6,48.5));
#102550=CARTESIAN_POINT('',(99.,8.6,48.5));
#102551=CARTESIAN_POINT('',(121.,8.6,48.5));
#102552=CARTESIAN_POINT('',(99.,8.6,48.5));
#102553=CARTESIAN_POINT('',(121.,8.6,49.7));
#102554=CARTESIAN_POINT('',(121.,8.6,48.5));
#102555=CARTESIAN_POINT('',(119.7,8.6,49.7));
#102556=CARTESIAN_POINT('',(99.,8.6,49.7));
#102557=CARTESIAN_POINT('Ctrl Pts',(119.7,8.6,49.7));
#102558=CARTESIAN_POINT('Ctrl Pts',(118.5,8.6,48.98));
#102559=CARTESIAN_POINT('Ctrl Pts',(117.3,8.6,49.7));
#102560=CARTESIAN_POINT('',(99.,8.6,49.7));
#102561=CARTESIAN_POINT('Origin',(118.5,10.2,48.5));
#102562=CARTESIAN_POINT('',(117.4,10.2,48.5));
#102563=CARTESIAN_POINT('Origin',(118.5,10.2,48.5));
#102564=CARTESIAN_POINT('',(117.4,10.2,48.8));
#102565=CARTESIAN_POINT('',(117.4,10.2,48.5));
#102566=CARTESIAN_POINT('Origin',(118.5,10.2,48.8));
#102567=CARTESIAN_POINT('Origin',(118.5,10.2,49.25));
#102568=CARTESIAN_POINT('',(116.5,10.2,49.7));
#102569=CARTESIAN_POINT('',(116.95,10.2,49.25));
#102570=CARTESIAN_POINT('Origin',(118.5,10.2,49.7));
#102571=CARTESIAN_POINT('',(119.7,11.8,49.7));
#102572=CARTESIAN_POINT('Origin',(118.5,10.2,49.7));
#102573=CARTESIAN_POINT('',(117.3,11.8,49.7));
#102574=CARTESIAN_POINT('Ctrl Pts',(117.3,11.8,49.7));
#102575=CARTESIAN_POINT('Ctrl Pts',(118.5,11.8,48.98));
#102576=CARTESIAN_POINT('Ctrl Pts',(119.7,11.8,49.7));
#102577=CARTESIAN_POINT('Origin',(118.5,10.2,49.7));
#102578=CARTESIAN_POINT('Origin',(110.,10.2,49.7));
#102579=CARTESIAN_POINT('',(102.7,11.8,49.7));
#102580=CARTESIAN_POINT('',(120.2,11.8,49.7));
#102581=CARTESIAN_POINT('Origin',(101.5,10.2,49.7));
#102582=CARTESIAN_POINT('Origin',(110.,10.2,49.7));
#102583=CARTESIAN_POINT('',(121.,11.,49.7));
#102584=CARTESIAN_POINT('',(121.,8.6,49.7));
#102585=CARTESIAN_POINT('',(120.2,11.8,49.7));
#102586=CARTESIAN_POINT('Origin',(120.2,11.,49.7));
#102587=CARTESIAN_POINT('',(120.2,11.8,49.7));
#102588=CARTESIAN_POINT('Origin',(101.5,10.2,48.5));
#102589=CARTESIAN_POINT('',(100.4,10.2,48.5));
#102590=CARTESIAN_POINT('Origin',(101.5,10.2,48.5));
#102591=CARTESIAN_POINT('',(100.4,10.2,48.8));
#102592=CARTESIAN_POINT('',(100.4,10.2,48.5));
#102593=CARTESIAN_POINT('Origin',(101.5,10.2,48.8));
#102594=CARTESIAN_POINT('Origin',(101.5,10.2,49.25));
#102595=CARTESIAN_POINT('',(99.5,10.2,49.7));
#102596=CARTESIAN_POINT('',(99.95,10.2,49.25));
#102597=CARTESIAN_POINT('Origin',(101.5,10.2,49.7));
#102598=CARTESIAN_POINT('',(100.3,11.8,49.7));
#102599=CARTESIAN_POINT('Ctrl Pts',(100.3,11.8,49.7));
#102600=CARTESIAN_POINT('Ctrl Pts',(101.5,11.8,48.98));
#102601=CARTESIAN_POINT('Ctrl Pts',(102.7,11.8,49.7));
#102602=CARTESIAN_POINT('Origin',(101.5,10.2,49.7));
#102603=CARTESIAN_POINT('Origin',(110.,10.2,49.7));
#102604=CARTESIAN_POINT('',(99.8,11.8,49.7));
#102605=CARTESIAN_POINT('',(120.2,11.8,49.7));
#102606=CARTESIAN_POINT('',(99.,11.,49.7));
#102607=CARTESIAN_POINT('Origin',(99.8,11.,49.7));
#102608=CARTESIAN_POINT('',(99.,11.,49.7));
#102609=CARTESIAN_POINT('Origin',(99.8,11.,48.5));
#102610=CARTESIAN_POINT('',(99.8,11.8,48.5));
#102611=CARTESIAN_POINT('',(99.,11.,48.5));
#102612=CARTESIAN_POINT('Origin',(99.8,11.,48.5));
#102613=CARTESIAN_POINT('',(99.,11.,48.5));
#102614=CARTESIAN_POINT('',(99.8,11.8,48.5));
#102615=CARTESIAN_POINT('Origin',(120.2,11.8,48.5));
#102616=CARTESIAN_POINT('',(120.2,11.8,48.5));
#102617=CARTESIAN_POINT('',(120.2,11.8,48.5));
#102618=CARTESIAN_POINT('',(120.2,11.8,48.5));
#102619=CARTESIAN_POINT('Origin',(120.2,11.,48.5));
#102620=CARTESIAN_POINT('',(121.,11.,48.5));
#102621=CARTESIAN_POINT('Origin',(120.2,11.,48.5));
#102622=CARTESIAN_POINT('',(121.,11.,48.5));
#102623=CARTESIAN_POINT('Origin',(121.,8.6,48.5));
#102624=CARTESIAN_POINT('',(121.,8.6,48.5));
#102625=CARTESIAN_POINT('Origin',(99.,11.,48.5));
#102626=CARTESIAN_POINT('',(99.,11.,48.5));
#102627=CARTESIAN_POINT('Origin',(110.,10.2,48.5));
#102628=CARTESIAN_POINT('',(0.,0.,0.));
#102629=CARTESIAN_POINT('Origin',(110.,10.75,10.13));
#102630=CARTESIAN_POINT('',(108.044515157092,10.751507398398,6.80586969212423));
#102631=CARTESIAN_POINT('',(108.044569492149,10.7516873045422,6.70413030787577));
#102632=CARTESIAN_POINT('',(108.046,10.75,10.13));
#102633=CARTESIAN_POINT('',(110.862570875312,12.5048480452433,6.58));
#102634=CARTESIAN_POINT('Ctrl Pts',(108.044515157092,10.751507398398,6.80586969212423));
#102635=CARTESIAN_POINT('Ctrl Pts',(108.043711910884,10.8492225887016,6.80028600079932));
#102636=CARTESIAN_POINT('Ctrl Pts',(108.05041787597,10.9468235741413,6.79470230947441));
#102637=CARTESIAN_POINT('Ctrl Pts',(108.065019752885,11.0432231509002,6.7891186181495));
#102638=CARTESIAN_POINT('Ctrl Pts',(108.160730597505,11.675092941758,6.75251922644771));
#102639=CARTESIAN_POINT('Ctrl Pts',(108.595681572202,12.2553453835437,6.71591983474591));
#102640=CARTESIAN_POINT('Ctrl Pts',(109.175396647758,12.5247754482411,6.67932044304411));
#102641=CARTESIAN_POINT('Ctrl Pts',(109.699791138726,12.7684945571377,6.64621362869607));
#102642=CARTESIAN_POINT('Ctrl Pts',(110.342639138428,12.7578826479092,6.61310681434804));
#102643=CARTESIAN_POINT('Ctrl Pts',(110.863615890953,12.505874778859,6.58));
#102644=CARTESIAN_POINT('',(109.138474140329,12.5038213116275,6.58));
#102645=CARTESIAN_POINT('Origin',(110.,10.75,6.58));
#102646=CARTESIAN_POINT('Ctrl Pts',(109.13847414033,12.5038213116275,6.58));
#102647=CARTESIAN_POINT('Ctrl Pts',(108.562316880239,12.2207968236057,6.6165993917018));
#102648=CARTESIAN_POINT('Ctrl Pts',(108.141185267799,11.6340572295968,6.65319878340359));
#102649=CARTESIAN_POINT('Ctrl Pts',(108.059472317674,11.0011909565928,6.68979817510539));
#102650=CARTESIAN_POINT('Ctrl Pts',(108.048806194589,10.918581901917,6.69457555269552));
#102651=CARTESIAN_POINT('Ctrl Pts',(108.043923256952,10.8351869177435,6.69935293028564));
#102652=CARTESIAN_POINT('Ctrl Pts',(108.044569492149,10.7516873045422,6.70413030787577));
#102653=CARTESIAN_POINT('Origin',(110.,10.75,10.13));
#102654=CARTESIAN_POINT('',(108.048945433675,10.7497217851578,7.50586969212423));
#102655=CARTESIAN_POINT('',(108.048986005899,10.7499472362473,7.40413030787577));
#102656=CARTESIAN_POINT('',(108.046,10.75,10.13));
#102657=CARTESIAN_POINT('Ctrl Pts',(108.048945433675,10.7497217851578,7.50586969212423));
#102658=CARTESIAN_POINT('Ctrl Pts',(108.049389547632,11.0898217190185,7.48654901767677));
#102659=CARTESIAN_POINT('Ctrl Pts',(108.134132298949,11.4301285218672,7.46722834322932));
#102660=CARTESIAN_POINT('Ctrl Pts',(108.301860293071,11.7228908251559,7.44790766878186));
#102661=CARTESIAN_POINT('Ctrl Pts',(108.619589499312,12.2774740640964,7.41130827708006));
#102662=CARTESIAN_POINT('Ctrl Pts',(109.235104542373,12.6614477089837,7.37470888537826));
#102663=CARTESIAN_POINT('Ctrl Pts',(109.872908683461,12.7029554058002,7.33810949367646));
#102664=CARTESIAN_POINT('Ctrl Pts',(110.51071282455,12.7444631026166,7.30151010197467));
#102665=CARTESIAN_POINT('Ctrl Pts',(111.170806063666,12.4435048513622,7.26491071027287));
#102666=CARTESIAN_POINT('Ctrl Pts',(111.557730049867,11.9347725404045,7.22831131857107));
#102667=CARTESIAN_POINT('Ctrl Pts',(111.944654036068,11.4260402294468,7.19171192686928));
#102668=CARTESIAN_POINT('Ctrl Pts',(112.058408769352,10.7095338587858,7.15511253516748));
#102669=CARTESIAN_POINT('Ctrl Pts',(111.848090495719,10.1059857264717,7.11851314346568));
#102670=CARTESIAN_POINT('Ctrl Pts',(111.637772222086,9.50243759415752,7.08191375176388));
#102671=CARTESIAN_POINT('Ctrl Pts',(111.103380941534,9.01184770019013,7.04531436006208));
#102672=CARTESIAN_POINT('Ctrl Pts',(110.484081604292,8.85373963219972,7.00871496836028));
#102673=CARTESIAN_POINT('Ctrl Pts',(109.864782267049,8.69563156420931,6.97211557665849));
#102674=CARTESIAN_POINT('Ctrl Pts',(109.160574873114,8.87000532219587,6.93551618495669));
#102675=CARTESIAN_POINT('Ctrl Pts',(108.686706533419,9.29893577115414,6.89891679325489));
#102676=CARTESIAN_POINT('Ctrl Pts',(108.285132688644,9.66242755800698,6.86790109287801));
#102677=CARTESIAN_POINT('Ctrl Pts',(108.048976944515,10.2087293527696,6.83688539250112));
#102678=CARTESIAN_POINT('Ctrl Pts',(108.044515157092,10.751507398398,6.80586969212423));
#102679=CARTESIAN_POINT('Ctrl Pts',(108.044569492149,10.7516873045422,6.70413030787577));
#102680=CARTESIAN_POINT('Ctrl Pts',(108.048874051536,10.1954980941472,6.73595232198744));
#102681=CARTESIAN_POINT('Ctrl Pts',(108.29850053233,9.63466663527941,6.76777433609911));
#102682=CARTESIAN_POINT('Ctrl Pts',(108.718378388755,9.27054355030639,6.79959635021079));
#102683=CARTESIAN_POINT('Ctrl Pts',(109.201291697771,8.85175536902323,6.83619574191258));
#102684=CARTESIAN_POINT('Ctrl Pts',(109.909412603614,8.69317195845609,6.87279513361438));
#102685=CARTESIAN_POINT('Ctrl Pts',(110.525208044422,8.86480594334321,6.90939452531618));
#102686=CARTESIAN_POINT('Ctrl Pts',(111.14100348523,9.03643992823033,6.94599391701798));
#102687=CARTESIAN_POINT('Ctrl Pts',(111.664473461004,9.53829130857172,6.98259330871977));
#102688=CARTESIAN_POINT('Ctrl Pts',(111.861602039404,10.1462061785723,7.01919270042156));
#102689=CARTESIAN_POINT('Ctrl Pts',(112.058730617804,10.7541210485729,7.05579209212336));
#102690=CARTESIAN_POINT('Ctrl Pts',(111.929517798829,11.4680994082327,7.09239148382517));
#102691=CARTESIAN_POINT('Ctrl Pts',(111.531658092341,11.9683395872945,7.12899087552696));
#102692=CARTESIAN_POINT('Ctrl Pts',(111.133798385853,12.4685797663562,7.16559026722876));
#102693=CARTESIAN_POINT('Ctrl Pts',(110.46729179185,12.7550817648198,7.20218965893055));
#102694=CARTESIAN_POINT('Ctrl Pts',(109.830530205499,12.6997228916506,7.23878905063235));
#102695=CARTESIAN_POINT('Ctrl Pts',(109.193768619148,12.6443640184814,7.27538844233415));
#102696=CARTESIAN_POINT('Ctrl Pts',(108.586752040449,12.2471442736793,7.31198783403595));
#102697=CARTESIAN_POINT('Ctrl Pts',(108.281142413997,11.6858003617248,7.34858722573775));
#102698=CARTESIAN_POINT('Ctrl Pts',(108.126545121574,11.4018359790796,7.36710158645042));
#102699=CARTESIAN_POINT('Ctrl Pts',(108.049077765418,11.0758722780451,7.38561594716309));
#102700=CARTESIAN_POINT('Ctrl Pts',(108.048986005899,10.7499472362473,7.40413030787577));
#102701=CARTESIAN_POINT('Origin',(110.,10.75,10.13));
#102702=CARTESIAN_POINT('',(108.043619792706,10.7489886882952,8.20586969212423));
#102703=CARTESIAN_POINT('',(108.043932396619,10.7488069461449,8.10413030787577));
#102704=CARTESIAN_POINT('',(108.046,10.75,10.13));
#102705=CARTESIAN_POINT('Ctrl Pts',(108.043619792706,10.7489886882952,8.20586969212423));
#102706=CARTESIAN_POINT('Ctrl Pts',(108.047304171251,11.3268472727125,8.17281203455422));
#102707=CARTESIAN_POINT('Ctrl Pts',(108.319782513348,11.9077308098779,8.13975437698421));
#102708=CARTESIAN_POINT('Ctrl Pts',(108.768450547222,12.2710129638945,8.10669671941421));
#102709=CARTESIAN_POINT('Ctrl Pts',(109.265188015117,12.6732164722637,8.07009732771241));
#102710=CARTESIAN_POINT('Ctrl Pts',(109.977890832777,12.8086940538942,8.03349793601062));
#102711=CARTESIAN_POINT('Ctrl Pts',(110.587558939682,12.616807124334,7.99689854430882));
#102712=CARTESIAN_POINT('Ctrl Pts',(111.197227046588,12.4249201947739,7.96029915260702));
#102713=CARTESIAN_POINT('Ctrl Pts',(111.703860442739,11.9056687540232,7.92369976090523));
#102714=CARTESIAN_POINT('Ctrl Pts',(111.880693974763,11.2914654024873,7.88710036920343));
#102715=CARTESIAN_POINT('Ctrl Pts',(112.057527506788,10.6772620509515,7.85050097750163));
#102716=CARTESIAN_POINT('Ctrl Pts',(111.904561174686,9.96810678863055,7.81390158579984));
#102717=CARTESIAN_POINT('Ctrl Pts',(111.490261658278,9.48141227895056,7.77730219409804));
#102718=CARTESIAN_POINT('Ctrl Pts',(111.075962141869,8.99471776927057,7.74070280239624));
#102719=CARTESIAN_POINT('Ctrl Pts',(110.400329441155,8.73048401223154,7.70410341069444));
#102720=CARTESIAN_POINT('Ctrl Pts',(109.765771025388,8.80697907788465,7.66750401899264));
#102721=CARTESIAN_POINT('Ctrl Pts',(109.131212609621,8.88347414353777,7.63090462729084));
#102722=CARTESIAN_POINT('Ctrl Pts',(108.537728478803,9.30069803188303,7.59430523558905));
#102723=CARTESIAN_POINT('Ctrl Pts',(108.250958098105,9.87190639255244,7.55770584388725));
#102724=CARTESIAN_POINT('Ctrl Pts',(108.115572669697,10.14157611378,7.54042712663291));
#102725=CARTESIAN_POINT('Ctrl Pts',(108.04854825709,10.4455662231262,7.52314840937857));
#102726=CARTESIAN_POINT('Ctrl Pts',(108.048945433675,10.7497217851578,7.50586969212423));
#102727=CARTESIAN_POINT('Ctrl Pts',(108.048986005899,10.7499472362473,7.40413030787577));
#102728=CARTESIAN_POINT('Ctrl Pts',(108.048896374192,10.4315800739931,7.42221533886489));
#102729=CARTESIAN_POINT('Ctrl Pts',(108.12263541912,10.113249798825,7.44030036985402));
#102730=CARTESIAN_POINT('Ctrl Pts',(108.270432104423,9.83413722201615,7.45838540084314));
#102731=CARTESIAN_POINT('Ctrl Pts',(108.569534095507,9.26928607336913,7.49498479254494));
#102732=CARTESIAN_POINT('Ctrl Pts',(109.171940751879,8.86505185518214,7.53158418424673));
#102733=CARTESIAN_POINT('Ctrl Pts',(109.808011482606,8.80235313266459,7.56818357594853));
#102734=CARTESIAN_POINT('Ctrl Pts',(110.444082213333,8.73965441014704,7.60478296765033));
#102735=CARTESIAN_POINT('Ctrl Pts',(111.113817018416,9.01849118329893,7.64138235935213));
#102736=CARTESIAN_POINT('Ctrl Pts',(111.51745195286,9.51406494419263,7.67798175105392));
#102737=CARTESIAN_POINT('Ctrl Pts',(111.921086887305,10.0096387050863,7.71458114275572));
#102738=CARTESIAN_POINT('Ctrl Pts',(112.058621951111,10.7219494537218,7.75118053445752));
#102739=CARTESIAN_POINT('Ctrl Pts',(111.868495572048,11.3321693276087,7.78777992615932));
#102740=CARTESIAN_POINT('Ctrl Pts',(111.678369192984,11.9423892014956,7.82437931786111));
#102741=CARTESIAN_POINT('Ctrl Pts',(111.160581371051,12.4505182006339,7.86097870956291));
#102742=CARTESIAN_POINT('Ctrl Pts',(110.5468907788,12.6291234308646,7.89757810126471));
#102743=CARTESIAN_POINT('Ctrl Pts',(109.933200186548,12.8077286610953,7.93417749296651));
#102744=CARTESIAN_POINT('Ctrl Pts',(109.223606823978,12.6568101224185,7.9707768846683));
#102745=CARTESIAN_POINT('Ctrl Pts',(108.735718548346,12.2439169655075,8.0073762763701));
#102746=CARTESIAN_POINT('Ctrl Pts',(108.305791934843,11.880075968388,8.03962762020532));
#102747=CARTESIAN_POINT('Ctrl Pts',(108.048021872612,11.3128086655436,8.07187896404054));
#102748=CARTESIAN_POINT('Ctrl Pts',(108.043932396619,10.7488069461449,8.10413030787577));
#102749=CARTESIAN_POINT('Origin',(110.,10.75,10.13));
#102750=CARTESIAN_POINT('',(108.046780828974,10.7516319787095,8.90586969212423));
#102751=CARTESIAN_POINT('',(108.046385982006,10.751669101789,8.80413030787576));
#102752=CARTESIAN_POINT('',(108.046,10.75,10.13));
#102753=CARTESIAN_POINT('Ctrl Pts',(108.046780828974,10.7516319787095,8.90586969212423));
#102754=CARTESIAN_POINT('Ctrl Pts',(108.045300812305,10.930595849109,8.89567444313347));
#102755=CARTESIAN_POINT('Ctrl Pts',(108.067935018338,11.1091924125775,8.88547919414272));
#102756=CARTESIAN_POINT('Ctrl Pts',(108.116203099833,11.2805692246058,8.87528394515196));
#102757=CARTESIAN_POINT('Ctrl Pts',(108.289478163829,11.8957858885357,8.83868455345016));
#102758=CARTESIAN_POINT('Ctrl Pts',(108.793097157889,12.4179615658071,8.80208516174836));
#102759=CARTESIAN_POINT('Ctrl Pts',(109.401644233603,12.6133745840746,8.76548577004656));
#102760=CARTESIAN_POINT('Ctrl Pts',(110.010191309318,12.808787602342,8.72888637834476));
#102761=CARTESIAN_POINT('Ctrl Pts',(110.723666466687,12.6774379616055,8.69228698664297));
#102762=CARTESIAN_POINT('Ctrl Pts',(111.222723911923,12.2781167156913,8.65568759494117));
#102763=CARTESIAN_POINT('Ctrl Pts',(111.721781357158,11.8787954697771,8.61908820323938));
#102764=CARTESIAN_POINT('Ctrl Pts',(112.006421090259,11.2115026186853,8.58248881153758));
#102765=CARTESIAN_POINT('Ctrl Pts',(111.94924063397,10.5749131216331,8.54588941983578));
#102766=CARTESIAN_POINT('Ctrl Pts',(111.892060177682,9.93832362458086,8.50929002813398));
#102767=CARTESIAN_POINT('Ctrl Pts',(111.493059532004,9.33243748156825,8.47269063643218));
#102768=CARTESIAN_POINT('Ctrl Pts',(110.930828208466,9.02844450748747,8.43609124473038));
#102769=CARTESIAN_POINT('Ctrl Pts',(110.368596884928,8.72445153340668,8.39949185302859));
#102770=CARTESIAN_POINT('Ctrl Pts',(109.643134883529,8.72235172825773,8.36289246132679));
#102771=CARTESIAN_POINT('Ctrl Pts',(109.079153209653,9.02308493605,8.326293069625));
#102772=CARTESIAN_POINT('Ctrl Pts',(108.515171535777,9.32381814384228,8.2896936779232));
#102773=CARTESIAN_POINT('Ctrl Pts',(108.112670189424,9.9273843645758,8.2530942862214));
#102774=CARTESIAN_POINT('Ctrl Pts',(108.051805575312,10.5636321924966,8.2164948945196));
#102775=CARTESIAN_POINT('Ctrl Pts',(108.045915688317,10.6252020859741,8.21295316038781));
#102776=CARTESIAN_POINT('Ctrl Pts',(108.043225055443,10.6870780260698,8.20941142625602));
#102777=CARTESIAN_POINT('Ctrl Pts',(108.043619792706,10.7489886882952,8.20586969212423));
#102778=CARTESIAN_POINT('Ctrl Pts',(108.043932396619,10.7488069461449,8.10413030787577));
#102779=CARTESIAN_POINT('Ctrl Pts',(108.043381063396,10.6727696037847,8.10847835574234));
#102780=CARTESIAN_POINT('Ctrl Pts',(108.047440572113,10.5967916159432,8.11282640360892));
#102781=CARTESIAN_POINT('Ctrl Pts',(108.056310690425,10.5213794633641,8.11717445147549));
#102782=CARTESIAN_POINT('Ctrl Pts',(108.130974296833,9.88660289327707,8.15377384317729));
#102783=CARTESIAN_POINT('Ctrl Pts',(108.546484698346,9.29191752824843,8.19037323487909));
#102784=CARTESIAN_POINT('Ctrl Pts',(109.116862635547,9.00349960882683,8.22697262658088));
#102785=CARTESIAN_POINT('Ctrl Pts',(109.687240572748,8.71508168940523,8.26357201828268));
#102786=CARTESIAN_POINT('Ctrl Pts',(110.412486045638,8.73293121559066,8.30017140998448));
#102787=CARTESIAN_POINT('Ctrl Pts',(110.967985017009,9.04905897482588,8.33677080168628));
#102788=CARTESIAN_POINT('Ctrl Pts',(111.52348398838,9.36518673406111,8.37337019338807));
#102789=CARTESIAN_POINT('Ctrl Pts',(111.909236458231,9.97959272634614,8.40996958508987));
#102790=CARTESIAN_POINT('Ctrl Pts',(111.952582667526,10.6172736803138,8.44656897679167));
#102791=CARTESIAN_POINT('Ctrl Pts',(111.99592887682,11.2549546342814,8.48316836849346));
#102792=CARTESIAN_POINT('Ctrl Pts',(111.696868825557,11.9159105499316,8.51976776019526));
#102793=CARTESIAN_POINT('Ctrl Pts',(111.189259422973,12.3043028494267,8.55636715189706));
#102794=CARTESIAN_POINT('Ctrl Pts',(110.68165002039,12.6926951489219,8.59296654359886));
#102795=CARTESIAN_POINT('Ctrl Pts',(109.965491266485,12.808523832262,8.62956593530066));
#102796=CARTESIAN_POINT('Ctrl Pts',(109.361330105331,12.599944892835,8.66616532700245));
#102797=CARTESIAN_POINT('Ctrl Pts',(108.757168944176,12.391365953408,8.70276471870425));
#102798=CARTESIAN_POINT('Ctrl Pts',(108.265005375772,11.8583793912139,8.73936411040605));
#102799=CARTESIAN_POINT('Ctrl Pts',(108.105127894314,11.2395457492598,8.77596350210785));
#102800=CARTESIAN_POINT('Ctrl Pts',(108.064114116421,11.0807947774987,8.78535243736382));
#102801=CARTESIAN_POINT('Ctrl Pts',(108.044967736627,10.9163942996569,8.79474137261979));
#102802=CARTESIAN_POINT('Ctrl Pts',(108.046385982006,10.751669101789,8.80413030787576));
#102803=CARTESIAN_POINT('Origin',(110.,10.75,10.13));
#102804=CARTESIAN_POINT('',(108.04785445166,10.7486597361157,9.60586969212423));
#102805=CARTESIAN_POINT('',(108.048142496813,10.7488058307817,9.50413030787576));
#102806=CARTESIAN_POINT('',(108.046,10.75,10.13));
#102807=CARTESIAN_POINT('Ctrl Pts',(108.04785445166,10.7486597361157,9.60586969212423));
#102808=CARTESIAN_POINT('Ctrl Pts',(108.050592274151,11.169344087362,9.58193746001092));
#102809=CARTESIAN_POINT('Ctrl Pts',(108.184359614202,11.5916163945113,9.55800522789762));
#102810=CARTESIAN_POINT('Ctrl Pts',(108.435439206868,11.9257312565921,9.53407299578431));
#102811=CARTESIAN_POINT('Ctrl Pts',(108.819413435298,12.4366907296905,9.49747360408251));
#102812=CARTESIAN_POINT('Ctrl Pts',(109.47775012871,12.741473154812,9.46087421238071));
#102813=CARTESIAN_POINT('Ctrl Pts',(110.115783029776,12.7036603474404,9.42427482067892));
#102814=CARTESIAN_POINT('Ctrl Pts',(110.753815930842,12.6658475400688,9.38767542897712));
#102815=CARTESIAN_POINT('Ctrl Pts',(111.371545039561,12.2854395002041,9.35107603727532));
#102816=CARTESIAN_POINT('Ctrl Pts',(111.692479729901,11.7327038348298,9.31447664557353));
#102817=CARTESIAN_POINT('Ctrl Pts',(112.013414420241,11.1799681694555,9.27787725387173));
#102818=CARTESIAN_POINT('Ctrl Pts',(112.037554692202,10.4549048785716,9.24127786216993));
#102819=CARTESIAN_POINT('Ctrl Pts',(111.754095552424,9.88204651271007,9.20467847046813));
#102820=CARTESIAN_POINT('Ctrl Pts',(111.470636412645,9.30918814684853,9.16807907876633));
#102821=CARTESIAN_POINT('Ctrl Pts',(110.879577861129,8.88853470600938,9.13147968706454));
#102822=CARTESIAN_POINT('Ctrl Pts',(110.245472995097,8.80836731797791,9.09488029536274));
#102823=CARTESIAN_POINT('Ctrl Pts',(109.611368129065,8.72819992994645,9.05828090366094));
#102824=CARTESIAN_POINT('Ctrl Pts',(108.934216948517,8.98851859472268,9.02168151195914));
#102825=CARTESIAN_POINT('Ctrl Pts',(108.51710692521,9.47280675240502,8.98508212025735));
#102826=CARTESIAN_POINT('Ctrl Pts',(108.216188465381,9.82218998076296,8.95867797754631));
#102827=CARTESIAN_POINT('Ctrl Pts',(108.050613846824,10.2881428007179,8.93227383483527));
#102828=CARTESIAN_POINT('Ctrl Pts',(108.046780828974,10.7516319787095,8.90586969212423));
#102829=CARTESIAN_POINT('Ctrl Pts',(108.046385982006,10.751669101789,8.80413030787576));
#102830=CARTESIAN_POINT('Ctrl Pts',(108.050496256821,10.2742722830963,8.83134076432159));
#102831=CARTESIAN_POINT('Ctrl Pts',(108.227333346095,9.79414806941248,8.85855122076741));
#102832=CARTESIAN_POINT('Ctrl Pts',(108.545184991362,9.44091305650114,8.88576167721324));
#102833=CARTESIAN_POINT('Ctrl Pts',(108.972710964378,8.96579472741058,8.92236106891503));
#102834=CARTESIAN_POINT('Ctrl Pts',(109.655354304921,8.72023879094344,8.95896046061684));
#102835=CARTESIAN_POINT('Ctrl Pts',(110.287569294919,8.81415412860432,8.99555985231863));
#102836=CARTESIAN_POINT('Ctrl Pts',(110.919784284918,8.9080694662652,9.03215924402043));
#102837=CARTESIAN_POINT('Ctrl Pts',(111.501570924371,9.34145607805408,9.06875863572223));
#102838=CARTESIAN_POINT('Ctrl Pts',(111.772526149646,9.92033356978501,9.10535802742402));
#102839=CARTESIAN_POINT('Ctrl Pts',(112.043481374921,10.4992110615159,9.14195741912582));
#102840=CARTESIAN_POINT('Ctrl Pts',(112.003605186016,11.2235794331889,9.17855681082762));
#102841=CARTESIAN_POINT('Ctrl Pts',(111.670745847484,11.7692171748484,9.21515620252942));
#102842=CARTESIAN_POINT('Ctrl Pts',(111.337886508951,12.3148549165078,9.25175559423121));
#102843=CARTESIAN_POINT('Ctrl Pts',(110.71204402079,12.6817620281538,9.28835498593301));
#102844=CARTESIAN_POINT('Ctrl Pts',(110.073340492925,12.7057138105415,9.3249543776348));
#102845=CARTESIAN_POINT('Ctrl Pts',(109.434636965061,12.7296655929293,9.3615537693366));
#102846=CARTESIAN_POINT('Ctrl Pts',(108.783072397493,12.410662046059,9.39815316103841));
#102847=CARTESIAN_POINT('Ctrl Pts',(108.410281898036,11.8914866152722,9.4347525527402));
#102848=CARTESIAN_POINT('Ctrl Pts',(108.174728183565,11.5634372112182,9.45787847111873));
#102849=CARTESIAN_POINT('Ctrl Pts',(108.050476378586,11.1554682039619,9.48100438949724));
#102850=CARTESIAN_POINT('Ctrl Pts',(108.048142496813,10.7488058307817,9.50413030787576));
#102851=CARTESIAN_POINT('Origin',(110.,10.75,10.13));
#102852=CARTESIAN_POINT('',(108.042985073083,10.7503289497149,10.3058696921242));
#102853=CARTESIAN_POINT('',(108.042916139437,10.7500816311095,10.2041303078758));
#102854=CARTESIAN_POINT('',(108.046,10.75,10.13));
#102855=CARTESIAN_POINT('Ctrl Pts',(108.042985073083,10.7503289497149,10.3058696921242));
#102856=CARTESIAN_POINT('Ctrl Pts',(108.042940614159,10.769013669924,10.3047998685902));
#102857=CARTESIAN_POINT('Ctrl Pts',(108.043185641729,10.7876971962134,10.3037300450561));
#102858=CARTESIAN_POINT('Ctrl Pts',(108.043723784935,10.8063722760494,10.3026602215221));
#102859=CARTESIAN_POINT('Ctrl Pts',(108.062134030542,11.4452594758757,10.2660608298203));
#102860=CARTESIAN_POINT('Ctrl Pts',(108.423598228993,12.074261194306,10.2294614381185));
#102861=CARTESIAN_POINT('Ctrl Pts',(108.966327885768,12.4118412750302,10.1928620464167));
#102862=CARTESIAN_POINT('Ctrl Pts',(109.509057542544,12.7494213557543,10.1562626547149));
#102863=CARTESIAN_POINT('Ctrl Pts',(110.233052657643,12.7955797987723,10.1196632630131));
#102864=CARTESIAN_POINT('Ctrl Pts',(110.814258787462,12.5296564528512,10.0830638713113));
#102865=CARTESIAN_POINT('Ctrl Pts',(111.395464917281,12.26373310693,10.0464644796095));
#102866=CARTESIAN_POINT('Ctrl Pts',(111.83388206182,11.6857279720698,10.0098650879077));
#102867=CARTESIAN_POINT('Ctrl Pts',(111.933278201169,11.0543515401945,9.97326569620588));
#102868=CARTESIAN_POINT('Ctrl Pts',(112.032674340518,10.4229751083192,9.93666630450408));
#102869=CARTESIAN_POINT('Ctrl Pts',(111.793049474678,9.73822737942879,9.90006691280229));
#102870=CARTESIAN_POINT('Ctrl Pts',(111.321657783896,9.3065959798443,9.86346752110049));
#102871=CARTESIAN_POINT('Ctrl Pts',(110.850266093114,8.87496458025981,9.82686812939869));
#102872=CARTESIAN_POINT('Ctrl Pts',(110.147107577391,8.6964495099812,9.79026873769689));
#102873=CARTESIAN_POINT('Ctrl Pts',(109.526910384509,8.85095269178194,9.75366934599509));
#102874=CARTESIAN_POINT('Ctrl Pts',(108.906713191627,9.00545587358267,9.7170699542933));
#102875=CARTESIAN_POINT('Ctrl Pts',(108.369477321586,9.49297730746276,9.6804705625915));
#102876=CARTESIAN_POINT('Ctrl Pts',(108.155665268289,10.0953062849405,9.6438711708897));
#102877=CARTESIAN_POINT('Ctrl Pts',(108.081664273324,10.3037741563371,9.63120401130121));
#102878=CARTESIAN_POINT('Ctrl Pts',(108.046405341763,10.5259945125633,9.61853685171272));
#102879=CARTESIAN_POINT('Ctrl Pts',(108.04785445166,10.7486597361157,9.60586969212423));
#102880=CARTESIAN_POINT('Ctrl Pts',(108.048142496813,10.7488058307817,9.50413030787576));
#102881=CARTESIAN_POINT('Ctrl Pts',(108.046782745676,10.5118788233028,9.51760378119904));
#102882=CARTESIAN_POINT('Ctrl Pts',(108.086806636952,10.2753953377931,9.53107725452231));
#102883=CARTESIAN_POINT('Ctrl Pts',(108.170313609378,10.0554187963128,9.54455072784559));
#102884=CARTESIAN_POINT('Ctrl Pts',(108.397152251522,9.45787372284372,9.58115011954739));
#102885=CARTESIAN_POINT('Ctrl Pts',(108.944845967157,8.98213089060881,9.61774951124919));
#102886=CARTESIAN_POINT('Ctrl Pts',(109.568251414047,8.84112899987964,9.65434890295099));
#102887=CARTESIAN_POINT('Ctrl Pts',(110.191656860937,8.70012710915047,9.69094829465279));
#102888=CARTESIAN_POINT('Ctrl Pts',(110.890774039081,8.89386615992705,9.72754768635458));
#102889=CARTESIAN_POINT('Ctrl Pts',(111.352683671185,9.33563009708535,9.76414707805638));
#102890=CARTESIAN_POINT('Ctrl Pts',(111.814593303289,9.77739403424364,9.80074646975817));
#102891=CARTESIAN_POINT('Ctrl Pts',(112.039295389352,10.4671828577836,9.83734586145997));
#102892=CARTESIAN_POINT('Ctrl Pts',(111.92621506643,11.0962525875984,9.87394525316177));
#102893=CARTESIAN_POINT('Ctrl Pts',(111.813134743508,11.7253223174132,9.91054464486356));
#102894=CARTESIAN_POINT('Ctrl Pts',(111.3622720116,12.2936729535027,9.94714403656536));
#102895=CARTESIAN_POINT('Ctrl Pts',(110.775429436335,12.5469152806487,9.98374342826716));
#102896=CARTESIAN_POINT('Ctrl Pts',(110.18858686107,12.8001576077948,10.020342819969));
#102897=CARTESIAN_POINT('Ctrl Pts',(109.465764442448,12.7382916259973,10.0569422116708));
#102898=CARTESIAN_POINT('Ctrl Pts',(108.930491734476,12.3890080556661,10.0935416033726));
#102899=CARTESIAN_POINT('Ctrl Pts',(108.395219026505,12.0397244853349,10.1301409950744));
#102900=CARTESIAN_POINT('Ctrl Pts',(108.047496029185,11.4030233264699,10.1667403867761));
#102901=CARTESIAN_POINT('Ctrl Pts',(108.04296078492,10.7638869435582,10.2033397784779));
#102902=CARTESIAN_POINT('Ctrl Pts',(108.042928131883,10.7592852632532,10.2036032882772));
#102903=CARTESIAN_POINT('Ctrl Pts',(108.042913268912,10.7546834567117,10.2038667980765));
#102904=CARTESIAN_POINT('Ctrl Pts',(108.042916139437,10.7500816311095,10.2041303078758));
#102905=CARTESIAN_POINT('Origin',(110.,10.75,10.13));
#102906=CARTESIAN_POINT('',(108.048535129176,10.7509086719559,11.0058696921242));
#102907=CARTESIAN_POINT('',(108.048310783185,10.7510873236897,10.9041303078758));
#102908=CARTESIAN_POINT('',(108.046,10.75,10.13));
#102909=CARTESIAN_POINT('Ctrl Pts',(108.048535129176,10.7509086719559,11.0058696921242));
#102910=CARTESIAN_POINT('Ctrl Pts',(108.047412644922,11.0114136919884,10.9910628854676));
#102911=CARTESIAN_POINT('Ctrl Pts',(108.096036433601,11.2715169252527,10.976256078811));
#102912=CARTESIAN_POINT('Ctrl Pts',(108.196425832272,11.5098122693262,10.9614492721544));
#102913=CARTESIAN_POINT('Ctrl Pts',(108.444567853022,12.0988295261007,10.9248498804526));
#102914=CARTESIAN_POINT('Ctrl Pts',(109.00898588976,12.5546055767633,10.8882504887508));
#102915=CARTESIAN_POINT('Ctrl Pts',(109.637050927409,12.6731386933476,10.851651097049));
#102916=CARTESIAN_POINT('Ctrl Pts',(110.265115965058,12.7916718099319,10.8150517053472));
#102917=CARTESIAN_POINT('Ctrl Pts',(110.956828003617,12.5729619924379,10.7784523136454));
#102918=CARTESIAN_POINT('Ctrl Pts',(111.402582247255,12.1149020121669,10.7418529219436));
#102919=CARTESIAN_POINT('Ctrl Pts',(111.848336490893,11.6568420318959,10.7052535302418));
#102920=CARTESIAN_POINT('Ctrl Pts',(112.04813293961,10.9594318888478,10.66865413854));
#102921=CARTESIAN_POINT('Ctrl Pts',(111.912544295249,10.3348268050029,10.6320547468382));
#102922=CARTESIAN_POINT('Ctrl Pts',(111.776955650888,9.71022172115799,10.5954553551364));
#102923=CARTESIAN_POINT('Ctrl Pts',(111.30598191345,9.1584216965162,10.5588559634346));
#102924=CARTESIAN_POINT('Ctrl Pts',(110.710427174364,8.92640802451273,10.5222565717328));
#102925=CARTESIAN_POINT('Ctrl Pts',(110.114872435277,8.69439435250926,10.485657180031));
#102926=CARTESIAN_POINT('Ctrl Pts',(109.394736694541,8.7821670331441,10.4490577883292));
#102927=CARTESIAN_POINT('Ctrl Pts',(108.872346970554,9.15043971407259,10.4124583966274));
#102928=CARTESIAN_POINT('Ctrl Pts',(108.365227030973,9.50794754993976,10.3769288284597));
#102929=CARTESIAN_POINT('Ctrl Pts',(108.044461584221,10.1297966663688,10.341399260292));
#102930=CARTESIAN_POINT('Ctrl Pts',(108.042985073083,10.7503289497149,10.3058696921242));
#102931=CARTESIAN_POINT('Ctrl Pts',(108.042916139437,10.7500816311095,10.2041303078758));
#102932=CARTESIAN_POINT('Ctrl Pts',(108.043311961662,10.1155268931863,10.2404661897783));
#102933=CARTESIAN_POINT('Ctrl Pts',(108.380895852216,9.48060973009477,10.2768020716808));
#102934=CARTESIAN_POINT('Ctrl Pts',(108.907340147268,9.12633446092207,10.3131379535833));
#102935=CARTESIAN_POINT('Ctrl Pts',(109.437602245088,8.76948996815607,10.3497373452851));
#102936=CARTESIAN_POINT('Ctrl Pts',(110.159473931937,8.69737258958249,10.3863367369869));
#102937=CARTESIAN_POINT('Ctrl Pts',(110.749851193771,8.94226148910796,10.4229361286887));
#102938=CARTESIAN_POINT('Ctrl Pts',(111.340228455606,9.18715038863343,10.4595355203905));
#102939=CARTESIAN_POINT('Ctrl Pts',(111.799111292426,9.74904556625794,10.4961349120923));
#102940=CARTESIAN_POINT('Ctrl Pts',(111.921107403561,10.3764472185271,10.5327343037941));
#102941=CARTESIAN_POINT('Ctrl Pts',(112.043103514695,11.0038488707963,10.5693336954959));
#102942=CARTESIAN_POINT('Ctrl Pts',(111.828212900144,11.6967569977101,10.6059330871977));
#102943=CARTESIAN_POINT('Ctrl Pts',(111.372618886398,12.145031443827,10.6425324788995));
#102944=CARTESIAN_POINT('Ctrl Pts',(110.917024872652,12.5933058899439,10.6791318706013));
#102945=CARTESIAN_POINT('Ctrl Pts',(110.220727459712,12.7969466552638,10.7157312623031));
#102946=CARTESIAN_POINT('Ctrl Pts',(109.595383820435,12.6648057561534,10.7523306540049));
#102947=CARTESIAN_POINT('Ctrl Pts',(108.970040181158,12.5326648570429,10.7889300457067));
#102948=CARTESIAN_POINT('Ctrl Pts',(108.415650315544,12.0647422935019,10.8255294374085));
#102949=CARTESIAN_POINT('Ctrl Pts',(108.180354709203,11.4704764758426,10.8621288291103));
#102950=CARTESIAN_POINT('Ctrl Pts',(108.090346260485,11.2431499005374,10.8761293220321));
#102951=CARTESIAN_POINT('Ctrl Pts',(108.047031470958,10.9973352807835,10.8901298149539));
#102952=CARTESIAN_POINT('Ctrl Pts',(108.048310783185,10.7510873236897,10.9041303078758));
#102953=CARTESIAN_POINT('Origin',(110.,10.75,10.13));
#102954=CARTESIAN_POINT('',(108.045710748453,10.7483378582515,11.7058696921242));
#102955=CARTESIAN_POINT('',(108.04612122492,10.7483233200191,11.6041303078758));
#102956=CARTESIAN_POINT('',(108.046,10.75,10.13));
#102957=CARTESIAN_POINT('Ctrl Pts',(108.045710748453,10.7483378582515,11.7058696921242));
#102958=CARTESIAN_POINT('Ctrl Pts',(108.050148979404,11.2486837218457,11.6773259023451));
#102959=CARTESIAN_POINT('Ctrl Pts',(108.246601184755,11.7521292435267,11.6487821125659));
#102960=CARTESIAN_POINT('Ctrl Pts',(108.593113995841,12.1104654471406,11.6202383227868));
#102961=CARTESIAN_POINT('Ctrl Pts',(109.037419331633,12.5699309623533,11.583638931085));
#102962=CARTESIAN_POINT('Ctrl Pts',(109.728437171546,12.7908243149632,11.5470395393832));
#102963=CARTESIAN_POINT('Ctrl Pts',(110.356873438286,12.6742753994169,11.5104401476814));
#102964=CARTESIAN_POINT('Ctrl Pts',(110.985309705026,12.5577264838707,11.4738407559796));
#102965=CARTESIAN_POINT('Ctrl Pts',(111.551164398593,12.1037353001683,11.4372413642778));
#102966=CARTESIAN_POINT('Ctrl Pts',(111.801165467383,11.5155046846917,11.400641972576));
#102967=CARTESIAN_POINT('Ctrl Pts',(112.051166536173,10.9272740692151,11.3640425808742));
#102968=CARTESIAN_POINT('Ctrl Pts',(111.985313980186,10.2048040219644,11.3274431891724));
#102969=CARTESIAN_POINT('Ctrl Pts',(111.633082878848,9.67146637800422,11.2908437974706));
#102970=CARTESIAN_POINT('Ctrl Pts',(111.28085177751,9.13812873404405,11.2542444057688));
#102971=CARTESIAN_POINT('Ctrl Pts',(110.642242130822,8.79392349337443,11.217645014067));
#102972=CARTESIAN_POINT('Ctrl Pts',(110.003090527121,8.7929141787187,11.1810456223652));
#102973=CARTESIAN_POINT('Ctrl Pts',(109.36393892342,8.79190486406298,11.1444462306634));
#102974=CARTESIAN_POINT('Ctrl Pts',(108.724245362707,9.13409147542115,11.1078468389616));
#102975=CARTESIAN_POINT('Ctrl Pts',(108.370331584732,9.66631401254336,11.0712474472598));
#102976=CARTESIAN_POINT('Ctrl Pts',(108.159598680535,9.98321832061778,11.0494548622146));
#102977=CARTESIAN_POINT('Ctrl Pts',(108.050187195968,10.3674986676641,11.0276622771694));
#102978=CARTESIAN_POINT('Ctrl Pts',(108.048535129176,10.7509086719559,11.0058696921242));
#102979=CARTESIAN_POINT('Ctrl Pts',(108.048310783185,10.7510873236897,10.9041303078758));
#102980=CARTESIAN_POINT('Ctrl Pts',(108.050375785303,10.3536061286908,10.9267292066557));
#102981=CARTESIAN_POINT('Ctrl Pts',(108.168629869771,9.95499588151061,10.9493281054357));
#102982=CARTESIAN_POINT('Ctrl Pts',(108.394243058791,9.63118813810347,10.9719270042157));
#102983=CARTESIAN_POINT('Ctrl Pts',(108.759628361785,9.10677468980156,11.0085263959175));
#102984=CARTESIAN_POINT('Ctrl Pts',(109.406600314839,8.77855686497553,11.0451257876193));
#102985=CARTESIAN_POINT('Ctrl Pts',(110.045579427837,8.79344234627983,11.0817251793211));
#102986=CARTESIAN_POINT('Ctrl Pts',(110.684558540835,8.80832782758412,11.1183245710229));
#102987=CARTESIAN_POINT('Ctrl Pts',(111.315544813776,9.16631661501872,11.1549239627247));
#102988=CARTESIAN_POINT('Ctrl Pts',(111.656113819574,9.70717578031639,11.1915233544265));
#102989=CARTESIAN_POINT('Ctrl Pts',(111.996682825373,10.2480349456141,11.2281227461283));
#102990=CARTESIAN_POINT('Ctrl Pts',(112.04683456403,10.9717644887748,11.2647221378301));
#102991=CARTESIAN_POINT('Ctrl Pts',(111.784121516993,11.5544288341185,11.3013215295319));
#102992=CARTESIAN_POINT('Ctrl Pts',(111.521408469956,12.1370931794621,11.3379209212337));
#102993=CARTESIAN_POINT('Ctrl Pts',(110.945830637226,12.5786923269888,11.3745203129355));
#102994=CARTESIAN_POINT('Ctrl Pts',(110.315012069668,12.6815700175268,11.4111197046373));
#102995=CARTESIAN_POINT('Ctrl Pts',(109.684193502111,12.7844477080649,11.4477190963391));
#102996=CARTESIAN_POINT('Ctrl Pts',(108.998134199725,12.5486039416144,11.4843184880409));
#102997=CARTESIAN_POINT('Ctrl Pts',(108.563908838614,12.0796005086416,11.5209178797427));
#102998=CARTESIAN_POINT('Ctrl Pts',(108.234823709282,11.7241582217096,11.548655355787));
#102999=CARTESIAN_POINT('Ctrl Pts',(108.050382574886,11.2347977446687,11.5763928318314));
#103000=CARTESIAN_POINT('Ctrl Pts',(108.04612122492,10.7483233200191,11.6041303078758));
#103001=CARTESIAN_POINT('Origin',(110.,10.75,10.13));
#103002=CARTESIAN_POINT('',(108.044526058825,10.7514351493348,12.4058696921242));
#103003=CARTESIAN_POINT('',(108.044157220265,10.7512978840258,12.3041303078758));
#103004=CARTESIAN_POINT('',(108.046,10.75,10.13));
#103005=CARTESIAN_POINT('Ctrl Pts',(108.044526058825,10.7514351493348,12.4058696921242));
#103006=CARTESIAN_POINT('Ctrl Pts',(108.043703950285,10.8508683356403,12.4001883109243));
#103007=CARTESIAN_POINT('Ctrl Pts',(108.05065038668,10.9501864196576,12.3945069297244));
#103008=CARTESIAN_POINT('Ctrl Pts',(108.065770181827,11.0482442275904,12.3888255485245));
#103009=CARTESIAN_POINT('Ctrl Pts',(108.163171726549,11.6799314873731,12.3522261568227));
#103010=CARTESIAN_POINT('Ctrl Pts',(108.599761238115,12.2593182797734,12.3156267651209));
#103011=CARTESIAN_POINT('Ctrl Pts',(109.18012462215,12.5270758880419,12.2790273734191));
#103012=CARTESIAN_POINT('Ctrl Pts',(109.760488006184,12.7948334963104,12.2424279817173));
#103013=CARTESIAN_POINT('Ctrl Pts',(110.484625262688,12.7509619204471,12.2058285900155));
#103014=CARTESIAN_POINT('Ctrl Pts',(111.028418379987,12.4150976327762,12.1692291983137));
#103015=CARTESIAN_POINT('Ctrl Pts',(111.572211497286,12.0792333451053,12.1326298066119));
#103016=CARTESIAN_POINT('Ctrl Pts',(111.935660475381,11.4513763456268,12.0960304149101));
#103017=CARTESIAN_POINT('Ctrl Pts',(111.956088422006,10.8125504704608,12.0594310232083));
#103018=CARTESIAN_POINT('Ctrl Pts',(111.97651636863,10.1737245952948,12.0228316315065));
#103019=CARTESIAN_POINT('Ctrl Pts',(111.653923283786,9.52392984444133,11.9862322398047));
#103020=CARTESIAN_POINT('Ctrl Pts',(111.132699274202,9.15400914676403,11.9496328481029));
#103021=CARTESIAN_POINT('Ctrl Pts',(110.611475264618,8.78408844908674,11.9130334564011));
#103022=CARTESIAN_POINT('Ctrl Pts',(109.891620330295,8.69404180458565,11.8764340646993));
#103023=CARTESIAN_POINT('Ctrl Pts',(109.295335796589,8.9241733850372,11.8398346729976));
#103024=CARTESIAN_POINT('Ctrl Pts',(108.699051262883,9.15430496548875,11.8032352812958));
#103025=CARTESIAN_POINT('Ctrl Pts',(108.226337129794,9.70461477089292,11.7666358895939));
#103026=CARTESIAN_POINT('Ctrl Pts',(108.088776479085,10.3287885125027,11.7300364978922));
#103027=CARTESIAN_POINT('Ctrl Pts',(108.058499094932,10.466170445895,11.7219808959695));
#103028=CARTESIAN_POINT('Ctrl Pts',(108.044458195024,10.6071307119006,11.7139252940469));
#103029=CARTESIAN_POINT('Ctrl Pts',(108.045710748453,10.7483378582515,11.7058696921242));
#103030=CARTESIAN_POINT('Ctrl Pts',(108.04612122492,10.7483233200191,11.6041303078758));
#103031=CARTESIAN_POINT('Ctrl Pts',(108.044759755552,10.5928983882826,11.6129922235332));
#103032=CARTESIAN_POINT('Ctrl Pts',(108.061790220506,10.4377680516706,11.6218541391906));
#103033=CARTESIAN_POINT('Ctrl Pts',(108.098371525177,10.2873938172196,11.630716054848));
#103034=CARTESIAN_POINT('Ctrl Pts',(108.249450992684,9.66635365826534,11.6673154465498));
#103035=CARTESIAN_POINT('Ctrl Pts',(108.734001347535,9.12643643985169,11.7039148382516));
#103036=CARTESIAN_POINT('Ctrl Pts',(109.335141712287,8.90930480675388,11.7405142299534));
#103037=CARTESIAN_POINT('Ctrl Pts',(109.936282077039,8.69217317365606,11.7771136216552));
#103038=CARTESIAN_POINT('Ctrl Pts',(110.654012451694,8.79782712587406,11.813713013357));
#103039=CARTESIAN_POINT('Ctrl Pts',(111.167082441064,9.1789767949659,11.8503124050588));
#103040=CARTESIAN_POINT('Ctrl Pts',(111.680152430435,9.56012646405774,11.8869117967606));
#103041=CARTESIAN_POINT('Ctrl Pts',(111.98856203452,10.2167718500234,11.9235111884624));
#103042=CARTESIAN_POINT('Ctrl Pts',(111.954269571355,10.8550037142087,11.9601105801642));
#103043=CARTESIAN_POINT('Ctrl Pts',(111.919977108191,11.493235578394,11.996709971866));
#103044=CARTESIAN_POINT('Ctrl Pts',(111.542982577776,12.113053920799,12.0333093635678));
#103045=CARTESIAN_POINT('Ctrl Pts',(110.99202572961,12.4370329850584,12.0699087552696));
#103046=CARTESIAN_POINT('Ctrl Pts',(110.441068881443,12.7610120493179,12.1065081469714));
#103047=CARTESIAN_POINT('Ctrl Pts',(109.716149715525,12.7891518354319,12.1431075386732));
#103048=CARTESIAN_POINT('Ctrl Pts',(109.141736268846,12.5088572115586,12.179706930375));
#103049=CARTESIAN_POINT('Ctrl Pts',(108.567322822166,12.2285625876853,12.2163063220768));
#103050=CARTESIAN_POINT('Ctrl Pts',(108.143415094725,11.6398335538247,12.2529057137786));
#103051=CARTESIAN_POINT('Ctrl Pts',(108.059750815919,11.0061805088822,12.2895051054804));
#103052=CARTESIAN_POINT('Ctrl Pts',(108.048606668854,10.9217774300347,12.2943801729455));
#103053=CARTESIAN_POINT('Ctrl Pts',(108.043499273272,10.8365772892847,12.2992552404106));
#103054=CARTESIAN_POINT('Ctrl Pts',(108.044157220265,10.7512978840258,12.3041303078758));
#103055=CARTESIAN_POINT('Origin',(110.,10.75,10.13));
#103056=CARTESIAN_POINT('',(108.048941223895,10.7496876406009,13.1058696921242));
#103057=CARTESIAN_POINT('',(108.048980644574,10.7499134704375,13.0041303078758));
#103058=CARTESIAN_POINT('',(108.046,10.75,10.13));
#103059=CARTESIAN_POINT('Ctrl Pts',(108.048941223895,10.7496876406009,13.1058696921242));
#103060=CARTESIAN_POINT('Ctrl Pts',(108.049427891664,11.0915066401091,13.0864513278018));
#103061=CARTESIAN_POINT('Ctrl Pts',(108.135074391136,11.4335566218935,13.0670329634793));
#103062=CARTESIAN_POINT('Ctrl Pts',(108.304422957909,11.7273573425776,13.0476145991569));
#103063=CARTESIAN_POINT('Ctrl Pts',(108.62360815943,12.2811077759316,13.0110152074551));
#103064=CARTESIAN_POINT('Ctrl Pts',(109.240136984181,12.6634573039523,12.9744158157533));
#103065=CARTESIAN_POINT('Ctrl Pts',(109.878048356021,12.7032830865787,12.9378164240515));
#103066=CARTESIAN_POINT('Ctrl Pts',(110.515959727861,12.7431088692051,12.9012170323497));
#103067=CARTESIAN_POINT('Ctrl Pts',(111.17525364679,12.4404109064371,12.8646176406479));
#103068=CARTESIAN_POINT('Ctrl Pts',(111.56083918769,11.9306676298148,12.8280182489461));
#103069=CARTESIAN_POINT('Ctrl Pts',(111.94642472859,11.4209243531925,12.7914188572443));
#103070=CARTESIAN_POINT('Ctrl Pts',(112.05830189146,10.7041357627159,12.7548194655425));
#103071=CARTESIAN_POINT('Ctrl Pts',(111.846393492449,10.1011340438354,12.7182200738407));
#103072=CARTESIAN_POINT('Ctrl Pts',(111.634485093438,9.49813232495484,12.6816206821389));
#103073=CARTESIAN_POINT('Ctrl Pts',(111.098791132546,9.00891747767032,12.6450212904371));
#103074=CARTESIAN_POINT('Ctrl Pts',(110.479084870382,8.85245653454336,12.6084218987353));
#103075=CARTESIAN_POINT('Ctrl Pts',(109.859378608218,8.69599559141641,12.5718225070335));
#103076=CARTESIAN_POINT('Ctrl Pts',(109.155660044781,8.872288552447,12.5352231153317));
#103077=CARTESIAN_POINT('Ctrl Pts',(108.682907552003,9.30242889654483,12.4986237236299));
#103078=CARTESIAN_POINT('Ctrl Pts',(108.283541173031,9.66579787776891,12.467705713128));
#103079=CARTESIAN_POINT('Ctrl Pts',(108.048999963953,10.2103209043556,12.4367877026261));
#103080=CARTESIAN_POINT('Ctrl Pts',(108.044526058825,10.7514351493348,12.4058696921242));
#103081=CARTESIAN_POINT('Ctrl Pts',(108.044157220265,10.7512978840258,12.3041303078758));
#103082=CARTESIAN_POINT('Ctrl Pts',(108.048438786391,10.1963452556777,12.3358546321124));
#103083=CARTESIAN_POINT('Ctrl Pts',(108.296865792646,9.63803600659926,12.3675789563491));
#103084=CARTESIAN_POINT('Ctrl Pts',(108.714645515603,9.27417507348757,12.3993032805858));
#103085=CARTESIAN_POINT('Ctrl Pts',(109.196625324267,8.85439973906008,12.4359026722876));
#103086=CARTESIAN_POINT('Ctrl Pts',(109.904005771767,8.69342612622964,12.4725020639894));
#103087=CARTESIAN_POINT('Ctrl Pts',(110.520169044345,8.86330463874869,12.5091014556912));
#103088=CARTESIAN_POINT('Ctrl Pts',(111.136332316922,9.03318315126774,12.545700847393));
#103089=CARTESIAN_POINT('Ctrl Pts',(111.661278414578,9.53391378913629,12.5823002390948));
#103090=CARTESIAN_POINT('Ctrl Pts',(111.860045572213,10.1413737179372,12.6188996307966));
#103091=CARTESIAN_POINT('Ctrl Pts',(112.058812729848,10.7488336467382,12.6554990224984));
#103092=CARTESIAN_POINT('Ctrl Pts',(111.931400947464,11.4630228664716,12.6920984142002));
#103093=CARTESIAN_POINT('Ctrl Pts',(111.534838876806,11.9642755498955,12.728697805902));
#103094=CARTESIAN_POINT('Ctrl Pts',(111.138276806148,12.4655282333194,12.7652971976038));
#103095=CARTESIAN_POINT('Ctrl Pts',(110.472564447218,12.7538443804338,12.8018965893056));
#103096=CARTESIAN_POINT('Ctrl Pts',(109.835669034371,12.7001768448261,12.8384959810074));
#103097=CARTESIAN_POINT('Ctrl Pts',(109.198773621524,12.6465093092184,12.8750953727092));
#103098=CARTESIAN_POINT('Ctrl Pts',(108.59069515476,12.2508580908886,12.911694764411));
#103099=CARTESIAN_POINT('Ctrl Pts',(108.283605344712,11.6903117653571,12.9482941561128));
#103100=CARTESIAN_POINT('Ctrl Pts',(108.12743960496,11.4052546624268,12.9669062067004));
#103101=CARTESIAN_POINT('Ctrl Pts',(108.049111717213,11.0775544875257,12.9855182572881));
#103102=CARTESIAN_POINT('Ctrl Pts',(108.048980644574,10.7499134704375,13.0041303078758));
#103103=CARTESIAN_POINT('Origin',(110.,10.75,10.13));
#103104=CARTESIAN_POINT('',(108.04401647614,10.7486495636155,13.8058696921242));
#103105=CARTESIAN_POINT('',(108.043923528227,10.7487415210877,13.7041303078758));
#103106=CARTESIAN_POINT('',(108.046,10.75,10.13));
#103107=CARTESIAN_POINT('Ctrl Pts',(108.04401647614,10.7486495636155,13.8058696921242));
#103108=CARTESIAN_POINT('Ctrl Pts',(108.04772980719,11.3276092745096,13.7727143446792));
#103109=CARTESIAN_POINT('Ctrl Pts',(108.321504296629,11.911076308,13.7395589972342));
#103110=CARTESIAN_POINT('Ctrl Pts',(108.772311391298,12.2745082768577,13.7064036497892));
#103111=CARTESIAN_POINT('Ctrl Pts',(109.269946515379,12.6756920981778,13.6698042580874));
#103112=CARTESIAN_POINT('Ctrl Pts',(109.983303336603,12.8087539116218,13.6332048663856));
#103113=CARTESIAN_POINT('Ctrl Pts',(110.592540776308,12.6151257353379,13.5966054746838));
#103114=CARTESIAN_POINT('Ctrl Pts',(111.201778216014,12.421497559054,13.560006082982));
#103115=CARTESIAN_POINT('Ctrl Pts',(111.706896274201,11.9011793930423,13.5234066912802));
#103116=CARTESIAN_POINT('Ctrl Pts',(111.882075975322,11.2865802792359,13.4868072995784));
#103117=CARTESIAN_POINT('Ctrl Pts',(112.057255676443,10.6719811654296,13.4502079078766));
#103118=CARTESIAN_POINT('Ctrl Pts',(111.902497020499,9.96310110382854,13.4136085161748));
#103119=CARTESIAN_POINT('Ctrl Pts',(111.486937042034,9.47746498726815,13.377009124473));
#103120=CARTESIAN_POINT('Ctrl Pts',(111.071377063569,8.99182887070775,13.3404097327712));
#103121=CARTESIAN_POINT('Ctrl Pts',(110.395015762583,8.72943669918797,13.3038103410694));
#103122=CARTESIAN_POINT('Ctrl Pts',(109.760651801791,8.80761723079152,13.2672109493676));
#103123=CARTESIAN_POINT('Ctrl Pts',(109.126287841,8.88579776239506,13.2306115576658));
#103124=CARTESIAN_POINT('Ctrl Pts',(108.533921220403,9.30455099712193,13.194012165964));
#103125=CARTESIAN_POINT('Ctrl Pts',(108.24865869925,9.87650328382905,13.1574127742622));
#103126=CARTESIAN_POINT('Ctrl Pts',(108.114746550486,10.1449975795173,13.1402317468829));
#103127=CARTESIAN_POINT('Ctrl Pts',(108.048510628808,10.4472521989845,13.1230507195036));
#103128=CARTESIAN_POINT('Ctrl Pts',(108.048941223895,10.7496876406009,13.1058696921242));
#103129=CARTESIAN_POINT('Ctrl Pts',(108.048980644574,10.7499134704375,13.0041303078758));
#103130=CARTESIAN_POINT('Ctrl Pts',(108.04885397136,10.433269653595,13.0221176489899));
#103131=CARTESIAN_POINT('Ctrl Pts',(108.121762890827,10.1166810899737,13.040104990104));
#103132=CARTESIAN_POINT('Ctrl Pts',(108.268031420165,9.83869284548097,13.0580923312181));
#103133=CARTESIAN_POINT('Ctrl Pts',(108.565648458999,9.27306168386946,13.0946917229199));
#103134=CARTESIAN_POINT('Ctrl Pts',(109.16698369,8.86724079337956,13.1312911146217));
#103135=CARTESIAN_POINT('Ctrl Pts',(109.802886885463,8.80286509693592,13.1678905063235));
#103136=CARTESIAN_POINT('Ctrl Pts',(110.438790080927,8.73848940049229,13.2044898980253));
#103137=CARTESIAN_POINT('Ctrl Pts',(111.109261240853,9.01555889809494,13.2410892897271));
#103138=CARTESIAN_POINT('Ctrl Pts',(111.514197467183,9.51007429098298,13.2776886814289));
#103139=CARTESIAN_POINT('Ctrl Pts',(111.919133693514,10.004589683871,13.3142880731307));
#103140=CARTESIAN_POINT('Ctrl Pts',(112.058534986249,10.7165509720445,13.3508874648325));
#103141=CARTESIAN_POINT('Ctrl Pts',(111.870017324534,11.3272598408929,13.3874868565343));
#103142=CARTESIAN_POINT('Ctrl Pts',(111.68149966282,11.9379687097414,13.4240862482361));
#103143=CARTESIAN_POINT('Ctrl Pts',(111.165063046655,12.447425159265,13.4606856399379));
#103144=CARTESIAN_POINT('Ctrl Pts',(110.551838236876,12.6276618241303,13.4972850316397));
#103145=CARTESIAN_POINT('Ctrl Pts',(109.938613427096,12.8078984889955,13.5338844233415));
#103146=CARTESIAN_POINT('Ctrl Pts',(109.228600423702,12.6589153692025,13.5704838150433));
#103147=CARTESIAN_POINT('Ctrl Pts',(108.739640464735,12.2472714195058,13.6070832067451));
#103148=CARTESIAN_POINT('Ctrl Pts',(108.307464369448,11.8834324761199,13.6394322404553));
#103149=CARTESIAN_POINT('Ctrl Pts',(108.047979944815,11.3143969128506,13.6717812741655));
#103150=CARTESIAN_POINT('Ctrl Pts',(108.043923528227,10.7487415210877,13.7041303078758));
#103151=CARTESIAN_POINT('Origin',(110.,10.75,5.2859437743963));
#103152=CARTESIAN_POINT('',(108.446841388827,10.7497513433749,13.3359437743963));
#103153=CARTESIAN_POINT('',(108.442847005198,10.7489981760756,13.4740562256037));
#103154=CARTESIAN_POINT('',(108.4445,10.7499999999999,5.2859437743963));
#103155=CARTESIAN_POINT('',(109.142424689894,12.0477460604818,13.926));
#103156=CARTESIAN_POINT('Ctrl Pts',(108.446841388827,10.7497513433749,13.3359437743963));
#103157=CARTESIAN_POINT('Ctrl Pts',(108.446498609576,10.508994777646,13.3531248017756));
#103158=CARTESIAN_POINT('Ctrl Pts',(108.611548063658,9.7558240105893,13.4069052208568));
#103159=CARTESIAN_POINT('Ctrl Pts',(109.77603224924,8.93263191544926,13.4972850316397));
#103160=CARTESIAN_POINT('Ctrl Pts',(111.391303493381,9.55927115209057,13.6070832067451));
#103161=CARTESIAN_POINT('Ctrl Pts',(111.760894725706,11.2522029880481,13.7168813818505));
#103162=CARTESIAN_POINT('Ctrl Pts',(110.592954496938,12.4552890943434,13.8231869796021));
#103163=CARTESIAN_POINT('Ctrl Pts',(109.526460624714,12.3008132614142,13.892893185652));
#103164=CARTESIAN_POINT('Ctrl Pts',(109.140566776777,12.049156215532,13.926));
#103165=CARTESIAN_POINT('',(110.948473540785,11.982873956425,13.926));
#103166=CARTESIAN_POINT('Origin',(110.,10.75,13.926));
#103167=CARTESIAN_POINT('Ctrl Pts',(108.442847005198,10.7489981760756,13.4740562256037));
#103168=CARTESIAN_POINT('Ctrl Pts',(108.442422725546,10.6898336234053,13.4783065835953));
#103169=CARTESIAN_POINT('Ctrl Pts',(108.472082002041,10.1216556996131,13.5191563332887));
#103170=CARTESIAN_POINT('Ctrl Pts',(109.169225983483,9.11850985467691,13.5966054746838));
#103171=CARTESIAN_POINT('Ctrl Pts',(110.901845461742,9.15519245562723,13.7064036497892));
#103172=CARTESIAN_POINT('Ctrl Pts',(111.825924765157,10.6229447474917,13.8162018248946));
#103173=CARTESIAN_POINT('Ctrl Pts',(111.353491586843,11.6712858186231,13.8894006082982));
#103174=CARTESIAN_POINT('Ctrl Pts',(110.948473540785,11.982873956425,13.926));
#103175=CARTESIAN_POINT('Origin',(110.,10.75,5.2859437743963));
#103176=CARTESIAN_POINT('',(108.443326655324,10.7511424640687,12.6359437743963));
#103177=CARTESIAN_POINT('',(108.446872770028,10.7499311173313,12.7740562256037));
#103178=CARTESIAN_POINT('',(108.4445,10.7499999999999,5.2859437743963));
#103179=CARTESIAN_POINT('Ctrl Pts',(108.443326655324,10.7511424640687,12.6359437743963));
#103180=CARTESIAN_POINT('Ctrl Pts',(108.446888149401,10.3203834015993,12.6668617848982));
#103181=CARTESIAN_POINT('Ctrl Pts',(108.854614518196,9.37378473252757,12.7343791871019));
#103182=CARTESIAN_POINT('Ctrl Pts',(110.448258777128,8.97455089128206,12.8384959810074));
#103183=CARTESIAN_POINT('Ctrl Pts',(111.727591360803,10.1428830739091,12.9482941561128));
#103184=CARTESIAN_POINT('Ctrl Pts',(111.460408770971,11.8547018853006,13.0580923312181));
#103185=CARTESIAN_POINT('Ctrl Pts',(109.885897474817,12.5775985297513,13.1678905063236));
#103186=CARTESIAN_POINT('Ctrl Pts',(108.643912399514,11.8073629977093,13.2605076540496));
#103187=CARTESIAN_POINT('Ctrl Pts',(108.447228805263,11.0218595592065,13.3165254100738));
#103188=CARTESIAN_POINT('Ctrl Pts',(108.446841388827,10.7497513433749,13.3359437743963));
#103189=CARTESIAN_POINT('Ctrl Pts',(108.446872770028,10.7499311173313,12.7740562256037));
#103190=CARTESIAN_POINT('Ctrl Pts',(108.446771930629,10.4978638414365,12.7920435667178));
#103191=CARTESIAN_POINT('Ctrl Pts',(108.622907167769,9.7330410716517,12.8466302995338));
#103192=CARTESIAN_POINT('Ctrl Pts',(109.815568107276,8.92815438021742,12.9378164240515));
#103193=CARTESIAN_POINT('Ctrl Pts',(111.416772645554,9.58984568552079,13.0476145991569));
#103194=CARTESIAN_POINT('Ctrl Pts',(111.749687759447,11.2901360392881,13.1574127742623));
#103195=CARTESIAN_POINT('Ctrl Pts',(110.516345144641,12.5068087730147,13.2672109493676));
#103196=CARTESIAN_POINT('Ctrl Pts',(108.886346860443,12.1647837277323,13.3727587664815));
#103197=CARTESIAN_POINT('Ctrl Pts',(108.446076153613,11.1992934482799,13.4417071918935));
#103198=CARTESIAN_POINT('Ctrl Pts',(108.442847005198,10.7489981760756,13.4740562256037));
#103199=CARTESIAN_POINT('Origin',(110.,10.75,5.2859437743963));
#103200=CARTESIAN_POINT('',(108.444269738597,10.7486768364944,11.9359437743963));
#103201=CARTESIAN_POINT('',(108.443033037933,10.7510331927338,12.0740562256037));
#103202=CARTESIAN_POINT('',(108.4445,10.7499999999999,5.2859437743963));
#103203=CARTESIAN_POINT('Ctrl Pts',(108.444269738597,10.7486768364944,11.9359437743963));
#103204=CARTESIAN_POINT('Ctrl Pts',(108.443272631709,10.6362675651798,11.9439993763189));
#103205=CARTESIAN_POINT('Ctrl Pts',(108.505232777979,10.0142334536265,11.9886543699434));
#103206=CARTESIAN_POINT('Ctrl Pts',(109.340676086711,9.04165274898235,12.0699087552696));
#103207=CARTESIAN_POINT('Ctrl Pts',(111.059817873312,9.25670017301735,12.179706930375));
#103208=CARTESIAN_POINT('Ctrl Pts',(111.830227612529,10.8085257640398,12.2895051054804));
#103209=CARTESIAN_POINT('Ctrl Pts',(110.962246723952,12.3079600977483,12.3993032805858));
#103210=CARTESIAN_POINT('Ctrl Pts',(109.232877989319,12.4127332342713,12.5091014556912));
#103211=CARTESIAN_POINT('Ctrl Pts',(108.483824735014,11.4186837877046,12.5879816202947));
#103212=CARTESIAN_POINT('Ctrl Pts',(108.442672208121,10.8302971832592,12.6302623931964));
#103213=CARTESIAN_POINT('Ctrl Pts',(108.443326655324,10.7511424640687,12.6359437743963));
#103214=CARTESIAN_POINT('Ctrl Pts',(108.443033037933,10.7510331927338,12.0740562256037));
#103215=CARTESIAN_POINT('Ctrl Pts',(108.446441418747,10.3092579555816,12.1057805498404));
#103216=CARTESIAN_POINT('Ctrl Pts',(108.872356835445,9.35206525720305,12.1741042657789));
#103217=CARTESIAN_POINT('Ctrl Pts',(110.486699725726,8.98470055506267,12.2790273734191));
#103218=CARTESIAN_POINT('Ctrl Pts',(111.74036449784,10.1805344965231,12.3888255485245));
#103219=CARTESIAN_POINT('Ctrl Pts',(111.436082469949,11.8861455476417,12.4986237236299));
#103220=CARTESIAN_POINT('Ctrl Pts',(109.846242795973,12.5746958549649,12.6084218987353));
#103221=CARTESIAN_POINT('Ctrl Pts',(108.63194517067,11.7846031923792,12.7002327327266));
#103222=CARTESIAN_POINT('Ctrl Pts',(108.44697711163,11.010752817475,12.755444175016));
#103223=CARTESIAN_POINT('Ctrl Pts',(108.446872770028,10.7499311173313,12.7740562256037));
#103224=CARTESIAN_POINT('Origin',(110.,10.75,5.2859437743963));
#103225=CARTESIAN_POINT('',(108.446518113323,10.7507233568205,11.2359437743963));
#103226=CARTESIAN_POINT('',(108.444596502233,10.7486652631983,11.3740562256037));
#103227=CARTESIAN_POINT('',(108.4445,10.7499999999999,5.2859437743963));
#103228=CARTESIAN_POINT('Ctrl Pts',(108.446518113323,10.7507233568205,11.2359437743963));
#103229=CARTESIAN_POINT('Ctrl Pts',(108.447833256565,10.4455062321144,11.2577363594415));
#103230=CARTESIAN_POINT('Ctrl Pts',(108.68120743127,9.62583808482625,11.3161283361885));
#103231=CARTESIAN_POINT('Ctrl Pts',(110.002891673014,8.91883917199709,11.4111197046373));
#103232=CARTESIAN_POINT('Ctrl Pts',(111.528005243266,9.74086258836599,11.5209178797427));
#103233=CARTESIAN_POINT('Ctrl Pts',(111.685272875053,11.4662497303801,11.630716054848));
#103234=CARTESIAN_POINT('Ctrl Pts',(110.333911090238,12.5504615311719,11.7405142299534));
#103235=CARTESIAN_POINT('Ctrl Pts',(108.80471363849,12.061632542384,11.8422568031362));
#103236=CARTESIAN_POINT('Ctrl Pts',(108.447802833911,11.1469818471499,11.9073999846171));
#103237=CARTESIAN_POINT('Ctrl Pts',(108.444269738597,10.7486768364944,11.9359437743963));
#103238=CARTESIAN_POINT('Ctrl Pts',(108.444596502233,10.7486652631983,11.3740562256037));
#103239=CARTESIAN_POINT('Ctrl Pts',(108.443512691792,10.6249377906722,11.3829181412611));
#103240=CARTESIAN_POINT('Ctrl Pts',(108.513060951864,9.99142337839694,11.4283794486203));
#103241=CARTESIAN_POINT('Ctrl Pts',(109.377920764104,9.02774086435358,11.5104401476814));
#103242=CARTESIAN_POINT('Ctrl Pts',(111.091988723841,9.28006131881894,11.6202383227868));
#103243=CARTESIAN_POINT('Ctrl Pts',(111.82852578498,10.8482474465615,11.7300364978922));
#103244=CARTESIAN_POINT('Ctrl Pts',(110.928195705052,12.3284840355239,11.8398346729976));
#103245=CARTESIAN_POINT('Ctrl Pts',(109.196959631481,12.3956868563535,11.9496328481029));
#103246=CARTESIAN_POINT('Ctrl Pts',(108.477098834361,11.3959340229695,12.0277066989717));
#103247=CARTESIAN_POINT('Ctrl Pts',(108.442509273068,10.8189206619663,12.0691811581386));
#103248=CARTESIAN_POINT('Ctrl Pts',(108.443033037933,10.7510331927338,12.0740562256037));
#103249=CARTESIAN_POINT('Origin',(110.,10.75,5.2859437743963));
#103250=CARTESIAN_POINT('',(108.442099939192,10.7502618635012,10.5359437743963));
#103251=CARTESIAN_POINT('',(108.446339520596,10.7508655742063,10.6740562256037));
#103252=CARTESIAN_POINT('',(108.4445,10.7499999999999,5.2859437743963));
#103253=CARTESIAN_POINT('Ctrl Pts',(108.442099939192,10.7502618635012,10.5359437743963));
#103254=CARTESIAN_POINT('Ctrl Pts',(108.443275329712,10.2562813278079,10.571473342564));
#103255=CARTESIAN_POINT('Ctrl Pts',(108.961660747072,9.2513179908291,10.6436023024336));
#103256=CARTESIAN_POINT('Ctrl Pts',(110.664716078704,9.04374360829103,10.7523306540049));
#103257=CARTESIAN_POINT('Ctrl Pts',(111.789485242344,10.3615403406303,10.8621288291103));
#103258=CARTESIAN_POINT('Ctrl Pts',(111.312335739819,12.0270799683344,10.9719270042157));
#103259=CARTESIAN_POINT('Ctrl Pts',(109.660404200444,12.5493979639002,11.0817251793211));
#103260=CARTESIAN_POINT('Ctrl Pts',(108.580008787355,11.67696242414,11.1697307693813));
#103261=CARTESIAN_POINT('Ctrl Pts',(108.44562454922,10.9581008177522,11.2211369677397));
#103262=CARTESIAN_POINT('Ctrl Pts',(108.446518113323,10.7507233568205,11.2359437743963));
#103263=CARTESIAN_POINT('Ctrl Pts',(108.446339520596,10.7508655742063,10.6740562256037));
#103264=CARTESIAN_POINT('Ctrl Pts',(108.447983384872,10.4344469463554,10.6966551243837));
#103265=CARTESIAN_POINT('Ctrl Pts',(108.694577946579,9.60322729218201,10.7558534148655));
#103266=CARTESIAN_POINT('Ctrl Pts',(110.042646705583,8.91933335565637,10.851651097049));
#103267=CARTESIAN_POINT('Ctrl Pts',(111.549554301631,9.77427433649753,10.9614492721544));
#103268=CARTESIAN_POINT('Ctrl Pts',(111.669325585378,11.5026693790562,11.0712474472598));
#103269=CARTESIAN_POINT('Ctrl Pts',(110.294743212587,12.5572867904855,11.1810456223652));
#103270=CARTESIAN_POINT('Ctrl Pts',(108.788550810402,12.0395092632441,11.2819818818132));
#103271=CARTESIAN_POINT('Ctrl Pts',(108.447988789783,11.1359277849703,11.3463187495593));
#103272=CARTESIAN_POINT('Ctrl Pts',(108.444596502233,10.7486652631983,11.3740562256037));
#103273=CARTESIAN_POINT('Origin',(110.,10.75,5.2859437743963));
#103274=CARTESIAN_POINT('',(108.445976253612,10.7489330703828,9.8359437743963));
#103275=CARTESIAN_POINT('',(108.442045063917,10.7500649832092,9.97405622560371));
#103276=CARTESIAN_POINT('',(108.4445,10.7499999999999,5.2859437743963));
#103277=CARTESIAN_POINT('Ctrl Pts',(108.445976253612,10.7489330703828,9.8359437743963));
#103278=CARTESIAN_POINT('Ctrl Pts',(108.444822676107,10.571678333824,9.84861093398479));
#103279=CARTESIAN_POINT('Ctrl Pts',(108.55398870796,9.88365650751954,9.89787748527507));
#103280=CARTESIAN_POINT('Ctrl Pts',(109.557350442899,8.97314330652884,9.98374342826716));
#103281=CARTESIAN_POINT('Ctrl Pts',(111.236618208315,9.39946908721214,10.0935416033726));
#103282=CARTESIAN_POINT('Ctrl Pts',(111.808885064222,11.0347686147797,10.2033397784779));
#103283=CARTESIAN_POINT('Ctrl Pts',(110.761866842631,12.4151478173515,10.3131379535833));
#103284=CARTESIAN_POINT('Ctrl Pts',(109.032837566985,12.3049132347807,10.4229361286887));
#103285=CARTESIAN_POINT('Ctrl Pts',(108.44893261916,11.288831373407,10.4972047356264));
#103286=CARTESIAN_POINT('Ctrl Pts',(108.442064547249,10.7651360100137,10.5348739508622));
#103287=CARTESIAN_POINT('Ctrl Pts',(108.442099939192,10.7502618635012,10.5359437743963));
#103288=CARTESIAN_POINT('Ctrl Pts',(108.442045063917,10.7500649832092,9.97405622560371));
#103289=CARTESIAN_POINT('Ctrl Pts',(108.442360161907,10.2449217412237,10.0103921075062));
#103290=CARTESIAN_POINT('Ctrl Pts',(108.98178269135,9.23039281468085,10.0833273811105));
#103291=CARTESIAN_POINT('Ctrl Pts',(110.701603433992,9.05857701162966,10.1928620464167));
#103292=CARTESIAN_POINT('Ctrl Pts',(111.797497373615,10.4004827672002,10.3026602215221));
#103293=CARTESIAN_POINT('Ctrl Pts',(111.284300314861,12.0552707785837,10.4124583966274));
#103294=CARTESIAN_POINT('Ctrl Pts',(109.621418084829,12.5416011938169,10.5222565717329));
#103295=CARTESIAN_POINT('Ctrl Pts',(108.569941145921,11.654121434041,10.6094558480583));
#103296=CARTESIAN_POINT('Ctrl Pts',(108.445321112116,10.9468935666625,10.6600557326819));
#103297=CARTESIAN_POINT('Ctrl Pts',(108.446339520596,10.7508655742063,10.6740562256037));
#103298=CARTESIAN_POINT('Origin',(110.,10.75,5.2859437743963));
#103299=CARTESIAN_POINT('',(108.445121586218,10.7512991519358,9.1359437743963));
#103300=CARTESIAN_POINT('',(108.446205554653,10.7490493704098,9.2740562256037));
#103301=CARTESIAN_POINT('',(108.4445,10.7499999999999,5.2859437743963));
#103302=CARTESIAN_POINT('Ctrl Pts',(108.445121586218,10.7512991519358,9.1359437743963));
#103303=CARTESIAN_POINT('Ctrl Pts',(108.448172895975,10.3823342510321,9.16234791710734));
#103304=CARTESIAN_POINT('Ctrl Pts',(108.762681159919,9.49725890698745,9.22535145152017));
#103305=CARTESIAN_POINT('Ctrl Pts',(110.229678498517,8.93329800817414,9.32495437763481));
#103306=CARTESIAN_POINT('Ctrl Pts',(111.641231584828,9.93789334168282,9.4347525527402));
#103307=CARTESIAN_POINT('Ctrl Pts',(111.583580316096,11.6694736113398,9.5445507278456));
#103308=CARTESIAN_POINT('Ctrl Pts',(110.108333189259,12.577955759768,9.65434890295098));
#103309=CARTESIAN_POINT('Ctrl Pts',(108.717491883739,11.9340542572433,9.75147991846789));
#103310=CARTESIAN_POINT('Ctrl Pts',(108.448155722847,11.0838227880714,9.81201154228299));
#103311=CARTESIAN_POINT('Ctrl Pts',(108.445976253612,10.7489330703828,9.8359437743963));
#103312=CARTESIAN_POINT('Ctrl Pts',(108.446205554653,10.7490493704098,9.2740562256037));
#103313=CARTESIAN_POINT('Ctrl Pts',(108.445123112026,10.5604414071891,9.28752969892698));
#103314=CARTESIAN_POINT('Ctrl Pts',(108.563532910115,9.86081023996671,9.33760256395205));
#103315=CARTESIAN_POINT('Ctrl Pts',(109.596031461916,8.9639517015356,9.42427482067892));
#103316=CARTESIAN_POINT('Ctrl Pts',(111.265647793446,9.42663505898133,9.53407299578432));
#103317=CARTESIAN_POINT('Ctrl Pts',(111.802276393556,11.073973618372,9.6438711708897));
#103318=CARTESIAN_POINT('Ctrl Pts',(110.725535892815,12.4312961584497,9.7536693459951));
#103319=CARTESIAN_POINT('Ctrl Pts',(108.99930722521,12.2835491758203,9.86346752110049));
#103320=CARTESIAN_POINT('Ctrl Pts',(108.443697953399,11.266196081649,9.93692981430336));
#103321=CARTESIAN_POINT('Ctrl Pts',(108.442042778809,10.7537283095778,9.97379271580443));
#103322=CARTESIAN_POINT('Ctrl Pts',(108.442045063917,10.7500649832092,9.97405622560371));
#103323=CARTESIAN_POINT('Origin',(110.,10.75,5.2859437743963));
#103324=CARTESIAN_POINT('',(108.442605213692,10.749194935846,8.4359437743963));
#103325=CARTESIAN_POINT('',(108.444807264591,10.7513287041109,8.5740562256037));
#103326=CARTESIAN_POINT('',(108.4445,10.7499999999999,5.2859437743963));
#103327=CARTESIAN_POINT('Ctrl Pts',(108.442605213692,10.749194935846,8.4359437743963));
#103328=CARTESIAN_POINT('Ctrl Pts',(108.442290979397,10.6999103733631,8.43948550852809));
#103329=CARTESIAN_POINT('Ctrl Pts',(108.466566776117,10.1416447851508,8.47962663436168));
#103330=CARTESIAN_POINT('Ctrl Pts',(109.138403361389,9.13420003397936,8.55636715189706));
#103331=CARTESIAN_POINT('Ctrl Pts',(110.870935822764,9.13921474264243,8.66616532700245));
#103332=CARTESIAN_POINT('Ctrl Pts',(111.823820425147,10.5861787581841,8.77596350210785));
#103333=CARTESIAN_POINT('Ctrl Pts',(111.144050049243,12.179792928921,8.88576167721324));
#103334=CARTESIAN_POINT('Ctrl Pts',(109.440144306221,12.4934792638734,8.99555985231863));
#103335=CARTESIAN_POINT('Ctrl Pts',(108.526644069975,11.5463195852755,9.07895388471298));
#103336=CARTESIAN_POINT('Ctrl Pts',(108.443943405087,10.8937650170363,9.12574852540554));
#103337=CARTESIAN_POINT('Ctrl Pts',(108.445121586218,10.7512991519358,9.1359437743963));
#103338=CARTESIAN_POINT('Ctrl Pts',(108.444807264591,10.7513287041109,8.5740562256037));
#103339=CARTESIAN_POINT('Ctrl Pts',(108.448079287351,10.3712924955763,8.60126668204952));
#103340=CARTESIAN_POINT('Ctrl Pts',(108.778198422012,9.47499754635645,8.66507653019715));
#103341=CARTESIAN_POINT('Ctrl Pts',(110.269066191156,8.93871247704089,8.76548577004656));
#103342=CARTESIAN_POINT('Ctrl Pts',(111.658476300169,9.97371689050704,8.87528394515196));
#103343=CARTESIAN_POINT('Ctrl Pts',(111.563244859267,11.7036375693259,8.98508212025735));
#103344=CARTESIAN_POINT('Ctrl Pts',(110.068621537362,12.5798770967034,9.09488029536274));
#103345=CARTESIAN_POINT('Ctrl Pts',(108.703514451318,11.9115258327128,9.19120499714486));
#103346=CARTESIAN_POINT('Ctrl Pts',(108.448063463097,11.0727767611375,9.25093030722518));
#103347=CARTESIAN_POINT('Ctrl Pts',(108.446205554653,10.7490493704098,9.2740562256037));
#103348=CARTESIAN_POINT('Origin',(110.,10.75,5.2859437743963));
#103349=CARTESIAN_POINT('',(108.446844740062,10.7497785244693,7.7359437743963));
#103350=CARTESIAN_POINT('',(108.442854064965,10.7490502583051,7.8740562256037));
#103351=CARTESIAN_POINT('',(108.4445,10.7499999999999,5.2859437743963));
#103352=CARTESIAN_POINT('Ctrl Pts',(108.446844740062,10.7497785244693,7.7359437743963));
#103353=CARTESIAN_POINT('Ctrl Pts',(108.446528563922,10.5076526407742,7.75322249165064));
#103354=CARTESIAN_POINT('Ctrl Pts',(108.612900212043,9.75307183152967,7.80710060060678));
#103355=CARTESIAN_POINT('Ctrl Pts',(109.780842261901,8.93199962740631,7.8975781012647));
#103356=CARTESIAN_POINT('Ctrl Pts',(111.394373478833,9.56303689824699,8.0073762763701));
#103357=CARTESIAN_POINT('Ctrl Pts',(111.759684322617,11.256625962536,8.11717445147549));
#103358=CARTESIAN_POINT('Ctrl Pts',(110.549753543119,12.4966908797639,8.22697262658089));
#103359=CARTESIAN_POINT('Ctrl Pts',(108.902595277997,12.1835827892781,8.33322906755448));
#103360=CARTESIAN_POINT('Ctrl Pts',(108.445538197739,11.2092046738507,8.40288611682629));
#103361=CARTESIAN_POINT('Ctrl Pts',(108.442605213692,10.749194935846,8.4359437743963));
#103362=CARTESIAN_POINT('Ctrl Pts',(108.442854064965,10.7490502583051,7.8740562256037));
#103363=CARTESIAN_POINT('Ctrl Pts',(108.442415170989,10.6885200197988,7.87840427347028));
#103364=CARTESIAN_POINT('Ctrl Pts',(108.472848633662,10.1189256629246,7.91935171303865));
#103365=CARTESIAN_POINT('Ctrl Pts',(109.173686477906,9.11587493853038,7.99689854430882));
#103366=CARTESIAN_POINT('Ctrl Pts',(110.90570183064,9.15850278599423,8.10669671941421));
#103367=CARTESIAN_POINT('Ctrl Pts',(111.8269474297,10.6258137189513,8.2164948945196));
#103368=CARTESIAN_POINT('Ctrl Pts',(111.112738765821,12.2042941592694,8.32629306962499));
#103369=CARTESIAN_POINT('Ctrl Pts',(109.402424116335,12.4809136837355,8.43609124473039));
#103370=CARTESIAN_POINT('Ctrl Pts',(108.518334029221,11.5234918702337,8.51867896338995));
#103371=CARTESIAN_POINT('Ctrl Pts',(108.443678257074,10.8824597405917,8.56466729034773));
#103372=CARTESIAN_POINT('Ctrl Pts',(108.444807264591,10.7513287041109,8.5740562256037));
#103373=CARTESIAN_POINT('Origin',(110.,10.75,5.2859437743963));
#103374=CARTESIAN_POINT('',(108.443317976897,10.7511999786121,7.0359437743963));
#103375=CARTESIAN_POINT('',(108.446877037961,10.7499579969204,7.17405622560371));
#103376=CARTESIAN_POINT('',(108.4445,10.7499999999999,5.2859437743963));
#103377=CARTESIAN_POINT('Ctrl Pts',(108.443317976897,10.7511999786121,7.0359437743963));
#103378=CARTESIAN_POINT('Ctrl Pts',(108.446869824562,10.3191164320538,7.06695947477319));
#103379=CARTESIAN_POINT('Ctrl Pts',(108.856701971244,9.37104702086914,7.13457456685187));
#103380=CARTESIAN_POINT('Ctrl Pts',(110.452949548444,8.97578890357189,7.23878905063235));
#103381=CARTESIAN_POINT('Ctrl Pts',(111.729171099463,10.1474049425682,7.34858722573775));
#103382=CARTESIAN_POINT('Ctrl Pts',(111.457504537093,11.8585497627777,7.45838540084314));
#103383=CARTESIAN_POINT('Ctrl Pts',(109.881084321976,12.5772916662981,7.56818357594853));
#103384=CARTESIAN_POINT('Ctrl Pts',(108.642449345411,11.8046002560737,7.66070303379958));
#103385=CARTESIAN_POINT('Ctrl Pts',(108.447198281137,11.0205182619924,7.71662309994884));
#103386=CARTESIAN_POINT('Ctrl Pts',(108.446844740062,10.7497785244693,7.7359437743963));
#103387=CARTESIAN_POINT('Ctrl Pts',(108.446877037961,10.7499579969204,7.17405622560371));
#103388=CARTESIAN_POINT('Ctrl Pts',(108.446805685801,10.4965188357708,7.19214125659283));
#103389=CARTESIAN_POINT('Ctrl Pts',(108.624301182411,9.73027362155383,7.24682567928375));
#103390=CARTESIAN_POINT('Ctrl Pts',(109.82036714101,8.92767494081165,7.33810949367647));
#103391=CARTESIAN_POINT('Ctrl Pts',(111.41981313278,9.59358681487167,7.44790766878186));
#103392=CARTESIAN_POINT('Ctrl Pts',(111.748271359623,11.29471174246,7.55770584388725));
#103393=CARTESIAN_POINT('Ctrl Pts',(110.511701824797,12.5082142882526,7.66750401899264));
#103394=CARTESIAN_POINT('Ctrl Pts',(108.884174677395,12.1620667174056,7.77295414623146));
#103395=CARTESIAN_POINT('Ctrl Pts',(108.446109530629,11.1980291091366,7.84180488176848));
#103396=CARTESIAN_POINT('Ctrl Pts',(108.442854064965,10.7490502583051,7.8740562256037));
#103397=CARTESIAN_POINT('Origin',(110.,10.75,13.926));
#103398=CARTESIAN_POINT('',(109.07607384819,9.02823449157528,13.926));
#103399=CARTESIAN_POINT('Ctrl Pts',(109.140566776777,12.049156215532,13.926));
#103400=CARTESIAN_POINT('Ctrl Pts',(109.096212441881,12.0275126749281,13.926));
#103401=CARTESIAN_POINT('Ctrl Pts',(109.053058974181,12.0037020680889,13.926));
#103402=CARTESIAN_POINT('Ctrl Pts',(109.011284708367,11.9777581097249,13.926));
#103403=CARTESIAN_POINT('Ctrl Pts',(108.960679148907,11.9463294657494,13.926));
#103404=CARTESIAN_POINT('Ctrl Pts',(108.912096233717,11.9117718230936,13.926));
#103405=CARTESIAN_POINT('Ctrl Pts',(108.86562338902,11.8743978959904,13.926));
#103406=CARTESIAN_POINT('Ctrl Pts',(108.850452021899,11.8621969306191,13.926));
#103407=CARTESIAN_POINT('Ctrl Pts',(108.835505668127,11.8496954296351,13.926));
#103408=CARTESIAN_POINT('Ctrl Pts',(108.820787810844,11.8369031865342,13.926));
#103409=CARTESIAN_POINT('Ctrl Pts',(108.80591914035,11.8239798619021,13.926));
#103410=CARTESIAN_POINT('Ctrl Pts',(108.791278940907,11.810755083877,13.926));
#103411=CARTESIAN_POINT('Ctrl Pts',(108.77689730581,11.797263909003,13.926));
#103412=CARTESIAN_POINT('Ctrl Pts',(108.731524838567,11.7547007452223,13.926));
#103413=CARTESIAN_POINT('Ctrl Pts',(108.688682887307,11.7094570944331,13.926));
#103414=CARTESIAN_POINT('Ctrl Pts',(108.648464424372,11.6618791784732,13.926));
#103415=CARTESIAN_POINT('Ctrl Pts',(108.616938129699,11.6245839839531,13.926));
#103416=CARTESIAN_POINT('Ctrl Pts',(108.58702407997,11.5858532354006,13.926));
#103417=CARTESIAN_POINT('Ctrl Pts',(108.558777269814,11.5458338354115,13.926));
#103418=CARTESIAN_POINT('Ctrl Pts',(108.546234964393,11.5280641993131,13.926));
#103419=CARTESIAN_POINT('Ctrl Pts',(108.53402150688,11.5100402877822,13.926));
#103420=CARTESIAN_POINT('Ctrl Pts',(108.522142432535,11.4917740517978,13.926));
#103421=CARTESIAN_POINT('Ctrl Pts',(108.515052248395,11.4808716049466,13.926));
#103422=CARTESIAN_POINT('Ctrl Pts',(108.508085351031,11.469889115632,13.926));
#103423=CARTESIAN_POINT('Ctrl Pts',(108.501246091907,11.4588352992566,13.926));
#103424=CARTESIAN_POINT('Ctrl Pts',(108.46722064447,11.4038423473526,13.926));
#103425=CARTESIAN_POINT('Ctrl Pts',(108.436323746455,11.3470439400103,13.926));
#103426=CARTESIAN_POINT('Ctrl Pts',(108.408653404881,11.2887905666606,13.926));
#103427=CARTESIAN_POINT('Ctrl Pts',(108.380421099685,11.2293541115438,13.926));
#103428=CARTESIAN_POINT('Ctrl Pts',(108.355546974404,11.1684022291955,13.926));
#103429=CARTESIAN_POINT('Ctrl Pts',(108.334168214284,11.1062649443926,13.926));
#103430=CARTESIAN_POINT('Ctrl Pts',(108.319757574467,11.0643804746918,13.926));
#103431=CARTESIAN_POINT('Ctrl Pts',(108.306935789132,11.0219565288301,13.926));
#103432=CARTESIAN_POINT('Ctrl Pts',(108.295755797419,10.9790864894013,13.926));
#103433=CARTESIAN_POINT('Ctrl Pts',(108.28804833841,10.9495319888175,13.926));
#103434=CARTESIAN_POINT('Ctrl Pts',(108.281121359323,10.919765349962,13.926));
#103435=CARTESIAN_POINT('Ctrl Pts',(108.274995069302,10.8898160442948,13.926));
#103436=CARTESIAN_POINT('Ctrl Pts',(108.273006324846,10.8800937628803,13.926));
#103437=CARTESIAN_POINT('Ctrl Pts',(108.27110240947,10.8703540703402,13.926));
#103438=CARTESIAN_POINT('Ctrl Pts',(108.269285497152,10.8606070238497,13.926));
#103439=CARTESIAN_POINT('Ctrl Pts',(108.256865790514,10.7939800012846,13.926));
#103440=CARTESIAN_POINT('Ctrl Pts',(108.248483734475,10.7268949524802,13.926));
#103441=CARTESIAN_POINT('Ctrl Pts',(108.244266995922,10.659703975981,13.926));
#103442=CARTESIAN_POINT('Ctrl Pts',(108.242731581514,10.6352381495744,13.926));
#103443=CARTESIAN_POINT('Ctrl Pts',(108.241748823705,10.6107579684671,13.926));
#103444=CARTESIAN_POINT('Ctrl Pts',(108.24132633562,10.5862795120633,13.926));
#103445=CARTESIAN_POINT('Ctrl Pts',(108.240204685504,10.521292440333,13.926));
#103446=CARTESIAN_POINT('Ctrl Pts',(108.243028159913,10.4563182246449,13.926));
#103447=CARTESIAN_POINT('Ctrl Pts',(108.249591140909,10.391599767868,13.926));
#103448=CARTESIAN_POINT('Ctrl Pts',(108.253023120763,10.3577565432754,13.926));
#103449=CARTESIAN_POINT('Ctrl Pts',(108.257478553759,10.3239830677188,13.926));
#103450=CARTESIAN_POINT('Ctrl Pts',(108.26293352207,10.2903134507712,13.926));
#103451=CARTESIAN_POINT('Ctrl Pts',(108.265675912799,10.273386634687,13.926));
#103452=CARTESIAN_POINT('Ctrl Pts',(108.268670983993,10.2564860659407,13.926));
#103453=CARTESIAN_POINT('Ctrl Pts',(108.271916040856,10.2396160874463,13.926));
#103454=CARTESIAN_POINT('Ctrl Pts',(108.274212856499,10.2276757017639,13.926));
#103455=CARTESIAN_POINT('Ctrl Pts',(108.276635216349,10.2157492185281,13.926));
#103456=CARTESIAN_POINT('Ctrl Pts',(108.279181283577,10.2038426088341,13.926));
#103457=CARTESIAN_POINT('Ctrl Pts',(108.293323163217,10.1377085180316,13.926));
#103458=CARTESIAN_POINT('Ctrl Pts',(108.311217290379,10.0724644861745,13.926));
#103459=CARTESIAN_POINT('Ctrl Pts',(108.332610647139,10.0083733770064,13.926));
#103460=CARTESIAN_POINT('Ctrl Pts',(108.354477710045,9.94286311923765,13.926));
#103461=CARTESIAN_POINT('Ctrl Pts',(108.380000809587,9.87855654185356,13.926));
#103462=CARTESIAN_POINT('Ctrl Pts',(108.408964920281,9.81572791433377,13.926));
#103463=CARTESIAN_POINT('Ctrl Pts',(108.438204666487,9.75230138131932,13.926));
#103464=CARTESIAN_POINT('Ctrl Pts',(108.470951499624,9.69038007622194,13.926));
#103465=CARTESIAN_POINT('Ctrl Pts',(108.507036609764,9.63025378709743,13.926));
#103466=CARTESIAN_POINT('Ctrl Pts',(108.521435797672,9.60626134999678,13.926));
#103467=CARTESIAN_POINT('Ctrl Pts',(108.53636709129,9.58255489670699,13.926));
#103468=CARTESIAN_POINT('Ctrl Pts',(108.551821908304,9.55915372538839,13.926));
#103469=CARTESIAN_POINT('Ctrl Pts',(108.55754106392,9.55049396964837,13.926));
#103470=CARTESIAN_POINT('Ctrl Pts',(108.563330918209,9.54187763709662,13.926));
#103471=CARTESIAN_POINT('Ctrl Pts',(108.569185682118,9.53331319880462,13.926));
#103472=CARTESIAN_POINT('Ctrl Pts',(108.60991484744,9.47373395213159,13.926));
#103473=CARTESIAN_POINT('Ctrl Pts',(108.653849190263,9.41656157277207,13.926));
#103474=CARTESIAN_POINT('Ctrl Pts',(108.700756166978,9.36208419964962,13.926));
#103475=CARTESIAN_POINT('Ctrl Pts',(108.747781963714,9.30746882994174,13.926));
#103476=CARTESIAN_POINT('Ctrl Pts',(108.797795870477,9.2555611149366,13.926));
#103477=CARTESIAN_POINT('Ctrl Pts',(108.850613754612,9.20666582811862,13.926));
#103478=CARTESIAN_POINT('Ctrl Pts',(108.902318938299,9.15880060542464,13.926));
#103479=CARTESIAN_POINT('Ctrl Pts',(108.956711742704,9.11382134718746,13.926));
#103480=CARTESIAN_POINT('Ctrl Pts',(109.013660238129,9.0720416880423,13.926));
#103481=CARTESIAN_POINT('Ctrl Pts',(109.034135713973,9.05702007254222,13.926));
#103482=CARTESIAN_POINT('Ctrl Pts',(109.054941918824,9.04241240218612,13.926));
#103483=CARTESIAN_POINT('Ctrl Pts',(109.07607384819,9.02823449157529,13.926));
#103484=CARTESIAN_POINT('',(108.046,10.75,13.926));
#103485=CARTESIAN_POINT('Origin',(110.,10.75,13.926));
#103486=CARTESIAN_POINT('',(110.799022681602,8.96531988605745,13.926));
#103487=CARTESIAN_POINT('Origin',(110.,10.75,13.926));
#103488=CARTESIAN_POINT('Ctrl Pts',(110.800030261768,8.96425629420691,13.926));
#103489=CARTESIAN_POINT('Ctrl Pts',(110.853254520143,8.99427974873486,13.926));
#103490=CARTESIAN_POINT('Ctrl Pts',(110.904869181937,9.02687709790755,13.926));
#103491=CARTESIAN_POINT('Ctrl Pts',(110.954657890784,9.06206156501285,13.926));
#103492=CARTESIAN_POINT('Ctrl Pts',(111.013441596184,9.10360257695933,13.926));
#103493=CARTESIAN_POINT('Ctrl Pts',(111.069681245781,9.14875005427251,13.926));
#103494=CARTESIAN_POINT('Ctrl Pts',(111.123200852482,9.19717009084562,13.926));
#103495=CARTESIAN_POINT('Ctrl Pts',(111.146304270927,9.21807211974725,13.926));
#103496=CARTESIAN_POINT('Ctrl Pts',(111.168900259238,9.23958434779001,13.926));
#103497=CARTESIAN_POINT('Ctrl Pts',(111.190972005754,9.26168122696303,13.926));
#103498=CARTESIAN_POINT('Ctrl Pts',(111.201661060319,9.27238245294035,13.926));
#103499=CARTESIAN_POINT('Ctrl Pts',(111.212227772727,9.28322163766534,13.926));
#103500=CARTESIAN_POINT('Ctrl Pts',(111.222658638307,9.2941834023316,13.926));
#103501=CARTESIAN_POINT('Ctrl Pts',(111.271809717873,9.34583612119508,13.926));
#103502=CARTESIAN_POINT('Ctrl Pts',(111.318010893287,9.40026995040382,13.926));
#103503=CARTESIAN_POINT('Ctrl Pts',(111.361098000433,9.45715214147117,13.926));
#103504=CARTESIAN_POINT('Ctrl Pts',(111.392784241534,9.49898328168631,13.926));
#103505=CARTESIAN_POINT('Ctrl Pts',(111.422785486411,9.54213928816585,13.926));
#103506=CARTESIAN_POINT('Ctrl Pts',(111.451019604943,9.58649413012682,13.926));
#103507=CARTESIAN_POINT('Ctrl Pts',(111.465995132324,9.61002017537955,13.926));
#103508=CARTESIAN_POINT('Ctrl Pts',(111.480473263727,9.63388355125054,13.926));
#103509=CARTESIAN_POINT('Ctrl Pts',(111.494439972729,9.65806567929226,13.926));
#103510=CARTESIAN_POINT('Ctrl Pts',(111.500869702427,9.66919819066671,13.926));
#103511=CARTESIAN_POINT('Ctrl Pts',(111.507191762579,9.6803997476648,13.926));
#103512=CARTESIAN_POINT('Ctrl Pts',(111.51339693583,9.69165399486125,13.926));
#103513=CARTESIAN_POINT('Ctrl Pts',(111.547016349844,9.75262911684645,13.926));
#103514=CARTESIAN_POINT('Ctrl Pts',(111.577261792345,9.81523933357153,13.926));
#103515=CARTESIAN_POINT('Ctrl Pts',(111.603978750335,9.87917776379081,13.926));
#103516=CARTESIAN_POINT('Ctrl Pts',(111.630092665242,9.94167300470077,13.926));
#103517=CARTESIAN_POINT('Ctrl Pts',(111.65283571523,10.005438163468,13.926));
#103518=CARTESIAN_POINT('Ctrl Pts',(111.672015533369,10.0701944516723,13.926));
#103519=CARTESIAN_POINT('Ctrl Pts',(111.685399646162,10.11538286061,13.926));
#103520=CARTESIAN_POINT('Ctrl Pts',(111.697047632966,10.161054073457,13.926));
#103521=CARTESIAN_POINT('Ctrl Pts',(111.706879216135,10.2071119606939,13.926));
#103522=CARTESIAN_POINT('Ctrl Pts',(111.71515302186,10.2458721486039,13.926));
#103523=CARTESIAN_POINT('Ctrl Pts',(111.722140229568,10.2849062042654,13.926));
#103524=CARTESIAN_POINT('Ctrl Pts',(111.727785830159,10.324154890653,13.926));
#103525=CARTESIAN_POINT('Ctrl Pts',(111.729386111696,10.3352801814318,13.926));
#103526=CARTESIAN_POINT('Ctrl Pts',(111.73087832549,10.3464216841658,13.926));
#103527=CARTESIAN_POINT('Ctrl Pts',(111.732259848983,10.3575652207405,13.926));
#103528=CARTESIAN_POINT('Ctrl Pts',(111.740282047033,10.4222732462359,13.926));
#103529=CARTESIAN_POINT('Ctrl Pts',(111.744593192869,10.4871654619733,13.926));
#103530=CARTESIAN_POINT('Ctrl Pts',(111.745022935266,10.5519847273788,13.926));
#103531=CARTESIAN_POINT('Ctrl Pts',(111.745188833282,10.5770075958328,13.926));
#103532=CARTESIAN_POINT('Ctrl Pts',(111.744775756678,10.6020195479022,13.926));
#103533=CARTESIAN_POINT('Ctrl Pts',(111.743771826316,10.6270054623453,13.926));
#103534=CARTESIAN_POINT('Ctrl Pts',(111.741048994449,10.6947715611111,13.926));
#103535=CARTESIAN_POINT('Ctrl Pts',(111.733983491,10.7623480550873,13.926));
#103536=CARTESIAN_POINT('Ctrl Pts',(111.722746501004,10.8294016522599,13.926));
#103537=CARTESIAN_POINT('Ctrl Pts',(111.717656379603,10.8597755290813,13.926));
#103538=CARTESIAN_POINT('Ctrl Pts',(111.711709616642,10.8900417576836,13.926));
#103539=CARTESIAN_POINT('Ctrl Pts',(111.704918977153,10.9201671810666,13.926));
#103540=CARTESIAN_POINT('Ctrl Pts',(111.700644111634,10.9391318358552,13.926));
#103541=CARTESIAN_POINT('Ctrl Pts',(111.696034781489,10.9580406592758,13.926));
#103542=CARTESIAN_POINT('Ctrl Pts',(111.691093828577,10.9768850263927,13.926));
#103543=CARTESIAN_POINT('Ctrl Pts',(111.687299350237,10.9913568386387,13.926));
#103544=CARTESIAN_POINT('Ctrl Pts',(111.683307875461,11.0057949971679,13.926));
#103545=CARTESIAN_POINT('Ctrl Pts',(111.679129091647,11.0201676983228,13.926));
#103546=CARTESIAN_POINT('Ctrl Pts',(111.661041641071,11.0823785073483,13.926));
#103547=CARTESIAN_POINT('Ctrl Pts',(111.639426529773,11.1434585617679,13.926));
#103548=CARTESIAN_POINT('Ctrl Pts',(111.614463340613,11.2031288954202,13.926));
#103549=CARTESIAN_POINT('Ctrl Pts',(111.589577411983,11.2626145506798,13.926));
#103550=CARTESIAN_POINT('Ctrl Pts',(111.561363371937,11.320700065467,13.926));
#103551=CARTESIAN_POINT('Ctrl Pts',(111.529957992456,11.3770783554949,13.926));
#103552=CARTESIAN_POINT('Ctrl Pts',(111.499178456137,11.4323331447748,13.926));
#103553=CARTESIAN_POINT('Ctrl Pts',(111.465332776718,11.4859487286863,13.926));
#103554=CARTESIAN_POINT('Ctrl Pts',(111.428521000927,11.5375954324615,13.926));
#103555=CARTESIAN_POINT('Ctrl Pts',(111.420177735821,11.5493009840742,13.926));
#103556=CARTESIAN_POINT('Ctrl Pts',(111.41168201237,11.5609052067453,13.926));
#103557=CARTESIAN_POINT('Ctrl Pts',(111.403034843024,11.5724039121731,13.926));
#103558=CARTESIAN_POINT('Ctrl Pts',(111.396582580946,11.5809839061578,13.926));
#103559=CARTESIAN_POINT('Ctrl Pts',(111.390051334627,11.5894980275904,13.926));
#103560=CARTESIAN_POINT('Ctrl Pts',(111.383443257475,11.5979431486214,13.926));
#103561=CARTESIAN_POINT('Ctrl Pts',(111.345215317679,11.6467984466027,13.926));
#103562=CARTESIAN_POINT('Ctrl Pts',(111.304403622696,11.6933678052254,13.926));
#103563=CARTESIAN_POINT('Ctrl Pts',(111.261138232155,11.7373789713312,13.926));
#103564=CARTESIAN_POINT('Ctrl Pts',(111.218651929526,11.7805976202061,13.926));
#103565=CARTESIAN_POINT('Ctrl Pts',(111.173798814374,11.8213499371724,13.926));
#103566=CARTESIAN_POINT('Ctrl Pts',(111.126677325675,11.8593349320108,13.926));
#103567=CARTESIAN_POINT('Ctrl Pts',(111.081054798031,11.8961116028012,13.926));
#103568=CARTESIAN_POINT('Ctrl Pts',(111.033305320964,11.9302945290462,13.926));
#103569=CARTESIAN_POINT('Ctrl Pts',(110.983504216739,11.961563551928,13.926));
#103570=CARTESIAN_POINT('Ctrl Pts',(110.971937739318,11.9688258898376,13.926));
#103571=CARTESIAN_POINT('Ctrl Pts',(110.960260553415,11.9759308302077,13.926));
#103572=CARTESIAN_POINT('Ctrl Pts',(110.948473540785,11.982873956425,13.926));
#103573=CARTESIAN_POINT('Ctrl Pts',(109.314174270871,12.1461458803668,6.34992591772793));
#103574=CARTESIAN_POINT('Ctrl Pts',(108.85551888803,11.9208415860382,6.38652530942973));
#103575=CARTESIAN_POINT('Ctrl Pts',(108.18502735973,10.9866824883096,6.45972409283332));
#103576=CARTESIAN_POINT('Ctrl Pts',(108.80047449685,9.36512639286223,6.56952226793872));
#103577=CARTESIAN_POINT('Ctrl Pts',(110.491593333654,8.98640096532305,6.67932044304411));
#103578=CARTESIAN_POINT('Ctrl Pts',(111.741732863822,10.1849114394086,6.7891186181495));
#103579=CARTESIAN_POINT('Ctrl Pts',(111.433149639798,11.8900189191182,6.8989167932549));
#103580=CARTESIAN_POINT('Ctrl Pts',(109.841413191019,12.5742367163702,7.00871496836029));
#103581=CARTESIAN_POINT('Ctrl Pts',(108.391749493731,11.6256052224506,7.11851314346568));
#103582=CARTESIAN_POINT('Ctrl Pts',(108.38171275925,9.89305824642555,7.22831131857108));
#103583=CARTESIAN_POINT('Ctrl Pts',(109.82036714101,8.92767494081165,7.33810949367647));
#103584=CARTESIAN_POINT('Ctrl Pts',(111.41981313278,9.59358681487167,7.44790766878186));
#103585=CARTESIAN_POINT('Ctrl Pts',(111.748271359623,11.29471174246,7.55770584388725));
#103586=CARTESIAN_POINT('Ctrl Pts',(110.511701824797,12.5082142882526,7.66750401899264));
#103587=CARTESIAN_POINT('Ctrl Pts',(108.817066499089,12.1477939398722,7.77730219409804));
#103588=CARTESIAN_POINT('Ctrl Pts',(108.181373638266,10.5360895014301,7.88710036920342));
#103589=CARTESIAN_POINT('Ctrl Pts',(109.173686477906,9.11587493853038,7.99689854430882));
#103590=CARTESIAN_POINT('Ctrl Pts',(110.90570183064,9.15850278599423,8.10669671941421));
#103591=CARTESIAN_POINT('Ctrl Pts',(111.8269474297,10.6258137189513,8.2164948945196));
#103592=CARTESIAN_POINT('Ctrl Pts',(111.112738765821,12.2042941592694,8.32629306962499));
#103593=CARTESIAN_POINT('Ctrl Pts',(109.402424116335,12.4809136837355,8.43609124473039));
#103594=CARTESIAN_POINT('Ctrl Pts',(108.227049862518,11.2080468503276,8.54588941983577));
#103595=CARTESIAN_POINT('Ctrl Pts',(108.638792317746,9.52514378590672,8.65568759494117));
#103596=CARTESIAN_POINT('Ctrl Pts',(110.269066191156,8.93871247704089,8.76548577004656));
#103597=CARTESIAN_POINT('Ctrl Pts',(111.658476300169,9.97371689050704,8.87528394515196));
#103598=CARTESIAN_POINT('Ctrl Pts',(111.563244859267,11.7036375693259,8.98508212025735));
#103599=CARTESIAN_POINT('Ctrl Pts',(110.068621537362,12.5798770967034,9.09488029536274));
#103600=CARTESIAN_POINT('Ctrl Pts',(108.512569308827,11.8180398134534,9.20467847046814));
#103601=CARTESIAN_POINT('Ctrl Pts',(108.288041326803,10.1001103129093,9.31447664557353));
#103602=CARTESIAN_POINT('Ctrl Pts',(109.596031461916,8.9639517015356,9.42427482067892));
#103603=CARTESIAN_POINT('Ctrl Pts',(111.265647793446,9.42663505898133,9.53407299578432));
#103604=CARTESIAN_POINT('Ctrl Pts',(111.802276393556,11.073973618372,9.6438711708897));
#103605=CARTESIAN_POINT('Ctrl Pts',(110.725535892815,12.4312961584497,9.7536693459951));
#103606=CARTESIAN_POINT('Ctrl Pts',(108.99930722521,12.2835491758203,9.86346752110049));
#103607=CARTESIAN_POINT('Ctrl Pts',(108.16888277946,10.7629934143855,9.97326569620588));
#103608=CARTESIAN_POINT('Ctrl Pts',(108.977645283184,9.23080615549536,10.0830638713113));
#103609=CARTESIAN_POINT('Ctrl Pts',(110.701603433992,9.05857701162966,10.1928620464167));
#103610=CARTESIAN_POINT('Ctrl Pts',(111.797497373615,10.4004827672002,10.3026602215221));
#103611=CARTESIAN_POINT('Ctrl Pts',(111.284300314861,12.0552707785837,10.4124583966274));
#103612=CARTESIAN_POINT('Ctrl Pts',(109.621418084829,12.5416011938169,10.5222565717329));
#103613=CARTESIAN_POINT('Ctrl Pts',(108.297436351006,11.4241187768446,10.6320547468382));
#103614=CARTESIAN_POINT('Ctrl Pts',(108.497562458434,9.70317597569252,10.7418529219436));
#103615=CARTESIAN_POINT('Ctrl Pts',(110.042646705583,8.91933335565637,10.851651097049));
#103616=CARTESIAN_POINT('Ctrl Pts',(111.549554301631,9.77427433649753,10.9614492721544));
#103617=CARTESIAN_POINT('Ctrl Pts',(111.669325585378,11.5026693790562,11.0712474472598));
#103618=CARTESIAN_POINT('Ctrl Pts',(110.294743212587,12.5572867904855,11.1810456223652));
#103619=CARTESIAN_POINT('Ctrl Pts',(108.656311413926,11.99404987332,11.2908437974706));
#103620=CARTESIAN_POINT('Ctrl Pts',(108.220728220139,10.3171593391372,11.400641972576));
#103621=CARTESIAN_POINT('Ctrl Pts',(109.377920764104,9.02774086435358,11.5104401476814));
#103622=CARTESIAN_POINT('Ctrl Pts',(111.091988723841,9.28006131881894,11.6202383227868));
#103623=CARTESIAN_POINT('Ctrl Pts',(111.82852578498,10.8482474465615,11.7300364978922));
#103624=CARTESIAN_POINT('Ctrl Pts',(110.928195705052,12.3284840355239,11.8398346729976));
#103625=CARTESIAN_POINT('Ctrl Pts',(109.196959631481,12.3956868563535,11.9496328481029));
#103626=CARTESIAN_POINT('Ctrl Pts',(108.184592481991,10.989697073083,12.0594310232083));
#103627=CARTESIAN_POINT('Ctrl Pts',(108.797349235318,9.36913421129256,12.1692291983137));
#103628=CARTESIAN_POINT('Ctrl Pts',(110.486699725726,8.98470055506267,12.2790273734191));
#103629=CARTESIAN_POINT('Ctrl Pts',(111.74036449784,10.1805344965231,12.3888255485245));
#103630=CARTESIAN_POINT('Ctrl Pts',(111.436082469949,11.8861455476417,12.4986237236299));
#103631=CARTESIAN_POINT('Ctrl Pts',(109.846242795973,12.5746958549649,12.6084218987353));
#103632=CARTESIAN_POINT('Ctrl Pts',(108.394043120869,11.6298102816096,12.7182200738407));
#103633=CARTESIAN_POINT('Ctrl Pts',(108.379472480118,9.897326941871,12.8280182489461));
#103634=CARTESIAN_POINT('Ctrl Pts',(109.815568107276,8.92815438021742,12.9378164240515));
#103635=CARTESIAN_POINT('Ctrl Pts',(111.416772645554,9.58984568552079,13.0476145991569));
#103636=CARTESIAN_POINT('Ctrl Pts',(111.749687759447,11.2901360392881,13.1574127742623));
#103637=CARTESIAN_POINT('Ctrl Pts',(110.516345144641,12.5068087730147,13.2672109493676));
#103638=CARTESIAN_POINT('Ctrl Pts',(108.820707641908,12.1510105496194,13.377009124473));
#103639=CARTESIAN_POINT('Ctrl Pts',(108.180898216782,10.5406506448061,13.4868072995784));
#103640=CARTESIAN_POINT('Ctrl Pts',(109.169225983483,9.11850985467691,13.5966054746838));
#103641=CARTESIAN_POINT('Ctrl Pts',(110.901845461742,9.15519245562723,13.7064036497892));
#103642=CARTESIAN_POINT('Ctrl Pts',(111.825924765157,10.6229447474917,13.8162018248946));
#103643=CARTESIAN_POINT('Ctrl Pts',(111.353491586843,11.6712858186231,13.8894006082982));
#103644=CARTESIAN_POINT('Ctrl Pts',(110.948473540785,11.982873956425,13.926));
#103645=CARTESIAN_POINT('Ctrl Pts',(109.255607560691,12.2653710241204,6.42661727848529));
#103646=CARTESIAN_POINT('Ctrl Pts',(108.757784885433,12.0208266652274,6.46321667018709));
#103647=CARTESIAN_POINT('Ctrl Pts',(108.030036124939,11.006894204069,6.53641545359068));
#103648=CARTESIAN_POINT('Ctrl Pts',(108.698039928543,9.24686385510494,6.64621362869608));
#103649=CARTESIAN_POINT('Ctrl Pts',(110.533573392254,8.83579682617836,6.75601180380147));
#103650=CARTESIAN_POINT('Ctrl Pts',(111.890469721474,10.1366551892434,6.86580997890685));
#103651=CARTESIAN_POINT('Ctrl Pts',(111.55553475315,11.9873718687096,6.97560815401225));
#103652=CARTESIAN_POINT('Ctrl Pts',(109.827870526628,12.7300190653413,7.08540632911764));
#103653=CARTESIAN_POINT('Ctrl Pts',(108.254411483071,11.7003783245928,7.19520450422304));
#103654=CARTESIAN_POINT('Ctrl Pts',(108.243517652545,9.81987892813574,7.30500267932843));
#103655=CARTESIAN_POINT('Ctrl Pts',(109.80502723009,8.77205583953947,7.41480085443382));
#103656=CARTESIAN_POINT('Ctrl Pts',(111.54105936302,9.49483386206473,7.52459902953921));
#103657=CARTESIAN_POINT('Ctrl Pts',(111.897566578055,11.3412278957591,7.6343972046446));
#103658=CARTESIAN_POINT('Ctrl Pts',(110.555399066238,12.6583585920924,7.74419537975));
#103659=CARTESIAN_POINT('Ctrl Pts',(108.716048819862,12.2671598211621,7.85399355485539));
#103660=CARTESIAN_POINT('Ctrl Pts',(108.026070390618,10.5178224203886,7.96379172996078));
#103661=CARTESIAN_POINT('Ctrl Pts',(109.103122685223,8.97632734676019,8.07358990506617));
#103662=CARTESIAN_POINT('Ctrl Pts',(110.983045059936,9.02259543792151,8.18338808017156));
#103663=CARTESIAN_POINT('Ctrl Pts',(111.982961262494,10.6152087188446,8.29318625527695));
#103664=CARTESIAN_POINT('Ctrl Pts',(111.207762101979,12.3284849280402,8.40298443038235));
#103665=CARTESIAN_POINT('Ctrl Pts',(109.35139358175,12.6287266276911,8.51278260548774));
#103666=CARTESIAN_POINT('Ctrl Pts',(108.075647177468,11.2471621765583,8.62258078059314));
#103667=CARTESIAN_POINT('Ctrl Pts',(108.522550753109,9.42054607856372,8.73237895569852));
#103668=CARTESIAN_POINT('Ctrl Pts',(110.292043342592,8.78403593618604,8.84217713080392));
#103669=CARTESIAN_POINT('Ctrl Pts',(111.800103388054,9.90742549028566,8.95197530590931));
#103670=CARTESIAN_POINT('Ctrl Pts',(111.696739571882,11.7850743145046,9.0617734810147));
#103671=CARTESIAN_POINT('Ctrl Pts',(110.074481535784,12.7361411110688,9.1715716561201));
#103672=CARTESIAN_POINT('Ctrl Pts',(108.385548815859,11.9092460420318,9.28136983122549));
#103673=CARTESIAN_POINT('Ctrl Pts',(108.141847063164,10.0446123936324,9.39116800633088));
#103674=CARTESIAN_POINT('Ctrl Pts',(109.561534202208,8.81143048714838,9.50096618143628));
#103675=CARTESIAN_POINT('Ctrl Pts',(111.373728934706,9.31362510955542,9.61076435654167));
#103676=CARTESIAN_POINT('Ctrl Pts',(111.956183420843,11.1016396393559,9.72056253164705));
#103677=CARTESIAN_POINT('Ctrl Pts',(110.787493688441,12.5748719688305,9.83036070675245));
#103678=CARTESIAN_POINT('Ctrl Pts',(108.913852158082,12.4145079986135,9.94015888185784));
#103679=CARTESIAN_POINT('Ctrl Pts',(108.012512863595,10.764102998792,10.0499570569632));
#103680=CARTESIAN_POINT('Ctrl Pts',(108.890340374869,9.10107321924012,10.1597552320686));
#103681=CARTESIAN_POINT('Ctrl Pts',(110.76151749559,8.91413641142274,10.269553407174));
#103682=CARTESIAN_POINT('Ctrl Pts',(111.950996292159,10.3706354260943,10.3793515822794));
#103683=CARTESIAN_POINT('Ctrl Pts',(111.393974305104,12.1667355605971,10.4891497573848));
#103684=CARTESIAN_POINT('Ctrl Pts',(109.58908873881,12.6945966027392,10.5989479324902));
#103685=CARTESIAN_POINT('Ctrl Pts',(108.15204438398,11.4816857612167,10.7087461075956));
#103686=CARTESIAN_POINT('Ctrl Pts',(108.369260441867,9.61378148867087,10.818544282701));
#103687=CARTESIAN_POINT('Ctrl Pts',(110.046288559686,8.76300191715408,10.9283424578064));
#103688=CARTESIAN_POINT('Ctrl Pts',(111.68187989666,9.69095135848281,11.0381406329118));
#103689=CARTESIAN_POINT('Ctrl Pts',(111.811879157814,11.5669442633493,11.1479388080172));
#103690=CARTESIAN_POINT('Ctrl Pts',(110.319913076557,12.7116216851622,11.2577369831225));
#103691=CARTESIAN_POINT('Ctrl Pts',(108.541565908397,12.1002866406013,11.3675351582279));
#103692=CARTESIAN_POINT('Ctrl Pts',(108.068785692704,10.2801965183178,11.4773333333333));
#103693=CARTESIAN_POINT('Ctrl Pts',(109.324797743531,8.88066698338174,11.5871315084387));
#103694=CARTESIAN_POINT('Ctrl Pts',(111.185240091344,9.15453457190998,11.6969296835441));
#103695=CARTESIAN_POINT('Ctrl Pts',(111.984674402855,10.8566373763707,11.8067278586495));
#103696=CARTESIAN_POINT('Ctrl Pts',(111.007459819155,12.4632801114172,11.9165260337549));
#103697=CARTESIAN_POINT('Ctrl Pts',(109.128383270856,12.5362217780843,12.0263242088603));
#103698=CARTESIAN_POINT('Ctrl Pts',(108.029564110423,11.0101662220434,12.1361223839657));
#103699=CARTESIAN_POINT('Ctrl Pts',(108.694647782467,9.2512139248252,12.2459205590711));
#103700=CARTESIAN_POINT('Ctrl Pts',(110.52826189024,8.83395120784152,12.3557187341765));
#103701=CARTESIAN_POINT('Ctrl Pts',(111.888984502638,10.1319044733503,12.4655169092819));
#103702=CARTESIAN_POINT('Ctrl Pts',(111.558718034992,11.9831677271628,12.5753150843873));
#103703=CARTESIAN_POINT('Ctrl Pts',(109.833112560077,12.7305174124926,12.6851132594926));
#103704=CARTESIAN_POINT('Ctrl Pts',(108.256900976578,11.7049424785926,12.7949114345981));
#103705=CARTESIAN_POINT('Ctrl Pts',(108.241086062745,9.82451215270046,12.9047096097034));
#103706=CARTESIAN_POINT('Ctrl Pts',(109.799818378518,8.77257622110816,13.0145077848088));
#103707=CARTESIAN_POINT('Ctrl Pts',(111.537759230629,9.49077325557974,13.1243059599142));
#103708=CARTESIAN_POINT('Ctrl Pts',(111.899103932626,11.3362614462647,13.2341041350196));
#103709=CARTESIAN_POINT('Ctrl Pts',(110.560438906591,12.656833051606,13.343902310125));
#103710=CARTESIAN_POINT('Ctrl Pts',(108.720000901374,12.2706511162161,13.4537004852304));
#103711=CARTESIAN_POINT('Ctrl Pts',(108.025554370084,10.5227730667402,13.5634986603358));
#103712=CARTESIAN_POINT('Ctrl Pts',(109.098281282833,8.9791872739609,13.6732968354412));
#103713=CARTESIAN_POINT('Ctrl Pts',(110.978859372918,9.01900241889038,13.7830950105466));
#103714=CARTESIAN_POINT('Ctrl Pts',(111.981851266585,10.612094748965,13.892893185652));
#103715=CARTESIAN_POINT('Ctrl Pts',(111.469074228514,11.7499598567076,13.9660919690556));
#103716=CARTESIAN_POINT('Ctrl Pts',(111.029469299063,12.0881563461465,14.0026913607574));
#103717=CARTESIAN_POINT('Ctrl Pts',(109.19704085051,12.384596167874,6.50330863924264));
#103718=CARTESIAN_POINT('Ctrl Pts',(108.660050882836,12.1208117444166,6.53990803094444));
#103719=CARTESIAN_POINT('Ctrl Pts',(107.875044890149,11.0271059198285,6.61310681434804));
#103720=CARTESIAN_POINT('Ctrl Pts',(108.595605360236,9.12860131734766,6.72290498945343));
#103721=CARTESIAN_POINT('Ctrl Pts',(110.575553450855,8.68519268703365,6.83270316455883));
#103722=CARTESIAN_POINT('Ctrl Pts',(112.039206579126,10.0883989390783,6.94250133966421));
#103723=CARTESIAN_POINT('Ctrl Pts',(111.677919866503,12.0847248183011,7.05229951476961));
#103724=CARTESIAN_POINT('Ctrl Pts',(109.814327862238,12.8858014143123,7.16209768987499));
#103725=CARTESIAN_POINT('Ctrl Pts',(108.11707347241,11.775151426735,7.27189586498039));
#103726=CARTESIAN_POINT('Ctrl Pts',(108.10532254584,9.74669960984593,7.38169404008578));
#103727=CARTESIAN_POINT('Ctrl Pts',(109.78968731917,8.61643673826731,7.49149221519118));
#103728=CARTESIAN_POINT('Ctrl Pts',(111.662305593259,9.39608090925777,7.60129039029656));
#103729=CARTESIAN_POINT('Ctrl Pts',(112.046861796486,11.3877440490583,7.71108856540196));
#103730=CARTESIAN_POINT('Ctrl Pts',(110.599096307678,12.8085028959323,7.82088674050736));
#103731=CARTESIAN_POINT('Ctrl Pts',(108.615031140635,12.3865257024519,7.93068491561274));
#103732=CARTESIAN_POINT('Ctrl Pts',(107.87076714297,10.4995553393472,8.04048309071814));
#103733=CARTESIAN_POINT('Ctrl Pts',(109.032558892541,8.83677975499,8.15028126582352));
#103734=CARTESIAN_POINT('Ctrl Pts',(111.060388289232,8.8866880898488,8.26007944092893));
#103735=CARTESIAN_POINT('Ctrl Pts',(112.138975095289,10.6046037187379,8.36987761603431));
#103736=CARTESIAN_POINT('Ctrl Pts',(111.302785438136,12.452675696811,8.47967579113971));
#103737=CARTESIAN_POINT('Ctrl Pts',(109.300363047166,12.7765395716466,8.5894739662451));
#103738=CARTESIAN_POINT('Ctrl Pts',(107.924244492418,11.286277502789,8.69927214135049));
#103739=CARTESIAN_POINT('Ctrl Pts',(108.406309188473,9.3159483712207,8.80907031645588));
#103740=CARTESIAN_POINT('Ctrl Pts',(110.315020494028,8.62935939533118,8.91886849156128));
#103741=CARTESIAN_POINT('Ctrl Pts',(111.94173047594,9.84113409006431,9.02866666666666));
#103742=CARTESIAN_POINT('Ctrl Pts',(111.830234284497,11.8665110596832,9.13846484177206));
#103743=CARTESIAN_POINT('Ctrl Pts',(110.080341534207,12.8924051254342,9.24826301687745));
#103744=CARTESIAN_POINT('Ctrl Pts',(108.258528322892,12.0004522706103,9.35806119198285));
#103745=CARTESIAN_POINT('Ctrl Pts',(107.995652799526,9.98911447435552,9.46785936708823));
#103746=CARTESIAN_POINT('Ctrl Pts',(109.5270369425,8.65890927276113,9.57765754219364));
#103747=CARTESIAN_POINT('Ctrl Pts',(111.481810075966,9.20061516012953,9.68745571729902));
#103748=CARTESIAN_POINT('Ctrl Pts',(112.110090448129,11.1293056603398,9.79725389240442));
#103749=CARTESIAN_POINT('Ctrl Pts',(110.849451484067,12.7184477792114,9.9070520675098));
#103750=CARTESIAN_POINT('Ctrl Pts',(108.828397090954,12.5454668214067,10.0168502426152));
#103751=CARTESIAN_POINT('Ctrl Pts',(107.856142947729,10.7652125831984,10.1266484177206));
#103752=CARTESIAN_POINT('Ctrl Pts',(108.803035466554,8.97134028298489,10.236446592826));
#103753=CARTESIAN_POINT('Ctrl Pts',(110.821431557188,8.76969581121582,10.3462447679314));
#103754=CARTESIAN_POINT('Ctrl Pts',(112.104495210703,10.3407880849884,10.4560429430368));
#103755=CARTESIAN_POINT('Ctrl Pts',(111.503648295348,12.2782003426105,10.5658411181422));
#103756=CARTESIAN_POINT('Ctrl Pts',(109.556759392791,12.8475920116615,10.6756392932476));
#103757=CARTESIAN_POINT('Ctrl Pts',(108.006652416955,11.5392527455888,10.7854374683529));
#103758=CARTESIAN_POINT('Ctrl Pts',(108.240958425299,9.52438700164923,10.8952356434583));
#103759=CARTESIAN_POINT('Ctrl Pts',(110.04993041379,8.6066704786518,11.0050338185637));
#103760=CARTESIAN_POINT('Ctrl Pts',(111.814205491688,9.60762838046807,11.1148319936691));
#103761=CARTESIAN_POINT('Ctrl Pts',(111.95443273025,11.6312191476424,11.2246301687745));
#103762=CARTESIAN_POINT('Ctrl Pts',(110.345082940527,12.8659565798388,11.3344283438799));
#103763=CARTESIAN_POINT('Ctrl Pts',(108.426820402868,12.2065234078826,11.4442265189853));
#103764=CARTESIAN_POINT('Ctrl Pts',(107.916843165269,10.2432336974984,11.5540246940907));
#103765=CARTESIAN_POINT('Ctrl Pts',(109.271674722958,8.7335931024099,11.6638228691961));
#103766=CARTESIAN_POINT('Ctrl Pts',(111.278491458847,9.02900782500102,11.7736210443015));
#103767=CARTESIAN_POINT('Ctrl Pts',(112.14082302073,10.8650273061799,11.8834192194069));
#103768=CARTESIAN_POINT('Ctrl Pts',(111.086723933259,12.5980761873106,11.9932173945123));
#103769=CARTESIAN_POINT('Ctrl Pts',(109.059806910231,12.6767566998151,12.1030155696177));
#103770=CARTESIAN_POINT('Ctrl Pts',(107.874535738854,11.0306353710037,12.2128137447231));
#103771=CARTESIAN_POINT('Ctrl Pts',(108.591946329617,9.13329363835785,12.3226119198284));
#103772=CARTESIAN_POINT('Ctrl Pts',(110.569824054753,8.68320186062037,12.4324100949338));
#103773=CARTESIAN_POINT('Ctrl Pts',(112.037604507435,10.0832744501776,12.5422082700392));
#103774=CARTESIAN_POINT('Ctrl Pts',(111.681353600035,12.0801899066839,12.6520064451446));
#103775=CARTESIAN_POINT('Ctrl Pts',(109.819982324182,12.8863389700205,12.76180462025));
#103776=CARTESIAN_POINT('Ctrl Pts',(108.119758832288,11.7800746755757,12.8716027953554));
#103777=CARTESIAN_POINT('Ctrl Pts',(108.102699645371,9.75169736352991,12.9814009704608));
#103778=CARTESIAN_POINT('Ctrl Pts',(109.784068649759,8.61699806199891,13.0911991455662));
#103779=CARTESIAN_POINT('Ctrl Pts',(111.658745815704,9.39170082563866,13.2009973206716));
#103780=CARTESIAN_POINT('Ctrl Pts',(112.048520105805,11.3823868532413,13.310795495777));
#103781=CARTESIAN_POINT('Ctrl Pts',(110.604532668541,12.8068573301973,13.4205936708824));
#103782=CARTESIAN_POINT('Ctrl Pts',(108.619294160841,12.3902916828128,13.5303918459878));
#103783=CARTESIAN_POINT('Ctrl Pts',(107.870210523387,10.5048954886742,13.6401900210931));
#103784=CARTESIAN_POINT('Ctrl Pts',(109.027336582184,8.83986469324491,13.7499881961986));
#103785=CARTESIAN_POINT('Ctrl Pts',(111.055873284095,8.88281238215351,13.8597863713039));
#103786=CARTESIAN_POINT('Ctrl Pts',(112.137777768013,10.6012447504384,13.9695845464093));
#103787=CARTESIAN_POINT('Ctrl Pts',(111.584656870185,11.8286338947921,14.0427833298129));
#103788=CARTESIAN_POINT('Ctrl Pts',(111.11046505734,12.193438735868,14.0793827215147));
#103789=CARTESIAN_POINT('Ctrl Pts',(109.13847414033,12.5038213116276,6.58));
#103790=CARTESIAN_POINT('Ctrl Pts',(108.562316880239,12.2207968236057,6.6165993917018));
#103791=CARTESIAN_POINT('Ctrl Pts',(107.720053655359,11.0473176355879,6.68979817510539));
#103792=CARTESIAN_POINT('Ctrl Pts',(108.493170791929,9.01033877959037,6.79959635021078));
#103793=CARTESIAN_POINT('Ctrl Pts',(110.617533509456,8.53458854788894,6.90939452531619));
#103794=CARTESIAN_POINT('Ctrl Pts',(112.187943436778,10.0401426889131,7.01919270042156));
#103795=CARTESIAN_POINT('Ctrl Pts',(111.800304979855,12.1820777678926,7.12899087552697));
#103796=CARTESIAN_POINT('Ctrl Pts',(109.800785197847,13.0415837632834,7.23878905063235));
#103797=CARTESIAN_POINT('Ctrl Pts',(107.979735461749,11.8499245288773,7.34858722573775));
#103798=CARTESIAN_POINT('Ctrl Pts',(107.967127439135,9.67352029155613,7.45838540084314));
#103799=CARTESIAN_POINT('Ctrl Pts',(109.77434740825,8.46081763699515,7.56818357594853));
#103800=CARTESIAN_POINT('Ctrl Pts',(111.783551823499,9.29732795645082,7.67798175105392));
#103801=CARTESIAN_POINT('Ctrl Pts',(112.196157014917,11.4342602023574,7.78777992615932));
#103802=CARTESIAN_POINT('Ctrl Pts',(110.642793549118,12.9586471997721,7.89757810126471));
#103803=CARTESIAN_POINT('Ctrl Pts',(108.514013461408,12.5058915837418,8.0073762763701));
#103804=CARTESIAN_POINT('Ctrl Pts',(107.715463895321,10.4812882583057,8.11717445147549));
#103805=CARTESIAN_POINT('Ctrl Pts',(108.961995099858,8.69723216321981,8.22697262658088));
#103806=CARTESIAN_POINT('Ctrl Pts',(111.137731518528,8.75078074177608,8.33677080168628));
#103807=CARTESIAN_POINT('Ctrl Pts',(112.294988928083,10.5939987186312,8.44656897679166));
#103808=CARTESIAN_POINT('Ctrl Pts',(111.397808774294,12.5768664655818,8.55636715189706));
#103809=CARTESIAN_POINT('Ctrl Pts',(109.249332512581,12.9243525156022,8.66616532700245));
#103810=CARTESIAN_POINT('Ctrl Pts',(107.772841807367,11.3253928290197,8.77596350210785));
#103811=CARTESIAN_POINT('Ctrl Pts',(108.290067623836,9.2113506638777,8.88576167721323));
#103812=CARTESIAN_POINT('Ctrl Pts',(110.337997645464,8.47468285447632,8.99555985231864));
#103813=CARTESIAN_POINT('Ctrl Pts',(112.083357563825,9.77484268984296,9.10535802742402));
#103814=CARTESIAN_POINT('Ctrl Pts',(111.963728997112,11.9479478048619,9.21515620252942));
#103815=CARTESIAN_POINT('Ctrl Pts',(110.086201532629,13.0486691397997,9.3249543776348));
#103816=CARTESIAN_POINT('Ctrl Pts',(108.131507829924,12.0916584991887,9.43475255274021));
#103817=CARTESIAN_POINT('Ctrl Pts',(107.849458535887,9.93361655507863,9.54455072784558));
#103818=CARTESIAN_POINT('Ctrl Pts',(109.492539682792,8.5063880583739,9.65434890295099));
#103819=CARTESIAN_POINT('Ctrl Pts',(111.589891217225,9.08760521070363,9.76414707805638));
#103820=CARTESIAN_POINT('Ctrl Pts',(112.263997475416,11.1569716813237,9.87394525316177));
#103821=CARTESIAN_POINT('Ctrl Pts',(110.911409279692,12.8620235895922,9.98374342826716));
#103822=CARTESIAN_POINT('Ctrl Pts',(108.742942023825,12.6764256441999,10.0935416033726));
#103823=CARTESIAN_POINT('Ctrl Pts',(107.699773031864,10.7663221676049,10.2033397784779));
#103824=CARTESIAN_POINT('Ctrl Pts',(108.715730558239,8.84160734672965,10.3131379535833));
#103825=CARTESIAN_POINT('Ctrl Pts',(110.881345618785,8.6252552110089,10.4229361286887));
#103826=CARTESIAN_POINT('Ctrl Pts',(112.257994129247,10.3109407438825,10.5327343037941));
#103827=CARTESIAN_POINT('Ctrl Pts',(111.613322285592,12.3896651246239,10.6425324788995));
#103828=CARTESIAN_POINT('Ctrl Pts',(109.524430046773,13.0005874205838,10.7523306540049));
#103829=CARTESIAN_POINT('Ctrl Pts',(107.861260449929,11.596819729961,10.8621288291103));
#103830=CARTESIAN_POINT('Ctrl Pts',(108.112656408731,9.43499251462759,10.9719270042157));
#103831=CARTESIAN_POINT('Ctrl Pts',(110.053572267893,8.45033904014951,11.0817251793211));
#103832=CARTESIAN_POINT('Ctrl Pts',(111.946531086717,9.52430540245334,11.1915233544265));
#103833=CARTESIAN_POINT('Ctrl Pts',(112.096986302686,11.6954940319355,11.3013215295319));
#103834=CARTESIAN_POINT('Ctrl Pts',(110.370252804496,13.0202914745154,11.4111197046373));
#103835=CARTESIAN_POINT('Ctrl Pts',(108.312074897339,12.3127601751638,11.5209178797427));
#103836=CARTESIAN_POINT('Ctrl Pts',(107.764900637834,10.206270876679,11.630716054848));
#103837=CARTESIAN_POINT('Ctrl Pts',(109.218551702385,8.58651922143807,11.7405142299534));
#103838=CARTESIAN_POINT('Ctrl Pts',(111.371742826349,8.90348107809205,11.8503124050588));
#103839=CARTESIAN_POINT('Ctrl Pts',(112.296971638605,10.8734172359891,11.9601105801642));
#103840=CARTESIAN_POINT('Ctrl Pts',(111.165988047362,12.7328722632039,12.0699087552696));
#103841=CARTESIAN_POINT('Ctrl Pts',(108.991230549607,12.8172916215459,12.179706930375));
#103842=CARTESIAN_POINT('Ctrl Pts',(107.719507367285,11.0511045199641,12.2895051054804));
#103843=CARTESIAN_POINT('Ctrl Pts',(108.489244876767,9.01537335189051,12.3993032805858));
#103844=CARTESIAN_POINT('Ctrl Pts',(110.611386219267,8.5324525133992,12.5091014556912));
#103845=CARTESIAN_POINT('Ctrl Pts',(112.186224512233,10.0346444270048,12.6188996307966));
#103846=CARTESIAN_POINT('Ctrl Pts',(111.803989165079,12.177212086205,12.728697805902));
#103847=CARTESIAN_POINT('Ctrl Pts',(109.806852088287,13.0421605275483,12.8384959810074));
#103848=CARTESIAN_POINT('Ctrl Pts',(107.982616687997,11.8552068725587,12.9482941561128));
#103849=CARTESIAN_POINT('Ctrl Pts',(107.964313227998,9.67888257435937,13.0580923312181));
#103850=CARTESIAN_POINT('Ctrl Pts',(109.768318921001,8.46141990288965,13.1678905063235));
#103851=CARTESIAN_POINT('Ctrl Pts',(111.779732400779,9.29262839569759,13.2776886814289));
#103852=CARTESIAN_POINT('Ctrl Pts',(112.197936278984,11.4285122602179,13.3874868565343));
#103853=CARTESIAN_POINT('Ctrl Pts',(110.648626430491,12.9568816087886,13.4972850316397));
#103854=CARTESIAN_POINT('Ctrl Pts',(108.518587420307,12.5099322494094,13.6070832067451));
#103855=CARTESIAN_POINT('Ctrl Pts',(107.71486667669,10.4870179106083,13.7168813818505));
#103856=CARTESIAN_POINT('Ctrl Pts',(108.956391881534,8.70054211252889,13.8266795569559));
#103857=CARTESIAN_POINT('Ctrl Pts',(111.132887195271,8.74662234541666,13.9364777320613));
#103858=CARTESIAN_POINT('Ctrl Pts',(112.293704269442,10.5903947519117,14.0462759071667));
#103859=CARTESIAN_POINT('Ctrl Pts',(111.700239511856,11.9073079328766,14.1194746905703));
#103860=CARTESIAN_POINT('Ctrl Pts',(111.191460815618,12.2987211255895,14.1560740822721));
#103861=CARTESIAN_POINT('Ctrl Pts',(108.043923528227,10.7487415210877,13.7041303078758));
#103862=CARTESIAN_POINT('Ctrl Pts',(108.043390553338,10.6744197365054,13.7083806658673));
#103863=CARTESIAN_POINT('Ctrl Pts',(108.047267155266,10.600156305453,13.7126310238589));
#103864=CARTESIAN_POINT('Ctrl Pts',(108.055741001433,10.5264243340619,13.7168813818505));
#103865=CARTESIAN_POINT('Ctrl Pts',(108.128708411638,9.89152597791513,13.7534807735523));
#103866=CARTESIAN_POINT('Ctrl Pts',(108.542550146586,9.29603404522202,13.7900801652541));
#103867=CARTESIAN_POINT('Ctrl Pts',(109.112220233016,9.00596811769008,13.8266795569559));
#103868=CARTESIAN_POINT('Ctrl Pts',(109.627528300012,8.74358236850237,13.8597863713039));
#103869=CARTESIAN_POINT('Ctrl Pts',(110.27034322046,8.73111204555335,13.892893185652));
#103870=CARTESIAN_POINT('Ctrl Pts',(110.800030261768,8.96425629420689,13.926));
#103871=CARTESIAN_POINT('',(109.094485737464,9.48253146637784,6.58));
#103872=CARTESIAN_POINT('Ctrl Pts',(109.094485737464,9.48253146637783,6.58));
#103873=CARTESIAN_POINT('Ctrl Pts',(109.050936912807,9.50575319919841,6.58));
#103874=CARTESIAN_POINT('Ctrl Pts',(109.008665973235,9.53109748968633,6.58));
#103875=CARTESIAN_POINT('Ctrl Pts',(108.967849928603,9.55852424242646,6.58));
#103876=CARTESIAN_POINT('Ctrl Pts',(108.918405134776,9.59174917019158,6.58));
#103877=CARTESIAN_POINT('Ctrl Pts',(108.87109400725,9.62802846914193,6.58));
#103878=CARTESIAN_POINT('Ctrl Pts',(108.825992689794,9.66704649021906,6.58));
#103879=CARTESIAN_POINT('Ctrl Pts',(108.811269067091,9.67978418067566,6.58));
#103880=CARTESIAN_POINT('Ctrl Pts',(108.796781101392,9.6928141355179,6.58));
#103881=CARTESIAN_POINT('Ctrl Pts',(108.782531922016,9.70612644259636,6.58));
#103882=CARTESIAN_POINT('Ctrl Pts',(108.768136779111,9.71957511621697,6.58));
#103883=CARTESIAN_POINT('Ctrl Pts',(108.753980780056,9.73331684541932,6.58));
#103884=CARTESIAN_POINT('Ctrl Pts',(108.740092740145,9.74731551635198,6.58));
#103885=CARTESIAN_POINT('Ctrl Pts',(108.696277375476,9.7914799107319,6.58));
#103886=CARTESIAN_POINT('Ctrl Pts',(108.655087119634,9.83823222524873,6.58));
#103887=CARTESIAN_POINT('Ctrl Pts',(108.616602456003,9.88722312609965,6.58));
#103888=CARTESIAN_POINT('Ctrl Pts',(108.586435257704,9.92562590999792,6.58));
#103889=CARTESIAN_POINT('Ctrl Pts',(108.557930796962,9.96540544741069,6.58));
#103890=CARTESIAN_POINT('Ctrl Pts',(108.531138759219,10.006412957565,6.58));
#103891=CARTESIAN_POINT('Ctrl Pts',(108.519242344837,10.024621439436,6.58));
#103892=CARTESIAN_POINT('Ctrl Pts',(108.507683697692,10.0430722310019,6.58));
#103893=CARTESIAN_POINT('Ctrl Pts',(108.496467920523,10.0617531902008,6.58));
#103894=CARTESIAN_POINT('Ctrl Pts',(108.489773727828,10.0729030141253,6.58));
#103895=CARTESIAN_POINT('Ctrl Pts',(108.483205613724,10.0841284017624,6.58));
#103896=CARTESIAN_POINT('Ctrl Pts',(108.476767613657,10.0954204877901,6.58));
#103897=CARTESIAN_POINT('Ctrl Pts',(108.444738154717,10.1515993324623,6.58));
#103898=CARTESIAN_POINT('Ctrl Pts',(108.415900039582,10.2094701677432,6.58));
#103899=CARTESIAN_POINT('Ctrl Pts',(108.390338629852,10.2686792144268,6.58));
#103900=CARTESIAN_POINT('Ctrl Pts',(108.364258095986,10.3290907317699,6.58));
#103901=CARTESIAN_POINT('Ctrl Pts',(108.341587974258,10.3908961572324,6.58));
#103902=CARTESIAN_POINT('Ctrl Pts',(108.32245351373,10.4537607571801,6.58));
#103903=CARTESIAN_POINT('Ctrl Pts',(108.30955567597,10.4961354773764,6.58));
#103904=CARTESIAN_POINT('Ctrl Pts',(108.298265032162,10.5389922949493,6.58));
#103905=CARTESIAN_POINT('Ctrl Pts',(108.288631134875,10.5822359881016,6.58));
#103906=CARTESIAN_POINT('Ctrl Pts',(108.281989541746,10.6120481198671,6.58));
#103907=CARTESIAN_POINT('Ctrl Pts',(108.276135541372,10.6420442390975,6.58));
#103908=CARTESIAN_POINT('Ctrl Pts',(108.271088271902,10.672194168098,6.58));
#103909=CARTESIAN_POINT('Ctrl Pts',(108.269449801862,10.6819815899274,6.58));
#103910=CARTESIAN_POINT('Ctrl Pts',(108.267896731562,10.6917833667726,6.58));
#103911=CARTESIAN_POINT('Ctrl Pts',(108.266430872539,10.7015893700294,6.58));
#103912=CARTESIAN_POINT('Ctrl Pts',(108.256410853655,10.7686192386944,6.58));
#103913=CARTESIAN_POINT('Ctrl Pts',(108.250442320048,10.8359619127518,6.58));
#103914=CARTESIAN_POINT('Ctrl Pts',(108.248640216193,10.9032609407739,6.58));
#103915=CARTESIAN_POINT('Ctrl Pts',(108.247984029468,10.9277660372508,6.58));
#103916=CARTESIAN_POINT('Ctrl Pts',(108.247880654352,10.9522656427428,6.58));
#103917=CARTESIAN_POINT('Ctrl Pts',(108.248337121755,10.9767434152174,6.58));
#103918=CARTESIAN_POINT('Ctrl Pts',(108.249548986487,11.0417288862322,6.58));
#103919=CARTESIAN_POINT('Ctrl Pts',(108.254702968127,11.1065599084768,6.58));
#103920=CARTESIAN_POINT('Ctrl Pts',(108.263584862996,11.1710011132196,6.58));
#103921=CARTESIAN_POINT('Ctrl Pts',(108.268229471318,11.2046993454291,6.58));
#103922=CARTESIAN_POINT('Ctrl Pts',(108.273894368221,11.2382911384497,6.58));
#103923=CARTESIAN_POINT('Ctrl Pts',(108.280554427054,11.2717432628227,6.58));
#103924=CARTESIAN_POINT('Ctrl Pts',(108.283902653934,11.2885607271757,6.58));
#103925=CARTESIAN_POINT('Ctrl Pts',(108.287502455648,11.3053428915284,6.58));
#103926=CARTESIAN_POINT('Ctrl Pts',(108.291350983268,11.3220855124536,6.58));
#103927=CARTESIAN_POINT('Ctrl Pts',(108.294074929971,11.3339357605395,6.58));
#103928=CARTESIAN_POINT('Ctrl Pts',(108.296923840734,11.3457676088853,6.58));
#103929=CARTESIAN_POINT('Ctrl Pts',(108.299895665582,11.3575751561644,6.58));
#103930=CARTESIAN_POINT('Ctrl Pts',(108.316402383052,11.4231590505621,6.58));
#103931=CARTESIAN_POINT('Ctrl Pts',(108.33662697865,11.4877187759529,6.58));
#103932=CARTESIAN_POINT('Ctrl Pts',(108.360307162796,11.5510007167747,6.58));
#103933=CARTESIAN_POINT('Ctrl Pts',(108.384511690055,11.6156838903606,6.58));
#103934=CARTESIAN_POINT('Ctrl Pts',(108.412326689962,11.6790329257557,6.58));
#103935=CARTESIAN_POINT('Ctrl Pts',(108.443527431511,11.7407814451632,6.58));
#103936=CARTESIAN_POINT('Ctrl Pts',(108.475025086212,11.8031175771291,6.58));
#103937=CARTESIAN_POINT('Ctrl Pts',(108.509973535022,11.8638235615249,6.58));
#103938=CARTESIAN_POINT('Ctrl Pts',(108.548193675815,11.9226158531736,6.58));
#103939=CARTESIAN_POINT('Ctrl Pts',(108.563444783309,11.9460759331508,6.58));
#103940=CARTESIAN_POINT('Ctrl Pts',(108.579217385883,11.9692311139236,6.58));
#103941=CARTESIAN_POINT('Ctrl Pts',(108.595502214161,11.9920624177307,6.58));
#103942=CARTESIAN_POINT('Ctrl Pts',(108.601528527372,12.0005112994394,6.58));
#103943=CARTESIAN_POINT('Ctrl Pts',(108.607623934891,12.0089142481693,6.58));
#103944=CARTESIAN_POINT('Ctrl Pts',(108.613782347307,12.0172630060722,6.58));
#103945=CARTESIAN_POINT('Ctrl Pts',(108.656623913337,12.0753419132332,6.58));
#103946=CARTESIAN_POINT('Ctrl Pts',(108.702582196294,12.1309004454991,6.58));
#103947=CARTESIAN_POINT('Ctrl Pts',(108.751414460567,12.1836589933253,6.58));
#103948=CARTESIAN_POINT('Ctrl Pts',(108.800370406047,12.2365511667563,6.58));
#103949=CARTESIAN_POINT('Ctrl Pts',(108.852215343132,12.2866301616735,6.58));
#103950=CARTESIAN_POINT('Ctrl Pts',(108.906754319057,12.3335980072095,6.58));
#103951=CARTESIAN_POINT('Ctrl Pts',(108.960144301937,12.3795763635418,6.58));
#103952=CARTESIAN_POINT('Ctrl Pts',(109.016116578056,12.4225741338096,6.58));
#103953=CARTESIAN_POINT('Ctrl Pts',(109.074528046071,12.4622826185796,6.58));
#103954=CARTESIAN_POINT('Ctrl Pts',(109.095529607657,12.4765596127507,6.58));
#103955=CARTESIAN_POINT('Ctrl Pts',(109.116846828723,12.490411052127,6.58));
#103956=CARTESIAN_POINT('Ctrl Pts',(109.138474140329,12.5038213116275,6.58));
#103957=CARTESIAN_POINT('Ctrl Pts',(109.094485737464,9.48253146637784,6.58));
#103958=CARTESIAN_POINT('Ctrl Pts',(109.471097310481,9.21718459007931,6.61310681434804));
#103959=CARTESIAN_POINT('Ctrl Pts',(110.531359103967,9.02452446360541,6.68281302039787));
#103960=CARTESIAN_POINT('Ctrl Pts',(111.741732863822,10.1849114394086,6.7891186181495));
#103961=CARTESIAN_POINT('Ctrl Pts',(111.433149639798,11.8900189191182,6.8989167932549));
#103962=CARTESIAN_POINT('Ctrl Pts',(109.841413191019,12.5742367163702,7.00871496836029));
#103963=CARTESIAN_POINT('Ctrl Pts',(108.630525892921,11.7818558153983,7.10042811247656));
#103964=CARTESIAN_POINT('Ctrl Pts',(108.446950083986,11.0094136788633,7.15554186489103));
#103965=CARTESIAN_POINT('Ctrl Pts',(108.446877037961,10.7499579969204,7.17405622560371));
#103966=CARTESIAN_POINT('Origin',(110.,10.75,6.58));
#103967=CARTESIAN_POINT('',(108.046,10.75,6.58));
#103968=CARTESIAN_POINT('Origin',(110.,10.75,6.58));
#103969=CARTESIAN_POINT('',(110.90360677865,9.48387400327716,6.58));
#103970=CARTESIAN_POINT('Ctrl Pts',(110.863615890953,12.505874778859,6.58));
#103971=CARTESIAN_POINT('Ctrl Pts',(110.91572812803,12.4739601120705,6.58));
#103972=CARTESIAN_POINT('Ctrl Pts',(110.966139416693,12.439530981949,6.58));
#103973=CARTESIAN_POINT('Ctrl Pts',(111.014633065925,12.4025819390746,6.58));
#103974=CARTESIAN_POINT('Ctrl Pts',(111.071887742848,12.3589575563801,6.58));
#103975=CARTESIAN_POINT('Ctrl Pts',(111.126470551244,12.3118203447527,6.58));
#103976=CARTESIAN_POINT('Ctrl Pts',(111.178217601733,12.2615103151031,6.58));
#103977=CARTESIAN_POINT('Ctrl Pts',(111.200555824445,12.2397924271013,6.58));
#103978=CARTESIAN_POINT('Ctrl Pts',(111.22236504181,12.217482947574,6.58));
#103979=CARTESIAN_POINT('Ctrl Pts',(111.243629369983,12.1946080117045,6.58));
#103980=CARTESIAN_POINT('Ctrl Pts',(111.253927421759,12.1835299624928,6.58));
#103981=CARTESIAN_POINT('Ctrl Pts',(111.264098257918,12.1723184344817,6.58));
#103982=CARTESIAN_POINT('Ctrl Pts',(111.274128934465,12.160989281423,6.58));
#103983=CARTESIAN_POINT('Ctrl Pts',(111.321394235603,12.1076054614567,6.58));
#103984=CARTESIAN_POINT('Ctrl Pts',(111.365611705757,12.0515482090722,6.58));
#103985=CARTESIAN_POINT('Ctrl Pts',(111.406629229378,11.993155953854,6.58));
#103986=CARTESIAN_POINT('Ctrl Pts',(111.436793500335,11.9502143120222,6.58));
#103987=CARTESIAN_POINT('Ctrl Pts',(111.465226304169,11.9060091415309,6.58));
#103988=CARTESIAN_POINT('Ctrl Pts',(111.491850087055,11.8606693411838,6.58));
#103989=CARTESIAN_POINT('Ctrl Pts',(111.505971478861,11.836620877153,6.58));
#103990=CARTESIAN_POINT('Ctrl Pts',(111.519583686763,11.812253154722,6.58));
#103991=CARTESIAN_POINT('Ctrl Pts',(111.532673360189,11.7875852440055,6.58));
#103992=CARTESIAN_POINT('Ctrl Pts',(111.538699343551,11.7762290844812,6.58));
#103993=CARTESIAN_POINT('Ctrl Pts',(111.544615248108,11.7648077886736,6.58));
#103994=CARTESIAN_POINT('Ctrl Pts',(111.550412449506,11.7533380324003,6.58));
#103995=CARTESIAN_POINT('Ctrl Pts',(111.581821459515,11.6911953423588,6.58));
#103996=CARTESIAN_POINT('Ctrl Pts',(111.609799978483,11.6275397259463,6.58));
#103997=CARTESIAN_POINT('Ctrl Pts',(111.634204607343,11.5626834155388,6.58));
#103998=CARTESIAN_POINT('Ctrl Pts',(111.658058374836,11.4992910419925,6.58));
#103999=CARTESIAN_POINT('Ctrl Pts',(111.678497866089,11.4347505754478,6.58));
#104000=CARTESIAN_POINT('Ctrl Pts',(111.695340844405,11.3693475318887,6.58));
#104001=CARTESIAN_POINT('Ctrl Pts',(111.707094266335,11.3237077672309,6.58));
#104002=CARTESIAN_POINT('Ctrl Pts',(111.717095347781,11.2776478329959,6.58));
#104003=CARTESIAN_POINT('Ctrl Pts',(111.725267312939,11.2312666793572,6.58));
#104004=CARTESIAN_POINT('Ctrl Pts',(111.732144455438,11.1922344763675,6.58));
#104005=CARTESIAN_POINT('Ctrl Pts',(111.737725998123,11.152974769157,6.58));
#104006=CARTESIAN_POINT('Ctrl Pts',(111.741959093489,11.1135487316366,6.58));
#104007=CARTESIAN_POINT('Ctrl Pts',(111.743158992768,11.1023731568108,6.58));
#104008=CARTESIAN_POINT('Ctrl Pts',(111.744250311734,11.0911852598384,6.58));
#104009=CARTESIAN_POINT('Ctrl Pts',(111.74523093843,11.0799993039966,6.58));
#104010=CARTESIAN_POINT('Ctrl Pts',(111.750925211886,11.0150450337225,6.58));
#104011=CARTESIAN_POINT('Ctrl Pts',(111.752904211648,10.9500399141499,6.58));
#104012=CARTESIAN_POINT('Ctrl Pts',(111.751006925574,10.8852470369328,6.58));
#104013=CARTESIAN_POINT('Ctrl Pts',(111.750274493205,10.8602342561979,6.58));
#104014=CARTESIAN_POINT('Ctrl Pts',(111.74896384625,10.8352531697528,6.58));
#104015=CARTESIAN_POINT('Ctrl Pts',(111.747063655824,10.8103193158065,6.58));
#104016=CARTESIAN_POINT('Ctrl Pts',(111.741910029986,10.7426946440209,6.58));
#104017=CARTESIAN_POINT('Ctrl Pts',(111.732423328962,10.6754153544111,6.58));
#104018=CARTESIAN_POINT('Ctrl Pts',(111.718786593378,10.6088083758369,6.58));
#104019=CARTESIAN_POINT('Ctrl Pts',(111.712609441295,10.5786368267949,6.58));
#104020=CARTESIAN_POINT('Ctrl Pts',(111.705580063643,10.5486036087976,6.58));
#104021=CARTESIAN_POINT('Ctrl Pts',(111.697712407598,10.518741398877,6.58));
#104022=CARTESIAN_POINT('Ctrl Pts',(111.692759526394,10.49994241003,6.58));
#104023=CARTESIAN_POINT('Ctrl Pts',(111.687474399047,10.4812112234672,6.58));
#104024=CARTESIAN_POINT('Ctrl Pts',(111.681860175243,10.4625563565017,6.58));
#104025=CARTESIAN_POINT('Ctrl Pts',(111.677548653405,10.4482300900213,6.58));
#104026=CARTESIAN_POINT('Ctrl Pts',(111.673041469894,10.433944527391,6.58));
#104027=CARTESIAN_POINT('Ctrl Pts',(111.668349447529,10.4197311039683,6.58));
#104028=CARTESIAN_POINT('Ctrl Pts',(111.648040497254,10.358209719986,6.58));
#104029=CARTESIAN_POINT('Ctrl Pts',(111.624246746503,10.2979449974984,6.58));
#104030=CARTESIAN_POINT('Ctrl Pts',(111.597157677967,10.239209273296,6.58));
#104031=CARTESIAN_POINT('Ctrl Pts',(111.570152434372,10.1806553020634,6.58));
#104032=CARTESIAN_POINT('Ctrl Pts',(111.53987147901,10.1236200399665,6.58));
#104033=CARTESIAN_POINT('Ctrl Pts',(111.506462520857,10.0684054610765,6.58));
#104034=CARTESIAN_POINT('Ctrl Pts',(111.473719317685,10.0142911673477,6.58));
#104035=CARTESIAN_POINT('Ctrl Pts',(111.43797078304,9.96192508876454,6.58));
#104036=CARTESIAN_POINT('Ctrl Pts',(111.399328735281,9.91163309421039,6.58));
#104037=CARTESIAN_POINT('Ctrl Pts',(111.390569611906,9.90023323807856,6.58));
#104038=CARTESIAN_POINT('Ctrl Pts',(111.381661730486,9.88894014350557,6.58));
#104039=CARTESIAN_POINT('Ctrl Pts',(111.372606253593,9.87775796120325,6.58));
#104040=CARTESIAN_POINT('Ctrl Pts',(111.365851060438,9.86941629104745,6.58));
#104041=CARTESIAN_POINT('Ctrl Pts',(111.359019323853,9.86114327231143,6.58));
#104042=CARTESIAN_POINT('Ctrl Pts',(111.352113301533,9.852941945223,6.58));
#104043=CARTESIAN_POINT('Ctrl Pts',(111.312156197831,9.80549042222458,6.58));
#104044=CARTESIAN_POINT('Ctrl Pts',(111.269699060544,9.76041611218175,6.58));
#104045=CARTESIAN_POINT('Ctrl Pts',(111.224881640097,9.71798642199737,6.58));
#104046=CARTESIAN_POINT('Ctrl Pts',(111.180871242947,9.67632075946335,6.58));
#104047=CARTESIAN_POINT('Ctrl Pts',(111.134584090894,9.63720479812122,6.58));
#104048=CARTESIAN_POINT('Ctrl Pts',(111.08612936571,9.60093579887304,6.58));
#104049=CARTESIAN_POINT('Ctrl Pts',(111.039216000705,9.56582052799681,6.58));
#104050=CARTESIAN_POINT('Ctrl Pts',(110.990270163602,9.53337367842178,6.58));
#104051=CARTESIAN_POINT('Ctrl Pts',(110.93937862246,9.50391249752929,6.58));
#104052=CARTESIAN_POINT('Ctrl Pts',(110.927559307518,9.49707028038017,6.58));
#104053=CARTESIAN_POINT('Ctrl Pts',(110.915635013035,9.49038932175318,6.58));
#104054=CARTESIAN_POINT('Ctrl Pts',(110.90360677865,9.48387400327717,6.58));
#104055=CARTESIAN_POINT('Origin',(110.,10.75,6.58));
#104056=CARTESIAN_POINT('Origin',(110.,10.75,6.58));
#104057=CARTESIAN_POINT('Origin',(110.,10.75,5.2859437743963));
#104058=CARTESIAN_POINT('Ctrl Pts',(110.90360677865,9.48387400327716,6.58));
#104059=CARTESIAN_POINT('Ctrl Pts',(111.319548631087,9.78072272003922,6.6165993917018));
#104060=CARTESIAN_POINT('Ctrl Pts',(111.829309884247,10.8114276571461,6.68979817510539));
#104061=CARTESIAN_POINT('Ctrl Pts',(110.958511260717,12.3114074675171,6.79959635021079));
#104062=CARTESIAN_POINT('Ctrl Pts',(109.228325960441,12.4102596813202,6.90939452531617));
#104063=CARTESIAN_POINT('Ctrl Pts',(108.483008121587,11.4159579759326,6.98817700004468));
#104064=CARTESIAN_POINT('Ctrl Pts',(108.44267854523,10.8289870709956,7.03036008307139));
#104065=CARTESIAN_POINT('Ctrl Pts',(108.443317976897,10.7511999786121,7.0359437743963));
#104066=CARTESIAN_POINT('Ctrl Pts',(111.135099739944,9.15950806969049,6.34992591772793));
#104067=CARTESIAN_POINT('Ctrl Pts',(111.657600787621,9.53240578267863,6.38652530942973));
#104068=CARTESIAN_POINT('Ctrl Pts',(112.297956614477,10.8271646686361,6.45972409283333));
#104069=CARTESIAN_POINT('Ctrl Pts',(111.204070076144,12.7114208881571,6.56952226793872));
#104070=CARTESIAN_POINT('Ctrl Pts',(109.030632546899,12.8355978253293,6.67932044304411));
#104071=CARTESIAN_POINT('Ctrl Pts',(107.725779622808,11.0948404999723,6.7891186181495));
#104072=CARTESIAN_POINT('Ctrl Pts',(108.45636747918,9.04437908018243,6.8989167932549));
#104073=CARTESIAN_POINT('Ctrl Pts',(110.568989660983,8.52125780622274,7.00871496836028));
#104074=CARTESIAN_POINT('Ctrl Pts',(112.172163502637,9.99302748812491,7.11851314346568));
#104075=CARTESIAN_POINT('Ctrl Pts',(111.830899302783,12.1425466001077,7.22831131857107));
#104076=CARTESIAN_POINT('Ctrl Pts',(109.850619585433,13.0454213538711,7.33810949367646));
#104077=CARTESIAN_POINT('Ctrl Pts',(108.004074456252,11.893500419209,7.44790766878186));
#104078=CARTESIAN_POINT('Ctrl Pts',(107.944244347984,9.71792192022829,7.55770584388725));
#104079=CARTESIAN_POINT('Ctrl Pts',(109.72469674044,8.46625025519251,7.66750401899264));
#104080=CARTESIAN_POINT('Ctrl Pts',(111.751594842584,9.2589515263096,7.77730219409804));
#104081=CARTESIAN_POINT('Ctrl Pts',(112.21049383889,11.3864173132724,7.88710036920343));
#104082=CARTESIAN_POINT('Ctrl Pts',(110.690593650437,12.9441716355246,7.99689854430882));
#104083=CARTESIAN_POINT('Ctrl Pts',(108.552485197456,12.5377388906333,8.1066967194142));
#104084=CARTESIAN_POINT('Ctrl Pts',(107.710168843071,10.5309505853093,8.21649489451961));
#104085=CARTESIAN_POINT('Ctrl Pts',(108.91767288213,8.72025192310877,8.326293069625));
#104086=CARTESIAN_POINT('Ctrl Pts',(111.094058886326,8.72655133855564,8.43609124473038));
#104087=CARTESIAN_POINT('Ctrl Pts',(112.29106082336,10.5442097675935,8.54588941983578));
#104088=CARTESIAN_POINT('Ctrl Pts',(111.437141624057,12.5460883208689,8.65568759494117));
#104089=CARTESIAN_POINT('Ctrl Pts',(109.296716151948,12.9401372430785,8.76548577004656));
#104090=CARTESIAN_POINT('Ctrl Pts',(107.78585916977,11.3736102112643,8.87528394515196));
#104091=CARTESIAN_POINT('Ctrl Pts',(108.25706576797,9.2488372594989,8.98508212025735));
#104092=CARTESIAN_POINT('Ctrl Pts',(110.288519309612,8.46788126517022,9.09488029536274));
#104093=CARTESIAN_POINT('Ctrl Pts',(112.061694964162,9.72984158768768,9.20467847046813));
#104094=CARTESIAN_POINT('Ctrl Pts',(111.989274148281,11.9050314603394,9.31447664557353));
#104095=CARTESIAN_POINT('Ctrl Pts',(110.136086822123,13.0462555799335,9.42427482067892));
#104096=CARTESIAN_POINT('Ctrl Pts',(108.161076741885,12.1319083045691,9.53407299578431));
#104097=CARTESIAN_POINT('Ctrl Pts',(107.832241451546,9.98049874134283,9.64387117088971));
#104098=CARTESIAN_POINT('Ctrl Pts',(109.443949061668,8.51793443970259,9.75366934599509));
#104099=CARTESIAN_POINT('Ctrl Pts',(111.553424608837,9.05347965053842,9.86346752110049));
#104100=CARTESIAN_POINT('Ctrl Pts',(112.272299206359,11.1077228372095,9.97326569620588));
#104101=CARTESIAN_POINT('Ctrl Pts',(110.957047772743,12.8417382417903,10.0830638713113));
#104102=CARTESIAN_POINT('Ctrl Pts',(108.785062427444,12.7032629127364,10.1928620464167));
#104103=CARTESIAN_POINT('Ctrl Pts',(107.700669832091,10.8162577574453,10.3026602215221));
#104104=CARTESIAN_POINT('Ctrl Pts',(108.674600953806,8.86993971377894,10.4124583966274));
#104105=CARTESIAN_POINT('Ctrl Pts',(110.835008176012,8.60662167187442,10.5222565717328));
#104106=CARTESIAN_POINT('Ctrl Pts',(112.247929388326,10.2620217457998,10.6320547468382));
#104107=CARTESIAN_POINT('Ctrl Pts',(111.648540042177,12.354252174944,10.7418529219436));
#104108=CARTESIAN_POINT('Ctrl Pts',(109.573403926499,13.0103816274259,10.851651097049));
#104109=CARTESIAN_POINT('Ctrl Pts',(107.880149816284,11.6430534754381,10.9614492721544));
#104110=CARTESIAN_POINT('Ctrl Pts',(108.084551801994,9.47627808677931,11.0712474472598));
#104111=CARTESIAN_POINT('Ctrl Pts',(110.003632484133,8.44971825270481,11.1810456223652));
#104112=CARTESIAN_POINT('Ctrl Pts',(111.919461424199,9.48233397471366,11.2908437974706));
#104113=CARTESIAN_POINT('Ctrl Pts',(112.11701909216,11.6497441164658,11.400641972576));
#104114=CARTESIAN_POINT('Ctrl Pts',(110.419455011459,13.0117176675731,11.5104401476814));
#104115=CARTESIAN_POINT('Ctrl Pts',(108.34640149172,12.3490376097434,11.6202383227868));
#104116=CARTESIAN_POINT('Ctrl Pts',(107.753622996705,10.2549245762971,11.7300364978921));
#104117=CARTESIAN_POINT('Ctrl Pts',(109.171765395972,8.60399516008457,11.8398346729976));
#104118=CARTESIAN_POINT('Ctrl Pts',(111.33133019894,8.87413509358782,11.9496328481029));
#104119=CARTESIAN_POINT('Ctrl Pts',(112.299109453475,10.8235193461483,12.0594310232083));
#104120=CARTESIAN_POINT('Ctrl Pts',(111.208762519192,12.7070903445838,12.1692291983137));
#104121=CARTESIAN_POINT('Ctrl Pts',(109.036350749681,12.8387050721737,12.2790273734191));
#104122=CARTESIAN_POINT('Ctrl Pts',(107.726582214984,11.1005446949728,12.3888255485245));
#104123=CARTESIAN_POINT('Ctrl Pts',(108.451941481345,9.0485815134776,12.4986237236299));
#104124=CARTESIAN_POINT('Ctrl Pts',(110.563097171654,8.51970263038581,12.6084218987353));
#104125=CARTESIAN_POINT('Ctrl Pts',(112.170179054329,9.98734717223935,12.7182200738407));
#104126=CARTESIAN_POINT('Ctrl Pts',(111.83454756572,12.1377129436691,12.8280182489461));
#104127=CARTESIAN_POINT('Ctrl Pts',(109.856665808931,13.045806831973,12.9378164240515));
#104128=CARTESIAN_POINT('Ctrl Pts',(108.00707933468,11.8987582479109,13.0476145991569));
#104129=CARTESIAN_POINT('Ctrl Pts',(107.941554599805,9.7233042318488,13.1574127742623));
#104130=CARTESIAN_POINT('Ctrl Pts',(109.718654461597,8.46704452766819,13.2672109493676));
#104131=CARTESIAN_POINT('Ctrl Pts',(111.747738364555,9.25422104222753,13.377009124473));
#104132=CARTESIAN_POINT('Ctrl Pts',(112.212014332387,11.3808612270306,13.4868072995784));
#104133=CARTESIAN_POINT('Ctrl Pts',(110.696660157827,12.9418157250658,13.5966054746838));
#104134=CARTESIAN_POINT('Ctrl Pts',(108.556589694155,12.5426302847338,13.7064036497892));
#104135=CARTESIAN_POINT('Ctrl Pts',(107.710849413343,10.5347127971455,13.8162018248946));
#104136=CARTESIAN_POINT('Ctrl Pts',(108.510447412203,9.33175843476383,13.8894006082982));
#104137=CARTESIAN_POINT('Ctrl Pts',(109.07607384819,9.02823449157529,13.926));
#104138=CARTESIAN_POINT('Ctrl Pts',(111.057935419513,9.26763004755271,6.42661727848529));
#104139=CARTESIAN_POINT('Ctrl Pts',(111.544916735443,9.61517809513216,6.46321667018708));
#104140=CARTESIAN_POINT('Ctrl Pts',(112.141741037734,10.8219189981394,6.53641545359068));
#104141=CARTESIAN_POINT('Ctrl Pts',(111.122217137669,12.5780830812771,6.64621362869607));
#104142=CARTESIAN_POINT('Ctrl Pts',(109.096530351413,12.693818443993,6.75601180380146));
#104143=CARTESIAN_POINT('Ctrl Pts',(107.880381605119,11.0713981698394,6.86580997890686));
#104144=CARTESIAN_POINT('Ctrl Pts',(108.561303944473,9.16032755110486,6.97560815401225));
#104145=CARTESIAN_POINT('Ctrl Pts',(110.53030962347,8.6727681720058,7.08540632911764));
#104146=CARTESIAN_POINT('Ctrl Pts',(112.024499368246,10.044486639606,7.19520450422303));
#104147=CARTESIAN_POINT('Ctrl Pts',(111.706434380886,12.0478809876644,7.30500267932843));
#104148=CARTESIAN_POINT('Ctrl Pts',(109.860774497614,12.8893781246801,7.41480085443382));
#104149=CARTESIAN_POINT('Ctrl Pts',(108.139757896918,11.8157650188244,7.52459902953921));
#104150=CARTESIAN_POINT('Ctrl Pts',(108.083995052066,9.78808280640861,7.6343972046446));
#104151=CARTESIAN_POINT('Ctrl Pts',(109.74341191426,8.62150004593044,7.74419537975));
#104152=CARTESIAN_POINT('Ctrl Pts',(111.632521054667,9.3603133169554,7.85399355485539));
#104153=CARTESIAN_POINT('Ctrl Pts',(112.060224000132,11.3431535296936,7.96379172996079));
#104154=CARTESIAN_POINT('Ctrl Pts',(110.643646947998,12.7950113836044,8.07358990506617));
#104155=CARTESIAN_POINT('Ctrl Pts',(108.650887559929,12.4162080226842,8.18338808017156));
#104156=CARTESIAN_POINT('Ctrl Pts',(107.865832049491,10.5458416108559,8.29318625527696));
#104157=CARTESIAN_POINT('Ctrl Pts',(108.99124970855,8.85823462673231,8.40298443038235));
#104158=CARTESIAN_POINT('Ctrl Pts',(111.019684531805,8.86410580658457,8.51278260548774));
#104159=CARTESIAN_POINT('Ctrl Pts',(112.135314023955,10.5581994311237,8.62258078059314));
#104160=CARTESIAN_POINT('Ctrl Pts',(111.339444432452,12.4239898568863,8.73237895569853));
#104161=CARTESIAN_POINT('Ctrl Pts',(109.344525536706,12.7912512500102,8.84217713080392));
#104162=CARTESIAN_POINT('Ctrl Pts',(107.936376931771,11.3312170571891,8.95197530590931));
#104163=CARTESIAN_POINT('Ctrl Pts',(108.37555080575,9.35088662014198,9.0617734810147));
#104164=CARTESIAN_POINT('Ctrl Pts',(110.268905705914,8.62302017950486,9.1715716561201));
#104165=CARTESIAN_POINT('Ctrl Pts',(111.921540504384,9.79919217235273,9.28136983122548));
#104166=CARTESIAN_POINT('Ctrl Pts',(111.854042870886,11.8265121773396,9.39116800633089));
#104167=CARTESIAN_POINT('Ctrl Pts',(110.126835611168,12.8901556398784,9.50096618143627));
#104168=CARTESIAN_POINT('Ctrl Pts',(108.286087133963,12.0379658857068,9.61076435654167));
#104169=CARTESIAN_POINT('Ctrl Pts',(107.97960613622,10.0328095996804,9.72056253164706));
#104170=CARTESIAN_POINT('Ctrl Pts',(109.481749522078,8.66967072864468,9.83036070675245));
#104171=CARTESIAN_POINT('Ctrl Pts',(111.44782247533,9.16880946276298,9.94015888185785));
#104172=CARTESIAN_POINT('Ctrl Pts',(112.117827825647,11.0834047630663,10.0499570569632));
#104173=CARTESIAN_POINT('Ctrl Pts',(110.891987462706,12.699541433644,10.1597552320686));
#104174=CARTESIAN_POINT('Ctrl Pts',(108.867654140624,12.5704796867511,10.269553407174));
#104175=CARTESIAN_POINT('Ctrl Pts',(107.856978783287,10.8117535410786,10.3793515822794));
#104176=CARTESIAN_POINT('Ctrl Pts',(108.76470186133,8.99774660972897,10.4891497573848));
#104177=CARTESIAN_POINT('Ctrl Pts',(110.778244143576,8.75232898401329,10.5989479324902));
#104178=CARTESIAN_POINT('Ctrl Pts',(112.095114672999,10.2951946107433,10.7087461075956));
#104179=CARTESIAN_POINT('Ctrl Pts',(111.536471941391,12.2451947727408,10.818544282701));
#104180=CARTESIAN_POINT('Ctrl Pts',(109.602404017814,12.8567204062507,10.9283424578064));
#104181=CARTESIAN_POINT('Ctrl Pts',(108.024257680189,11.5823435112685,11.0381406329118));
#104182=CARTESIAN_POINT('Ctrl Pts',(108.214764375673,9.56286597187287,11.1479388080172));
#104183=CARTESIAN_POINT('Ctrl Pts',(110.003385547094,8.60609189246891,11.2577369831225));
#104184=CARTESIAN_POINT('Ctrl Pts',(111.788976030554,9.56851017926443,11.367535158228));
#104185=CARTESIAN_POINT('Ctrl Pts',(111.973103686457,11.5885793211039,11.4773333333333));
#104186=CARTESIAN_POINT('Ctrl Pts',(110.390940371052,12.857965622106,11.5871315084387));
#104187=CARTESIAN_POINT('Ctrl Pts',(108.458813468102,12.2403346947856,11.6969296835441));
#104188=CARTESIAN_POINT('Ctrl Pts',(107.906332180569,10.2885799083247,11.8067278586495));
#104189=CARTESIAN_POINT('Ctrl Pts',(109.228068959552,8.7498810230505,11.9165260337549));
#104190=CARTESIAN_POINT('Ctrl Pts',(111.240826090398,9.00165678673101,12.0263242088603));
#104191=CARTESIAN_POINT('Ctrl Pts',(112.142815506493,10.8185214854455,12.1361223839657));
#104192=CARTESIAN_POINT('Ctrl Pts',(111.126590587445,12.574046928972,12.2459205590711));
#104193=CARTESIAN_POINT('Ctrl Pts',(109.10185982956,12.6967144595395,12.3557187341765));
#104194=CARTESIAN_POINT('Ctrl Pts',(107.881129636909,11.0767145924571,12.4655169092819));
#104195=CARTESIAN_POINT('Ctrl Pts',(108.557178826907,9.16424430209567,12.5753150843872));
#104196=CARTESIAN_POINT('Ctrl Pts',(110.524817706812,8.67131871735124,12.6851132594926));
#104197=CARTESIAN_POINT('Ctrl Pts',(112.022649823154,10.0391924727959,12.794911434598));
#104198=CARTESIAN_POINT('Ctrl Pts',(111.709834634137,12.0433759242129,12.9047096097034));
#104199=CARTESIAN_POINT('Ctrl Pts',(109.866409697559,12.8897373978991,13.0145077848088));
#104200=CARTESIAN_POINT('Ctrl Pts',(108.142558503075,11.8206654192189,13.1243059599142));
#104201=CARTESIAN_POINT('Ctrl Pts',(108.081488153537,9.79309922734662,13.2341041350196));
#104202=CARTESIAN_POINT('Ctrl Pts',(109.737780390811,8.62224032359521,13.343902310125));
#104203=CARTESIAN_POINT('Ctrl Pts',(111.62892674083,9.35590441218188,13.4537004852304));
#104204=CARTESIAN_POINT('Ctrl Pts',(112.06164113016,11.3379751473697,13.5634986603358));
#104205=CARTESIAN_POINT('Ctrl Pts',(110.649301052932,12.7928156284369,13.6732968354412));
#104206=CARTESIAN_POINT('Ctrl Pts',(108.654713032074,12.4207668987791,13.7830950105466));
#104207=CARTESIAN_POINT('Ctrl Pts',(107.866466354452,10.5493480667357,13.892893185652));
#104208=CARTESIAN_POINT('Ctrl Pts',(108.61170751221,9.42817079637191,13.9660919690556));
#104209=CARTESIAN_POINT('Ctrl Pts',(109.13888254343,9.14528047504633,14.0026913607574));
#104210=CARTESIAN_POINT('Ctrl Pts',(110.980771099081,9.37575202541493,6.50330863924264));
#104211=CARTESIAN_POINT('Ctrl Pts',(111.432232683265,9.69795040758569,6.53990803094444));
#104212=CARTESIAN_POINT('Ctrl Pts',(111.985525460991,10.8166733276427,6.61310681434804));
#104213=CARTESIAN_POINT('Ctrl Pts',(111.040364199193,12.4447452743971,6.72290498945343));
#104214=CARTESIAN_POINT('Ctrl Pts',(109.162428155927,12.5520390626566,6.83270316455882));
#104215=CARTESIAN_POINT('Ctrl Pts',(108.034983587431,11.0479558397066,6.94250133966422));
#104216=CARTESIAN_POINT('Ctrl Pts',(108.666240409766,9.27627602202728,7.0522995147696));
#104217=CARTESIAN_POINT('Ctrl Pts',(110.491629585957,8.82427853778884,7.162097689875));
#104218=CARTESIAN_POINT('Ctrl Pts',(111.876835233855,10.0959457910871,7.27189586498039));
#104219=CARTESIAN_POINT('Ctrl Pts',(111.581969458989,11.953215375221,7.38169404008578));
#104220=CARTESIAN_POINT('Ctrl Pts',(109.870929409795,12.7333348954891,7.49149221519118));
#104221=CARTESIAN_POINT('Ctrl Pts',(108.275441337584,11.7380296184397,7.60129039029656));
#104222=CARTESIAN_POINT('Ctrl Pts',(108.223745756148,9.85824369258892,7.71108856540196));
#104223=CARTESIAN_POINT('Ctrl Pts',(109.762127088081,8.77674983666837,7.82088674050735));
#104224=CARTESIAN_POINT('Ctrl Pts',(111.51344726675,9.4616751076012,7.93068491561275));
#104225=CARTESIAN_POINT('Ctrl Pts',(111.909954161375,11.2998897461148,8.04048309071813));
#104226=CARTESIAN_POINT('Ctrl Pts',(110.596700245558,12.6458511316841,8.15028126582353));
#104227=CARTESIAN_POINT('Ctrl Pts',(108.749289922401,12.2946771547351,8.26007944092892));
#104228=CARTESIAN_POINT('Ctrl Pts',(108.021495255912,10.5607326364025,8.36987761603432));
#104229=CARTESIAN_POINT('Ctrl Pts',(109.064826534969,8.99621733035583,8.47967579113971));
#104230=CARTESIAN_POINT('Ctrl Pts',(110.945310177284,9.0016602746135,8.5894739662451));
#104231=CARTESIAN_POINT('Ctrl Pts',(111.979567224551,10.5721890946539,8.69927214135049));
#104232=CARTESIAN_POINT('Ctrl Pts',(111.241747240847,12.3018913929036,8.80907031645588));
#104233=CARTESIAN_POINT('Ctrl Pts',(109.392334921463,12.6423652569418,8.91886849156127));
#104234=CARTESIAN_POINT('Ctrl Pts',(108.086894693771,11.2888239031139,9.02866666666666));
#104235=CARTESIAN_POINT('Ctrl Pts',(108.494035843529,9.45293598078504,9.13846484177206));
#104236=CARTESIAN_POINT('Ctrl Pts',(110.249292102216,8.77815909383951,9.24826301687745));
#104237=CARTESIAN_POINT('Ctrl Pts',(111.781386044606,9.86854275701776,9.35806119198285));
#104238=CARTESIAN_POINT('Ctrl Pts',(111.718811593491,11.7479928943397,9.46785936708823));
#104239=CARTESIAN_POINT('Ctrl Pts',(110.117584400213,12.7340556998231,9.57765754219363));
#104240=CARTESIAN_POINT('Ctrl Pts',(108.41109752604,11.9440234668445,9.68745571729902));
#104241=CARTESIAN_POINT('Ctrl Pts',(108.126970820894,10.085120458018,9.79725389240441));
#104242=CARTESIAN_POINT('Ctrl Pts',(109.519549982488,8.82140701758676,9.90705206750981));
#104243=CARTESIAN_POINT('Ctrl Pts',(111.342220341822,9.28413927498756,10.0168502426152));
#104244=CARTESIAN_POINT('Ctrl Pts',(111.963356444935,11.059086688923,10.1266484177206));
#104245=CARTESIAN_POINT('Ctrl Pts',(110.826927152668,12.5573446254978,10.236446592826));
#104246=CARTESIAN_POINT('Ctrl Pts',(108.950245853805,12.4376964607659,10.3462447679314));
#104247=CARTESIAN_POINT('Ctrl Pts',(108.013287734483,10.8072493247118,10.4560429430368));
#104248=CARTESIAN_POINT('Ctrl Pts',(108.854802768855,9.12555350567899,10.5658411181422));
#104249=CARTESIAN_POINT('Ctrl Pts',(110.72148011114,8.89803629615216,10.6756392932476));
#104250=CARTESIAN_POINT('Ctrl Pts',(111.942299957671,10.3283674756868,10.7854374683529));
#104251=CARTESIAN_POINT('Ctrl Pts',(111.424403840605,12.1361373705376,10.8952356434583));
#104252=CARTESIAN_POINT('Ctrl Pts',(109.631404109129,12.7030591850754,11.0050338185637));
#104253=CARTESIAN_POINT('Ctrl Pts',(108.168365544094,11.5216335470989,11.1148319936691));
#104254=CARTESIAN_POINT('Ctrl Pts',(108.344976949352,9.64945385696643,11.2246301687745));
#104255=CARTESIAN_POINT('Ctrl Pts',(110.003138610054,8.76246553223299,11.3344283438799));
#104256=CARTESIAN_POINT('Ctrl Pts',(111.65849063691,9.6546863838152,11.4442265189853));
#104257=CARTESIAN_POINT('Ctrl Pts',(111.829188280755,11.527414525742,11.5540246940907));
#104258=CARTESIAN_POINT('Ctrl Pts',(110.362425730645,12.704213576639,11.6638228691961));
#104259=CARTESIAN_POINT('Ctrl Pts',(108.571225444483,12.1316317798277,11.7736210443015));
#104260=CARTESIAN_POINT('Ctrl Pts',(108.059041364434,10.3222352403522,11.8834192194069));
#104261=CARTESIAN_POINT('Ctrl Pts',(109.284372523132,8.89576688601643,11.9932173945123));
#104262=CARTESIAN_POINT('Ctrl Pts',(111.150321981855,9.12917847987418,12.1030155696177));
#104263=CARTESIAN_POINT('Ctrl Pts',(111.986521559511,10.8135236247426,12.212813744723));
#104264=CARTESIAN_POINT('Ctrl Pts',(111.044418655699,12.4410035133602,12.3226119198284));
#104265=CARTESIAN_POINT('Ctrl Pts',(109.167368909439,12.5547238469054,12.4324100949338));
#104266=CARTESIAN_POINT('Ctrl Pts',(108.035677058835,11.0528844899415,12.5422082700392));
#104267=CARTESIAN_POINT('Ctrl Pts',(108.662416172469,9.27990709071375,12.6520064451446));
#104268=CARTESIAN_POINT('Ctrl Pts',(110.48653824197,8.82293480431664,12.76180462025));
#104269=CARTESIAN_POINT('Ctrl Pts',(111.875120591979,10.0910377733525,12.8716027953554));
#104270=CARTESIAN_POINT('Ctrl Pts',(111.585121702554,11.9490389047567,12.9814009704608));
#104271=CARTESIAN_POINT('Ctrl Pts',(109.876153586188,12.7336679638252,13.0911991455662));
#104272=CARTESIAN_POINT('Ctrl Pts',(108.27803767147,11.7425725905269,13.2009973206716));
#104273=CARTESIAN_POINT('Ctrl Pts',(108.221421707269,9.86289422284445,13.310795495777));
#104274=CARTESIAN_POINT('Ctrl Pts',(109.756906320026,8.77743611952223,13.4205936708824));
#104275=CARTESIAN_POINT('Ctrl Pts',(111.510115117105,9.45758778213623,13.5303918459878));
#104276=CARTESIAN_POINT('Ctrl Pts',(111.911267927933,11.2950890677089,13.6401900210931));
#104277=CARTESIAN_POINT('Ctrl Pts',(110.601941948037,12.643815531808,13.7499881961985));
#104278=CARTESIAN_POINT('Ctrl Pts',(108.752836369992,12.2989035128244,13.8597863713039));
#104279=CARTESIAN_POINT('Ctrl Pts',(108.022083295562,10.5639833363259,13.9695845464093));
#104280=CARTESIAN_POINT('Ctrl Pts',(108.712967612216,9.52458315798,14.0427833298129));
#104281=CARTESIAN_POINT('Ctrl Pts',(109.20169123867,9.26232645851737,14.0793827215147));
#104282=CARTESIAN_POINT('Ctrl Pts',(110.90360677865,9.48387400327716,6.58));
#104283=CARTESIAN_POINT('Ctrl Pts',(111.319548631087,9.78072272003922,6.6165993917018));
#104284=CARTESIAN_POINT('Ctrl Pts',(111.829309884247,10.8114276571461,6.68979817510539));
#104285=CARTESIAN_POINT('Ctrl Pts',(110.958511260717,12.3114074675171,6.79959635021079));
#104286=CARTESIAN_POINT('Ctrl Pts',(109.228325960441,12.4102596813202,6.90939452531617));
#104287=CARTESIAN_POINT('Ctrl Pts',(108.189585569743,11.0245135095737,7.01919270042157));
#104288=CARTESIAN_POINT('Ctrl Pts',(108.771176875059,9.39222449294972,7.12899087552696));
#104289=CARTESIAN_POINT('Ctrl Pts',(110.452949548444,8.97578890357189,7.23878905063235));
#104290=CARTESIAN_POINT('Ctrl Pts',(111.729171099463,10.1474049425682,7.34858722573775));
#104291=CARTESIAN_POINT('Ctrl Pts',(111.457504537093,11.8585497627777,7.45838540084314));
#104292=CARTESIAN_POINT('Ctrl Pts',(109.881084321976,12.5772916662981,7.56818357594853));
#104293=CARTESIAN_POINT('Ctrl Pts',(108.41112477825,11.6602942180551,7.67798175105392));
#104294=CARTESIAN_POINT('Ctrl Pts',(108.36349646023,9.92840457876923,7.78777992615932));
#104295=CARTESIAN_POINT('Ctrl Pts',(109.780842261901,8.93199962740631,7.8975781012647));
#104296=CARTESIAN_POINT('Ctrl Pts',(111.394373478833,9.56303689824699,8.0073762763701));
#104297=CARTESIAN_POINT('Ctrl Pts',(111.759684322617,11.256625962536,8.11717445147549));
#104298=CARTESIAN_POINT('Ctrl Pts',(110.549753543119,12.4966908797639,8.22697262658089));
#104299=CARTESIAN_POINT('Ctrl Pts',(108.847692284874,12.1731462867861,8.33677080168627));
#104300=CARTESIAN_POINT('Ctrl Pts',(108.177158462332,10.5756236619491,8.44656897679167));
#104301=CARTESIAN_POINT('Ctrl Pts',(109.138403361389,9.13420003397936,8.55636715189706));
#104302=CARTESIAN_POINT('Ctrl Pts',(110.870935822764,9.13921474264243,8.66616532700245));
#104303=CARTESIAN_POINT('Ctrl Pts',(111.823820425147,10.5861787581841,8.77596350210785));
#104304=CARTESIAN_POINT('Ctrl Pts',(111.144050049243,12.179792928921,8.88576167721324));
#104305=CARTESIAN_POINT('Ctrl Pts',(109.440144306221,12.4934792638734,8.99555985231863));
#104306=CARTESIAN_POINT('Ctrl Pts',(108.237412455772,11.2464307490387,9.10535802742402));
#104307=CARTESIAN_POINT('Ctrl Pts',(108.612520881309,9.5549853414281,9.21515620252941));
#104308=CARTESIAN_POINT('Ctrl Pts',(110.229678498517,8.93329800817414,9.32495437763481));
#104309=CARTESIAN_POINT('Ctrl Pts',(111.641231584828,9.93789334168282,9.4347525527402));
#104310=CARTESIAN_POINT('Ctrl Pts',(111.583580316096,11.6694736113398,9.5445507278456));
#104311=CARTESIAN_POINT('Ctrl Pts',(110.108333189259,12.577955759768,9.65434890295098));
#104312=CARTESIAN_POINT('Ctrl Pts',(108.536107918118,11.8500810479822,9.76414707805638));
#104313=CARTESIAN_POINT('Ctrl Pts',(108.274335505568,10.1374313163555,9.87394525316177));
#104314=CARTESIAN_POINT('Ctrl Pts',(109.557350442899,8.97314330652884,9.98374342826716));
#104315=CARTESIAN_POINT('Ctrl Pts',(111.236618208315,9.39946908721214,10.0935416033726));
#104316=CARTESIAN_POINT('Ctrl Pts',(111.808885064222,11.0347686147797,10.2033397784779));
#104317=CARTESIAN_POINT('Ctrl Pts',(110.761866842631,12.4151478173515,10.3131379535833));
#104318=CARTESIAN_POINT('Ctrl Pts',(109.032837566985,12.3049132347807,10.4229361286887));
#104319=CARTESIAN_POINT('Ctrl Pts',(108.169596685679,10.802745108345,10.5327343037941));
#104320=CARTESIAN_POINT('Ctrl Pts',(108.944903676379,9.25336040162902,10.6425324788995));
#104321=CARTESIAN_POINT('Ctrl Pts',(110.664716078704,9.04374360829103,10.7523306540049));
#104322=CARTESIAN_POINT('Ctrl Pts',(111.789485242344,10.3615403406303,10.8621288291103));
#104323=CARTESIAN_POINT('Ctrl Pts',(111.312335739819,12.0270799683344,10.9719270042157));
#104324=CARTESIAN_POINT('Ctrl Pts',(109.660404200444,12.5493979639002,11.0817251793211));
#104325=CARTESIAN_POINT('Ctrl Pts',(108.312473407999,11.4609235829293,11.1915233544265));
#104326=CARTESIAN_POINT('Ctrl Pts',(108.475189523031,9.73604174205998,11.3013215295319));
#104327=CARTESIAN_POINT('Ctrl Pts',(110.002891673014,8.91883917199709,11.4111197046373));
#104328=CARTESIAN_POINT('Ctrl Pts',(111.528005243266,9.74086258836599,11.5209178797427));
#104329=CARTESIAN_POINT('Ctrl Pts',(111.685272875053,11.4662497303801,11.630716054848));
#104330=CARTESIAN_POINT('Ctrl Pts',(110.333911090238,12.5504615311719,11.7405142299534));
#104331=CARTESIAN_POINT('Ctrl Pts',(108.683637420865,12.0229288648699,11.8503124050588));
#104332=CARTESIAN_POINT('Ctrl Pts',(108.211750548298,10.3558905723798,11.9601105801642));
#104333=CARTESIAN_POINT('Ctrl Pts',(109.340676086711,9.04165274898235,12.0699087552696));
#104334=CARTESIAN_POINT('Ctrl Pts',(111.059817873312,9.25670017301735,12.179706930375));
#104335=CARTESIAN_POINT('Ctrl Pts',(111.830227612529,10.8085257640398,12.2895051054804));
#104336=CARTESIAN_POINT('Ctrl Pts',(110.962246723952,12.3079600977483,12.3993032805858));
#104337=CARTESIAN_POINT('Ctrl Pts',(109.232877989319,12.4127332342713,12.5091014556912));
#104338=CARTESIAN_POINT('Ctrl Pts',(108.190224480761,11.0290543874259,12.6188996307966));
#104339=CARTESIAN_POINT('Ctrl Pts',(108.76765351803,9.39556987933182,12.728697805902));
#104340=CARTESIAN_POINT('Ctrl Pts',(110.448258777128,8.97455089128206,12.8384959810074));
#104341=CARTESIAN_POINT('Ctrl Pts',(111.727591360803,10.1428830739091,12.9482941561128));
#104342=CARTESIAN_POINT('Ctrl Pts',(111.460408770971,11.8547018853006,13.0580923312181));
#104343=CARTESIAN_POINT('Ctrl Pts',(109.885897474817,12.5775985297513,13.1678905063236));
#104344=CARTESIAN_POINT('Ctrl Pts',(108.413516839864,11.6644797618349,13.2776886814289));
#104345=CARTESIAN_POINT('Ctrl Pts',(108.361355261002,9.93268921834226,13.3874868565343));
#104346=CARTESIAN_POINT('Ctrl Pts',(109.77603224924,8.93263191544926,13.4972850316397));
#104347=CARTESIAN_POINT('Ctrl Pts',(111.391303493381,9.55927115209057,13.6070832067451));
#104348=CARTESIAN_POINT('Ctrl Pts',(111.760894725706,11.2522029880481,13.7168813818505));
#104349=CARTESIAN_POINT('Ctrl Pts',(110.554582843142,12.4948154351791,13.8266795569559));
#104350=CARTESIAN_POINT('Ctrl Pts',(108.850959707911,12.1770401268697,13.9364777320613));
#104351=CARTESIAN_POINT('Ctrl Pts',(108.177700236671,10.578618605916,14.0462759071667));
#104352=CARTESIAN_POINT('Ctrl Pts',(108.814227712222,9.62099551958808,14.1194746905703));
#104353=CARTESIAN_POINT('Ctrl Pts',(109.264499933909,9.37937244198841,14.1560740822721));
#104354=CARTESIAN_POINT('Ctrl Pts',(109.07607384819,9.02823449157531,13.926));
#104355=CARTESIAN_POINT('Ctrl Pts',(108.510447412203,9.33175843476385,13.8894006082982));
#104356=CARTESIAN_POINT('Ctrl Pts',(108.110648412773,9.9332356159547,13.8528012165964));
#104357=CARTESIAN_POINT('Ctrl Pts',(108.051705626527,10.5686271211482,13.8162018248946));
#104358=CARTESIAN_POINT('Ctrl Pts',(108.04615904351,10.6284181822157,13.8127577806378));
#104359=CARTESIAN_POINT('Ctrl Pts',(108.043630750232,10.6885095554155,13.809313736381));
#104360=CARTESIAN_POINT('Ctrl Pts',(108.04401647614,10.7486495636155,13.8058696921242));
#104361=CARTESIAN_POINT('Origin',(110.,10.75,6.58));
#104362=CARTESIAN_POINT('',(107.846,10.75,6.38));
#104363=CARTESIAN_POINT('Origin',(110.,10.75,6.38));
#104364=CARTESIAN_POINT('Origin',(107.846,10.75,6.58));
#104365=CARTESIAN_POINT('Origin',(112.,10.75,6.38));
#104366=CARTESIAN_POINT('',(106.5,10.75,6.38));
#104367=CARTESIAN_POINT('Origin',(110.,10.75,6.38));
#104368=CARTESIAN_POINT('Origin',(110.,10.75,10.13));
#104369=CARTESIAN_POINT('Origin',(110.,10.75,13.926));
#104370=CARTESIAN_POINT('Origin',(114.,11.35,3.78));
#104371=CARTESIAN_POINT('',(113.448187929913,11.35,4.88));
#104372=CARTESIAN_POINT('',(113.448187929913,11.35,4.18));
#104373=CARTESIAN_POINT('',(113.448187929913,11.35,5.28));
#104374=CARTESIAN_POINT('',(106.551812070087,11.35,4.88));
#104375=CARTESIAN_POINT('',(114.,11.35,4.88));
#104376=CARTESIAN_POINT('',(106.551812070087,11.35,4.18));
#104377=CARTESIAN_POINT('',(106.551812070087,11.35,5.28));
#104378=CARTESIAN_POINT('',(106.958618734851,11.35,3.78));
#104379=CARTESIAN_POINT('Ctrl Pts',(106.958618734851,11.35,3.78));
#104380=CARTESIAN_POINT('Ctrl Pts',(106.767542877162,11.35,3.96746275283796));
#104381=CARTESIAN_POINT('Ctrl Pts',(106.551812070087,11.35,4.18));
#104382=CARTESIAN_POINT('',(113.041381265149,11.35,3.78));
#104383=CARTESIAN_POINT('',(113.55,11.35,3.78));
#104384=CARTESIAN_POINT('Ctrl Pts',(113.448187929913,11.35,4.18));
#104385=CARTESIAN_POINT('Ctrl Pts',(113.232457122838,11.35,3.96746275283796));
#104386=CARTESIAN_POINT('Ctrl Pts',(113.041381265149,11.35,3.78));
#104387=CARTESIAN_POINT('Origin',(106.,10.15,3.78));
#104388=CARTESIAN_POINT('',(113.448187929913,10.15,4.18));
#104389=CARTESIAN_POINT('',(113.448187929913,10.15,4.88));
#104390=CARTESIAN_POINT('',(113.448187929913,10.15,5.28));
#104391=CARTESIAN_POINT('',(113.041381265149,10.15,3.78));
#104392=CARTESIAN_POINT('Ctrl Pts',(113.041381265149,10.15,3.78));
#104393=CARTESIAN_POINT('Ctrl Pts',(113.232457122844,10.15,3.96746275284386));
#104394=CARTESIAN_POINT('Ctrl Pts',(113.448187929913,10.15,4.18));
#104395=CARTESIAN_POINT('',(106.958618734851,10.15,3.78));
#104396=CARTESIAN_POINT('',(109.55,10.15,3.78));
#104397=CARTESIAN_POINT('',(106.551812070087,10.15,4.18));
#104398=CARTESIAN_POINT('Ctrl Pts',(106.551812070087,10.15,4.18));
#104399=CARTESIAN_POINT('Ctrl Pts',(106.767542877156,10.15,3.96746275284386));
#104400=CARTESIAN_POINT('Ctrl Pts',(106.958618734851,10.15,3.78));
#104401=CARTESIAN_POINT('',(106.551812070087,10.15,4.88));
#104402=CARTESIAN_POINT('',(106.551812070087,10.15,5.28));
#104403=CARTESIAN_POINT('',(106.,10.15,4.88));
#104404=CARTESIAN_POINT('Origin',(110.,10.75,4.88));
#104405=CARTESIAN_POINT('Origin',(110.,10.75,4.88));
#104406=CARTESIAN_POINT('',(106.5,10.75,4.88));
#104407=CARTESIAN_POINT('Origin',(110.,10.75,4.88));
#104408=CARTESIAN_POINT('Origin',(110.,10.75,4.88));
#104409=CARTESIAN_POINT('Origin',(110.,10.75,3.98));
#104410=CARTESIAN_POINT('Origin',(110.,10.75,4.18));
#104411=CARTESIAN_POINT('Origin',(110.,10.75,3.78));
#104412=CARTESIAN_POINT('Origin',(110.,10.75,3.98));
#104413=CARTESIAN_POINT('Origin',(110.,10.75,3.78));
#104414=CARTESIAN_POINT('Origin',(110.,10.75,4.18));
#104415=CARTESIAN_POINT('Origin',(113.1,10.75,3.78));
#104416=CARTESIAN_POINT('Origin',(113.1,10.75,3.78));
#104417=CARTESIAN_POINT('Origin',(110.,10.75,5.28));
#104418=CARTESIAN_POINT('',(106.5,10.75,5.28));
#104419=CARTESIAN_POINT('Origin',(110.,10.75,14.13));
#104420=CARTESIAN_POINT('',(108.5,10.75,14.38));
#104421=CARTESIAN_POINT('Origin',(110.,10.75,14.38));
#104422=CARTESIAN_POINT('',(108.25,10.75,14.13));
#104423=CARTESIAN_POINT('Origin',(110.,10.75,14.38));
#104424=CARTESIAN_POINT('',(0.,0.,0.));
#104425=CARTESIAN_POINT('Origin',(110.,21.8,63.));
#104426=CARTESIAN_POINT('',(108.535151454168,22.7758449541571,63.0010722055425));
#104427=CARTESIAN_POINT('',(108.535593634877,22.8471550458429,63.0009419999783));
#104428=CARTESIAN_POINT('',(108.5365,21.8,63.));
#104429=CARTESIAN_POINT('',(110.634804239707,22.9365,64.3198481804742));
#104430=CARTESIAN_POINT('Ctrl Pts',(108.535151454168,22.7758449541571,63.0010722055425));
#104431=CARTESIAN_POINT('Ctrl Pts',(108.534609827122,22.7795299873345,63.0686757060681));
#104432=CARTESIAN_POINT('Ctrl Pts',(108.538890809892,22.7832150205118,63.1362086042706));
#104433=CARTESIAN_POINT('Ctrl Pts',(108.548231063953,22.7869000536892,63.2030316078625));
#104434=CARTESIAN_POINT('Ctrl Pts',(108.614676337293,22.8131148691669,63.6784011973634));
#104435=CARTESIAN_POINT('Ctrl Pts',(108.937156278306,22.8393296846445,64.1178451327055));
#104436=CARTESIAN_POINT('Ctrl Pts',(109.370783358443,22.8655445001221,64.3239705993014));
#104437=CARTESIAN_POINT('Ctrl Pts',(109.76201538597,22.8891963334148,64.5099434960951));
#104438=CARTESIAN_POINT('Ctrl Pts',(110.243723602036,22.9128481667074,64.5059900849878));
#104439=CARTESIAN_POINT('Ctrl Pts',(110.635601384839,22.9365,64.3206560833115));
#104440=CARTESIAN_POINT('',(109.365992905425,22.9365,64.3190402776368));
#104441=CARTESIAN_POINT('Origin',(110.,22.9365,63.));
#104442=CARTESIAN_POINT('Ctrl Pts',(109.365992905425,22.9365,64.3190402776368));
#104443=CARTESIAN_POINT('Ctrl Pts',(108.931467947367,22.9102851845224,64.1101824354244));
#104444=CARTESIAN_POINT('Ctrl Pts',(108.611923832083,22.8840703690447,63.6711875655686));
#104445=CARTESIAN_POINT('Ctrl Pts',(108.547797686055,22.8578555535671,63.1962282360989));
#104446=CARTESIAN_POINT('Ctrl Pts',(108.53907256493,22.854288717659,63.1316043980001));
#104447=CARTESIAN_POINT('Ctrl Pts',(108.535075951473,22.850721881751,63.0663147562245));
#104448=CARTESIAN_POINT('Ctrl Pts',(108.535593634877,22.8471550458429,63.0009419999783));
#104449=CARTESIAN_POINT('Origin',(110.,21.8,63.));
#104450=CARTESIAN_POINT('',(108.538691682754,22.2758449541571,63.0000133350456));
#104451=CARTESIAN_POINT('',(108.538693030964,22.3471550458429,63.0000503801031));
#104452=CARTESIAN_POINT('',(108.5365,21.8,63.));
#104453=CARTESIAN_POINT('Ctrl Pts',(108.538691682754,22.2758449541571,63.0000133350456));
#104454=CARTESIAN_POINT('Ctrl Pts',(108.538672353139,22.2889077611353,63.2411582590056));
#104455=CARTESIAN_POINT('Ctrl Pts',(108.595183258915,22.3019705681134,63.4822945262169));
#104456=CARTESIAN_POINT('Ctrl Pts',(108.708275285749,22.3150333750916,63.6930719321842));
#104457=CARTESIAN_POINT('Ctrl Pts',(108.935231606881,22.3412481905693,64.1160660722281));
#104458=CARTESIAN_POINT('Ctrl Pts',(109.390060544541,22.3674630060469,64.4167941097764));
#104459=CARTESIAN_POINT('Ctrl Pts',(109.868150657905,22.3936778215245,64.4599709248855));
#104460=CARTESIAN_POINT('Ctrl Pts',(110.346240771269,22.4198926370022,64.5031477399947));
#104461=CARTESIAN_POINT('Ctrl Pts',(110.847592060336,22.4461074524798,64.2887733326647));
#104462=CARTESIAN_POINT('Ctrl Pts',(111.146657814542,22.4723222679575,63.9132814736071));
#104463=CARTESIAN_POINT('Ctrl Pts',(111.445723568747,22.4985370834351,63.5377896145496));
#104464=CARTESIAN_POINT('Ctrl Pts',(111.542503788091,22.5247518989128,63.0011803037645));
#104465=CARTESIAN_POINT('Ctrl Pts',(111.393469204247,22.5509667143904,62.544871616519));
#104466=CARTESIAN_POINT('Ctrl Pts',(111.244434620402,22.5771815298681,62.0885629292735));
#104467=CARTESIAN_POINT('Ctrl Pts',(110.849585233369,22.6033963453457,61.7125548655677));
#104468=CARTESIAN_POINT('Ctrl Pts',(110.386531995343,22.6296111608233,61.5859716219114));
#104469=CARTESIAN_POINT('Ctrl Pts',(109.923478757317,22.655825976301,61.4593883782552));
#104470=CARTESIAN_POINT('Ctrl Pts',(109.392221668298,22.6820407917786,61.5822299546486));
#104471=CARTESIAN_POINT('Ctrl Pts',(109.031798426622,22.7082556072563,61.8992983646752));
#104472=CARTESIAN_POINT('Ctrl Pts',(108.722040107787,22.7307853895566,62.1717962679423));
#104473=CARTESIAN_POINT('Ctrl Pts',(108.538462886891,22.7533151718568,62.5877537695155));
#104474=CARTESIAN_POINT('Ctrl Pts',(108.535151454168,22.7758449541571,63.0010722055425));
#104475=CARTESIAN_POINT('Ctrl Pts',(108.535593634877,22.8471550458429,63.0009419999783));
#104476=CARTESIAN_POINT('Ctrl Pts',(108.538880717169,22.8245070662733,62.5858511782983));
#104477=CARTESIAN_POINT('Ctrl Pts',(108.724172575191,22.8018590867037,62.1674093960939));
#104478=CARTESIAN_POINT('Ctrl Pts',(109.036631363694,22.7792111071341,61.8947847597746));
#104479=CARTESIAN_POINT('Ctrl Pts',(109.398299364136,22.7529962916565,61.5792244020037));
#104480=CARTESIAN_POINT('Ctrl Pts',(109.930343541793,22.7267814761789,61.4590274755454));
#104481=CARTESIAN_POINT('Ctrl Pts',(110.392891232344,22.7005666607012,61.5877509572053));
#104482=CARTESIAN_POINT('Ctrl Pts',(110.855438922895,22.6743518452236,61.7164744388652));
#104483=CARTESIAN_POINT('Ctrl Pts',(111.248490126339,22.6481370297459,62.0941183286433));
#104484=CARTESIAN_POINT('Ctrl Pts',(111.395458055825,22.6219222142683,62.5510554934448));
#104485=CARTESIAN_POINT('Ctrl Pts',(111.542425985311,22.5957073987906,63.0079926582463));
#104486=CARTESIAN_POINT('Ctrl Pts',(111.443310640837,22.569492583313,63.5442230980713));
#104487=CARTESIAN_POINT('Ctrl Pts',(111.142589280421,22.5432777678353,63.9183940558093));
#104488=CARTESIAN_POINT('Ctrl Pts',(110.841867920004,22.5170629523577,64.2925650135474));
#104489=CARTESIAN_POINT('Ctrl Pts',(110.339540543643,22.4908481368801,64.5046764891985));
#104490=CARTESIAN_POINT('Ctrl Pts',(109.861640737496,22.4646333214024,64.4593626824467));
#104491=CARTESIAN_POINT('Ctrl Pts',(109.383740931348,22.4384185059248,64.4140488756948));
#104492=CARTESIAN_POINT('Ctrl Pts',(108.930268695415,22.4122036904471,64.1113097865399));
#104493=CARTESIAN_POINT('Ctrl Pts',(108.705202697107,22.3859888749695,63.6873119495992));
#104494=CARTESIAN_POINT('Ctrl Pts',(108.594067392366,22.3730442652606,63.4779461228103));
#104495=CARTESIAN_POINT('Ctrl Pts',(108.538624017936,22.3600996555518,63.2390139680548));
#104496=CARTESIAN_POINT('Ctrl Pts',(108.538693030964,22.3471550458429,63.0000503801031));
#104497=CARTESIAN_POINT('Origin',(110.,21.8,63.));
#104498=CARTESIAN_POINT('',(108.535165354128,21.7758449541571,62.9989599428665));
#104499=CARTESIAN_POINT('',(108.535223168726,21.8471550458429,62.9989389776376));
#104500=CARTESIAN_POINT('',(108.5365,21.8,63.));
#104501=CARTESIAN_POINT('Ctrl Pts',(108.535165354128,21.7758449541571,62.9989599428665));
#104502=CARTESIAN_POINT('Ctrl Pts',(108.538492774415,21.7982855349361,63.4106834579473));
#104503=CARTESIAN_POINT('Ctrl Pts',(108.720485196504,21.820726115715,63.8249854635966));
#104504=CARTESIAN_POINT('Ctrl Pts',(109.02811348844,21.843166696494,64.0974234057879));
#104505=CARTESIAN_POINT('Ctrl Pts',(109.387481144217,21.8693815119716,64.4156821199451));
#104506=CARTESIAN_POINT('Ctrl Pts',(109.91829942634,21.8955963274493,64.5403441919538));
#104507=CARTESIAN_POINT('Ctrl Pts',(110.381769684567,21.9218111429269,64.4153280294225));
#104508=CARTESIAN_POINT('Ctrl Pts',(110.845239942795,21.9480259584046,64.2903118668911));
#104509=CARTESIAN_POINT('Ctrl Pts',(111.241362177127,21.9742407738822,63.9156174698199));
#104510=CARTESIAN_POINT('Ctrl Pts',(111.391933201201,22.0004555893599,63.4598081819617));
#104511=CARTESIAN_POINT('Ctrl Pts',(111.542504225274,22.0266704048375,63.0039988941035));
#104512=CARTESIAN_POINT('Ctrl Pts',(111.447524039089,22.0528852203152,62.4670747154584));
#104513=CARTESIAN_POINT('Ctrl Pts',(111.149721391282,22.0791000357928,62.0905813507677));
#104514=CARTESIAN_POINT('Ctrl Pts',(110.851918743475,22.1053148512705,61.7140879860771));
#104515=CARTESIAN_POINT('Ctrl Pts',(110.351293634045,22.1315296667481,61.4980254353409));
#104516=CARTESIAN_POINT('Ctrl Pts',(109.873061584462,22.1577444822257,61.5395932303822));
#104517=CARTESIAN_POINT('Ctrl Pts',(109.39482953488,22.1839592977034,61.5811610254236));
#104518=CARTESIAN_POINT('Ctrl Pts',(108.938990545144,22.210174113181,61.8803591662424));
#104519=CARTESIAN_POINT('Ctrl Pts',(108.710612902578,22.2363889286587,62.3025883579216));
#104520=CARTESIAN_POINT('Ctrl Pts',(108.596035529387,22.2495409371582,62.5144213163656));
#104521=CARTESIAN_POINT('Ctrl Pts',(108.538711144364,22.2626929456576,62.7572217133958));
#104522=CARTESIAN_POINT('Ctrl Pts',(108.538691682754,22.2758449541571,63.0000133350456));
#104523=CARTESIAN_POINT('Ctrl Pts',(108.538693030964,22.3471550458429,63.0000503801031));
#104524=CARTESIAN_POINT('Ctrl Pts',(108.538763779879,22.3338848400741,62.7550761356344));
#104525=CARTESIAN_POINT('Ctrl Pts',(108.597174646194,22.3206146343053,62.5100688568027));
#104526=CARTESIAN_POINT('Ctrl Pts',(108.713732195287,22.3073444285366,62.296848641938));
#104527=CARTESIAN_POINT('Ctrl Pts',(108.943987452459,22.2811296130589,61.8756397559441));
#104528=CARTESIAN_POINT('Ctrl Pts',(109.401157727483,22.2549147975813,61.5784785686831));
#104529=CARTESIAN_POINT('Ctrl Pts',(109.879570904104,22.2286999821036,61.5390428883785));
#104530=CARTESIAN_POINT('Ctrl Pts',(110.357984080725,22.202485166626,61.4996072080739));
#104531=CARTESIAN_POINT('Ctrl Pts',(110.857640158943,22.1762703511483,61.7178970347256));
#104532=CARTESIAN_POINT('Ctrl Pts',(111.153761860065,22.1500555356707,62.0957132578734));
#104533=CARTESIAN_POINT('Ctrl Pts',(111.449883561187,22.123840720193,62.4735294810212));
#104534=CARTESIAN_POINT('Ctrl Pts',(111.542470885215,22.0976259047154,63.010872100665));
#104535=CARTESIAN_POINT('Ctrl Pts',(111.389870482629,22.0714110892377,63.4660060388398));
#104536=CARTESIAN_POINT('Ctrl Pts',(111.237270080043,22.0451962737601,63.9211399770146));
#104537=CARTESIAN_POINT('Ctrl Pts',(110.839481950845,22.0189814582824,64.2940652337204));
#104538=CARTESIAN_POINT('Ctrl Pts',(110.37545920875,21.9927666428048,64.4170148824867));
#104539=CARTESIAN_POINT('Ctrl Pts',(109.911436466654,21.9665518273272,64.539964531253));
#104540=CARTESIAN_POINT('Ctrl Pts',(109.381179111661,21.9403370118495,64.4129385720798));
#104541=CARTESIAN_POINT('Ctrl Pts',(109.023233243215,21.9141221963719,64.0930817722642));
#104542=CARTESIAN_POINT('Ctrl Pts',(108.718435944223,21.8917998128622,63.8207179953862));
#104543=CARTESIAN_POINT('Ctrl Pts',(108.53857871652,21.8694774293526,63.4085359193364));
#104544=CARTESIAN_POINT('Ctrl Pts',(108.535223168726,21.8471550458429,62.9989389776376));
#104545=CARTESIAN_POINT('Origin',(110.,21.8,63.));
#104546=CARTESIAN_POINT('',(108.536119189169,21.2758449541571,63.0012553724788));
#104547=CARTESIAN_POINT('',(108.536055248516,21.3471550458429,63.0012487939741));
#104548=CARTESIAN_POINT('',(108.5365,21.8,63.));
#104549=CARTESIAN_POINT('Ctrl Pts',(108.536119189169,21.2758449541571,63.0012553724788));
#104550=CARTESIAN_POINT('Ctrl Pts',(108.535196141184,21.2814484932592,63.1042391566118));
#104551=CARTESIAN_POINT('Ctrl Pts',(108.54515759093,21.2870520323614,63.2070458445866));
#104552=CARTESIAN_POINT('Ctrl Pts',(108.566672435597,21.2926555714635,63.3073748311208));
#104553=CARTESIAN_POINT('Ctrl Pts',(108.667324482937,21.3188703869411,63.7767399628927));
#104554=CARTESIAN_POINT('Ctrl Pts',(109.020835529846,21.3450852024187,64.191877821057));
#104555=CARTESIAN_POINT('Ctrl Pts',(109.468165106858,21.3713000178964,64.3660347715043));
#104556=CARTESIAN_POINT('Ctrl Pts',(109.915494683871,21.397514833374,64.5401917219516));
#104557=CARTESIAN_POINT('Ctrl Pts',(110.456642790987,21.4237296488517,64.4733677646819));
#104558=CARTESIAN_POINT('Ctrl Pts',(110.848166840665,21.4499444643293,64.1956230388321));
#104559=CARTESIAN_POINT('Ctrl Pts',(111.239690890343,21.476159279807,63.9178783129823));
#104560=CARTESIAN_POINT('Ctrl Pts',(111.481590882581,21.5023740952846,63.4292128185525));
#104561=CARTESIAN_POINT('Ctrl Pts',(111.465042009041,21.5285889107623,62.9494629121278));
#104562=CARTESIAN_POINT('Ctrl Pts',(111.4484931355,21.5548037262399,62.4697130057031));
#104563=CARTESIAN_POINT('Ctrl Pts',(111.17349539618,21.5810185417176,61.9988786872835));
#104564=CARTESIAN_POINT('Ctrl Pts',(110.763762457964,21.6072333571952,61.7487733211406));
#104565=CARTESIAN_POINT('Ctrl Pts',(110.354029519748,21.6334481726728,61.4986679549978));
#104566=CARTESIAN_POINT('Ctrl Pts',(109.809561382636,21.6596629881505,61.4692915411317));
#104567=CARTESIAN_POINT('Ctrl Pts',(109.375297068792,21.6858778036281,61.6738598094909));
#104568=CARTESIAN_POINT('Ctrl Pts',(108.941032754949,21.7120926191058,61.87842807785));
#104569=CARTESIAN_POINT('Ctrl Pts',(108.616972264375,21.7383074345834,62.3169410284346));
#104570=CARTESIAN_POINT('Ctrl Pts',(108.548900533804,21.7645222500611,62.7921251818797));
#104571=CARTESIAN_POINT('Ctrl Pts',(108.539100018986,21.7682964847597,62.86053903441));
#104572=CARTESIAN_POINT('Ctrl Pts',(108.534605722217,21.7720707194584,62.9297130195276));
#104573=CARTESIAN_POINT('Ctrl Pts',(108.535165354128,21.7758449541571,62.9989599428665));
#104574=CARTESIAN_POINT('Ctrl Pts',(108.535223168726,21.8471550458429,62.9989389776376));
#104575=CARTESIAN_POINT('Ctrl Pts',(108.534638050138,21.8432626138749,62.9275161284974));
#104576=CARTESIAN_POINT('Ctrl Pts',(108.539419661893,21.8393701819069,62.856171883249));
#104577=CARTESIAN_POINT('Ctrl Pts',(108.549841384691,21.8354777499389,62.7856612678053));
#104578=CARTESIAN_POINT('Ctrl Pts',(108.620029776514,21.8092629344613,62.3107852036201));
#104579=CARTESIAN_POINT('Ctrl Pts',(108.94604094206,21.7830481189837,61.8737207157076));
#104580=CARTESIAN_POINT('Ctrl Pts',(109.381212483832,21.756833303506,61.6710895313997));
#104581=CARTESIAN_POINT('Ctrl Pts',(109.816384025604,21.7306184880284,61.4684583470919));
#104582=CARTESIAN_POINT('Ctrl Pts',(110.360715943603,21.7044036725507,61.5002604663887));
#104583=CARTESIAN_POINT('Ctrl Pts',(110.769330222778,21.6781888570731,61.7521891040544));
#104584=CARTESIAN_POINT('Ctrl Pts',(111.177944501954,21.6519740415954,62.0041177417202));
#104585=CARTESIAN_POINT('Ctrl Pts',(111.450841142307,21.6257592261178,62.4761728977549));
#104586=CARTESIAN_POINT('Ctrl Pts',(111.465252320939,21.5995444106401,62.9559916183289));
#104587=CARTESIAN_POINT('Ctrl Pts',(111.479663499571,21.5733295951625,63.4358103389028));
#104588=CARTESIAN_POINT('Ctrl Pts',(111.235589216481,21.5471147796848,63.923392624016));
#104589=CARTESIAN_POINT('Ctrl Pts',(110.842831074243,21.5208999642072,64.1993901943523));
#104590=CARTESIAN_POINT('Ctrl Pts',(110.450072932004,21.4946851487296,64.4753877646886));
#104591=CARTESIAN_POINT('Ctrl Pts',(109.908630930616,21.4684703332519,64.539800620248));
#104592=CARTESIAN_POINT('Ctrl Pts',(109.46208276499,21.4422555177743,64.3636516574638));
#104593=CARTESIAN_POINT('Ctrl Pts',(109.015534599365,21.4160407022966,64.1875026946796));
#104594=CARTESIAN_POINT('Ctrl Pts',(108.663880269501,21.389825886819,63.7707919135518));
#104595=CARTESIAN_POINT('Ctrl Pts',(108.565318787313,21.3636110713413,63.3009840605131));
#104596=CARTESIAN_POINT('Ctrl Pts',(108.54469520437,21.3581257295085,63.2026787082648));
#104597=CARTESIAN_POINT('Ctrl Pts',(108.535152996528,21.3526403876757,63.102048562661));
#104598=CARTESIAN_POINT('Ctrl Pts',(108.536055248516,21.3471550458429,63.0012487939741));
#104599=CARTESIAN_POINT('Origin',(110.,21.8,63.));
#104600=CARTESIAN_POINT('',(108.538910502742,20.7758449541571,62.9995078540291));
#104601=CARTESIAN_POINT('',(108.538556703894,20.8471550458429,62.999470885696));
#104602=CARTESIAN_POINT('',(108.5365,21.8,63.));
#104603=CARTESIAN_POINT('Ctrl Pts',(108.538910502742,20.7758449541571,62.9995078540291));
#104604=CARTESIAN_POINT('Ctrl Pts',(108.539674695123,20.79082626706,63.2759626459345));
#104605=CARTESIAN_POINT('Ctrl Pts',(108.614868059699,20.8058075799629,63.553027697966));
#104606=CARTESIAN_POINT('Ctrl Pts',(108.761582448019,20.8207888928659,63.7847945943861));
#104607=CARTESIAN_POINT('Ctrl Pts',(109.018308319953,20.8470037083435,64.1903482640043));
#104608=CARTESIAN_POINT('Ctrl Pts',(109.494025855479,20.8732185238212,64.4572025982981));
#104609=CARTESIAN_POINT('Ctrl Pts',(109.974076621128,20.8994333392988,64.465653338363));
#104610=CARTESIAN_POINT('Ctrl Pts',(110.454127386776,20.9256481547764,64.474104078428));
#104611=CARTESIAN_POINT('Ctrl Pts',(110.938511382548,20.9518629702541,64.2241512242641));
#104612=CARTESIAN_POINT('Ctrl Pts',(111.209619270879,20.9780777857317,63.8280556122507));
#104613=CARTESIAN_POINT('Ctrl Pts',(111.48072715921,21.0042926012094,63.4319600002372));
#104614=CARTESIAN_POINT('Ctrl Pts',(111.5385589401,21.030507416687,62.8897216303742));
#104615=CARTESIAN_POINT('Ctrl Pts',(111.356956870685,21.0567222321647,62.445359190286));
#104616=CARTESIAN_POINT('Ctrl Pts',(111.175354801269,21.0829370476423,62.0009967501978));
#104617=CARTESIAN_POINT('Ctrl Pts',(110.754318881549,21.10915186312,61.6545102398845));
#104618=CARTESIAN_POINT('Ctrl Pts',(110.283326143503,21.1353666785976,61.5617338445643));
#104619=CARTESIAN_POINT('Ctrl Pts',(109.812333405456,21.1615814940752,61.4689574492441));
#104620=CARTESIAN_POINT('Ctrl Pts',(109.291383849084,21.1877963095529,61.629891168917));
#104621=CARTESIAN_POINT('Ctrl Pts',(108.954805594784,21.2140111250305,61.9721542314433));
#104622=CARTESIAN_POINT('Ctrl Pts',(108.6901725125,21.234622401406,62.2412569676757));
#104623=CARTESIAN_POINT('Ctrl Pts',(108.539514400086,21.2552336777816,62.6224541901762));
#104624=CARTESIAN_POINT('Ctrl Pts',(108.536119189169,21.2758449541571,63.0012553724788));
#104625=CARTESIAN_POINT('Ctrl Pts',(108.536055248516,21.3471550458429,63.0012487939741));
#104626=CARTESIAN_POINT('Ctrl Pts',(108.539464919121,21.3264255721981,62.6203197266359));
#104627=CARTESIAN_POINT('Ctrl Pts',(108.69203553938,21.3056960985532,62.2369682132769));
#104628=CARTESIAN_POINT('Ctrl Pts',(108.959392687981,21.2849666249084,61.967509145852));
#104629=CARTESIAN_POINT('Ctrl Pts',(109.297496705348,21.2587518094308,61.626747009179));
#104630=CARTESIAN_POINT('Ctrl Pts',(109.819173374592,21.2325369939531,61.4681276607825));
#104631=CARTESIAN_POINT('Ctrl Pts',(110.289739334968,21.2063221784755,61.5630066225246));
#104632=CARTESIAN_POINT('Ctrl Pts',(110.760305295344,21.1801073629978,61.6578855842667));
#104633=CARTESIAN_POINT('Ctrl Pts',(111.179760546851,21.1538925475202,62.0062628561474));
#104634=CARTESIAN_POINT('Ctrl Pts',(111.35939915459,21.1276777320425,62.45141943501));
#104635=CARTESIAN_POINT('Ctrl Pts',(111.539037762329,21.1014629165649,62.8965760138725));
#104636=CARTESIAN_POINT('Ctrl Pts',(111.478859726299,21.0752481010872,63.4385118997171));
#104637=CARTESIAN_POINT('Ctrl Pts',(111.205950097226,21.0490332856096,63.8334159433577));
#104638=CARTESIAN_POINT('Ctrl Pts',(110.933040468152,21.022818470132,64.2283199869983));
#104639=CARTESIAN_POINT('Ctrl Pts',(110.447399246034,20.9966036546543,64.4761921884351));
#104640=CARTESIAN_POINT('Ctrl Pts',(109.967474020253,20.9703888391767,64.465545900025));
#104641=CARTESIAN_POINT('Ctrl Pts',(109.487548794472,20.944174023699,64.4548996116149));
#104642=CARTESIAN_POINT('Ctrl Pts',(109.013339565028,20.9179592082214,64.1857348333581));
#104643=CARTESIAN_POINT('Ctrl Pts',(108.758236669621,20.8917443927437,63.7790903264723));
#104644=CARTESIAN_POINT('Ctrl Pts',(108.613599991322,20.8768812771101,63.5485335127969));
#104645=CARTESIAN_POINT('Ctrl Pts',(108.539397099341,20.8620181614765,63.273782550778));
#104646=CARTESIAN_POINT('Ctrl Pts',(108.538556703894,20.8471550458429,62.999470885696));
#104647=CARTESIAN_POINT('Origin',(110.,23.8608671147362,63.));
#104648=CARTESIAN_POINT('',(108.821943542907,21.1108671147362,63.0010102596085));
#104649=CARTESIAN_POINT('',(108.823905130175,21.0121328852639,62.9995741958514));
#104650=CARTESIAN_POINT('',(108.82225,23.8608671147362,63.));
#104651=CARTESIAN_POINT('',(109.068873933122,20.6635,63.7239975350757));
#104652=CARTESIAN_POINT('Ctrl Pts',(108.821943542907,21.1108671147362,63.0010102596084));
#104653=CARTESIAN_POINT('Ctrl Pts',(108.824675835122,21.0902558383607,62.696170428753));
#104654=CARTESIAN_POINT('Ctrl Pts',(109.100121495157,21.0434297465075,61.9992340416389));
#104655=CARTESIAN_POINT('Ctrl Pts',(110.26820909347,20.9703888391767,61.6383839750614));
#104656=CARTESIAN_POINT('Ctrl Pts',(111.284693660161,20.8917443927437,62.4748878784196));
#104657=CARTESIAN_POINT('Ctrl Pts',(111.145073475788,20.8130999463108,63.7839850566352));
#104658=CARTESIAN_POINT('Ctrl Pts',(110.013761905485,20.7370184820629,64.367766846319));
#104659=CARTESIAN_POINT('Ctrl Pts',(109.284876061192,20.6871518332926,63.997935414755));
#104660=CARTESIAN_POINT('Ctrl Pts',(109.068873933122,20.6635,63.7239975350757));
#104661=CARTESIAN_POINT('',(110.383133178262,20.6635,64.1136893777958));
#104662=CARTESIAN_POINT('Origin',(110.,20.6635,63.));
#104663=CARTESIAN_POINT('Ctrl Pts',(108.823905130175,21.0121328852639,62.9995741958514));
#104664=CARTESIAN_POINT('Ctrl Pts',(108.823388600688,21.0007811854198,62.8309749199433));
#104665=CARTESIAN_POINT('Ctrl Pts',(108.935645570376,20.9632146700981,62.2737067942396));
#104666=CARTESIAN_POINT('Ctrl Pts',(109.786099850077,20.8994333392988,61.6289388285546));
#104667=CARTESIAN_POINT('Ctrl Pts',(111.02805441837,20.8207888928659,62.0667289458579));
#104668=CARTESIAN_POINT('Ctrl Pts',(111.343096451131,20.7421444464329,63.3456128208481));
#104669=CARTESIAN_POINT('Ctrl Pts',(110.750010398298,20.6897148154776,63.9874756972607));
#104670=CARTESIAN_POINT('Ctrl Pts',(110.383133178262,20.6635,64.1136893777958));
#104671=CARTESIAN_POINT('Origin',(110.,23.8608671147362,63.));
#104672=CARTESIAN_POINT('',(108.821175945217,21.6108671147362,62.9991630151766));
#104673=CARTESIAN_POINT('',(108.821892086737,21.5121328852639,63.0010049655641));
#104674=CARTESIAN_POINT('',(108.82225,23.8608671147362,63.));
#104675=CARTESIAN_POINT('Ctrl Pts',(108.821175945217,21.6108671147362,62.9991630151766));
#104676=CARTESIAN_POINT('Ctrl Pts',(108.820725582058,21.6070928800375,62.9434366305081));
#104677=CARTESIAN_POINT('Ctrl Pts',(108.849463542357,21.5771038298612,62.5011162097095));
#104678=CARTESIAN_POINT('Ctrl Pts',(109.40858460534,21.5208999642072,61.7445234309101));
#104679=CARTESIAN_POINT('Ctrl Pts',(110.72306499171,21.4422555177743,61.815445340232));
#104680=CARTESIAN_POINT('Ctrl Pts',(111.38697736783,21.3636110713413,62.9521555251011));
#104681=CARTESIAN_POINT('Ctrl Pts',(110.80297111735,21.2849666249084,64.1319145672564));
#104682=CARTESIAN_POINT('Ctrl Pts',(109.496506102338,21.2063221784755,64.2932440835005));
#104683=CARTESIAN_POINT('Ctrl Pts',(108.866720300925,21.1482890084181,63.553669094296));
#104684=CARTESIAN_POINT('Ctrl Pts',(108.821200721065,21.1164706538383,63.0838863455412));
#104685=CARTESIAN_POINT('Ctrl Pts',(108.821943542907,21.1108671147362,63.0010102596084));
#104686=CARTESIAN_POINT('Ctrl Pts',(108.821892086737,21.5121328852639,63.0010049655641));
#104687=CARTESIAN_POINT('Ctrl Pts',(108.824636015371,21.491403411619,62.694452721589));
#104688=CARTESIAN_POINT('Ctrl Pts',(109.102687866082,21.4444591224965,61.9958149525211));
#104689=CARTESIAN_POINT('Ctrl Pts',(110.274298694314,21.3713000178964,61.6395786914333));
#104690=CARTESIAN_POINT('Ctrl Pts',(111.286967138036,21.2926555714635,62.4806473596071));
#104691=CARTESIAN_POINT('Ctrl Pts',(111.141682515009,21.2140111250305,63.7890142667887));
#104692=CARTESIAN_POINT('Ctrl Pts',(109.969224812209,21.1353666785976,64.3874389034312));
#104693=CARTESIAN_POINT('Ctrl Pts',(108.989617906622,21.0680739320087,63.8314065465111));
#104694=CARTESIAN_POINT('Ctrl Pts',(108.824581437478,21.0269960008975,63.2203262037437));
#104695=CARTESIAN_POINT('Ctrl Pts',(108.823905130175,21.0121328852639,62.9995741958514));
#104696=CARTESIAN_POINT('Origin',(110.,23.8608671147362,63.));
#104697=CARTESIAN_POINT('',(108.824013754263,22.1108671147362,63.0000107313632));
#104698=CARTESIAN_POINT('',(108.82122247145,22.0121328852639,62.999146143432));
#104699=CARTESIAN_POINT('',(108.82225,23.8608671147362,63.));
#104700=CARTESIAN_POINT('Ctrl Pts',(108.824013754263,22.1108671147362,63.0000107313632));
#104701=CARTESIAN_POINT('Ctrl Pts',(108.824029415972,22.0977151062367,62.8046244434246));
#104702=CARTESIAN_POINT('Ctrl Pts',(108.962111740001,22.0583482822596,62.2197696197103));
#104703=CARTESIAN_POINT('Ctrl Pts',(109.879825660995,21.9927666428048,61.6174115390114));
#104704=CARTESIAN_POINT('Ctrl Pts',(111.088458163825,21.9141221963719,62.1390398324099));
#104705=CARTESIAN_POINT('Ctrl Pts',(111.317763761938,21.8354777499389,63.4353072421795));
#104706=CARTESIAN_POINT('Ctrl Pts',(110.361426977206,21.756833303506,64.3399119421809));
#104707=CARTESIAN_POINT('Ctrl Pts',(109.141402582769,21.6819630917717,64.0533905957354));
#104708=CARTESIAN_POINT('Ctrl Pts',(108.823853682998,21.6333076955151,63.33049705678));
#104709=CARTESIAN_POINT('Ctrl Pts',(108.821175945217,21.6108671147362,62.9991630151766));
#104710=CARTESIAN_POINT('Ctrl Pts',(108.82122247145,22.0121328852639,62.999146143432));
#104711=CARTESIAN_POINT('Ctrl Pts',(108.820751597916,22.0082404532959,62.9416686848909));
#104712=CARTESIAN_POINT('Ctrl Pts',(108.850515147101,21.9781332058502,62.4975803603857));
#104713=CARTESIAN_POINT('Ctrl Pts',(109.414184741874,21.9218111429269,61.7419008351798));
#104714=CARTESIAN_POINT('Ctrl Pts',(110.728336261702,21.843166696494,61.8186789957575));
#104715=CARTESIAN_POINT('Ctrl Pts',(111.38717606664,21.7645222500611,62.9583365837722));
#104716=CARTESIAN_POINT('Ctrl Pts',(110.797920541717,21.6858778036281,64.1354804914431));
#104717=CARTESIAN_POINT('Ctrl Pts',(109.49074599344,21.6072333571952,64.2909890134145));
#104718=CARTESIAN_POINT('Ctrl Pts',(108.865543924084,21.5493183844071,63.5501238496472));
#104719=CARTESIAN_POINT('Ctrl Pts',(108.821166000452,21.5176182270967,63.0821234674916));
#104720=CARTESIAN_POINT('Ctrl Pts',(108.821892086737,21.5121328852639,63.0010049655641));
#104721=CARTESIAN_POINT('Origin',(110.,23.8608671147362,63.));
#104722=CARTESIAN_POINT('',(108.821164759239,22.6108671147362,63.0008628562198));
#104723=CARTESIAN_POINT('',(108.824014839234,22.5121328852639,63.0000405433321));
#104724=CARTESIAN_POINT('',(108.82225,23.8608671147362,63.));
#104725=CARTESIAN_POINT('Ctrl Pts',(108.821164759239,22.6108671147362,63.0008628562198));
#104726=CARTESIAN_POINT('Ctrl Pts',(108.823829631046,22.5883373324359,62.668245303756));
#104727=CARTESIAN_POINT('Ctrl Pts',(109.143460468695,22.539592734658,61.9440114145794));
#104728=CARTESIAN_POINT('Ctrl Pts',(110.365948167423,22.4646333214024,61.6613378858167));
#104729=CARTESIAN_POINT('Ctrl Pts',(111.319211984801,22.3859888749695,62.5691141011147));
#104730=CARTESIAN_POINT('Ctrl Pts',(111.085560662631,22.3073444285365,63.8646213422023));
#104731=CARTESIAN_POINT('Ctrl Pts',(109.875174983029,22.2286999821036,64.3821740410055));
#104732=CARTESIAN_POINT('Ctrl Pts',(108.960740012569,22.1632075441702,63.7775594016063));
#104733=CARTESIAN_POINT('Ctrl Pts',(108.823998198777,22.1239299217143,63.1940718411642));
#104734=CARTESIAN_POINT('Ctrl Pts',(108.824013754263,22.1108671147362,63.0000107313632));
#104735=CARTESIAN_POINT('Ctrl Pts',(108.824014839234,22.5121328852639,63.0000405433321));
#104736=CARTESIAN_POINT('Ctrl Pts',(108.824071774344,22.4988626794951,62.8028977921035));
#104737=CARTESIAN_POINT('Ctrl Pts',(108.963936678654,22.4593776582486,62.2162275067456));
#104738=CARTESIAN_POINT('Ctrl Pts',(109.885989617323,22.3936778215245,61.6168920710419));
#104739=CARTESIAN_POINT('Ctrl Pts',(111.092282639778,22.3150333750916,62.1438975579004));
#104740=CARTESIAN_POINT('Ctrl Pts',(111.315811278397,22.2363889286587,63.4411751874573));
#104741=CARTESIAN_POINT('Ctrl Pts',(110.355452612535,22.1577444822257,64.3415087462245));
#104742=CARTESIAN_POINT('Ctrl Pts',(109.138641455968,22.0829924677608,64.0500151858993));
#104743=CARTESIAN_POINT('Ctrl Pts',(108.823922844811,22.0344552687735,63.3287688274674));
#104744=CARTESIAN_POINT('Ctrl Pts',(108.82122247145,22.0121328852639,62.999146143432));
#104745=CARTESIAN_POINT('Origin',(110.,20.6635,63.));
#104746=CARTESIAN_POINT('',(109.768242272559,20.6635,61.5549669187969));
#104747=CARTESIAN_POINT('Ctrl Pts',(109.068873933122,20.6635,63.7239975350756));
#104748=CARTESIAN_POINT('Ctrl Pts',(109.041776223981,20.6635,63.6968600192059));
#104749=CARTESIAN_POINT('Ctrl Pts',(109.016146947533,20.6635,63.6684047525815));
#104750=CARTESIAN_POINT('Ctrl Pts',(108.992115422948,20.6635,63.6387040998972));
#104751=CARTESIAN_POINT('Ctrl Pts',(108.961661304745,20.6635,63.6010657393193));
#104752=CARTESIAN_POINT('Ctrl Pts',(108.933771170535,20.6635,63.5614286691606));
#104753=CARTESIAN_POINT('Ctrl Pts',(108.908428625451,20.6635,63.5200940182358));
#104754=CARTESIAN_POINT('Ctrl Pts',(108.899116069597,20.6635,63.5049048869096));
#104755=CARTESIAN_POINT('Ctrl Pts',(108.890147843561,20.6635,63.4894861345279));
#104756=CARTESIAN_POINT('Ctrl Pts',(108.881524308389,20.6635,63.4738514603582));
#104757=CARTESIAN_POINT('Ctrl Pts',(108.876113389274,20.6635,63.464041335436));
#104758=CARTESIAN_POINT('Ctrl Pts',(108.870840777671,20.6635,63.4541507322455));
#104759=CARTESIAN_POINT('Ctrl Pts',(108.865709654558,20.6635,63.4441901037785));
#104760=CARTESIAN_POINT('Ctrl Pts',(108.842551675354,20.6635,63.3992354180603));
#104761=CARTESIAN_POINT('Ctrl Pts',(108.822250117441,20.6635,63.3528167020419));
#104762=CARTESIAN_POINT('Ctrl Pts',(108.804784889777,20.6635,63.3052653277658));
#104763=CARTESIAN_POINT('Ctrl Pts',(108.792325591787,20.6635,63.2713432539566));
#104764=CARTESIAN_POINT('Ctrl Pts',(108.781310429759,20.6635,63.2368437412891));
#104765=CARTESIAN_POINT('Ctrl Pts',(108.771744228615,20.6635,63.2018765378799));
#104766=CARTESIAN_POINT('Ctrl Pts',(108.768234596496,20.6635,63.1890478278897));
#104767=CARTESIAN_POINT('Ctrl Pts',(108.76492009768,20.6635,63.1761560983945));
#104768=CARTESIAN_POINT('Ctrl Pts',(108.761801339773,20.6635,63.1632065587171));
#104769=CARTESIAN_POINT('Ctrl Pts',(108.759408740941,20.6635,63.1532721378926));
#104770=CARTESIAN_POINT('Ctrl Pts',(108.757133691864,20.6635,63.1433134201745));
#104771=CARTESIAN_POINT('Ctrl Pts',(108.754975905346,20.6635,63.1333330868544));
#104772=CARTESIAN_POINT('Ctrl Pts',(108.743883262358,20.6635,63.0820266793297));
#104773=CARTESIAN_POINT('Ctrl Pts',(108.735886220507,20.6635,63.030151426245));
#104774=CARTESIAN_POINT('Ctrl Pts',(108.730968273879,20.6635,62.9780444433024));
#104775=CARTESIAN_POINT('Ctrl Pts',(108.725962577061,20.6635,62.9250077232215));
#104776=CARTESIAN_POINT('Ctrl Pts',(108.724146366546,20.6635,62.8717298546305));
#104777=CARTESIAN_POINT('Ctrl Pts',(108.725548337084,20.6635,62.8185401910312));
#104778=CARTESIAN_POINT('Ctrl Pts',(108.726365137912,20.6635,62.7875514076506));
#104779=CARTESIAN_POINT('Ctrl Pts',(108.728275190858,20.6635,62.7565921586689));
#104780=CARTESIAN_POINT('Ctrl Pts',(108.731292161217,20.6635,62.7257258953858));
#104781=CARTESIAN_POINT('Ctrl Pts',(108.732846162307,20.6635,62.7098270958947));
#104782=CARTESIAN_POINT('Ctrl Pts',(108.734693943388,20.6635,62.693952958583));
#104783=CARTESIAN_POINT('Ctrl Pts',(108.736838021663,20.6635,62.6781121640002));
#104784=CARTESIAN_POINT('Ctrl Pts',(108.738124124167,20.6635,62.6686102321863));
#104785=CARTESIAN_POINT('Ctrl Pts',(108.739516716316,20.6635,62.6591219348981));
#104786=CARTESIAN_POINT('Ctrl Pts',(108.741014126988,20.6635,62.6496611766502));
#104787=CARTESIAN_POINT('Ctrl Pts',(108.749581424227,20.6635,62.5955323197334));
#104788=CARTESIAN_POINT('Ctrl Pts',(108.761589938658,20.6635,62.5421986312183));
#104789=CARTESIAN_POINT('Ctrl Pts',(108.777050275135,20.6635,62.4900067495456));
#104790=CARTESIAN_POINT('Ctrl Pts',(108.780620366447,20.6635,62.4779546325946));
#104791=CARTESIAN_POINT('Ctrl Pts',(108.784374733632,20.6635,62.46596334393));
#104792=CARTESIAN_POINT('Ctrl Pts',(108.788313895805,20.6635,62.4540370771723));
#104793=CARTESIAN_POINT('Ctrl Pts',(108.804806146037,20.6635,62.4041048918261));
#104794=CARTESIAN_POINT('Ctrl Pts',(108.824533476475,20.6635,62.3553118205143));
#104795=CARTESIAN_POINT('Ctrl Pts',(108.847241455824,20.6635,62.3078108423137));
#104796=CARTESIAN_POINT('Ctrl Pts',(108.858185154999,20.6635,62.2849186065964));
#104797=CARTESIAN_POINT('Ctrl Pts',(108.869821912433,20.6635,62.2623265854079));
#104798=CARTESIAN_POINT('Ctrl Pts',(108.882127306327,20.6635,62.2400529186177));
#104799=CARTESIAN_POINT('Ctrl Pts',(108.889977865108,20.6635,62.2258428305948));
#104800=CARTESIAN_POINT('Ctrl Pts',(108.898100619865,20.6635,62.2117623333824));
#104801=CARTESIAN_POINT('Ctrl Pts',(108.906489735732,20.6635,62.1978163501422));
#104802=CARTESIAN_POINT('Ctrl Pts',(108.911474485511,20.6635,62.1895297514128));
#104803=CARTESIAN_POINT('Ctrl Pts',(108.91655258614,20.6635,62.1812919793157));
#104804=CARTESIAN_POINT('Ctrl Pts',(108.921716096233,20.6635,62.1731141652028));
#104805=CARTESIAN_POINT('Ctrl Pts',(108.950996938535,20.6635,62.1267400357672));
#104806=CARTESIAN_POINT('Ctrl Pts',(108.98307363302,20.6635,62.0822030694366));
#104807=CARTESIAN_POINT('Ctrl Pts',(109.017648867747,20.6635,62.0396614569002));
#104808=CARTESIAN_POINT('Ctrl Pts',(109.052976298894,20.6635,61.9961943365865));
#104809=CARTESIAN_POINT('Ctrl Pts',(109.090912650005,20.6635,61.9548094783859));
#104810=CARTESIAN_POINT('Ctrl Pts',(109.131193500982,20.6635,61.915691025615));
#104811=CARTESIAN_POINT('Ctrl Pts',(109.153761696009,20.6635,61.8937740886615));
#104812=CARTESIAN_POINT('Ctrl Pts',(109.177066737589,20.6635,61.8725689315292));
#104813=CARTESIAN_POINT('Ctrl Pts',(109.20106819572,20.6635,61.8521115596512));
#104814=CARTESIAN_POINT('Ctrl Pts',(109.21741187414,20.6635,61.838181209859));
#104815=CARTESIAN_POINT('Ctrl Pts',(109.234078558871,20.6635,61.8245976553156));
#104816=CARTESIAN_POINT('Ctrl Pts',(109.251056464039,20.6635,61.811373170307));
#104817=CARTESIAN_POINT('Ctrl Pts',(109.262906518497,20.6635,61.8021428874198));
#104818=CARTESIAN_POINT('Ctrl Pts',(109.274913506492,20.6635,61.7930838780324));
#104819=CARTESIAN_POINT('Ctrl Pts',(109.287044553329,20.6635,61.7842211755186));
#104820=CARTESIAN_POINT('Ctrl Pts',(109.334074367695,20.6635,61.7498621247611));
#104821=CARTESIAN_POINT('Ctrl Pts',(109.383026217507,20.6635,61.7184001999552));
#104822=CARTESIAN_POINT('Ctrl Pts',(109.433611071353,20.6635,61.6900214570481));
#104823=CARTESIAN_POINT('Ctrl Pts',(109.486215208434,20.6635,61.6605098707017));
#104824=CARTESIAN_POINT('Ctrl Pts',(109.540585931337,20.6635,61.6343312922889));
#104825=CARTESIAN_POINT('Ctrl Pts',(109.59644465953,20.6635,61.6117317920506));
#104826=CARTESIAN_POINT('Ctrl Pts',(109.648871874635,20.6635,61.5905206241888));
#104827=CARTESIAN_POINT('Ctrl Pts',(109.702610962679,20.6635,61.5724618781725));
#104828=CARTESIAN_POINT('Ctrl Pts',(109.757458309662,20.6635,61.5578017530401));
#104829=CARTESIAN_POINT('Ctrl Pts',(109.761048227392,20.6635,61.5568422053859));
#104830=CARTESIAN_POINT('Ctrl Pts',(109.764642899831,20.6635,61.5558972351112));
#104831=CARTESIAN_POINT('Ctrl Pts',(109.768242272559,20.6635,61.5549669187969));
#104832=CARTESIAN_POINT('',(108.5365,20.6635,63.));
#104833=CARTESIAN_POINT('Origin',(110.,20.6635,63.));
#104834=CARTESIAN_POINT('',(110.984655829999,20.6635,61.9158283453366));
#104835=CARTESIAN_POINT('Origin',(110.,20.6635,63.));
#104836=CARTESIAN_POINT('Ctrl Pts',(110.985650158356,20.6635,61.9152813028828));
#104837=CARTESIAN_POINT('Ctrl Pts',(111.01753748414,20.6635,61.9498143114107));
#104838=CARTESIAN_POINT('Ctrl Pts',(111.047590571521,20.6635,61.985887892205));
#104839=CARTESIAN_POINT('Ctrl Pts',(111.07563943333,20.6635,62.0234571627525));
#104840=CARTESIAN_POINT('Ctrl Pts',(111.109740975853,20.6635,62.069133528726));
#104841=CARTESIAN_POINT('Ctrl Pts',(111.140881244931,20.6635,62.117021111467));
#104842=CARTESIAN_POINT('Ctrl Pts',(111.169005155357,20.6635,62.1667916134042));
#104843=CARTESIAN_POINT('Ctrl Pts',(111.180163381995,20.6635,62.1865381753901));
#104844=CARTESIAN_POINT('Ctrl Pts',(111.190846276038,20.6635,62.2065812716683));
#104845=CARTESIAN_POINT('Ctrl Pts',(111.201048327816,20.6635,62.2269007098618));
#104846=CARTESIAN_POINT('Ctrl Pts',(111.206203924178,20.6635,62.2371691170324));
#104847=CARTESIAN_POINT('Ctrl Pts',(111.211235029523,20.6635,62.2475049057826));
#104848=CARTESIAN_POINT('Ctrl Pts',(111.216137759321,20.6635,62.2578978974652));
#104849=CARTESIAN_POINT('Ctrl Pts',(111.240666969565,20.6635,62.309895843215));
#104850=CARTESIAN_POINT('Ctrl Pts',(111.262014626778,20.6635,62.3633797304262));
#104851=CARTESIAN_POINT('Ctrl Pts',(111.280130648338,20.6635,62.4180079217357));
#104852=CARTESIAN_POINT('Ctrl Pts',(111.292319973414,20.6635,62.4547643795463));
#104853=CARTESIAN_POINT('Ctrl Pts',(111.303045197808,20.6635,62.4920392539845));
#104854=CARTESIAN_POINT('Ctrl Pts',(111.312277796759,20.6635,62.5297289224477));
#104855=CARTESIAN_POINT('Ctrl Pts',(111.316855469064,20.6635,62.5484160713672));
#104856=CARTESIAN_POINT('Ctrl Pts',(111.321066037847,20.6635,62.5672051745102));
#104857=CARTESIAN_POINT('Ctrl Pts',(111.324905042817,20.6635,62.5860834048704));
#104858=CARTESIAN_POINT('Ctrl Pts',(111.327193300271,20.6635,62.5973358652554));
#104859=CARTESIAN_POINT('Ctrl Pts',(111.329348014919,20.6635,62.6086127768341));
#104860=CARTESIAN_POINT('Ctrl Pts',(111.331367617159,20.6635,62.6199046362027));
#104861=CARTESIAN_POINT('Ctrl Pts',(111.341260805276,20.6635,62.6752187404727));
#104862=CARTESIAN_POINT('Ctrl Pts',(111.347926440227,20.6635,62.7309425734807));
#104863=CARTESIAN_POINT('Ctrl Pts',(111.351312093896,20.6635,62.7867588839852));
#104864=CARTESIAN_POINT('Ctrl Pts',(111.35461246061,20.6635,62.841169143064));
#104865=CARTESIAN_POINT('Ctrl Pts',(111.354795821637,20.6635,62.8956683041584));
#104866=CARTESIAN_POINT('Ctrl Pts',(111.351765888959,20.6635,62.9499533707069));
#104867=CARTESIAN_POINT('Ctrl Pts',(111.349967907017,20.6635,62.9821664855527));
#104868=CARTESIAN_POINT('Ctrl Pts',(111.347037527234,20.6635,63.0143039622647));
#104869=CARTESIAN_POINT('Ctrl Pts',(111.342946754139,20.6635,63.0462987518364));
#104870=CARTESIAN_POINT('Ctrl Pts',(111.340744516677,20.6635,63.0635229103341));
#104871=CARTESIAN_POINT('Ctrl Pts',(111.338205881635,20.6635,63.08070565807));
#104872=CARTESIAN_POINT('Ctrl Pts',(111.335325774837,20.6635,63.0978360597344));
#104873=CARTESIAN_POINT('Ctrl Pts',(111.33322107784,20.6635,63.1103544514009));
#104874=CARTESIAN_POINT('Ctrl Pts',(111.330933144632,20.6635,63.122848499884));
#104875=CARTESIAN_POINT('Ctrl Pts',(111.328465426181,20.6635,63.1352879085258));
#104876=CARTESIAN_POINT('Ctrl Pts',(111.318197868588,20.6635,63.1870451682013));
#104877=CARTESIAN_POINT('Ctrl Pts',(111.304808954063,20.6635,63.2379451290125));
#104878=CARTESIAN_POINT('Ctrl Pts',(111.288220844963,20.6635,63.287708390006));
#104879=CARTESIAN_POINT('Ctrl Pts',(111.283849056323,20.6635,63.3008234749018));
#104880=CARTESIAN_POINT('Ctrl Pts',(111.27925480147,20.6635,63.3138594947431));
#104881=CARTESIAN_POINT('Ctrl Pts',(111.274436108329,20.6635,63.3268110592629));
#104882=CARTESIAN_POINT('Ctrl Pts',(111.256199056831,20.6635,63.3758281562749));
#104883=CARTESIAN_POINT('Ctrl Pts',(111.234749877029,20.6635,63.4236380914674));
#104884=CARTESIAN_POINT('Ctrl Pts',(111.210305646014,20.6635,63.4700291885761));
#104885=CARTESIAN_POINT('Ctrl Pts',(111.198884231714,20.6635,63.4917051390112));
#104886=CARTESIAN_POINT('Ctrl Pts',(111.186808460553,20.6635,63.5130708662858));
#104887=CARTESIAN_POINT('Ctrl Pts',(111.174098316205,20.6635,63.534102023797));
#104888=CARTESIAN_POINT('Ctrl Pts',(111.165070142502,20.6635,63.5490407166999));
#104889=CARTESIAN_POINT('Ctrl Pts',(111.155721872651,20.6635,63.5638105668429));
#104890=CARTESIAN_POINT('Ctrl Pts',(111.146060360571,20.6635,63.5784022275922));
#104891=CARTESIAN_POINT('Ctrl Pts',(111.140434667663,20.6635,63.586898641168));
#104892=CARTESIAN_POINT('Ctrl Pts',(111.134707479,20.6635,63.5953274435488));
#104893=CARTESIAN_POINT('Ctrl Pts',(111.128883474863,20.6635,63.6036831587769));
#104894=CARTESIAN_POINT('Ctrl Pts',(111.098850688879,20.6635,63.6467712818803));
#104895=CARTESIAN_POINT('Ctrl Pts',(111.066222949058,20.6635,63.6879543999203));
#104896=CARTESIAN_POINT('Ctrl Pts',(111.031239521506,20.6635,63.7270332019964));
#104897=CARTESIAN_POINT('Ctrl Pts',(110.996431658519,20.6635,63.765915886844));
#104898=CARTESIAN_POINT('Ctrl Pts',(110.959290675624,20.6635,63.8027159560329));
#104899=CARTESIAN_POINT('Ctrl Pts',(110.920024086437,20.6635,63.8371945338622));
#104900=CARTESIAN_POINT('Ctrl Pts',(110.900351992054,20.6635,63.8544678914741));
#104901=CARTESIAN_POINT('Ctrl Pts',(110.880146046364,20.6635,63.8711578526716));
#104902=CARTESIAN_POINT('Ctrl Pts',(110.859430862329,20.6635,63.8872295854972));
#104903=CARTESIAN_POINT('Ctrl Pts',(110.844179452001,20.6635,63.8990622871329));
#104904=CARTESIAN_POINT('Ctrl Pts',(110.82865198741,20.6635,63.910559808957));
#104905=CARTESIAN_POINT('Ctrl Pts',(110.812858139265,20.6635,63.9217070126001));
#104906=CARTESIAN_POINT('Ctrl Pts',(110.805217406484,20.6635,63.9270997961395));
#104907=CARTESIAN_POINT('Ctrl Pts',(110.797515069741,20.6635,63.9324099343249));
#104908=CARTESIAN_POINT('Ctrl Pts',(110.789763069932,20.6635,63.9376287369471));
#104909=CARTESIAN_POINT('Ctrl Pts',(110.747931937301,20.6635,63.965790299129));
#104910=CARTESIAN_POINT('Ctrl Pts',(110.704574423533,20.6635,63.9913545250727));
#104911=CARTESIAN_POINT('Ctrl Pts',(110.659887444905,20.6635,64.0141163397133));
#104912=CARTESIAN_POINT('Ctrl Pts',(110.616084819746,20.6635,64.0364276989777));
#104913=CARTESIAN_POINT('Ctrl Pts',(110.571003947828,20.6635,64.056046817182));
#104914=CARTESIAN_POINT('Ctrl Pts',(110.524819939819,20.6635,64.0727319238977));
#104915=CARTESIAN_POINT('Ctrl Pts',(110.478635931809,20.6635,64.0894170306134));
#104916=CARTESIAN_POINT('Ctrl Pts',(110.431347991186,20.6635,64.1031686027959));
#104917=CARTESIAN_POINT('Ctrl Pts',(110.383133178262,20.6635,64.1136893777958));
#104918=CARTESIAN_POINT('Ctrl Pts',(109.489783494612,23.1014778394209,64.0614961988294));
#104919=CARTESIAN_POINT('Ctrl Pts',(109.14010001709,23.0752630239433,63.8934180822146));
#104920=CARTESIAN_POINT('Ctrl Pts',(108.625794473154,23.022833392988,63.1868568140592));
#104921=CARTESIAN_POINT('Ctrl Pts',(109.087620120174,22.9441889465551,61.9533607581798));
#104922=CARTESIAN_POINT('Ctrl Pts',(110.372106003814,22.8655445001221,61.6631757288605));
#104923=CARTESIAN_POINT('Ctrl Pts',(111.321028562455,22.7869000536892,62.5749012318044));
#104924=CARTESIAN_POINT('Ctrl Pts',(111.081739672219,22.7082556072563,63.8694937849383));
#104925=CARTESIAN_POINT('Ctrl Pts',(109.868997477121,22.6296111608234,64.381583208474));
#104926=CARTESIAN_POINT('Ctrl Pts',(108.774203642059,22.5509667143904,63.6506963709226));
#104927=CARTESIAN_POINT('Ctrl Pts',(108.782267803706,22.4723222679575,62.3343124775264));
#104928=CARTESIAN_POINT('Ctrl Pts',(109.885989617323,22.3936778215245,61.6168920710419));
#104929=CARTESIAN_POINT('Ctrl Pts',(111.092282639778,22.3150333750916,62.1438975579004));
#104930=CARTESIAN_POINT('Ctrl Pts',(111.315811278397,22.2363889286587,63.4411751874573));
#104931=CARTESIAN_POINT('Ctrl Pts',(110.355452612535,22.1577444822257,64.3415087462245));
#104932=CARTESIAN_POINT('Ctrl Pts',(109.07528055956,22.0791000357928,64.0348367474211));
#104933=CARTESIAN_POINT('Ctrl Pts',(108.627113371416,22.0004555893599,62.7970823192364));
#104934=CARTESIAN_POINT('Ctrl Pts',(109.414184741874,21.9218111429269,61.7419008351798));
#104935=CARTESIAN_POINT('Ctrl Pts',(110.728336261702,21.843166696494,61.8186789957575));
#104936=CARTESIAN_POINT('Ctrl Pts',(111.38717606664,21.7645222500611,62.9583365837722));
#104937=CARTESIAN_POINT('Ctrl Pts',(110.797920541717,21.6858778036281,64.1354804914431));
#104938=CARTESIAN_POINT('Ctrl Pts',(109.49074599344,21.6072333571952,64.2909890134145));
#104939=CARTESIAN_POINT('Ctrl Pts',(108.641765698946,21.5285889107623,63.2849463981635));
#104940=CARTESIAN_POINT('Ctrl Pts',(109.014842533325,21.4499444643293,62.0225249249297));
#104941=CARTESIAN_POINT('Ctrl Pts',(110.274298694314,21.3713000178964,61.6395786914333));
#104942=CARTESIAN_POINT('Ctrl Pts',(111.286967138036,21.2926555714635,62.4806473596071));
#104943=CARTESIAN_POINT('Ctrl Pts',(111.141682515009,21.2140111250305,63.7890142667887));
#104944=CARTESIAN_POINT('Ctrl Pts',(109.969224812209,21.1353666785976,64.3874389034312));
#104945=CARTESIAN_POINT('Ctrl Pts',(108.82436675964,21.0567222321647,63.7376087341273));
#104946=CARTESIAN_POINT('Ctrl Pts',(108.737462181258,20.9780777857317,62.4239586110443));
#104947=CARTESIAN_POINT('Ctrl Pts',(109.786099850077,20.8994333392988,61.6289388285546));
#104948=CARTESIAN_POINT('Ctrl Pts',(111.02805441837,20.8207888928659,62.0667289458579));
#104949=CARTESIAN_POINT('Ctrl Pts',(111.343096451131,20.7421444464329,63.3456128208481));
#104950=CARTESIAN_POINT('Ctrl Pts',(110.750010398298,20.6897148154776,63.9874756972607));
#104951=CARTESIAN_POINT('Ctrl Pts',(110.383133178262,20.6635,64.1136893777958));
#104952=CARTESIAN_POINT('Ctrl Pts',(109.448519964883,23.0464852262806,64.1473442250985));
#104953=CARTESIAN_POINT('Ctrl Pts',(109.070555993849,23.020270410803,63.9656728666179));
#104954=CARTESIAN_POINT('Ctrl Pts',(108.514656221036,22.9678407798477,63.2019687746104));
#104955=CARTESIAN_POINT('Ctrl Pts',(109.013831808942,22.8891963334148,61.8687142816071));
#104956=CARTESIAN_POINT('Ctrl Pts',(110.402199909026,22.8105518869818,61.5550606689361));
#104957=CARTESIAN_POINT('Ctrl Pts',(111.427866151565,22.7319074405489,62.5405215606768));
#104958=CARTESIAN_POINT('Ctrl Pts',(111.169224880268,22.653262994116,63.939813702591));
#104959=CARTESIAN_POINT('Ctrl Pts',(109.858402707175,22.574618547683,64.4933181272659));
#104960=CARTESIAN_POINT('Ctrl Pts',(108.675067914533,22.4959741012501,63.7033211464101));
#104961=CARTESIAN_POINT('Ctrl Pts',(108.683784261615,22.4173296548172,62.2804752994193));
#104962=CARTESIAN_POINT('Ctrl Pts',(109.876769079051,22.3386852083842,61.5050338411687));
#104963=CARTESIAN_POINT('Ctrl Pts',(111.180620505572,22.2600407619513,62.0746606590593));
#104964=CARTESIAN_POINT('Ctrl Pts',(111.422226922012,22.1813963155184,63.4768550317411));
#104965=CARTESIAN_POINT('Ctrl Pts',(110.384199682239,22.1027518690854,64.4500026609583));
#104966=CARTESIAN_POINT('Ctrl Pts',(109.000494291929,22.0241074226525,64.118528702583));
#104967=CARTESIAN_POINT('Ctrl Pts',(108.5160817846,21.9454629762195,62.7806714433351));
#104968=CARTESIAN_POINT('Ctrl Pts',(109.366807197118,21.8668185297866,61.6401526327182));
#104969=CARTESIAN_POINT('Ctrl Pts',(110.787240128335,21.7881740833537,61.7231401924002));
#104970=CARTESIAN_POINT('Ctrl Pts',(111.499363305313,21.7095296369208,62.954967073778));
#104971=CARTESIAN_POINT('Ctrl Pts',(110.862452005608,21.6308851904878,64.2273119640051));
#104972=CARTESIAN_POINT('Ctrl Pts',(109.449560305369,21.5522407440549,64.3953971675455));
#104973=CARTESIAN_POINT('Ctrl Pts',(108.53191911251,21.4735962976219,63.3079913095836));
#104974=CARTESIAN_POINT('Ctrl Pts',(108.935168367584,21.394951851189,61.943472069145));
#104975=CARTESIAN_POINT('Ctrl Pts',(110.296482477488,21.3163074047561,61.5295552317508));
#104976=CARTESIAN_POINT('Ctrl Pts',(111.39105002481,21.2376629583231,62.4386449490808));
#104977=CARTESIAN_POINT('Ctrl Pts',(111.234015573429,21.1590185118902,63.8528254397129));
#104978=CARTESIAN_POINT('Ctrl Pts',(109.966735882778,21.0803740654573,64.4996473989114));
#104979=CARTESIAN_POINT('Ctrl Pts',(108.729287951621,21.0017296190243,63.7972625077853));
#104980=CARTESIAN_POINT('Ctrl Pts',(108.635355004663,20.9230851725914,62.3773715235486));
#104981=CARTESIAN_POINT('Ctrl Pts',(109.768800771936,20.8444407261585,61.5180548747612));
#104982=CARTESIAN_POINT('Ctrl Pts',(111.111197855729,20.7657962797256,61.9912510703265));
#104983=CARTESIAN_POINT('Ctrl Pts',(111.451718770783,20.6871518332926,63.3735641018379));
#104984=CARTESIAN_POINT('Ctrl Pts',(110.810667150952,20.6347222023373,64.067337348854));
#104985=CARTESIAN_POINT('Ctrl Pts',(110.414118901233,20.6085073868597,64.203758503871));
#104986=CARTESIAN_POINT('Ctrl Pts',(109.407256435154,22.9914926131403,64.2331922513677));
#104987=CARTESIAN_POINT('Ctrl Pts',(109.001011970608,22.9652777976627,64.0379276510211));
#104988=CARTESIAN_POINT('Ctrl Pts',(108.403517968918,22.9128481667074,63.2170807351616));
#104989=CARTESIAN_POINT('Ctrl Pts',(108.94004349771,22.8342037202745,61.7840678050346));
#104990=CARTESIAN_POINT('Ctrl Pts',(110.432293814238,22.7555592738415,61.4469456090116));
#104991=CARTESIAN_POINT('Ctrl Pts',(111.534703740675,22.6769148274086,62.5061418895491));
#104992=CARTESIAN_POINT('Ctrl Pts',(111.256710088316,22.5982703809757,64.0101336202436));
#104993=CARTESIAN_POINT('Ctrl Pts',(109.847807937229,22.5196259345427,64.6050530460577));
#104994=CARTESIAN_POINT('Ctrl Pts',(108.575932187007,22.4409814881098,63.7559459218976));
#104995=CARTESIAN_POINT('Ctrl Pts',(108.585300719525,22.3623370416768,62.2266381213122));
#104996=CARTESIAN_POINT('Ctrl Pts',(109.867548540779,22.2836925952439,61.3931756112954));
#104997=CARTESIAN_POINT('Ctrl Pts',(111.268958371366,22.205048148811,62.0054237602183));
#104998=CARTESIAN_POINT('Ctrl Pts',(111.528642565627,22.1264037023781,63.512534876025));
#104999=CARTESIAN_POINT('Ctrl Pts',(110.412946751943,22.0477592559451,64.5584965756923));
#105000=CARTESIAN_POINT('Ctrl Pts',(108.925708024299,21.9691148095122,64.2022206577448));
#105001=CARTESIAN_POINT('Ctrl Pts',(108.405050197784,21.8904703630793,62.7642605674339));
#105002=CARTESIAN_POINT('Ctrl Pts',(109.319429652362,21.8118259166463,61.5384044302566));
#105003=CARTESIAN_POINT('Ctrl Pts',(110.846143994968,21.7331814702134,61.6276013890428));
#105004=CARTESIAN_POINT('Ctrl Pts',(111.611550543987,21.6545370237804,62.9515975637838));
#105005=CARTESIAN_POINT('Ctrl Pts',(110.9269834695,21.5758925773475,64.3191434365672));
#105006=CARTESIAN_POINT('Ctrl Pts',(109.408374617299,21.4972481309146,64.4998053216764));
#105007=CARTESIAN_POINT('Ctrl Pts',(108.422072526074,21.4186036844816,63.3310362210038));
#105008=CARTESIAN_POINT('Ctrl Pts',(108.855494201844,21.3399592380487,61.8644192133603));
#105009=CARTESIAN_POINT('Ctrl Pts',(110.318666260662,21.2613147916158,61.4195317720684));
#105010=CARTESIAN_POINT('Ctrl Pts',(111.495132911584,21.1826703451828,62.3966425385543));
#105011=CARTESIAN_POINT('Ctrl Pts',(111.32634863185,21.1040258987499,63.9166366126373));
#105012=CARTESIAN_POINT('Ctrl Pts',(109.964246953347,21.025381452317,64.6118558943916));
#105013=CARTESIAN_POINT('Ctrl Pts',(108.634209143603,20.946737005884,63.8569162814432));
#105014=CARTESIAN_POINT('Ctrl Pts',(108.533247828067,20.8680925594511,62.3307844360529));
#105015=CARTESIAN_POINT('Ctrl Pts',(109.751501693796,20.7894481130182,61.4071709209678));
#105016=CARTESIAN_POINT('Ctrl Pts',(111.194341293088,20.7108036665852,61.9157731947952));
#105017=CARTESIAN_POINT('Ctrl Pts',(111.560341090435,20.6321592201523,63.4015153828277));
#105018=CARTESIAN_POINT('Ctrl Pts',(110.871323903606,20.579729589197,64.1471990004474));
#105019=CARTESIAN_POINT('Ctrl Pts',(110.445104624204,20.5535147737194,64.2938276299462));
#105020=CARTESIAN_POINT('Ctrl Pts',(109.365992905425,22.9365,64.3190402776368));
#105021=CARTESIAN_POINT('Ctrl Pts',(108.931467947367,22.9102851845224,64.1101824354244));
#105022=CARTESIAN_POINT('Ctrl Pts',(108.2923797168,22.8578555535671,63.2321926957128));
#105023=CARTESIAN_POINT('Ctrl Pts',(108.866255186478,22.7792111071341,61.699421328462));
#105024=CARTESIAN_POINT('Ctrl Pts',(110.46238771945,22.7005666607012,61.3388305490871));
#105025=CARTESIAN_POINT('Ctrl Pts',(111.641541329784,22.6219222142683,62.4717622184214));
#105026=CARTESIAN_POINT('Ctrl Pts',(111.344195296364,22.5432777678353,64.0804535378962));
#105027=CARTESIAN_POINT('Ctrl Pts',(109.837213167282,22.4646333214024,64.7167879648497));
#105028=CARTESIAN_POINT('Ctrl Pts',(108.476796459481,22.3859888749695,63.808570697385));
#105029=CARTESIAN_POINT('Ctrl Pts',(108.486817177434,22.3073444285366,62.1728009432052));
#105030=CARTESIAN_POINT('Ctrl Pts',(109.858328002507,22.2286999821036,61.2813173814221));
#105031=CARTESIAN_POINT('Ctrl Pts',(111.35729623716,22.1500555356707,61.9361868613773));
#105032=CARTESIAN_POINT('Ctrl Pts',(111.635058209242,22.0714110892377,63.5482147203088));
#105033=CARTESIAN_POINT('Ctrl Pts',(110.441693821647,21.9927666428048,64.6669904904262));
#105034=CARTESIAN_POINT('Ctrl Pts',(108.850921756668,21.9141221963719,64.2859126129067));
#105035=CARTESIAN_POINT('Ctrl Pts',(108.294018610968,21.8354777499389,62.7478496915326));
#105036=CARTESIAN_POINT('Ctrl Pts',(109.272052107606,21.756833303506,61.4366562277951));
#105037=CARTESIAN_POINT('Ctrl Pts',(110.905047861601,21.6781888570731,61.5320625856855));
#105038=CARTESIAN_POINT('Ctrl Pts',(111.72373778266,21.5995444106401,62.9482280537896));
#105039=CARTESIAN_POINT('Ctrl Pts',(110.991514933392,21.5208999642072,64.4109749091292));
#105040=CARTESIAN_POINT('Ctrl Pts',(109.367188929228,21.4422555177743,64.6042134758074));
#105041=CARTESIAN_POINT('Ctrl Pts',(108.312225939637,21.3636110713413,63.3540811324239));
#105042=CARTESIAN_POINT('Ctrl Pts',(108.775820036103,21.2849666249084,61.7853663575755));
#105043=CARTESIAN_POINT('Ctrl Pts',(110.340850043836,21.2063221784755,61.309508312386));
#105044=CARTESIAN_POINT('Ctrl Pts',(111.599215798358,21.1276777320425,62.354640128028));
#105045=CARTESIAN_POINT('Ctrl Pts',(111.41868169027,21.0490332856096,63.9804477855616));
#105046=CARTESIAN_POINT('Ctrl Pts',(109.961758023917,20.9703888391767,64.7240643898718));
#105047=CARTESIAN_POINT('Ctrl Pts',(108.539130335584,20.8917443927437,63.9165700551012));
#105048=CARTESIAN_POINT('Ctrl Pts',(108.431140651472,20.8130999463108,62.2841973485573));
#105049=CARTESIAN_POINT('Ctrl Pts',(109.734202615655,20.7344554998779,61.2962869671744));
#105050=CARTESIAN_POINT('Ctrl Pts',(111.277484730447,20.6558110534449,61.8402953192639));
#105051=CARTESIAN_POINT('Ctrl Pts',(111.668963410087,20.577166607012,63.4294666638175));
#105052=CARTESIAN_POINT('Ctrl Pts',(110.93198065626,20.5247369760567,64.2270606520407));
#105053=CARTESIAN_POINT('Ctrl Pts',(110.476090347175,20.4985221605791,64.3838967560213));
#105054=CARTESIAN_POINT('Ctrl Pts',(108.538556703894,20.8471550458429,62.999470885696));
#105055=CARTESIAN_POINT('Ctrl Pts',(108.537914852139,20.8358033459989,62.789965438622));
#105056=CARTESIAN_POINT('Ctrl Pts',(108.580066340676,20.8244516461548,62.5807162394158));
#105057=CARTESIAN_POINT('Ctrl Pts',(108.666315926188,20.8130999463108,62.3916077360841));
#105058=CARTESIAN_POINT('Ctrl Pts',(108.865494639533,20.7868851308332,61.9548938880963));
#105059=CARTESIAN_POINT('Ctrl Pts',(109.299848627594,20.7606703153555,61.6255904276354));
#105060=CARTESIAN_POINT('Ctrl Pts',(109.774239307423,20.7344554998779,61.5516067560865));
#105061=CARTESIAN_POINT('Ctrl Pts',(110.202249540204,20.7108036665852,61.4848563543015));
#105062=CARTESIAN_POINT('Ctrl Pts',(110.662850510825,20.6871518332926,61.6259418135298));
#105063=CARTESIAN_POINT('Ctrl Pts',(110.985650158356,20.6635,61.9152813028828));
#105064=CARTESIAN_POINT('',(109.315335575461,22.9365,62.0417048010816));
#105065=CARTESIAN_POINT('Ctrl Pts',(109.313848625014,22.9365,62.0406439634947));
#105066=CARTESIAN_POINT('Ctrl Pts',(109.280140163402,22.9365,62.0589325036321));
#105067=CARTESIAN_POINT('Ctrl Pts',(109.247463641323,22.9365,62.0789026699033));
#105068=CARTESIAN_POINT('Ctrl Pts',(109.215963639247,22.9365,62.1005219579104));
#105069=CARTESIAN_POINT('Ctrl Pts',(109.17604504973,22.9365,62.1279191460608));
#105070=CARTESIAN_POINT('Ctrl Pts',(109.138014421603,22.9365,62.1579629277155));
#105071=CARTESIAN_POINT('Ctrl Pts',(109.10194186794,22.9365,62.1903599905654));
#105072=CARTESIAN_POINT('Ctrl Pts',(109.088686393136,22.9365,62.202264843611));
#105073=CARTESIAN_POINT('Ctrl Pts',(109.07569551895,22.9365,62.214487933832));
#105074=CARTESIAN_POINT('Ctrl Pts',(109.062973496017,22.9365,62.2270162330653));
#105075=CARTESIAN_POINT('Ctrl Pts',(109.054990947041,22.9365,62.2348772283445));
#105076=CARTESIAN_POINT('Ctrl Pts',(109.047118030534,22.9365,62.2428547839097));
#105077=CARTESIAN_POINT('Ctrl Pts',(109.039360774909,22.9365,62.2509397869167));
#105078=CARTESIAN_POINT('Ctrl Pts',(109.004350387927,22.9365,62.2874293777846));
#105079=CARTESIAN_POINT('Ctrl Pts',(108.971660664562,22.9365,62.3261364097773));
#105080=CARTESIAN_POINT('Ctrl Pts',(108.941366794955,22.9365,62.3667375281165));
#105081=CARTESIAN_POINT('Ctrl Pts',(108.919755827294,22.9365,62.3957014560267));
#105082=CARTESIAN_POINT('Ctrl Pts',(108.899364514413,22.9365,62.4256304788392));
#105083=CARTESIAN_POINT('Ctrl Pts',(108.88022876161,22.9365,62.456420775291));
#105084=CARTESIAN_POINT('Ctrl Pts',(108.873208322306,22.9365,62.4677169813831));
#105085=CARTESIAN_POINT('Ctrl Pts',(108.866356958192,22.9365,62.4791292080189));
#105086=CARTESIAN_POINT('Ctrl Pts',(108.859676736391,22.9365,62.4906526352152));
#105087=CARTESIAN_POINT('Ctrl Pts',(108.854551817076,22.9365,62.4994931552399));
#105088=CARTESIAN_POINT('Ctrl Pts',(108.84953264866,22.9365,62.5083904700141));
#105089=CARTESIAN_POINT('Ctrl Pts',(108.844619720526,22.9365,62.5173419267744));
#105090=CARTESIAN_POINT('Ctrl Pts',(108.819363853716,22.9365,62.5633586389046));
#105091=CARTESIAN_POINT('Ctrl Pts',(108.796913055783,22.9365,62.6108029064586));
#105092=CARTESIAN_POINT('Ctrl Pts',(108.777347590366,22.9365,62.6593468910022));
#105093=CARTESIAN_POINT('Ctrl Pts',(108.757433018356,22.9365,62.7087570458501));
#105094=CARTESIAN_POINT('Ctrl Pts',(108.740506907496,22.9365,62.7593074094981));
#105095=CARTESIAN_POINT('Ctrl Pts',(108.726690634926,22.9365,62.8106904666182));
#105096=CARTESIAN_POINT('Ctrl Pts',(108.718641146458,22.9365,62.8406267119867));
#105097=CARTESIAN_POINT('Ctrl Pts',(108.711647982872,22.9365,62.8708462447828));
#105098=CARTESIAN_POINT('Ctrl Pts',(108.70574232762,22.9365,62.9012921401079));
#105099=CARTESIAN_POINT('Ctrl Pts',(108.702700407335,22.9365,62.9169743942613));
#105100=CARTESIAN_POINT('Ctrl Pts',(108.69994711036,22.9365,62.9327167416041));
#105101=CARTESIAN_POINT('Ctrl Pts',(108.697487323616,22.9365,62.9485115790764));
#105102=CARTESIAN_POINT('Ctrl Pts',(108.696011845669,22.9365,62.9579859509543));
#105103=CARTESIAN_POINT('Ctrl Pts',(108.694642326462,22.9365,62.9674776053876));
#105104=CARTESIAN_POINT('Ctrl Pts',(108.693381127268,22.9365,62.9769727381588));
#105105=CARTESIAN_POINT('Ctrl Pts',(108.686165290403,22.9365,63.0312982796293));
#105106=CARTESIAN_POINT('Ctrl Pts',(108.682474575773,22.9365,63.0858424425533));
#105107=CARTESIAN_POINT('Ctrl Pts',(108.682417947502,22.9365,63.1402759876227));
#105108=CARTESIAN_POINT('Ctrl Pts',(108.682404870894,22.9365,63.1528457892807));
#105109=CARTESIAN_POINT('Ctrl Pts',(108.682585765377,22.9365,63.1654098074689));
#105110=CARTESIAN_POINT('Ctrl Pts',(108.682962323821,22.9365,63.1779641704125));
#105111=CARTESIAN_POINT('Ctrl Pts',(108.684538870899,22.9365,63.2305258499371));
#105112=CARTESIAN_POINT('Ctrl Pts',(108.689540983861,22.9365,63.282917717116));
#105113=CARTESIAN_POINT('Ctrl Pts',(108.697768386234,22.9365,63.3349206222051));
#105114=CARTESIAN_POINT('Ctrl Pts',(108.701733434302,22.9365,63.3599824836571));
#105115=CARTESIAN_POINT('Ctrl Pts',(108.706448361201,22.9365,63.3849541166963));
#105116=CARTESIAN_POINT('Ctrl Pts',(108.711894928251,22.9365,63.4098111733684));
#105117=CARTESIAN_POINT('Ctrl Pts',(108.715369714143,22.9365,63.4256694101346));
#105118=CARTESIAN_POINT('Ctrl Pts',(108.719142342049,22.9365,63.4414810119392));
#105119=CARTESIAN_POINT('Ctrl Pts',(108.723208622296,22.9365,63.4572395968168));
#105120=CARTESIAN_POINT('Ctrl Pts',(108.725624775302,22.9365,63.4666032289071));
#105121=CARTESIAN_POINT('Ctrl Pts',(108.72814432376,22.9365,63.4759466662589));
#105122=CARTESIAN_POINT('Ctrl Pts',(108.730762828323,22.9365,63.4852569757922));
#105123=CARTESIAN_POINT('Ctrl Pts',(108.745611639966,22.9365,63.5380531536391));
#105124=CARTESIAN_POINT('Ctrl Pts',(108.763663964139,22.9365,63.5898852390345));
#105125=CARTESIAN_POINT('Ctrl Pts',(108.784679907723,22.9365,63.6405168651488));
#105126=CARTESIAN_POINT('Ctrl Pts',(108.806153060958,22.9365,63.6922500010769));
#105127=CARTESIAN_POINT('Ctrl Pts',(108.830720405626,22.9365,63.7427308344458));
#105128=CARTESIAN_POINT('Ctrl Pts',(108.85818097311,22.9365,63.7917074971016));
#105129=CARTESIAN_POINT('Ctrl Pts',(108.873566344295,22.9365,63.8191477215167));
#105130=CARTESIAN_POINT('Ctrl Pts',(108.889860870906,22.9365,63.8461157045169));
#105131=CARTESIAN_POINT('Ctrl Pts',(108.907036061991,22.9365,63.8725654110481));
#105132=CARTESIAN_POINT('Ctrl Pts',(108.918731424448,22.9365,63.8905762094857));
#105133=CARTESIAN_POINT('Ctrl Pts',(108.930835239067,22.9365,63.9083466601574));
#105134=CARTESIAN_POINT('Ctrl Pts',(108.943339707194,22.9365,63.9258616387831));
#105135=CARTESIAN_POINT('Ctrl Pts',(108.952067430166,22.9365,63.9380865394941));
#105136=CARTESIAN_POINT('Ctrl Pts',(108.960994393228,22.9365,63.9501920002347));
#105137=CARTESIAN_POINT('Ctrl Pts',(108.970096220285,22.9365,63.9621446561674));
#105138=CARTESIAN_POINT('Ctrl Pts',(109.005382339371,22.9365,64.008482917485));
#105139=CARTESIAN_POINT('Ctrl Pts',(109.043336506866,22.9365,64.0525920408315));
#105140=CARTESIAN_POINT('Ctrl Pts',(109.083734708758,22.9365,64.0942113100944));
#105141=CARTESIAN_POINT('Ctrl Pts',(109.125745560721,22.9365,64.137491973043));
#105142=CARTESIAN_POINT('Ctrl Pts',(109.170399693862,22.9365,64.1780813913725));
#105143=CARTESIAN_POINT('Ctrl Pts',(109.217500216637,22.9365,64.2156643028175));
#105144=CARTESIAN_POINT('Ctrl Pts',(109.261707283157,22.9365,64.2509384392477));
#105145=CARTESIAN_POINT('Ctrl Pts',(109.308070309815,22.9365,64.2835648234591));
#105146=CARTESIAN_POINT('Ctrl Pts',(109.356464298767,22.9365,64.3132494358575));
#105147=CARTESIAN_POINT('Ctrl Pts',(109.359631798921,22.9365,64.3151923634062));
#105148=CARTESIAN_POINT('Ctrl Pts',(109.362808011251,22.9365,64.3171226736369));
#105149=CARTESIAN_POINT('Ctrl Pts',(109.365992905425,22.9365,64.3190402776368));
#105150=CARTESIAN_POINT('Ctrl Pts',(109.313848625014,22.9365,62.0406439634947));
#105151=CARTESIAN_POINT('Ctrl Pts',(109.5989689641,22.9128481667074,61.8396332305574));
#105152=CARTESIAN_POINT('Ctrl Pts',(110.403030903449,22.8629815179371,61.6928883955224));
#105153=CARTESIAN_POINT('Ctrl Pts',(111.321028562455,22.7869000536892,62.5749012318044));
#105154=CARTESIAN_POINT('Ctrl Pts',(111.081739672219,22.7082556072563,63.8694937849383));
#105155=CARTESIAN_POINT('Ctrl Pts',(109.868997477121,22.6296111608234,64.381583208474));
#105156=CARTESIAN_POINT('Ctrl Pts',(108.958935560518,22.5642369201592,63.7740238170161));
#105157=CARTESIAN_POINT('Ctrl Pts',(108.823959301075,22.5250774949727,63.1923462254025));
#105158=CARTESIAN_POINT('Ctrl Pts',(108.824014839234,22.5121328852639,63.0000405433321));
#105159=CARTESIAN_POINT('Origin',(110.,22.9365,63.));
#105160=CARTESIAN_POINT('',(108.5365,22.9365,63.));
#105161=CARTESIAN_POINT('Origin',(110.,22.9365,63.));
#105162=CARTESIAN_POINT('Origin',(110.,22.9365,63.));
#105163=CARTESIAN_POINT('',(110.68466442454,22.9365,62.0417048010816));
#105164=CARTESIAN_POINT('Ctrl Pts',(110.635601384839,22.9365,64.3206560833115));
#105165=CARTESIAN_POINT('Ctrl Pts',(110.676008649758,22.9365,64.29664395265));
#105166=CARTESIAN_POINT('Ctrl Pts',(110.715096848639,22.9365,64.2706323584205));
#105167=CARTESIAN_POINT('Ctrl Pts',(110.75269025251,22.9365,64.2426158721913));
#105168=CARTESIAN_POINT('Ctrl Pts',(110.798395959551,22.9365,64.208553691594));
#105169=CARTESIAN_POINT('Ctrl Pts',(110.841893458597,22.9365,64.171527994697));
#105170=CARTESIAN_POINT('Ctrl Pts',(110.883036378868,22.9365,64.1318377603501));
#105171=CARTESIAN_POINT('Ctrl Pts',(110.899359931227,22.9365,64.1160905646174));
#105172=CARTESIAN_POINT('Ctrl Pts',(110.915312384528,22.9365,64.0999236554903));
#105173=CARTESIAN_POINT('Ctrl Pts',(110.930882702454,22.9365,64.0833548173767));
#105174=CARTESIAN_POINT('Ctrl Pts',(110.938751149424,22.9365,64.0749817690754));
#105175=CARTESIAN_POINT('Ctrl Pts',(110.946519473918,22.9365,64.0665086516793));
#105176=CARTESIAN_POINT('Ctrl Pts',(110.954181051429,22.9365,64.0579441144627));
#105177=CARTESIAN_POINT('Ctrl Pts',(110.992513235231,22.9365,64.0150942686878));
#105178=CARTESIAN_POINT('Ctrl Pts',(111.028219351981,22.9365,63.9699133129342));
#105179=CARTESIAN_POINT('Ctrl Pts',(111.061154023909,22.9365,63.9227144383136));
#105180=CARTESIAN_POINT('Ctrl Pts',(111.083314044193,22.9365,63.8909567811774));
#105181=CARTESIAN_POINT('Ctrl Pts',(111.104218450748,22.9365,63.8582849135692));
#105182=CARTESIAN_POINT('Ctrl Pts',(111.123810367769,22.9365,63.8247900295114));
#105183=CARTESIAN_POINT('Ctrl Pts',(111.133524372102,22.9365,63.8081826986134));
#105184=CARTESIAN_POINT('Ctrl Pts',(111.142915557738,22.9365,63.7913730101249));
#105185=CARTESIAN_POINT('Ctrl Pts',(111.151975993438,22.9365,63.774371987741));
#105186=CARTESIAN_POINT('Ctrl Pts',(111.157376487454,22.9365,63.7642384883516));
#105187=CARTESIAN_POINT('Ctrl Pts',(111.162655947466,22.9365,63.7540434900834));
#105188=CARTESIAN_POINT('Ctrl Pts',(111.167810160439,22.9365,63.7437956545731));
#105189=CARTESIAN_POINT('Ctrl Pts',(111.193058568018,22.9365,63.6935956474827));
#105190=CARTESIAN_POINT('Ctrl Pts',(111.215330076566,22.9365,63.6420829899276));
#105191=CARTESIAN_POINT('Ctrl Pts',(111.234484010569,22.9365,63.5895468299773));
#105192=CARTESIAN_POINT('Ctrl Pts',(111.253155448517,22.9365,63.5383340790941));
#105193=CARTESIAN_POINT('Ctrl Pts',(111.268864506929,22.9365,63.4861477038221));
#105194=CARTESIAN_POINT('Ctrl Pts',(111.281432532302,22.9365,63.4332506881232));
#105195=CARTESIAN_POINT('Ctrl Pts',(111.288890477405,22.9365,63.4018612671534));
#105196=CARTESIAN_POINT('Ctrl Pts',(111.295241437284,22.9365,63.3702215905818));
#105197=CARTESIAN_POINT('Ctrl Pts',(111.300439467589,22.9365,63.3383879468089));
#105198=CARTESIAN_POINT('Ctrl Pts',(111.303237788178,22.9365,63.3212505436816));
#105199=CARTESIAN_POINT('Ctrl Pts',(111.305701862008,22.9365,63.3040569534743));
#105200=CARTESIAN_POINT('Ctrl Pts',(111.307823708633,22.9365,63.2868162116301));
#105201=CARTESIAN_POINT('Ctrl Pts',(111.309374290931,22.9365,63.2742171911429));
#105202=CARTESIAN_POINT('Ctrl Pts',(111.310742299474,22.9365,63.2615892780674));
#105203=CARTESIAN_POINT('Ctrl Pts',(111.311922406986,22.9365,63.2489624959349));
#105204=CARTESIAN_POINT('Ctrl Pts',(111.316832543612,22.9365,63.1964255661834));
#105205=CARTESIAN_POINT('Ctrl Pts',(111.318506445729,22.9365,63.1438207242732));
#105206=CARTESIAN_POINT('Ctrl Pts',(111.316789870112,22.9365,63.0913935960303));
#105207=CARTESIAN_POINT('Ctrl Pts',(111.316337468087,22.9365,63.0775764715292));
#105208=CARTESIAN_POINT('Ctrl Pts',(111.315649293107,22.9365,63.063771725008));
#105209=CARTESIAN_POINT('Ctrl Pts',(111.314721918591,22.9365,63.0499839610383));
#105210=CARTESIAN_POINT('Ctrl Pts',(111.311212128646,22.9365,62.9978020705878));
#105211=CARTESIAN_POINT('Ctrl Pts',(111.304279381792,22.9365,62.945861746428));
#105212=CARTESIAN_POINT('Ctrl Pts',(111.294071418496,22.9365,62.8944277578466));
#105213=CARTESIAN_POINT('Ctrl Pts',(111.289301812052,22.9365,62.870395551204));
#105214=CARTESIAN_POINT('Ctrl Pts',(111.283816571269,22.9365,62.8464741949291));
#105215=CARTESIAN_POINT('Ctrl Pts',(111.27762791159,22.9365,62.8226927216789));
#105216=CARTESIAN_POINT('Ctrl Pts',(111.273232032717,22.9365,62.8058004572379));
#105217=CARTESIAN_POINT('Ctrl Pts',(111.268481212003,22.9365,62.7889787981868));
#105218=CARTESIAN_POINT('Ctrl Pts',(111.263379355067,22.9365,62.772238657017));
#105219=CARTESIAN_POINT('Ctrl Pts',(111.260408650344,22.9365,62.7624912224923));
#105220=CARTESIAN_POINT('Ctrl Pts',(111.257321389305,22.9365,62.7527796664));
#105221=CARTESIAN_POINT('Ctrl Pts',(111.254120497343,22.9365,62.7431105715656));
#105222=CARTESIAN_POINT('Ctrl Pts',(111.237614378183,22.9365,62.6932497098384));
#105223=CARTESIAN_POINT('Ctrl Pts',(111.218077977599,22.9365,62.6444752225303));
#105224=CARTESIAN_POINT('Ctrl Pts',(111.195683828977,22.9365,62.5970463507132));
#105225=CARTESIAN_POINT('Ctrl Pts',(111.173402073509,22.9365,62.5498555178851));
#105226=CARTESIAN_POINT('Ctrl Pts',(111.148290388776,22.9365,62.5039959316499));
#105227=CARTESIAN_POINT('Ctrl Pts',(111.120479595851,22.9365,62.4597557064098));
#105228=CARTESIAN_POINT('Ctrl Pts',(111.106546708327,22.9365,62.4375918621804));
#105229=CARTESIAN_POINT('Ctrl Pts',(111.091935832797,22.9365,62.4158350587755));
#105230=CARTESIAN_POINT('Ctrl Pts',(111.076660633439,22.9365,62.3945256988345));
#105231=CARTESIAN_POINT('Ctrl Pts',(111.065414384295,22.9365,62.3788368449371));
#105232=CARTESIAN_POINT('Ctrl Pts',(111.053807998656,22.9365,62.3633905874213));
#105233=CARTESIAN_POINT('Ctrl Pts',(111.04184643132,22.9365,62.3482041931514));
#105234=CARTESIAN_POINT('Ctrl Pts',(111.03605967185,22.9365,62.34085732895));
#105235=CARTESIAN_POINT('Ctrl Pts',(111.030190308028,22.9365,62.3335721238737));
#105236=CARTESIAN_POINT('Ctrl Pts',(111.024247308606,22.9365,62.3263603111232));
#105237=CARTESIAN_POINT('Ctrl Pts',(110.992177875478,22.9365,62.28744414602));
#105238=CARTESIAN_POINT('Ctrl Pts',(110.957905082491,22.9365,62.2505825372052));
#105239=CARTESIAN_POINT('Ctrl Pts',(110.921559226805,22.9365,62.2160281798043));
#105240=CARTESIAN_POINT('Ctrl Pts',(110.885932624875,22.9365,62.1821576239232));
#105241=CARTESIAN_POINT('Ctrl Pts',(110.848313451306,22.9365,62.1505033205639));
#105242=CARTESIAN_POINT('Ctrl Pts',(110.80880064351,22.9365,62.1213469237875));
#105243=CARTESIAN_POINT('Ctrl Pts',(110.769287835713,22.9365,62.0921905270111));
#105244=CARTESIAN_POINT('Ctrl Pts',(110.727880766146,22.9365,62.0655313526161));
#105245=CARTESIAN_POINT('Ctrl Pts',(110.684664424539,22.9365,62.0417048010816));
#105246=CARTESIAN_POINT('Origin',(110.,22.9365,63.));
#105247=CARTESIAN_POINT('Origin',(110.,23.8608671147362,63.));
#105248=CARTESIAN_POINT('Ctrl Pts',(110.684664424539,22.9365,62.0417048010816));
#105249=CARTESIAN_POINT('Ctrl Pts',(111.000350903699,22.9102851845224,62.2672504386186));
#105250=CARTESIAN_POINT('Ctrl Pts',(111.385893029549,22.8578555535671,63.0515319048078));
#105251=CARTESIAN_POINT('Ctrl Pts',(110.719412413741,22.7792111071341,64.1875760335126));
#105252=CARTESIAN_POINT('Ctrl Pts',(109.404193069561,22.7005666607012,64.2532266483724));
#105253=CARTESIAN_POINT('Ctrl Pts',(108.848682080452,22.6444519965686,63.4962309282256));
#105254=CARTESIAN_POINT('Ctrl Pts',(108.820728885475,22.6145521479135,63.0552666982041));
#105255=CARTESIAN_POINT('Ctrl Pts',(108.821164759239,22.6108671147362,63.0008628562198));
#105256=CARTESIAN_POINT('Ctrl Pts',(110.850780204045,23.1014778394209,61.8091997252243));
#105257=CARTESIAN_POINT('Ctrl Pts',(111.243059688018,23.0752630239433,62.0894680678567));
#105258=CARTESIAN_POINT('Ctrl Pts',(111.722143450431,23.022833392988,63.064034763478));
#105259=CARTESIAN_POINT('Ctrl Pts',(110.893958877104,22.9441889465551,64.4757100615968));
#105260=CARTESIAN_POINT('Ctrl Pts',(109.259636219318,22.8655445001222,64.5572890680476));
#105261=CARTESIAN_POINT('Ctrl Pts',(108.29219639628,22.7869000536892,63.2389572620213));
#105262=CARTESIAN_POINT('Ctrl Pts',(108.860964579279,22.7082556072563,61.705071531042));
#105263=CARTESIAN_POINT('Ctrl Pts',(110.454735846337,22.6296111608233,61.3365468018618));
#105264=CARTESIAN_POINT('Ctrl Pts',(111.639284007435,22.5509667143904,62.4645709929793));
#105265=CARTESIAN_POINT('Ctrl Pts',(111.348943349404,22.4723222679575,64.0743989253347));
#105266=CARTESIAN_POINT('Ctrl Pts',(109.844889482201,22.3936778215245,64.7175221473246));
#105267=CARTESIAN_POINT('Ctrl Pts',(108.48040266922,22.3150333750916,63.8153380346798));
#105268=CARTESIAN_POINT('Ctrl Pts',(108.483151555408,22.2363889286587,62.1795573070613));
#105269=CARTESIAN_POINT('Ctrl Pts',(109.850668524615,22.1577444822257,61.2819628846047));
#105270=CARTESIAN_POINT('Ctrl Pts',(111.352543852904,22.0791000357928,61.9301505368133));
#105271=CARTESIAN_POINT('Ctrl Pts',(111.637484411459,22.0004555893599,63.5409230727486));
#105272=CARTESIAN_POINT('Ctrl Pts',(110.449117708462,21.9218111429269,64.6650062639624));
#105273=CARTESIAN_POINT('Ctrl Pts',(108.856662862094,21.843166696494,64.2910200479365));
#105274=CARTESIAN_POINT('Ctrl Pts',(108.292911773801,21.7645222500611,62.7554539790191));
#105275=CARTESIAN_POINT('Ctrl Pts',(109.265093245523,21.6858778036281,61.4399151272655));
#105276=CARTESIAN_POINT('Ctrl Pts',(110.89849765686,21.6072333571952,61.5280443688639));
#105277=CARTESIAN_POINT('Ctrl Pts',(111.72349087482,21.5285889107623,62.9405473241227));
#105278=CARTESIAN_POINT('Ctrl Pts',(110.997790898104,21.4499444643293,64.4065438074122));
#105279=CARTESIAN_POINT('Ctrl Pts',(109.374346576754,21.3713000178964,64.6070156792213));
#105280=CARTESIAN_POINT('Ctrl Pts',(108.313813436029,21.2926555714635,63.3616021047284));
#105281=CARTESIAN_POINT('Ctrl Pts',(108.770434292712,21.2140111250305,61.79082488859));
#105282=CARTESIAN_POINT('Ctrl Pts',(110.333282961828,21.1353666785976,61.3080237295711));
#105283=CARTESIAN_POINT('Ctrl Pts',(111.59639072099,21.0567222321647,62.3474832605112));
#105284=CARTESIAN_POINT('Ctrl Pts',(111.42289537832,20.9780777857317,63.9741983701003));
#105285=CARTESIAN_POINT('Ctrl Pts',(109.969743391005,20.8994333392988,64.7240569325918));
#105286=CARTESIAN_POINT('Ctrl Pts',(108.542590784426,20.8207888928659,63.9234939297106));
#105287=CARTESIAN_POINT('Ctrl Pts',(108.429388159401,20.7421444464329,62.2907349148822));
#105288=CARTESIAN_POINT('Ctrl Pts',(109.29221212424,20.6897148154776,61.6313137282942));
#105289=CARTESIAN_POINT('Ctrl Pts',(109.768242272559,20.6635,61.5549669187969));
#105290=CARTESIAN_POINT('Ctrl Pts',(110.795408277543,23.0464852262806,61.8867014171768));
#105291=CARTESIAN_POINT('Ctrl Pts',(111.162156759912,23.020270410803,62.1487288581107));
#105292=CARTESIAN_POINT('Ctrl Pts',(111.610059976804,22.9678407798477,63.0598671439213));
#105293=CARTESIAN_POINT('Ctrl Pts',(110.83577672265,22.8891963334148,64.3796653855687));
#105294=CARTESIAN_POINT('Ctrl Pts',(109.307821836066,22.8105518869818,64.4559349281559));
#105295=CARTESIAN_POINT('Ctrl Pts',(108.403346579577,22.7319074405489,63.2234050384426));
#105296=CARTESIAN_POINT('Ctrl Pts',(108.935097222821,22.653262994116,61.7893502715054));
#105297=CARTESIAN_POINT('Ctrl Pts',(110.425139953365,22.574618547683,61.4448104965135));
#105298=CARTESIAN_POINT('Ctrl Pts',(111.532593333224,22.4959741012501,62.4994186956911));
#105299=CARTESIAN_POINT('Ctrl Pts',(111.261149120479,22.4173296548172,64.0044730642906));
#105300=CARTESIAN_POINT('Ctrl Pts',(109.854984649144,22.3386852083842,64.6057394452183));
#105301=CARTESIAN_POINT('Ctrl Pts',(108.579303691261,22.2600407619513,63.7622728158186));
#105302=CARTESIAN_POINT('Ctrl Pts',(108.581873669755,22.1813963155184,62.2329547559868));
#105303=CARTESIAN_POINT('Ctrl Pts',(109.860387570075,22.1027518690854,61.3937791027402));
#105304=CARTESIAN_POINT('Ctrl Pts',(111.264515289878,22.0241074226525,61.9997803020122));
#105305=CARTESIAN_POINT('Ctrl Pts',(111.530910861619,21.9454629762196,63.5057177958922));
#105306=CARTESIAN_POINT('Ctrl Pts',(110.41988746471,21.8668185297866,64.5566414900353));
#105307=CARTESIAN_POINT('Ctrl Pts',(108.931075477322,21.7881740833537,64.2069956819877));
#105308=CARTESIAN_POINT('Ctrl Pts',(108.404015397679,21.7095296369207,62.7713699397287));
#105309=CARTESIAN_POINT('Ctrl Pts',(109.312923698796,21.6308851904878,61.5414512284804));
#105310=CARTESIAN_POINT('Ctrl Pts',(110.84002010181,21.5522407440549,61.6238446926533));
#105311=CARTESIAN_POINT('Ctrl Pts',(111.611319705823,21.4735962976219,62.9444167244488));
#105312=CARTESIAN_POINT('Ctrl Pts',(110.932850971186,21.394951851189,64.3150007273602));
#105313=CARTESIAN_POINT('Ctrl Pts',(109.415066418616,21.3163074047561,64.5024251473144));
#105314=CARTESIAN_POINT('Ctrl Pts',(108.423556702321,21.2376629583232,63.3380677005772));
#105315=CARTESIAN_POINT('Ctrl Pts',(108.850458982579,21.1590185118902,61.8695224829609));
#105316=CARTESIAN_POINT('Ctrl Pts',(110.311591672375,21.0803740654573,61.4181438114013));
#105317=CARTESIAN_POINT('Ctrl Pts',(111.492491700714,21.0017296190243,62.3899514664806));
#105318=CARTESIAN_POINT('Ctrl Pts',(111.330288077476,20.9230851725914,63.9107939322786));
#105319=CARTESIAN_POINT('Ctrl Pts',(109.971712603172,20.8444407261585,64.611848922459));
#105320=CARTESIAN_POINT('Ctrl Pts',(108.637444373619,20.7657962797255,63.8633895246509));
#105321=CARTESIAN_POINT('Ctrl Pts',(108.53160939467,20.6871518332926,62.3368965133499));
#105322=CARTESIAN_POINT('Ctrl Pts',(109.338277580452,20.6347222023373,61.7203928997189));
#105323=CARTESIAN_POINT('Ctrl Pts',(109.783325923764,20.6085073868597,61.6490150233303));
#105324=CARTESIAN_POINT('Ctrl Pts',(110.740036351041,22.9914926131403,61.9642031091292));
#105325=CARTESIAN_POINT('Ctrl Pts',(111.081253831805,22.9652777976627,62.2079896483646));
#105326=CARTESIAN_POINT('Ctrl Pts',(111.497976503177,22.9128481667074,63.0556995243645));
#105327=CARTESIAN_POINT('Ctrl Pts',(110.777594568195,22.8342037202745,64.2836207095406));
#105328=CARTESIAN_POINT('Ctrl Pts',(109.356007452813,22.7555592738415,64.3545807882641));
#105329=CARTESIAN_POINT('Ctrl Pts',(108.514496762873,22.6769148274086,63.2078528148638));
#105330=CARTESIAN_POINT('Ctrl Pts',(109.009229866363,22.5982703809757,61.8736290119688));
#105331=CARTESIAN_POINT('Ctrl Pts',(110.395544060394,22.5196259345427,61.5530741911651));
#105332=CARTESIAN_POINT('Ctrl Pts',(111.425902659012,22.4409814881098,62.5342663984029));
#105333=CARTESIAN_POINT('Ctrl Pts',(111.173354891555,22.3623370416769,63.9345472032464));
#105334=CARTESIAN_POINT('Ctrl Pts',(109.865079816086,22.2836925952439,64.4939567431119));
#105335=CARTESIAN_POINT('Ctrl Pts',(108.678204713302,22.205048148811,63.7092075969576));
#105336=CARTESIAN_POINT('Ctrl Pts',(108.680595784103,22.1264037023781,62.2863522049122));
#105337=CARTESIAN_POINT('Ctrl Pts',(109.870106615535,22.0477592559451,61.5055953208758));
#105338=CARTESIAN_POINT('Ctrl Pts',(111.176486726852,21.9691148095122,62.0694100672111));
#105339=CARTESIAN_POINT('Ctrl Pts',(111.424337311778,21.8904703630792,63.4705125190358));
#105340=CARTESIAN_POINT('Ctrl Pts',(110.390657220958,21.8118259166463,64.4482767161081));
#105341=CARTESIAN_POINT('Ctrl Pts',(109.005488092549,21.7331814702134,64.122971316039));
#105342=CARTESIAN_POINT('Ctrl Pts',(108.515119021557,21.6545370237804,62.7872859004382));
#105343=CARTESIAN_POINT('Ctrl Pts',(109.360754152068,21.5758925773475,61.6429873296953));
#105344=CARTESIAN_POINT('Ctrl Pts',(110.78154254676,21.4972481309146,61.7196450164426));
#105345=CARTESIAN_POINT('Ctrl Pts',(111.499148536827,21.4186036844817,62.948286124775));
#105346=CARTESIAN_POINT('Ctrl Pts',(110.867911044268,21.3399592380487,64.2234576473083));
#105347=CARTESIAN_POINT('Ctrl Pts',(109.455786260477,21.2613147916158,64.3978346154074));
#105348=CARTESIAN_POINT('Ctrl Pts',(108.533299968613,21.1826703451828,63.3145332964259));
#105349=CARTESIAN_POINT('Ctrl Pts',(108.930483672445,21.1040258987499,61.9482200773318));
#105350=CARTESIAN_POINT('Ctrl Pts',(110.289900382923,21.025381452317,61.5282638932313));
#105351=CARTESIAN_POINT('Ctrl Pts',(111.388592680437,20.946737005884,62.4324196724501));
#105352=CARTESIAN_POINT('Ctrl Pts',(111.237680776632,20.8680925594511,63.8473894944569));
#105353=CARTESIAN_POINT('Ctrl Pts',(109.973681815339,20.7894481130182,64.4996409123262));
#105354=CARTESIAN_POINT('Ctrl Pts',(108.732297962812,20.7108036665852,63.8032851195911));
#105355=CARTESIAN_POINT('Ctrl Pts',(108.63383062994,20.6321592201523,62.3830581118176));
#105356=CARTESIAN_POINT('Ctrl Pts',(109.384343036664,20.579729589197,61.8094720711435));
#105357=CARTESIAN_POINT('Ctrl Pts',(109.798409574969,20.5535147737194,61.7430631278637));
#105358=CARTESIAN_POINT('Ctrl Pts',(110.684664424539,22.9365,62.0417048010816));
#105359=CARTESIAN_POINT('Ctrl Pts',(111.000350903699,22.9102851845224,62.2672504386186));
#105360=CARTESIAN_POINT('Ctrl Pts',(111.385893029549,22.8578555535671,63.0515319048078));
#105361=CARTESIAN_POINT('Ctrl Pts',(110.719412413741,22.7792111071341,64.1875760335126));
#105362=CARTESIAN_POINT('Ctrl Pts',(109.404193069561,22.7005666607012,64.2532266483724));
#105363=CARTESIAN_POINT('Ctrl Pts',(108.62564694617,22.6219222142683,63.192300591285));
#105364=CARTESIAN_POINT('Ctrl Pts',(109.083362509905,22.5432777678353,61.9579077524323));
#105365=CARTESIAN_POINT('Ctrl Pts',(110.365948167423,22.4646333214024,61.6613378858167));
#105366=CARTESIAN_POINT('Ctrl Pts',(111.319211984801,22.3859888749695,62.5691141011147));
#105367=CARTESIAN_POINT('Ctrl Pts',(111.085560662631,22.3073444285365,63.8646213422023));
#105368=CARTESIAN_POINT('Ctrl Pts',(109.875174983029,22.2286999821036,64.3821740410055));
#105369=CARTESIAN_POINT('Ctrl Pts',(108.777105735343,22.1500555356707,63.6561423780964));
#105370=CARTESIAN_POINT('Ctrl Pts',(108.77931789845,22.0714110892377,62.3397496538377));
#105371=CARTESIAN_POINT('Ctrl Pts',(109.879825660995,21.9927666428048,61.6174115390114));
#105372=CARTESIAN_POINT('Ctrl Pts',(111.088458163825,21.9141221963719,62.1390398324099));
#105373=CARTESIAN_POINT('Ctrl Pts',(111.317763761938,21.8354777499389,63.4353072421795));
#105374=CARTESIAN_POINT('Ctrl Pts',(110.361426977206,21.756833303506,64.3399119421809));
#105375=CARTESIAN_POINT('Ctrl Pts',(109.079900707777,21.6781888570731,64.0389469500903));
#105376=CARTESIAN_POINT('Ctrl Pts',(108.626222645435,21.5995444106401,62.8032018611478));
#105377=CARTESIAN_POINT('Ctrl Pts',(109.40858460534,21.5208999642072,61.7445234309101));
#105378=CARTESIAN_POINT('Ctrl Pts',(110.72306499171,21.4422555177743,61.815445340232));
#105379=CARTESIAN_POINT('Ctrl Pts',(111.38697736783,21.3636110713413,62.9521555251011));
#105380=CARTESIAN_POINT('Ctrl Pts',(110.80297111735,21.2849666249084,64.1319145672564));
#105381=CARTESIAN_POINT('Ctrl Pts',(109.496506102338,21.2063221784755,64.2932440835005));
#105382=CARTESIAN_POINT('Ctrl Pts',(108.643043234905,21.1276777320425,63.2909988922746));
#105383=CARTESIAN_POINT('Ctrl Pts',(109.010508362311,21.0490332856096,62.0269176717027));
#105384=CARTESIAN_POINT('Ctrl Pts',(110.26820909347,20.9703888391767,61.6383839750614));
#105385=CARTESIAN_POINT('Ctrl Pts',(111.284693660161,20.8917443927437,62.4748878784196));
#105386=CARTESIAN_POINT('Ctrl Pts',(111.145073475788,20.8130999463108,63.7839850566352));
#105387=CARTESIAN_POINT('Ctrl Pts',(109.975651027507,20.7344554998779,64.3874329021934));
#105388=CARTESIAN_POINT('Ctrl Pts',(108.827151552004,20.6558110534449,63.7431807145313));
#105389=CARTESIAN_POINT('Ctrl Pts',(108.73605186521,20.577166607012,62.4292197102853));
#105390=CARTESIAN_POINT('Ctrl Pts',(109.430408492876,20.5247369760567,61.8985512425682));
#105391=CARTESIAN_POINT('Ctrl Pts',(109.813493226174,20.4985221605791,61.8371112323971));
#105392=CARTESIAN_POINT('Ctrl Pts',(109.768242272559,20.6635,61.554966918797));
#105393=CARTESIAN_POINT('Ctrl Pts',(109.29221212424,20.6897148154776,61.6313137282943));
#105394=CARTESIAN_POINT('Ctrl Pts',(108.86080014182,20.7159296309553,61.9610243215882));
#105395=CARTESIAN_POINT('Ctrl Pts',(108.663961254782,20.7421444464329,62.3980061207066));
#105396=CARTESIAN_POINT('Ctrl Pts',(108.57961238167,20.7533779490077,62.585260391853));
#105397=CARTESIAN_POINT('Ctrl Pts',(108.538337485068,20.7646114515824,62.7922125631031));
#105398=CARTESIAN_POINT('Ctrl Pts',(108.538910502742,20.7758449541571,62.9995078540291));
#105399=CARTESIAN_POINT('Origin',(110.,23.1,63.));
#105400=CARTESIAN_POINT('',(108.983974596216,23.2,63.));
#105401=CARTESIAN_POINT('Origin',(110.,23.2,63.));
#105402=CARTESIAN_POINT('',(109.133974596216,23.05,63.));
#105403=CARTESIAN_POINT('',(109.083974596216,23.1,63.));
#105404=CARTESIAN_POINT('',(109.189703570316,23.,62.9034745854044));
#105405=CARTESIAN_POINT('Ctrl Pts',(109.189703570316,23.,62.9034745854044));
#105406=CARTESIAN_POINT('Ctrl Pts',(109.162667372368,23.0213072238479,62.9503026538943));
#105407=CARTESIAN_POINT('Ctrl Pts',(109.133974596216,23.05,63.));
#105408=CARTESIAN_POINT('',(109.511258324007,23.,62.3465254145956));
#105409=CARTESIAN_POINT('Origin',(110.,23.,63.));
#105410=CARTESIAN_POINT('',(109.566987298108,23.05,62.25));
#105411=CARTESIAN_POINT('Ctrl Pts',(109.566987298108,23.05,62.25));
#105412=CARTESIAN_POINT('Ctrl Pts',(109.538294521956,23.0213072238479,62.2996973461057));
#105413=CARTESIAN_POINT('Ctrl Pts',(109.511258324007,23.,62.3465254145956));
#105414=CARTESIAN_POINT('',(109.678445246309,23.,62.25));
#105415=CARTESIAN_POINT('Ctrl Pts',(109.678445246309,23.,62.25));
#105416=CARTESIAN_POINT('Ctrl Pts',(109.624372850412,23.0213072238479,62.25));
#105417=CARTESIAN_POINT('Ctrl Pts',(109.566987298108,23.05,62.25));
#105418=CARTESIAN_POINT('',(110.321554753691,23.,62.25));
#105419=CARTESIAN_POINT('Origin',(110.,23.,63.));
#105420=CARTESIAN_POINT('',(110.433012701892,23.05,62.25));
#105421=CARTESIAN_POINT('Ctrl Pts',(110.433012701892,23.05,62.25));
#105422=CARTESIAN_POINT('Ctrl Pts',(110.375627149588,23.0213072238479,62.25));
#105423=CARTESIAN_POINT('Ctrl Pts',(110.321554753691,23.,62.25));
#105424=CARTESIAN_POINT('',(110.488741675993,23.,62.3465254145956));
#105425=CARTESIAN_POINT('Ctrl Pts',(110.488741675993,23.,62.3465254145956));
#105426=CARTESIAN_POINT('Ctrl Pts',(110.461705478044,23.0213072238479,62.2996973461057));
#105427=CARTESIAN_POINT('Ctrl Pts',(110.433012701892,23.05,62.25));
#105428=CARTESIAN_POINT('',(110.810296429684,23.,62.9034745854044));
#105429=CARTESIAN_POINT('Origin',(110.,23.,63.));
#105430=CARTESIAN_POINT('',(110.866025403784,23.05,63.));
#105431=CARTESIAN_POINT('Ctrl Pts',(110.866025403784,23.05,63.));
#105432=CARTESIAN_POINT('Ctrl Pts',(110.837332627632,23.0213072238478,62.9503026538943));
#105433=CARTESIAN_POINT('Ctrl Pts',(110.810296429684,23.,62.9034745854044));
#105434=CARTESIAN_POINT('',(110.810296429684,23.,63.0965254145955));
#105435=CARTESIAN_POINT('Ctrl Pts',(110.810296429684,23.,63.0965254145956));
#105436=CARTESIAN_POINT('Ctrl Pts',(110.837332627632,23.0213072238479,63.0496973461056));
#105437=CARTESIAN_POINT('Ctrl Pts',(110.866025403784,23.05,63.));
#105438=CARTESIAN_POINT('',(110.488741675993,23.,63.6534745854045));
#105439=CARTESIAN_POINT('Origin',(110.,23.,63.));
#105440=CARTESIAN_POINT('',(110.433012701892,23.05,63.75));
#105441=CARTESIAN_POINT('Ctrl Pts',(110.433012701892,23.05,63.75));
#105442=CARTESIAN_POINT('Ctrl Pts',(110.461705478044,23.0213072238479,63.7003026538944));
#105443=CARTESIAN_POINT('Ctrl Pts',(110.488741675993,23.,63.6534745854045));
#105444=CARTESIAN_POINT('',(110.321554753691,23.,63.75));
#105445=CARTESIAN_POINT('Ctrl Pts',(110.321554753691,23.,63.75));
#105446=CARTESIAN_POINT('Ctrl Pts',(110.375627149588,23.0213072238479,63.75));
#105447=CARTESIAN_POINT('Ctrl Pts',(110.433012701892,23.05,63.75));
#105448=CARTESIAN_POINT('',(109.678445246309,23.,63.75));
#105449=CARTESIAN_POINT('Origin',(110.,23.,63.));
#105450=CARTESIAN_POINT('',(109.566987298108,23.05,63.75));
#105451=CARTESIAN_POINT('Ctrl Pts',(109.566987298108,23.05,63.75));
#105452=CARTESIAN_POINT('Ctrl Pts',(109.624372850412,23.0213072238479,63.75));
#105453=CARTESIAN_POINT('Ctrl Pts',(109.678445246309,23.,63.75));
#105454=CARTESIAN_POINT('',(109.511258324007,23.,63.6534745854045));
#105455=CARTESIAN_POINT('Ctrl Pts',(109.511258324007,23.,63.6534745854045));
#105456=CARTESIAN_POINT('Ctrl Pts',(109.538294521956,23.0213072238479,63.7003026538943));
#105457=CARTESIAN_POINT('Ctrl Pts',(109.566987298108,23.05,63.75));
#105458=CARTESIAN_POINT('',(109.189703570316,23.,63.0965254145955));
#105459=CARTESIAN_POINT('Origin',(110.,23.,63.));
#105460=CARTESIAN_POINT('Ctrl Pts',(109.133974596216,23.05,63.));
#105461=CARTESIAN_POINT('Ctrl Pts',(109.162667372368,23.0213072238479,63.0496973461056));
#105462=CARTESIAN_POINT('Ctrl Pts',(109.189703570316,23.,63.0965254145955));
#105463=CARTESIAN_POINT('Origin',(110.,23.1,63.));
#105464=CARTESIAN_POINT('',(110.321554753691,23.2,62.25));
#105465=CARTESIAN_POINT('',(110.321554753691,23.1,62.25));
#105466=CARTESIAN_POINT('',(109.678445246309,23.2,62.25));
#105467=CARTESIAN_POINT('',(109.678445246309,23.1,62.25));
#105468=CARTESIAN_POINT('Origin',(110.,23.2,63.));
#105469=CARTESIAN_POINT('Origin',(110.,23.1,63.));
#105470=CARTESIAN_POINT('',(110.810296429684,23.2,62.9034745854044));
#105471=CARTESIAN_POINT('',(110.810296429684,23.1,62.9034745854044));
#105472=CARTESIAN_POINT('',(110.488741675993,23.2,62.3465254145956));
#105473=CARTESIAN_POINT('',(110.488741675993,23.1,62.3465254145956));
#105474=CARTESIAN_POINT('Origin',(110.,23.2,63.));
#105475=CARTESIAN_POINT('Origin',(110.,23.1,63.));
#105476=CARTESIAN_POINT('',(109.189703570316,23.2,62.9034745854044));
#105477=CARTESIAN_POINT('',(109.189703570316,23.1,62.9034745854044));
#105478=CARTESIAN_POINT('',(109.511258324007,23.2,62.3465254145956));
#105479=CARTESIAN_POINT('Origin',(110.,23.2,63.));
#105480=CARTESIAN_POINT('',(109.511258324007,23.1,62.3465254145956));
#105481=CARTESIAN_POINT('Origin',(110.,23.1,63.));
#105482=CARTESIAN_POINT('',(110.488741675993,23.2,63.6534745854045));
#105483=CARTESIAN_POINT('',(110.488741675993,23.1,63.6534745854045));
#105484=CARTESIAN_POINT('',(110.810296429684,23.2,63.0965254145955));
#105485=CARTESIAN_POINT('',(110.810296429684,23.1,63.0965254145955));
#105486=CARTESIAN_POINT('Origin',(110.,23.2,63.));
#105487=CARTESIAN_POINT('Origin',(110.,23.1,63.));
#105488=CARTESIAN_POINT('',(109.511258324007,23.2,63.6534745854045));
#105489=CARTESIAN_POINT('',(109.511258324007,23.1,63.6534745854045));
#105490=CARTESIAN_POINT('',(109.189703570316,23.2,63.0965254145955));
#105491=CARTESIAN_POINT('Origin',(110.,23.2,63.));
#105492=CARTESIAN_POINT('',(109.189703570316,23.1,63.0965254145955));
#105493=CARTESIAN_POINT('Origin',(110.,23.1,63.));
#105494=CARTESIAN_POINT('',(110.321554753691,23.2,63.75));
#105495=CARTESIAN_POINT('',(110.321554753691,23.1,63.75));
#105496=CARTESIAN_POINT('',(109.678445246309,23.2,63.75));
#105497=CARTESIAN_POINT('Origin',(110.,23.2,63.));
#105498=CARTESIAN_POINT('',(109.678445246309,23.1,63.75));
#105499=CARTESIAN_POINT('Origin',(110.866025403784,23.2,63.));
#105500=CARTESIAN_POINT('',(110.907772228311,23.2,62.9276923788647));
#105501=CARTESIAN_POINT('',(110.866025403784,22.,63.));
#105502=CARTESIAN_POINT('',(110.866025403784,23.2,63.));
#105503=CARTESIAN_POINT('',(110.433012701892,22.,63.75));
#105504=CARTESIAN_POINT('',(110.866025403784,22.,63.));
#105505=CARTESIAN_POINT('',(110.433012701892,23.2,63.75));
#105506=CARTESIAN_POINT('Origin',(110.433012701892,23.2,62.25));
#105507=CARTESIAN_POINT('',(110.691265877365,23.2,62.6973076211353));
#105508=CARTESIAN_POINT('',(110.433012701892,22.,62.25));
#105509=CARTESIAN_POINT('',(110.433012701892,23.2,62.25));
#105510=CARTESIAN_POINT('',(110.433012701892,22.,62.25));
#105511=CARTESIAN_POINT('Origin',(109.566987298108,23.2,62.25));
#105512=CARTESIAN_POINT('',(110.383493649054,23.2,62.25));
#105513=CARTESIAN_POINT('',(109.566987298108,22.,62.25));
#105514=CARTESIAN_POINT('',(109.566987298108,23.2,62.25));
#105515=CARTESIAN_POINT('',(109.566987298108,22.,62.25));
#105516=CARTESIAN_POINT('Origin',(111.2,23.2,63.));
#105517=CARTESIAN_POINT('Origin',(111.2,23.2,63.));
#105518=CARTESIAN_POINT('Origin',(111.2,23.2,63.));
#105519=CARTESIAN_POINT('',(109.392227771689,23.2,62.5526923788647));
#105520=CARTESIAN_POINT('Origin',(111.2,23.2,63.));
#105521=CARTESIAN_POINT('Origin',(111.2,23.2,63.));
#105522=CARTESIAN_POINT('',(109.608734122635,23.2,63.8223076211353));
#105523=CARTESIAN_POINT('Origin',(111.2,23.2,63.));
#105524=CARTESIAN_POINT('',(110.816506350946,23.2,63.75));
#105525=CARTESIAN_POINT('Origin',(110.866025403784,22.,63.));
#105526=CARTESIAN_POINT('',(109.133974596216,22.,63.));
#105527=CARTESIAN_POINT('',(109.133974596216,22.,63.));
#105528=CARTESIAN_POINT('Origin',(110.,22.,63.));
#105529=CARTESIAN_POINT('Origin',(110.866025403784,22.,63.));
#105530=CARTESIAN_POINT('Origin',(110.,22.,63.));
#105531=CARTESIAN_POINT('Origin',(110.866025403784,22.,63.));
#105532=CARTESIAN_POINT('Origin',(110.,22.,63.));
#105533=CARTESIAN_POINT('Origin',(110.866025403784,22.,63.));
#105534=CARTESIAN_POINT('Origin',(110.,22.,63.));
#105535=CARTESIAN_POINT('Origin',(110.866025403784,22.,63.));
#105536=CARTESIAN_POINT('',(109.566987298108,22.,63.75));
#105537=CARTESIAN_POINT('',(110.433012701892,22.,63.75));
#105538=CARTESIAN_POINT('Origin',(110.,22.,63.));
#105539=CARTESIAN_POINT('Origin',(110.866025403784,22.,63.));
#105540=CARTESIAN_POINT('',(109.566987298108,22.,63.75));
#105541=CARTESIAN_POINT('Origin',(110.,22.,63.));
#105542=CARTESIAN_POINT('Origin',(110.,22.,63.));
#105543=CARTESIAN_POINT('',(110.,21.4796394397885,63.));
#105544=CARTESIAN_POINT('',(109.133974596216,22.,63.));
#105545=CARTESIAN_POINT('Origin',(109.133974596216,23.2,63.));
#105546=CARTESIAN_POINT('',(109.133974596216,23.2,63.));
#105547=CARTESIAN_POINT('Origin',(109.566987298108,23.2,63.75));
#105548=CARTESIAN_POINT('',(109.566987298108,23.2,63.75));
#105549=CARTESIAN_POINT('Origin',(110.433012701892,23.2,63.75));
#105550=CARTESIAN_POINT('Origin',(111.2,23.2,63.));
#105551=CARTESIAN_POINT('',(108.8,23.2,63.));
#105552=CARTESIAN_POINT('Origin',(110.,23.2,63.));
#105553=CARTESIAN_POINT('Origin',(110.,23.05,63.));
#105554=CARTESIAN_POINT('',(108.65,23.05,63.));
#105555=CARTESIAN_POINT('Origin',(110.,21.8,63.));
#105556=CARTESIAN_POINT('Origin',(110.,20.6635,63.));
#105557=CARTESIAN_POINT('Origin',(110.,20.45,63.));
#105558=CARTESIAN_POINT('',(109.,20.2,63.));
#105559=CARTESIAN_POINT('Origin',(110.,20.2,63.));
#105560=CARTESIAN_POINT('',(108.75,20.45,63.));
#105561=CARTESIAN_POINT('Origin',(110.,20.2,63.));
#105562=CARTESIAN_POINT('',(0.,0.,0.));
#105563=CARTESIAN_POINT('Origin',(110.,21.33,33.3));
#105564=CARTESIAN_POINT('',(109.032067739078,21.8642640831103,33.3006146958441));
#105565=CARTESIAN_POINT('',(109.032510608047,21.9222359168897,33.3005483021895));
#105566=CARTESIAN_POINT('',(109.03325,21.33,33.3));
#105567=CARTESIAN_POINT('',(110.425646877672,21.99325,34.1689059799454));
#105568=CARTESIAN_POINT('Ctrl Pts',(109.032067739078,21.8642640831103,33.3006146958441));
#105569=CARTESIAN_POINT('Ctrl Pts',(109.031818204458,21.8665686489192,33.3354978137518));
#105570=CARTESIAN_POINT('Ctrl Pts',(109.033539730099,21.8688732147281,33.3703553556597));
#105571=CARTESIAN_POINT('Ctrl Pts',(109.037313868836,21.871177780537,33.4049881195007));
#105572=CARTESIAN_POINT('Ctrl Pts',(109.071918534281,21.8923080924762,33.7225321446948));
#105573=CARTESIAN_POINT('Ctrl Pts',(109.27908341892,21.9134384044155,34.0211794023689));
#105574=CARTESIAN_POINT('Ctrl Pts',(109.564445284039,21.9345687163547,34.1649116522973));
#105575=CARTESIAN_POINT('Ctrl Pts',(109.828606087672,21.9541291442365,34.2979652634834));
#105576=CARTESIAN_POINT('Ctrl Pts',(110.1597761584,21.9736895721183,34.2982676985065));
#105577=CARTESIAN_POINT('Ctrl Pts',(110.426174626828,21.99325,34.1695497362104));
#105578=CARTESIAN_POINT('',(109.574880871485,21.99325,34.1682622236805));
#105579=CARTESIAN_POINT('Origin',(110.,21.99325,33.3));
#105580=CARTESIAN_POINT('Ctrl Pts',(109.574880871485,21.99325,34.1682622236805));
#105581=CARTESIAN_POINT('Ctrl Pts',(109.286692341569,21.9721196880608,34.0271591636317));
#105582=CARTESIAN_POINT('Ctrl Pts',(109.076879953927,21.9509893761215,33.7321151931956));
#105583=CARTESIAN_POINT('Ctrl Pts',(109.038873374224,21.9298590641823,33.4154564405219));
#105584=CARTESIAN_POINT('Ctrl Pts',(109.034302850829,21.9273180150847,33.3773762910182));
#105585=CARTESIAN_POINT('Ctrl Pts',(109.032216902585,21.9247769659872,33.3389835586544));
#105586=CARTESIAN_POINT('Ctrl Pts',(109.032510608047,21.9222359168897,33.3005483021895));
#105587=CARTESIAN_POINT('Origin',(110.,21.33,33.3));
#105588=CARTESIAN_POINT('',(109.034572229009,21.4642640831103,33.3004087423462));
#105589=CARTESIAN_POINT('',(109.034617182386,21.5222359168897,33.300357734449));
#105590=CARTESIAN_POINT('',(109.03325,21.33,33.3));
#105591=CARTESIAN_POINT('Ctrl Pts',(109.034572229009,21.4642640831103,33.3004087423462));
#105592=CARTESIAN_POINT('Ctrl Pts',(109.034056633714,21.4731201106171,33.4353604451549));
#105593=CARTESIAN_POINT('Ctrl Pts',(109.06044141107,21.4819761381238,33.5701194095229));
#105594=CARTESIAN_POINT('Ctrl Pts',(109.114708801304,21.4908321656306,33.6925157712021));
#105595=CARTESIAN_POINT('Ctrl Pts',(109.244189754576,21.5119624775698,33.9845511449109));
#105596=CARTESIAN_POINT('Ctrl Pts',(109.532403761939,21.5330927895091,34.2062074013583));
#105597=CARTESIAN_POINT('Ctrl Pts',(109.847891962672,21.5542231014483,34.256384606394));
#105598=CARTESIAN_POINT('Ctrl Pts',(110.163380163405,21.5753534133876,34.3065618114296));
#105599=CARTESIAN_POINT('Ctrl Pts',(110.506142557508,21.5964837253268,34.1852599650534));
#105600=CARTESIAN_POINT('Ctrl Pts',(110.719835444608,21.6176140372661,33.947802969508));
#105601=CARTESIAN_POINT('Ctrl Pts',(110.933528331708,21.6387443492053,33.7103459739625));
#105602=CARTESIAN_POINT('Ctrl Pts',(111.018151711806,21.6598746611446,33.3567338292479));
#105603=CARTESIAN_POINT('Ctrl Pts',(110.935113419845,21.6810049730838,33.0482654179561));
#105604=CARTESIAN_POINT('Ctrl Pts',(110.852075127883,21.702135285023,32.7397970066643));
#105605=CARTESIAN_POINT('Ctrl Pts',(110.601375163861,21.7232655969623,32.4764723287954));
#105606=CARTESIAN_POINT('Ctrl Pts',(110.297349367024,21.7443959089015,32.3783791328529));
#105607=CARTESIAN_POINT('Ctrl Pts',(109.993323570188,21.7655262208408,32.2802859369104));
#105608=CARTESIAN_POINT('Ctrl Pts',(109.635971940536,21.78665653278,32.3474242228943));
#105609=CARTESIAN_POINT('Ctrl Pts',(109.388318348837,21.8077868447193,32.5492137622433));
#105610=CARTESIAN_POINT('Ctrl Pts',(109.167674959425,21.8266125908496,32.7289952368599));
#105611=CARTESIAN_POINT('Ctrl Pts',(109.034106160108,21.84543833698,33.0156583194923));
#105612=CARTESIAN_POINT('Ctrl Pts',(109.032067739078,21.8642640831103,33.3006146958441));
#105613=CARTESIAN_POINT('Ctrl Pts',(109.032510608047,21.9222359168897,33.3005483021895));
#105614=CARTESIAN_POINT('Ctrl Pts',(109.034659235571,21.903646654048,33.0193718835565));
#105615=CARTESIAN_POINT('Ctrl Pts',(109.164161685767,21.8850573912062,32.7359196687374));
#105616=CARTESIAN_POINT('Ctrl Pts',(109.37993974096,21.8664681283645,32.5559234520905));
#105617=CARTESIAN_POINT('Ctrl Pts',(109.625213459164,21.8453378164253,32.3513227512442));
#105618=CARTESIAN_POINT('Ctrl Pts',(109.981961667339,21.8242075044861,32.2803948844628));
#105619=CARTESIAN_POINT('Ctrl Pts',(110.287104459141,21.8030771925468,32.3751482824717));
#105620=CARTESIAN_POINT('Ctrl Pts',(110.592247250944,21.7819468806076,32.4699016804807));
#105621=CARTESIAN_POINT('Ctrl Pts',(110.845784626375,21.7608165686683,32.7303363432799));
#105622=CARTESIAN_POINT('Ctrl Pts',(110.932233234354,21.7396862567291,33.0378396653247));
#105623=CARTESIAN_POINT('Ctrl Pts',(111.018681842333,21.7185559447898,33.3453429873695));
#105624=CARTESIAN_POINT('Ctrl Pts',(110.93804168286,21.6974256328506,33.6999149686599));
#105625=CARTESIAN_POINT('Ctrl Pts',(110.727018157058,21.6762953209113,33.9397490113778));
#105626=CARTESIAN_POINT('Ctrl Pts',(110.515994631257,21.6551650089721,34.1795830540957));
#105627=CARTESIAN_POINT('Ctrl Pts',(110.174587739126,21.6340346970328,34.3046791582411));
#105628=CARTESIAN_POINT('Ctrl Pts',(109.858555314241,21.6129043850936,34.2580160922735));
#105629=CARTESIAN_POINT('Ctrl Pts',(109.542522889355,21.5917740731543,34.211353026306));
#105630=CARTESIAN_POINT('Ctrl Pts',(109.251864931714,21.5706437612151,33.9929307902253));
#105631=CARTESIAN_POINT('Ctrl Pts',(109.119139823187,21.5495134492758,33.702358702714));
#105632=CARTESIAN_POINT('Ctrl Pts',(109.062027344887,21.5404209384805,33.5773236417016));
#105633=CARTESIAN_POINT('Ctrl Pts',(109.034158296165,21.5313284276851,33.4389290477532));
#105634=CARTESIAN_POINT('Ctrl Pts',(109.034617182386,21.5222359168897,33.300357734449));
#105635=CARTESIAN_POINT('Origin',(110.,21.33,33.3));
#105636=CARTESIAN_POINT('',(109.03353070876,21.0642640831103,33.2991467029023));
#105637=CARTESIAN_POINT('',(109.033423686584,21.1222359168897,33.299130763016));
#105638=CARTESIAN_POINT('',(109.03325,21.33,33.3));
#105639=CARTESIAN_POINT('Ctrl Pts',(109.03353070876,21.0642640831103,33.2991467029023));
#105640=CARTESIAN_POINT('Ctrl Pts',(109.035565999728,21.079671572315,33.5332918739583));
#105641=CARTESIAN_POINT('Ctrl Pts',(109.121178897119,21.0950790615196,33.7687652483135));
#105642=CARTESIAN_POINT('Ctrl Pts',(109.275829590741,21.1104865507242,33.9429499406045));
#105643=CARTESIAN_POINT('Ctrl Pts',(109.487922382399,21.1316168626634,34.1818322681708));
#105644=CARTESIAN_POINT('Ctrl Pts',(109.829863092622,21.1527471746027,34.3054413942131));
#105645=CARTESIAN_POINT('Ctrl Pts',(110.145681380272,21.1738774865419,34.2573863849353));
#105646=CARTESIAN_POINT('Ctrl Pts',(110.461499667922,21.1950077984812,34.2093313756574));
#105647=CARTESIAN_POINT('Ctrl Pts',(110.751195532998,21.2161381104204,33.9896122310594));
#105648=CARTESIAN_POINT('Ctrl Pts',(110.882634883733,21.2372684223596,33.6984520452764));
#105649=CARTESIAN_POINT('Ctrl Pts',(111.014074234468,21.2583987342989,33.4072918594934));
#105650=CARTESIAN_POINT('Ctrl Pts',(110.987257070861,21.2795290462381,33.0446906325254));
#105651=CARTESIAN_POINT('Ctrl Pts',(110.814414356613,21.3006593581774,32.7760358858918));
#105652=CARTESIAN_POINT('Ctrl Pts',(110.641571642365,21.3217896701166,32.5073811392581));
#105653=CARTESIAN_POINT('Ctrl Pts',(110.322703377475,21.3429199820559,32.3326728729586));
#105654=CARTESIAN_POINT('Ctrl Pts',(110.003252067877,21.3640502939951,32.3315998746245));
#105655=CARTESIAN_POINT('Ctrl Pts',(109.683800758279,21.3851806059344,32.3305268762904));
#105656=CARTESIAN_POINT('Ctrl Pts',(109.363766403974,21.4063109178736,32.5030891459216));
#105657=CARTESIAN_POINT('Ctrl Pts',(109.189123176412,21.4274412298128,32.7705775262224));
#105658=CARTESIAN_POINT('Ctrl Pts',(109.087675518873,21.4397155142453,32.92595755429));
#105659=CARTESIAN_POINT('Ctrl Pts',(109.035286834209,21.4519897986778,33.1133682680862));
#105660=CARTESIAN_POINT('Ctrl Pts',(109.034572229009,21.4642640831103,33.3004087423462));
#105661=CARTESIAN_POINT('Ctrl Pts',(109.034617182386,21.5222359168897,33.300357734449));
#105662=CARTESIAN_POINT('Ctrl Pts',(109.035224713264,21.5101981157458,33.1168997269377));
#105663=CARTESIAN_POINT('Ctrl Pts',(109.085484798468,21.498160314602,32.9331319697948));
#105664=CARTESIAN_POINT('Ctrl Pts',(109.183272991379,21.4861225134581,32.7796457768268));
#105665=CARTESIAN_POINT('Ctrl Pts',(109.354923527512,21.4649922015189,32.510226877393));
#105666=CARTESIAN_POINT('Ctrl Pts',(109.67301685919,21.4438618895796,32.3341110174673));
#105667=CARTESIAN_POINT('Ctrl Pts',(109.992460670067,21.4227315776404,32.3316244033515));
#105668=CARTESIAN_POINT('Ctrl Pts',(110.311904480944,21.4016012657011,32.3291377892357));
#105669=CARTESIAN_POINT('Ctrl Pts',(110.632698771019,21.3804709537619,32.5002804209298));
#105670=CARTESIAN_POINT('Ctrl Pts',(110.808524459441,21.3593406418227,32.7669923979043));
#105671=CARTESIAN_POINT('Ctrl Pts',(110.984350147864,21.3382103298834,33.0337043748788));
#105672=CARTESIAN_POINT('Ctrl Pts',(111.015207234633,21.3170800179441,33.3959856971337));
#105673=CARTESIAN_POINT('Ctrl Pts',(110.887020531404,21.2959497060049,33.6885919760826));
#105674=CARTESIAN_POINT('Ctrl Pts',(110.758833828174,21.2748193940657,33.9811982550316));
#105675=CARTESIAN_POINT('Ctrl Pts',(110.471603334946,21.2536890821264,34.2041294906745));
#105676=CARTESIAN_POINT('Ctrl Pts',(110.15634071544,21.2325587701872,34.2557022170651));
#105677=CARTESIAN_POINT('Ctrl Pts',(109.841078095934,21.2114284582479,34.3072749434557));
#105678=CARTESIAN_POINT('Ctrl Pts',(109.49778335015,21.1902981463087,34.1874891605939));
#105679=CARTESIAN_POINT('Ctrl Pts',(109.283040527393,21.1691678343694,33.9509823500262));
#105680=CARTESIAN_POINT('Ctrl Pts',(109.124054194299,21.1535238618762,33.7758828981285));
#105681=CARTESIAN_POINT('Ctrl Pts',(109.035530815549,21.1378798893829,33.5368053411001));
#105682=CARTESIAN_POINT('Ctrl Pts',(109.033423686584,21.1222359168897,33.299130763016));
#105683=CARTESIAN_POINT('Origin',(110.,21.33,33.3));
#105684=CARTESIAN_POINT('',(109.03325,20.66675,33.3));
#105685=CARTESIAN_POINT('',(109.031713168497,20.7222359168897,33.3003348740849));
#105686=CARTESIAN_POINT('',(109.03325,21.33,33.3));
#105687=CARTESIAN_POINT('',(109.033986956687,20.66675,33.3377407293226));
#105688=CARTESIAN_POINT('Origin',(110.,20.66675,33.3));
#105689=CARTESIAN_POINT('Ctrl Pts',(109.033986956687,20.66675,33.3377407293226));
#105690=CARTESIAN_POINT('Ctrl Pts',(109.046513639301,20.6878803119393,33.6583741407962));
#105691=CARTESIAN_POINT('Ctrl Pts',(109.231527122784,20.7090106238785,33.9695692430953));
#105692=CARTESIAN_POINT('Ctrl Pts',(109.505777853249,20.7301409358178,34.1323692963055));
#105693=CARTESIAN_POINT('Ctrl Pts',(109.780028583713,20.751271247757,34.2951693495157));
#105694=CARTESIAN_POINT('Ctrl Pts',(110.143516561158,20.7724015596962,34.3095743536369));
#105695=CARTESIAN_POINT('Ctrl Pts',(110.429820581278,20.7935318716355,34.1679742283488));
#105696=CARTESIAN_POINT('Ctrl Pts',(110.716124601398,20.8146621835747,34.0263741030606));
#105697=CARTESIAN_POINT('Ctrl Pts',(110.925244664191,20.835792495514,33.728768848363));
#105698=CARTESIAN_POINT('Ctrl Pts',(110.961965060678,20.8569228074532,33.4113700988134));
#105699=CARTESIAN_POINT('Ctrl Pts',(110.998685457165,20.8780531193925,33.0939713492637));
#105700=CARTESIAN_POINT('Ctrl Pts',(110.863006187345,20.8991834313317,32.7567791048619));
#105701=CARTESIAN_POINT('Ctrl Pts',(110.616716338203,20.920313743271,32.553375562571));
#105702=CARTESIAN_POINT('Ctrl Pts',(110.37042648906,20.9414440552102,32.3499720202801));
#105703=CARTESIAN_POINT('Ctrl Pts',(110.013526060595,20.9625743671494,32.2803571801001));
#105704=CARTESIAN_POINT('Ctrl Pts',(109.708846083157,20.9837046790887,32.3763854624997));
#105705=CARTESIAN_POINT('Ctrl Pts',(109.404166105719,21.0048349910279,32.4724137448993));
#105706=CARTESIAN_POINT('Ctrl Pts',(109.151706579308,21.0259653029672,32.7340851498784));
#105707=CARTESIAN_POINT('Ctrl Pts',(109.066599252649,21.0470956149064,33.0419986169131));
#105708=CARTESIAN_POINT('Ctrl Pts',(109.043549231178,21.0528184376411,33.1253922835335));
#105709=CARTESIAN_POINT('Ctrl Pts',(109.032774738123,21.0585412603757,33.2121778729827));
#105710=CARTESIAN_POINT('Ctrl Pts',(109.03353070876,21.0642640831103,33.2991467029023));
#105711=CARTESIAN_POINT('Ctrl Pts',(109.033423686584,21.1222359168897,33.299130763016));
#105712=CARTESIAN_POINT('Ctrl Pts',(109.032684716686,21.1167495774437,33.2157783144218));
#105713=CARTESIAN_POINT('Ctrl Pts',(109.042574117077,21.1112632379977,33.132598418788));
#105714=CARTESIAN_POINT('Ctrl Pts',(109.063779996857,21.1057768985517,33.0524111404063));
#105715=CARTESIAN_POINT('Ctrl Pts',(109.14545318881,21.0846465866125,32.7435745796278));
#105716=CARTESIAN_POINT('Ctrl Pts',(109.394990472447,21.0635162746732,32.4791292963446));
#105717=CARTESIAN_POINT('Ctrl Pts',(109.698575654323,21.042385962734,32.379698479835));
#105718=CARTESIAN_POINT('Ctrl Pts',(110.0021608362,21.0212556507947,32.2802676633254));
#105719=CARTESIAN_POINT('Ctrl Pts',(110.359793916316,21.0001253388555,32.3458513135895));
#105720=CARTESIAN_POINT('Ctrl Pts',(110.608345300104,20.9789950269162,32.5465259310458));
#105721=CARTESIAN_POINT('Ctrl Pts',(110.856896683892,20.957864714977,32.7472005485021));
#105722=CARTESIAN_POINT('Ctrl Pts',(110.996366371352,20.9367344030377,33.0829661331506));
#105723=CARTESIAN_POINT('Ctrl Pts',(110.963152234546,20.9156040910985,33.4006936208202));
#105724=CARTESIAN_POINT('Ctrl Pts',(110.92993809774,20.8944737791592,33.7184211084898));
#105725=CARTESIAN_POINT('Ctrl Pts',(110.724040136667,20.87334346722,34.0181104991805));
#105726=CARTESIAN_POINT('Ctrl Pts',(110.439344866371,20.8522131552808,34.1630239200884));
#105727=CARTESIAN_POINT('Ctrl Pts',(110.154649596075,20.8310828433415,34.3079373409964));
#105728=CARTESIAN_POINT('Ctrl Pts',(109.791157016555,20.8099525314023,34.2980747921216));
#105729=CARTESIAN_POINT('Ctrl Pts',(109.51472120639,20.788822219463,34.1380282434287));
#105730=CARTESIAN_POINT('Ctrl Pts',(109.238285396225,20.7676919075238,33.9779816947357));
#105731=CARTESIAN_POINT('Ctrl Pts',(109.048906355415,20.7465615955845,33.6677511462246));
#105732=CARTESIAN_POINT('Ctrl Pts',(109.032832060182,20.7254312836453,33.3486399636312));
#105733=CARTESIAN_POINT('Ctrl Pts',(109.032021798148,20.7243661613934,33.3325544263057));
#105734=CARTESIAN_POINT('Ctrl Pts',(109.03165188566,20.7233010391415,33.3164463242016));
#105735=CARTESIAN_POINT('Ctrl Pts',(109.031713168497,20.7222359168897,33.3003348740849));
#105736=CARTESIAN_POINT('Origin',(110.,22.7327725593024,33.3));
#105737=CARTESIAN_POINT('',(109.261214578509,20.9327725593024,33.2993477253114));
#105738=CARTESIAN_POINT('',(109.259825220088,20.8537274406976,33.3002559833966));
#105739=CARTESIAN_POINT('',(109.261,22.7327725593024,33.3));
#105740=CARTESIAN_POINT('',(110.376335103234,20.66675,33.9374365499136));
#105741=CARTESIAN_POINT('Ctrl Pts',(109.261214578509,20.9327725593024,33.2993477253114));
#105742=CARTESIAN_POINT('Ctrl Pts',(109.260636701808,20.9270497365678,33.2328672853729));
#105743=CARTESIAN_POINT('Ctrl Pts',(109.299283346943,20.9001966018939,32.9215791476215));
#105744=CARTESIAN_POINT('Ctrl Pts',(109.737518843697,20.8522131552808,32.4673530790804));
#105745=CARTESIAN_POINT('Ctrl Pts',(110.555980958936,20.788822219463,32.6269973518284));
#105746=CARTESIAN_POINT('Ctrl Pts',(110.859421941756,20.7270011677028,33.3811136304354));
#105747=CARTESIAN_POINT('Ctrl Pts',(110.570443245433,20.6863104278818,33.8213655281161));
#105748=CARTESIAN_POINT('Ctrl Pts',(110.376335103234,20.66675,33.9374365499136));
#105749=CARTESIAN_POINT('',(110.723592507189,20.66675,33.1498837665692));
#105750=CARTESIAN_POINT('Origin',(110.,20.66675,33.3));
#105751=CARTESIAN_POINT('Ctrl Pts',(109.259825220088,20.8537274406976,33.3002559833966));
#105752=CARTESIAN_POINT('Ctrl Pts',(109.260707716465,20.8336622510103,33.0682449168145));
#105753=CARTESIAN_POINT('Ctrl Pts',(109.502678324612,20.7924667493836,32.590042208654));
#105754=CARTESIAN_POINT('Ctrl Pts',(110.316393411479,20.7301409358178,32.4870507258606));
#105755=CARTESIAN_POINT('Ctrl Pts',(110.6737668031,20.6878803119393,32.9097131646266));
#105756=CARTESIAN_POINT('Ctrl Pts',(110.723592507189,20.66675,33.1498837665692));
#105757=CARTESIAN_POINT('Origin',(110.,22.7327725593024,33.3));
#105758=CARTESIAN_POINT('',(109.262010734148,21.3327725593024,33.3003124495411));
#105759=CARTESIAN_POINT('',(109.261132768953,21.2537274406976,33.2993355405936));
#105760=CARTESIAN_POINT('',(109.261,22.7327725593024,33.3));
#105761=CARTESIAN_POINT('Ctrl Pts',(109.262010734148,21.3327725593024,33.3003124495411));
#105762=CARTESIAN_POINT('Ctrl Pts',(109.262556990412,21.3204982748699,33.1573355573992));
#105763=CARTESIAN_POINT('Ctrl Pts',(109.371544768259,21.2870936784982,32.7674521813911));
#105764=CARTESIAN_POINT('Ctrl Pts',(110.002931624722,21.2325587701872,32.4270088899107));
#105765=CARTESIAN_POINT('Ctrl Pts',(110.734176458714,21.1691678343694,32.8276587232552));
#105766=CARTESIAN_POINT('Ctrl Pts',(110.795674934758,21.1057768985517,33.6591941979777));
#105767=CARTESIAN_POINT('Ctrl Pts',(110.131329723613,21.042385962734,34.1630652541699));
#105768=CARTESIAN_POINT('Ctrl Pts',(109.417966198001,20.9847178496509,33.9051894315055));
#105769=CARTESIAN_POINT('Ctrl Pts',(109.262770389241,20.948180048507,33.4783322418983));
#105770=CARTESIAN_POINT('Ctrl Pts',(109.261214578509,20.9327725593024,33.2993477253114));
#105771=CARTESIAN_POINT('Ctrl Pts',(109.261132768953,21.2537274406976,33.2993355405936));
#105772=CARTESIAN_POINT('Ctrl Pts',(109.260567887903,21.2482411012516,33.2356195235146));
#105773=CARTESIAN_POINT('Ctrl Pts',(109.297242958642,21.2216244498664,32.9271449511855));
#105774=CARTESIAN_POINT('Ctrl Pts',(109.728271023269,21.1738774865419,32.4703661604886));
#105775=CARTESIAN_POINT('Ctrl Pts',(110.548413292333,21.1104865507242,32.6207659046162));
#105776=CARTESIAN_POINT('Ctrl Pts',(110.868252234251,21.0470956149064,33.3907605269755));
#105777=CARTESIAN_POINT('Ctrl Pts',(110.39607661522,20.9837046790887,34.0780233965501));
#105778=CARTESIAN_POINT('Ctrl Pts',(109.56249704574,20.9203137432709,34.0554061006045));
#105779=CARTESIAN_POINT('Ctrl Pts',(109.265670790959,20.8769879971406,33.5691613111105));
#105780=CARTESIAN_POINT('Ctrl Pts',(109.259778374454,20.8547925629495,33.3125718475149));
#105781=CARTESIAN_POINT('Ctrl Pts',(109.259825220088,20.8537274406976,33.3002559833966));
#105782=CARTESIAN_POINT('Origin',(110.,22.7327725593024,33.3));
#105783=CARTESIAN_POINT('',(109.260096259818,21.7327725593024,33.3004698838673));
#105784=CARTESIAN_POINT('',(109.262045097267,21.6537274406976,33.3002734582445));
#105785=CARTESIAN_POINT('',(109.261,22.7327725593024,33.3));
#105786=CARTESIAN_POINT('Ctrl Pts',(109.260096259818,21.7327725593024,33.3004698838673));
#105787=CARTESIAN_POINT('Ctrl Pts',(109.261654463222,21.713946813172,33.0826444252441));
#105788=CARTESIAN_POINT('Ctrl Pts',(109.478357859312,21.6739907551024,32.6175592866656));
#105789=CARTESIAN_POINT('Ctrl Pts',(110.268062035357,21.6129043850936,32.4691917393687));
#105790=CARTESIAN_POINT('Ctrl Pts',(110.842979873719,21.5495134492758,33.0730612101061));
#105791=CARTESIAN_POINT('Ctrl Pts',(110.648917258071,21.4861225134581,33.8839824667209));
#105792=CARTESIAN_POINT('Ctrl Pts',(109.86287719836,21.4227315776404,34.1621579965021));
#105793=CARTESIAN_POINT('Ctrl Pts',(109.329908345882,21.3716149262551,33.7522685476019));
#105794=CARTESIAN_POINT('Ctrl Pts',(109.261616604411,21.3416285868091,33.4034718065368));
#105795=CARTESIAN_POINT('Ctrl Pts',(109.262010734148,21.3327725593024,33.3003124495411));
#105796=CARTESIAN_POINT('Ctrl Pts',(109.262045097267,21.6537274406976,33.3002734582445));
#105797=CARTESIAN_POINT('Ctrl Pts',(109.262509504114,21.6416896395538,33.1600350640879));
#105798=CARTESIAN_POINT('Ctrl Pts',(109.36836833146,21.6085215264707,32.7729796264293));
#105799=CARTESIAN_POINT('Ctrl Pts',(109.993204480012,21.5542231014483,32.4270322435203));
#105800=CARTESIAN_POINT('Ctrl Pts',(110.72886617238,21.4908321656306,32.8195051832315));
#105801=CARTESIAN_POINT('Ctrl Pts',(110.799629204568,21.4274412298128,33.6503070362846));
#105802=CARTESIAN_POINT('Ctrl Pts',(110.140937708849,21.3640502939951,34.1615442221346));
#105803=CARTESIAN_POINT('Ctrl Pts',(109.421812448308,21.3061456976234,33.9106199555457));
#105804=CARTESIAN_POINT('Ctrl Pts',(109.262743493862,21.2693714131909,33.4810179954207));
#105805=CARTESIAN_POINT('Ctrl Pts',(109.261132768953,21.2537274406976,33.2993355405936));
#105806=CARTESIAN_POINT('Origin',(110.,20.66675,33.3));
#105807=CARTESIAN_POINT('Ctrl Pts',(110.376335103234,20.66675,33.9374365499136));
#105808=CARTESIAN_POINT('Ctrl Pts',(110.362051118216,20.66675,33.9491714998516));
#105809=CARTESIAN_POINT('Ctrl Pts',(110.347327113967,20.66675,33.9603101779496));
#105810=CARTESIAN_POINT('Ctrl Pts',(110.33218889002,20.66675,33.9708180297552));
#105811=CARTESIAN_POINT('Ctrl Pts',(110.304729416617,20.66675,33.9898783949733));
#105812=CARTESIAN_POINT('Ctrl Pts',(110.275909391602,20.66675,34.0068653774463));
#105813=CARTESIAN_POINT('Ctrl Pts',(110.245983179273,20.66675,34.0218215741852));
#105814=CARTESIAN_POINT('Ctrl Pts',(110.233763985821,20.66675,34.0279283497184));
#105815=CARTESIAN_POINT('Ctrl Pts',(110.221359914847,20.66675,34.0336962029393));
#105816=CARTESIAN_POINT('Ctrl Pts',(110.208786594842,20.66675,34.0391264878303));
#105817=CARTESIAN_POINT('Ctrl Pts',(110.201157085926,20.66675,34.042421592622));
#105818=CARTESIAN_POINT('Ctrl Pts',(110.19346825675,20.66675,34.0455909818006));
#105819=CARTESIAN_POINT('Ctrl Pts',(110.185731523892,20.66675,34.0486322638215));
#105820=CARTESIAN_POINT('Ctrl Pts',(110.152517375499,20.66675,34.0616886267858));
#105821=CARTESIAN_POINT('Ctrl Pts',(110.118382926888,20.66675,34.0724046024287));
#105822=CARTESIAN_POINT('Ctrl Pts',(110.083616565184,20.66675,34.080825390986));
#105823=CARTESIAN_POINT('Ctrl Pts',(110.058360083766,20.66675,34.0869427837557));
#105824=CARTESIAN_POINT('Ctrl Pts',(110.03276907629,20.66675,34.0918481845548));
#105825=CARTESIAN_POINT('Ctrl Pts',(110.006943547618,20.66675,34.0955457613206));
#105826=CARTESIAN_POINT('Ctrl Pts',(109.999025934563,20.66675,34.0966793676233));
#105827=CARTESIAN_POINT('Ctrl Pts',(109.991089910533,20.66675,34.0976987562079));
#105828=CARTESIAN_POINT('Ctrl Pts',(109.983146762188,20.66675,34.0986034204503));
#105829=CARTESIAN_POINT('Ctrl Pts',(109.945618729961,20.66675,34.1028775781728));
#105830=CARTESIAN_POINT('Ctrl Pts',(109.907880244829,20.66675,34.1046023075043));
#105831=CARTESIAN_POINT('Ctrl Pts',(109.870239318907,20.66675,34.1038241003379));
#105832=CARTESIAN_POINT('Ctrl Pts',(109.83232030645,20.66675,34.1030401438725));
#105833=CARTESIAN_POINT('Ctrl Pts',(109.794498983599,20.66675,34.0997165237621));
#105834=CARTESIAN_POINT('Ctrl Pts',(109.757066157873,20.66675,34.0938532556067));
#105835=CARTESIAN_POINT('Ctrl Pts',(109.737844223589,20.66675,34.0908424394849));
#105836=CARTESIAN_POINT('Ctrl Pts',(109.718724464461,20.66675,34.0871611482163));
#105837=CARTESIAN_POINT('Ctrl Pts',(109.69974559798,20.66675,34.0828040554303));
#105838=CARTESIAN_POINT('Ctrl Pts',(109.690444770713,20.66675,34.0806688084476));
#105839=CARTESIAN_POINT('Ctrl Pts',(109.681175436593,20.66675,34.0783703804502));
#105840=CARTESIAN_POINT('Ctrl Pts',(109.671964996317,20.66675,34.0759144833926));
#105841=CARTESIAN_POINT('Ctrl Pts',(109.634271818598,20.66675,34.0658638711018));
#105842=CARTESIAN_POINT('Ctrl Pts',(109.597484896717,20.66675,34.0531628165186));
#105843=CARTESIAN_POINT('Ctrl Pts',(109.561907952814,20.66675,34.0378349421013));
#105844=CARTESIAN_POINT('Ctrl Pts',(109.527210364415,20.66675,34.0228859268347));
#105845=CARTESIAN_POINT('Ctrl Pts',(109.493662072607,20.66675,34.0054388458726));
#105846=CARTESIAN_POINT('Ctrl Pts',(109.461373044813,20.66675,33.985736470523));
#105847=CARTESIAN_POINT('Ctrl Pts',(109.446367008596,20.66675,33.9765799681977));
#105848=CARTESIAN_POINT('Ctrl Pts',(109.431633085047,20.66675,33.9669356125781));
#105849=CARTESIAN_POINT('Ctrl Pts',(109.417183333681,20.66675,33.9568241627759));
#105850=CARTESIAN_POINT('Ctrl Pts',(109.409788076771,20.66675,33.9516492108251));
#105851=CARTESIAN_POINT('Ctrl Pts',(109.402467266531,20.66675,33.946351878214));
#105852=CARTESIAN_POINT('Ctrl Pts',(109.39522261568,20.66675,33.9409347405269));
#105853=CARTESIAN_POINT('Ctrl Pts',(109.389483833801,20.66675,33.9366436059738));
#105854=CARTESIAN_POINT('Ctrl Pts',(109.383794686831,20.66675,33.9322785792095));
#105855=CARTESIAN_POINT('Ctrl Pts',(109.378162977365,20.66675,33.9278468206238));
#105856=CARTESIAN_POINT('Ctrl Pts',(109.347071246258,20.66675,33.9033798187109));
#105857=CARTESIAN_POINT('Ctrl Pts',(109.317666910692,20.66675,33.8768368840104));
#105858=CARTESIAN_POINT('Ctrl Pts',(109.290062958723,20.66675,33.848495844236));
#105859=CARTESIAN_POINT('Ctrl Pts',(109.261797091972,20.66675,33.8194752150602));
#105860=CARTESIAN_POINT('Ctrl Pts',(109.235418059424,20.66675,33.7885686279158));
#105861=CARTESIAN_POINT('Ctrl Pts',(109.211065944257,20.66675,33.7560230457913));
#105862=CARTESIAN_POINT('Ctrl Pts',(109.199623874339,20.66675,33.7407311985079));
#105863=CARTESIAN_POINT('Ctrl Pts',(109.188629635713,20.66675,33.7250768436632));
#105864=CARTESIAN_POINT('Ctrl Pts',(109.17810006173,20.66675,33.709082429934));
#105865=CARTESIAN_POINT('Ctrl Pts',(109.17231735898,20.66675,33.7002985094835));
#105866=CARTESIAN_POINT('Ctrl Pts',(109.166674831446,20.66675,33.6914119930594));
#105867=CARTESIAN_POINT('Ctrl Pts',(109.161175505246,20.66675,33.6824263847011));
#105868=CARTESIAN_POINT('Ctrl Pts',(109.156958433143,20.66675,33.6755359117666));
#105869=CARTESIAN_POINT('Ctrl Pts',(109.152828330105,20.66675,33.6685915480918));
#105870=CARTESIAN_POINT('Ctrl Pts',(109.148789996522,20.66675,33.661601815363));
#105871=CARTESIAN_POINT('Ctrl Pts',(109.127615458512,20.66675,33.6249519551497));
#105872=CARTESIAN_POINT('Ctrl Pts',(109.108928594472,20.66675,33.5870044942501));
#105873=CARTESIAN_POINT('Ctrl Pts',(109.092867816801,20.66675,33.548034950299));
#105874=CARTESIAN_POINT('Ctrl Pts',(109.076912664157,20.66675,33.5093216927643));
#105875=CARTESIAN_POINT('Ctrl Pts',(109.063548303014,20.66675,33.4695987840075));
#105876=CARTESIAN_POINT('Ctrl Pts',(109.052944594755,20.66675,33.4290994676753));
#105877=CARTESIAN_POINT('Ctrl Pts',(109.045075862302,20.66675,33.3990459923237));
#105878=CARTESIAN_POINT('Ctrl Pts',(109.038727971098,20.66675,33.368564132549));
#105879=CARTESIAN_POINT('Ctrl Pts',(109.033986956687,20.66675,33.3377407293226));
#105880=CARTESIAN_POINT('',(109.377034789147,20.66675,32.5586406032643));
#105881=CARTESIAN_POINT('Origin',(110.,20.66675,33.3));
#105882=CARTESIAN_POINT('Ctrl Pts',(109.377024795358,20.66675,32.5586208180317));
#105883=CARTESIAN_POINT('Ctrl Pts',(109.396809806408,20.66675,32.5453690358772));
#105884=CARTESIAN_POINT('Ctrl Pts',(109.417086018765,20.66675,32.5329219386122));
#105885=CARTESIAN_POINT('Ctrl Pts',(109.437834479318,20.66675,32.521328234985));
#105886=CARTESIAN_POINT('Ctrl Pts',(109.470704923652,20.66675,32.5029610800471));
#105887=CARTESIAN_POINT('Ctrl Pts',(109.504760685105,20.66675,32.4867341891181));
#105888=CARTESIAN_POINT('Ctrl Pts',(109.53977975488,20.66675,32.472656252588));
#105889=CARTESIAN_POINT('Ctrl Pts',(109.559613981063,20.66675,32.4646827404667));
#105890=CARTESIAN_POINT('Ctrl Pts',(109.57975732631,20.66675,32.4573991898274));
#105891=CARTESIAN_POINT('Ctrl Pts',(109.600169285294,20.66675,32.4508117735884));
#105892=CARTESIAN_POINT('Ctrl Pts',(109.609416808786,20.66675,32.4478273816213));
#105893=CARTESIAN_POINT('Ctrl Pts',(109.618717903772,20.66675,32.4449865447394));
#105894=CARTESIAN_POINT('Ctrl Pts',(109.628057331603,20.66675,32.4422928045765));
#105895=CARTESIAN_POINT('Ctrl Pts',(109.66815554816,20.66675,32.4307274090985));
#105896=CARTESIAN_POINT('Ctrl Pts',(109.709018022693,20.66675,32.4218504694604));
#105897=CARTESIAN_POINT('Ctrl Pts',(109.75033803836,20.66675,32.4156791778283));
#105898=CARTESIAN_POINT('Ctrl Pts',(109.774132683495,20.66675,32.4121253627575));
#105899=CARTESIAN_POINT('Ctrl Pts',(109.798079053289,20.66675,32.4094697570998));
#105900=CARTESIAN_POINT('Ctrl Pts',(109.822116736403,20.66675,32.4077233113639));
#105901=CARTESIAN_POINT('Ctrl Pts',(109.832278466539,20.66675,32.4069850159889));
#105902=CARTESIAN_POINT('Ctrl Pts',(109.842456487862,20.66675,32.4064092642038));
#105903=CARTESIAN_POINT('Ctrl Pts',(109.852646091747,20.66675,32.4059971752793));
#105904=CARTESIAN_POINT('Ctrl Pts',(109.861010040807,20.66675,32.4056589196601));
#105905=CARTESIAN_POINT('Ctrl Pts',(109.869372278937,20.66675,32.4054313258998));
#105906=CARTESIAN_POINT('Ctrl Pts',(109.877729756577,20.66675,32.4053143381012));
#105907=CARTESIAN_POINT('Ctrl Pts',(109.91781820896,20.66675,32.4047531807764));
#105908=CARTESIAN_POINT('Ctrl Pts',(109.957802808996,20.66675,32.406732837445));
#105909=CARTESIAN_POINT('Ctrl Pts',(109.997408074228,20.66675,32.41127414139));
#105910=CARTESIAN_POINT('Ctrl Pts',(110.03608830874,20.66675,32.4157093774766));
#105911=CARTESIAN_POINT('Ctrl Pts',(110.074407739332,20.66675,32.4225883582893));
#105912=CARTESIAN_POINT('Ctrl Pts',(110.112088050043,20.66675,32.4319736180715));
#105913=CARTESIAN_POINT('Ctrl Pts',(110.1299959605,20.66675,32.4364340481643));
#105914=CARTESIAN_POINT('Ctrl Pts',(110.147759098548,20.66675,32.4414611782776));
#105915=CARTESIAN_POINT('Ctrl Pts',(110.165344832615,20.66675,32.4470649103973));
#105916=CARTESIAN_POINT('Ctrl Pts',(110.173110216502,20.66675,32.4495393667345));
#105917=CARTESIAN_POINT('Ctrl Pts',(110.180840981897,20.66675,32.4521262789321));
#105918=CARTESIAN_POINT('Ctrl Pts',(110.188534182193,20.66675,32.4548266220958));
#105919=CARTESIAN_POINT('Ctrl Pts',(110.196113058415,20.66675,32.457486837066));
#105920=CARTESIAN_POINT('Ctrl Pts',(110.203647475052,20.66675,32.4602543667076));
#105921=CARTESIAN_POINT('Ctrl Pts',(110.211131498076,20.66675,32.4631281412987));
#105922=CARTESIAN_POINT('Ctrl Pts',(110.24432115308,20.66675,32.4758725685853));
#105923=CARTESIAN_POINT('Ctrl Pts',(110.276544706183,20.66675,32.4907119074751));
#105924=CARTESIAN_POINT('Ctrl Pts',(110.307588054684,20.66675,32.507684733064));
#105925=CARTESIAN_POINT('Ctrl Pts',(110.33659439538,20.66675,32.5235438328514));
#105926=CARTESIAN_POINT('Ctrl Pts',(110.364570383607,20.66675,32.5412666417595));
#105927=CARTESIAN_POINT('Ctrl Pts',(110.391403599684,20.66675,32.5607050382317));
#105928=CARTESIAN_POINT('Ctrl Pts',(110.405014168788,20.66675,32.5705647448612));
#105929=CARTESIAN_POINT('Ctrl Pts',(110.418330348652,20.66675,32.5808661044064));
#105930=CARTESIAN_POINT('Ctrl Pts',(110.43133494341,20.66675,32.5915910088429));
#105931=CARTESIAN_POINT('Ctrl Pts',(110.440046433796,20.66675,32.5987753851059));
#105932=CARTESIAN_POINT('Ctrl Pts',(110.448618068475,20.66675,32.6061498360859));
#105933=CARTESIAN_POINT('Ctrl Pts',(110.457044207542,20.66675,32.6137090329155));
#105934=CARTESIAN_POINT('Ctrl Pts',(110.46402254411,20.66675,32.6199693876567));
#105935=CARTESIAN_POINT('Ctrl Pts',(110.470902598729,20.66675,32.6263581673401));
#105936=CARTESIAN_POINT('Ctrl Pts',(110.477664901628,20.66675,32.6328561811291));
#105937=CARTESIAN_POINT('Ctrl Pts',(110.504570931299,20.66675,32.658710650293));
#105938=CARTESIAN_POINT('Ctrl Pts',(110.52967598653,20.66675,32.6863438203501));
#105939=CARTESIAN_POINT('Ctrl Pts',(110.55282817067,20.66675,32.715530046899));
#105940=CARTESIAN_POINT('Ctrl Pts',(110.575716238353,20.66675,32.7443833215888));
#105941=CARTESIAN_POINT('Ctrl Pts',(110.596696157522,20.66675,32.7747556685919));
#105942=CARTESIAN_POINT('Ctrl Pts',(110.6155730175,20.66675,32.8064437120442));
#105943=CARTESIAN_POINT('Ctrl Pts',(110.624095911369,20.66675,32.8207508495441));
#105944=CARTESIAN_POINT('Ctrl Pts',(110.632189398688,20.66675,32.83532628065));
#105945=CARTESIAN_POINT('Ctrl Pts',(110.639831931783,20.66675,32.85015126595));
#105946=CARTESIAN_POINT('Ctrl Pts',(110.643387138242,20.66675,32.8570476552539));
#105947=CARTESIAN_POINT('Ctrl Pts',(110.646845565571,20.66675,32.8639998037261));
#105948=CARTESIAN_POINT('Ctrl Pts',(110.650202196263,20.66675,32.8710002002437));
#105949=CARTESIAN_POINT('Ctrl Pts',(110.665521542891,20.66675,32.9029493512352));
#105950=CARTESIAN_POINT('Ctrl Pts',(110.67866190767,20.66675,32.9357692553209));
#105951=CARTESIAN_POINT('Ctrl Pts',(110.689468386051,20.66675,32.9692696922969));
#105952=CARTESIAN_POINT('Ctrl Pts',(110.699880421221,20.66675,33.0015473423944));
#105953=CARTESIAN_POINT('Ctrl Pts',(110.70812586013,20.66675,33.0344577142209));
#105954=CARTESIAN_POINT('Ctrl Pts',(110.714018973751,20.66675,33.0678288587027));
#105955=CARTESIAN_POINT('Ctrl Pts',(110.718801298005,20.66675,33.09490989666));
#105956=CARTESIAN_POINT('Ctrl Pts',(110.722033682588,20.66675,33.1222945339637));
#105957=CARTESIAN_POINT('Ctrl Pts',(110.723592507189,20.66675,33.1498837665692));
#105958=CARTESIAN_POINT('Ctrl Pts',(109.675031770393,22.1247415238079,33.9637142832168));
#105959=CARTESIAN_POINT('Ctrl Pts',(109.454735599089,22.1036112118687,33.8558527250311));
#105960=CARTESIAN_POINT('Ctrl Pts',(109.133967345731,22.0613505879902,33.4047795537825));
#105961=CARTESIAN_POINT('Ctrl Pts',(109.440802503731,21.9979596521725,32.6290335730239));
#105962=CARTESIAN_POINT('Ctrl Pts',(110.258915539699,21.9345687163547,32.4663782012585));
#105963=CARTESIAN_POINT('Ctrl Pts',(110.840340273426,21.871177780537,33.0636201432557));
#105964=CARTESIAN_POINT('Ctrl Pts',(110.655412180794,21.8077868447193,33.8767425456563));
#105965=CARTESIAN_POINT('Ctrl Pts',(109.87248062677,21.7443959089015,34.1636192592745));
#105966=CARTESIAN_POINT('Ctrl Pts',(109.205929096291,21.6810049730838,33.6627223392945));
#105967=CARTESIAN_POINT('Ctrl Pts',(109.263736762059,21.6176140372661,32.8309100417672));
#105968=CARTESIAN_POINT('Ctrl Pts',(109.993204480012,21.5542231014483,32.4270322435203));
#105969=CARTESIAN_POINT('Ctrl Pts',(110.72886617238,21.4908321656306,32.8195051832315));
#105970=CARTESIAN_POINT('Ctrl Pts',(110.799629204568,21.4274412298128,33.6503070362846));
#105971=CARTESIAN_POINT('Ctrl Pts',(110.140937708849,21.3640502939951,34.1615442221346));
#105972=CARTESIAN_POINT('Ctrl Pts',(109.353676833335,21.3006593581774,33.8868454058899));
#105973=CARTESIAN_POINT('Ctrl Pts',(109.156019502377,21.2372684223596,33.0768054602444));
#105974=CARTESIAN_POINT('Ctrl Pts',(109.728271023269,21.1738774865419,32.4703661604886));
#105975=CARTESIAN_POINT('Ctrl Pts',(110.548413292333,21.1104865507242,32.6207659046162));
#105976=CARTESIAN_POINT('Ctrl Pts',(110.868252234251,21.0470956149064,33.3907605269755));
#105977=CARTESIAN_POINT('Ctrl Pts',(110.39607661522,20.9837046790887,34.0780233965501));
#105978=CARTESIAN_POINT('Ctrl Pts',(109.56249704574,20.9203137432709,34.0554061006045));
#105979=CARTESIAN_POINT('Ctrl Pts',(109.128203450212,20.8569228074532,33.3439697147248));
#105980=CARTESIAN_POINT('Ctrl Pts',(109.488772271949,20.7935318716355,32.5918022902927));
#105981=CARTESIAN_POINT('Ctrl Pts',(110.316393411479,20.7301409358178,32.4870507258606));
#105982=CARTESIAN_POINT('Ctrl Pts',(110.6737668031,20.6878803119393,32.9097131646266));
#105983=CARTESIAN_POINT('Ctrl Pts',(110.723592507189,20.66675,33.1498837665692));
#105984=CARTESIAN_POINT('Ctrl Pts',(109.641648137424,22.080911015872,34.0318969300381));
#105985=CARTESIAN_POINT('Ctrl Pts',(109.398721179915,22.0597807039327,33.9129548712313));
#105986=CARTESIAN_POINT('Ctrl Pts',(109.045000752583,22.0175200800542,33.4155434434415));
#105987=CARTESIAN_POINT('Ctrl Pts',(109.383356752817,21.9541291442365,32.5601059213578));
#105988=CARTESIAN_POINT('Ctrl Pts',(110.285513651637,21.8907382084188,32.3807411400661));
#105989=CARTESIAN_POINT('Ctrl Pts',(110.926667516219,21.827347272601,33.0393370975301));
#105990=CARTESIAN_POINT('Ctrl Pts',(110.722741961658,21.7639563367833,33.935990680421));
#105991=CARTESIAN_POINT('Ctrl Pts',(109.859380700179,21.7005654009655,34.2523379269785));
#105992=CARTESIAN_POINT('Ctrl Pts',(109.124355055552,21.6371744651478,33.6999844109113));
#105993=CARTESIAN_POINT('Ctrl Pts',(109.188101239984,21.5737835293301,32.7827209402844));
#105994=CARTESIAN_POINT('Ctrl Pts',(109.992506383631,21.5103925935123,32.3373532148607));
#105995=CARTESIAN_POINT('Ctrl Pts',(110.803741801951,21.4470016576946,32.7701444730289));
#105996=CARTESIAN_POINT('Ctrl Pts',(110.881774243513,21.3836107218769,33.6862936973193));
#105997=CARTESIAN_POINT('Ctrl Pts',(110.155416086472,21.3202197860591,34.2500497235289));
#105998=CARTESIAN_POINT('Ctrl Pts',(109.287280757012,21.2568288502414,33.9471313965039));
#105999=CARTESIAN_POINT('Ctrl Pts',(109.069318303309,21.1934379144237,33.0538769278));
#106000=CARTESIAN_POINT('Ctrl Pts',(109.700356600874,21.1300469786059,32.3851387780128));
#106001=CARTESIAN_POINT('Ctrl Pts',(110.6047511937,21.0666560427882,32.550988924362));
#106002=CARTESIAN_POINT('Ctrl Pts',(110.957446842438,21.0032651069704,33.40008425725));
#106003=CARTESIAN_POINT('Ctrl Pts',(110.436765135345,20.9398741711527,34.1579488943238));
#106004=CARTESIAN_POINT('Ctrl Pts',(109.517552842839,20.876483235335,34.133008148152));
#106005=CARTESIAN_POINT('Ctrl Pts',(109.038644738343,20.8130922995172,33.3484866757211));
#106006=CARTESIAN_POINT('Ctrl Pts',(109.436254403179,20.7497013636995,32.519049909424));
#106007=CARTESIAN_POINT('Ctrl Pts',(110.348896162703,20.6863104278818,32.4035373306486));
#106008=CARTESIAN_POINT('Ctrl Pts',(110.742982134361,20.6440498040033,32.8696194222918));
#106009=CARTESIAN_POINT('Ctrl Pts',(110.797926378868,20.622919492064,33.1344624890934));
#106010=CARTESIAN_POINT('Ctrl Pts',(109.608264504454,22.037080507936,34.1000795768593));
#106011=CARTESIAN_POINT('Ctrl Pts',(109.342706760742,22.0159501959967,33.9700570174315));
#106012=CARTESIAN_POINT('Ctrl Pts',(108.956034159435,21.9736895721183,33.4263073331004));
#106013=CARTESIAN_POINT('Ctrl Pts',(109.325911001904,21.9102986363005,32.4911782696917));
#106014=CARTESIAN_POINT('Ctrl Pts',(110.312111763575,21.8469077004828,32.2951040788738));
#106015=CARTESIAN_POINT('Ctrl Pts',(111.012994759013,21.783516764665,33.0150540518046));
#106016=CARTESIAN_POINT('Ctrl Pts',(110.790071742523,21.7201258288473,33.9952388151856));
#106017=CARTESIAN_POINT('Ctrl Pts',(109.846280773588,21.6567348930296,34.3410565946825));
#106018=CARTESIAN_POINT('Ctrl Pts',(109.042781014812,21.5933439572118,33.737246482528));
#106019=CARTESIAN_POINT('Ctrl Pts',(109.112465717909,21.5299530213941,32.7345318388015));
#106020=CARTESIAN_POINT('Ctrl Pts',(109.99180828725,21.4665620855764,32.2476741862011));
#106021=CARTESIAN_POINT('Ctrl Pts',(110.878617431523,21.4031711497586,32.7207837628264));
#106022=CARTESIAN_POINT('Ctrl Pts',(110.963919282458,21.3397802139409,33.7222803583539));
#106023=CARTESIAN_POINT('Ctrl Pts',(110.169894464095,21.2763892781232,34.3385552249232));
#106024=CARTESIAN_POINT('Ctrl Pts',(109.220884680689,21.2129983423054,34.007417387118));
#106025=CARTESIAN_POINT('Ctrl Pts',(108.982617104241,21.1496074064877,33.0309483953555));
#106026=CARTESIAN_POINT('Ctrl Pts',(109.672442178479,21.0862164706699,32.2999113955371));
#106027=CARTESIAN_POINT('Ctrl Pts',(110.661089095066,21.0228255348522,32.4812119441078));
#106028=CARTESIAN_POINT('Ctrl Pts',(111.046641450625,20.9594345990345,33.4094079875246));
#106029=CARTESIAN_POINT('Ctrl Pts',(110.47745365547,20.8960436632168,34.2378743920975));
#106030=CARTESIAN_POINT('Ctrl Pts',(109.472608639937,20.832652727399,34.2106101956994));
#106031=CARTESIAN_POINT('Ctrl Pts',(108.949086026474,20.7692617915813,33.3530036367172));
#106032=CARTESIAN_POINT('Ctrl Pts',(109.383736534408,20.7058708557635,32.4462975285553));
#106033=CARTESIAN_POINT('Ctrl Pts',(110.381398913927,20.6424799199458,32.3200239354364));
#106034=CARTESIAN_POINT('Ctrl Pts',(110.812197465622,20.6002192960673,32.8295256799569));
#106035=CARTESIAN_POINT('Ctrl Pts',(110.872260250547,20.5790889841281,33.1190412116176));
#106036=CARTESIAN_POINT('Ctrl Pts',(109.574880871485,21.99325,34.1682622236805));
#106037=CARTESIAN_POINT('Ctrl Pts',(109.286692341569,21.9721196880608,34.0271591636317));
#106038=CARTESIAN_POINT('Ctrl Pts',(108.867067566286,21.9298590641823,33.4370712227594));
#106039=CARTESIAN_POINT('Ctrl Pts',(109.26846525099,21.8664681283645,32.4222506180256));
#106040=CARTESIAN_POINT('Ctrl Pts',(110.338709875513,21.8030771925468,32.2094670176815));
#106041=CARTESIAN_POINT('Ctrl Pts',(111.099322001806,21.7396862567291,32.9907710060791));
#106042=CARTESIAN_POINT('Ctrl Pts',(110.857401523387,21.6762953209113,34.0544869499503));
#106043=CARTESIAN_POINT('Ctrl Pts',(109.833180846996,21.6129043850936,34.4297752623866));
#106044=CARTESIAN_POINT('Ctrl Pts',(108.961206974073,21.5495134492758,33.7745085541447));
#106045=CARTESIAN_POINT('Ctrl Pts',(109.036830195834,21.4861225134581,32.6863427373186));
#106046=CARTESIAN_POINT('Ctrl Pts',(109.991110190869,21.4227315776404,32.1579951575416));
#106047=CARTESIAN_POINT('Ctrl Pts',(110.953493061094,21.3593406418227,32.6714230526239));
#106048=CARTESIAN_POINT('Ctrl Pts',(111.046064321402,21.2959497060049,33.7582670193886));
#106049=CARTESIAN_POINT('Ctrl Pts',(110.184372841718,21.2325587701872,34.4270607263175));
#106050=CARTESIAN_POINT('Ctrl Pts',(109.154488604366,21.1691678343694,34.0677033777321));
#106051=CARTESIAN_POINT('Ctrl Pts',(108.895915905173,21.1057768985517,33.0080198629111));
#106052=CARTESIAN_POINT('Ctrl Pts',(109.644527756083,21.042385962734,32.2146840130614));
#106053=CARTESIAN_POINT('Ctrl Pts',(110.717426996432,20.9789950269162,32.4114349638535));
#106054=CARTESIAN_POINT('Ctrl Pts',(111.135836058812,20.9156040910985,33.4187317177991));
#106055=CARTESIAN_POINT('Ctrl Pts',(110.518142175595,20.8522131552808,34.3177998898711));
#106056=CARTESIAN_POINT('Ctrl Pts',(109.427664437036,20.788822219463,34.2882122432469));
#106057=CARTESIAN_POINT('Ctrl Pts',(108.859527314605,20.7254312836453,33.3575205977135));
#106058=CARTESIAN_POINT('Ctrl Pts',(109.331218665638,20.6620403478275,32.3735451476867));
#106059=CARTESIAN_POINT('Ctrl Pts',(110.413901665152,20.5986494120098,32.2365105402243));
#106060=CARTESIAN_POINT('Ctrl Pts',(110.881412796884,20.5563887881313,32.7894319376221));
#106061=CARTESIAN_POINT('Ctrl Pts',(110.946594122226,20.5352584761921,33.1036199341418));
#106062=CARTESIAN_POINT('Ctrl Pts',(109.031713168497,20.7222359168897,33.3003348740849));
#106063=CARTESIAN_POINT('Ctrl Pts',(109.032777313761,20.7037406112598,33.0205677454497));
#106064=CARTESIAN_POINT('Ctrl Pts',(109.163857863559,20.6852453056299,32.7397911054646));
#106065=CARTESIAN_POINT('Ctrl Pts',(109.377024795358,20.66675,32.5586208180318));
#106066=CARTESIAN_POINT('',(109.570122622048,21.99325,32.6988956497206));
#106067=CARTESIAN_POINT('Ctrl Pts',(109.569164649808,21.99325,32.6980580125958));
#106068=CARTESIAN_POINT('Ctrl Pts',(109.552656141457,21.99325,32.7063773006967));
#106069=CARTESIAN_POINT('Ctrl Pts',(109.536515068327,21.99325,32.7153401328564));
#106070=CARTESIAN_POINT('Ctrl Pts',(109.520783466014,21.99325,32.7249368845833));
#106071=CARTESIAN_POINT('Ctrl Pts',(109.492247653832,21.99325,32.7423445903831));
#106072=CARTESIAN_POINT('Ctrl Pts',(109.465058040893,21.99325,32.7618350277424));
#106073=CARTESIAN_POINT('Ctrl Pts',(109.439278518602,21.99325,32.7831583285348));
#106074=CARTESIAN_POINT('Ctrl Pts',(109.428752468441,21.99325,32.7918648565767));
#106075=CARTESIAN_POINT('Ctrl Pts',(109.418461644647,21.99325,32.8008775159162));
#106076=CARTESIAN_POINT('Ctrl Pts',(109.408411128155,21.99325,32.8101814651125));
#106077=CARTESIAN_POINT('Ctrl Pts',(109.402312464482,21.99325,32.8158271109875));
#106078=CARTESIAN_POINT('Ctrl Pts',(109.39630479516,21.99325,32.8215778437279));
#106079=CARTESIAN_POINT('Ctrl Pts',(109.390394923749,21.99325,32.8274241886413));
#106080=CARTESIAN_POINT('Ctrl Pts',(109.365023548343,21.99325,32.8525228415979));
#106081=CARTESIAN_POINT('Ctrl Pts',(109.341420589248,21.99325,32.8794095287664));
#106082=CARTESIAN_POINT('Ctrl Pts',(109.319661313854,21.99325,32.9078022118923));
#106083=CARTESIAN_POINT('Ctrl Pts',(109.303854012061,21.99325,32.9284284369287));
#106084=CARTESIAN_POINT('Ctrl Pts',(109.289019941609,21.99325,32.9498506817826));
#106085=CARTESIAN_POINT('Ctrl Pts',(109.27519572685,21.99325,32.9719757958513));
#106086=CARTESIAN_POINT('Ctrl Pts',(109.270957505281,21.99325,32.9787589034131));
#106087=CARTESIAN_POINT('Ctrl Pts',(109.266816302605,21.99325,32.985605032468));
#106088=CARTESIAN_POINT('Ctrl Pts',(109.262777145955,21.99325,32.9925040649077));
#106089=CARTESIAN_POINT('Ctrl Pts',(109.243693734176,21.99325,33.0250992545292));
#106090=CARTESIAN_POINT('Ctrl Pts',(109.22685695248,21.99325,33.0589177702548));
#106091=CARTESIAN_POINT('Ctrl Pts',(109.212348822142,21.99325,33.0936591021481));
#106092=CARTESIAN_POINT('Ctrl Pts',(109.197733505773,21.99325,33.1286571029161));
#106093=CARTESIAN_POINT('Ctrl Pts',(109.185480484964,21.99325,33.1645926511776));
#106094=CARTESIAN_POINT('Ctrl Pts',(109.175707331983,21.99325,33.2011997647515));
#106095=CARTESIAN_POINT('Ctrl Pts',(109.170688778414,21.99325,33.2199976655723));
#106096=CARTESIAN_POINT('Ctrl Pts',(109.166324758574,21.99325,33.2389732173444));
#106097=CARTESIAN_POINT('Ctrl Pts',(109.162635799128,21.99325,33.2580931624287));
#106098=CARTESIAN_POINT('Ctrl Pts',(109.160827961278,21.99325,33.2674632194669));
#106099=CARTESIAN_POINT('Ctrl Pts',(109.159182106796,21.99325,33.2768704544511));
#106100=CARTESIAN_POINT('Ctrl Pts',(109.157704090945,21.99325,33.2862874962798));
#106101=CARTESIAN_POINT('Ctrl Pts',(109.151655446475,21.99325,33.3248258772845));
#106102=CARTESIAN_POINT('Ctrl Pts',(109.148397359835,21.99325,33.3636070754909));
#106103=CARTESIAN_POINT('Ctrl Pts',(109.148031034507,21.99325,33.402343751128));
#106104=CARTESIAN_POINT('Ctrl Pts',(109.147673763903,21.99325,33.4401229447785));
#106105=CARTESIAN_POINT('Ctrl Pts',(109.150065954734,21.99325,33.4778610549384));
#106106=CARTESIAN_POINT('Ctrl Pts',(109.155030030729,21.99325,33.5153593431265));
#106107=CARTESIAN_POINT('Ctrl Pts',(109.157337041179,21.99325,33.5327863411743));
#106108=CARTESIAN_POINT('Ctrl Pts',(109.160200273373,21.99325,33.550161722503));
#106109=CARTESIAN_POINT('Ctrl Pts',(109.163605617005,21.99325,33.567466063713));
#106110=CARTESIAN_POINT('Ctrl Pts',(109.165348451527,21.99325,33.5763223221422));
#106111=CARTESIAN_POINT('Ctrl Pts',(109.167233319974,21.99325,33.585159974556));
#106112=CARTESIAN_POINT('Ctrl Pts',(109.16925855919,21.99325,33.5939764130428));
#106113=CARTESIAN_POINT('Ctrl Pts',(109.170862832037,21.99325,33.6009602659919));
#106114=CARTESIAN_POINT('Ctrl Pts',(109.172554757612,21.99325,33.6079285998806));
#106115=CARTESIAN_POINT('Ctrl Pts',(109.17433094191,21.99325,33.614871383303));
#106116=CARTESIAN_POINT('Ctrl Pts',(109.184136912542,21.99325,33.6532011503192));
#106117=CARTESIAN_POINT('Ctrl Pts',(109.19652383406,21.99325,33.6908270002868));
#106118=CARTESIAN_POINT('Ctrl Pts',(109.211283288827,21.99325,33.7275332573707));
#106119=CARTESIAN_POINT('Ctrl Pts',(109.226396659773,21.99325,33.7651196918364));
#106120=CARTESIAN_POINT('Ctrl Pts',(109.243997870408,21.99325,33.8017429878313));
#106121=CARTESIAN_POINT('Ctrl Pts',(109.263917687932,21.99325,33.8371751681065));
#106122=CARTESIAN_POINT('Ctrl Pts',(109.273277196623,21.99325,33.8538233024993));
#106123=CARTESIAN_POINT('Ctrl Pts',(109.283149334381,21.99325,33.8702084251205));
#106124=CARTESIAN_POINT('Ctrl Pts',(109.293520375918,21.99325,33.8863060632989));
#106125=CARTESIAN_POINT('Ctrl Pts',(109.299216111555,21.99325,33.8951468235169));
#106126=CARTESIAN_POINT('Ctrl Pts',(109.305062366064,21.99325,33.9039008597167));
#106127=CARTESIAN_POINT('Ctrl Pts',(109.311057158114,21.99325,33.9125639871748));
#106128=CARTESIAN_POINT('Ctrl Pts',(109.31565416963,21.99325,33.9192071695175));
#106129=CARTESIAN_POINT('Ctrl Pts',(109.320335637454,21.99325,33.9257925969553));
#106130=CARTESIAN_POINT('Ctrl Pts',(109.325095709211,21.99325,33.9323124342923));
#106131=CARTESIAN_POINT('Ctrl Pts',(109.350054193339,21.99325,33.9664978972433));
#106132=CARTESIAN_POINT('Ctrl Pts',(109.377205344832,21.99325,33.9989327926013));
#106133=CARTESIAN_POINT('Ctrl Pts',(109.406353139311,21.99325,34.0293791252897));
#106134=CARTESIAN_POINT('Ctrl Pts',(109.435309246376,21.99325,34.0596252308639));
#106135=CARTESIAN_POINT('Ctrl Pts',(109.466236355712,21.99325,34.0879100272063));
#106136=CARTESIAN_POINT('Ctrl Pts',(109.498989823094,21.99325,34.1139838486523));
#106137=CARTESIAN_POINT('Ctrl Pts',(109.523294998801,21.99325,34.1333322982136));
#106138=CARTESIAN_POINT('Ctrl Pts',(109.548606893583,21.99325,34.1514630223488));
#106139=CARTESIAN_POINT('Ctrl Pts',(109.574880871485,21.99325,34.1682622236805));
#106140=CARTESIAN_POINT('Ctrl Pts',(109.569164649808,21.99325,32.6980580125958));
#106141=CARTESIAN_POINT('Ctrl Pts',(109.753810436789,21.9736895721183,32.5674578367501));
#106142=CARTESIAN_POINT('Ctrl Pts',(110.273314592313,21.9329988322973,32.4811689689149));
#106143=CARTESIAN_POINT('Ctrl Pts',(110.840340273426,21.871177780537,33.0636201432557));
#106144=CARTESIAN_POINT('Ctrl Pts',(110.655412180794,21.8077868447193,33.8767425456563));
#106145=CARTESIAN_POINT('Ctrl Pts',(109.87248062677,21.7443959089015,34.1636192592745));
#106146=CARTESIAN_POINT('Ctrl Pts',(109.332505785412,21.6930427742276,33.7578415773765));
#106147=CARTESIAN_POINT('Ctrl Pts',(109.261694316903,21.662819951493,33.4061997065318));
#106148=CARTESIAN_POINT('Ctrl Pts',(109.262045097267,21.6537274406976,33.3002734582445));
#106149=CARTESIAN_POINT('Origin',(110.,21.99325,33.3));
#106150=CARTESIAN_POINT('',(109.03325,21.99325,33.3));
#106151=CARTESIAN_POINT('Origin',(110.,21.99325,33.3));
#106152=CARTESIAN_POINT('Origin',(110.,21.99325,33.3));
#106153=CARTESIAN_POINT('',(110.429877377952,21.99325,32.6988956497206));
#106154=CARTESIAN_POINT('Ctrl Pts',(110.426174626828,21.99325,34.1695497362103));
#106155=CARTESIAN_POINT('Ctrl Pts',(110.446294741806,21.99325,34.1568125013073));
#106156=CARTESIAN_POINT('Ctrl Pts',(110.465877499818,21.99325,34.14330064166));
#106157=CARTESIAN_POINT('Ctrl Pts',(110.484870687874,21.99325,34.1290117969353));
#106158=CARTESIAN_POINT('Ctrl Pts',(110.514960367498,21.99325,34.1063749042409));
#106159=CARTESIAN_POINT('Ctrl Pts',(110.54357182032,21.99325,34.081788511877));
#106160=CARTESIAN_POINT('Ctrl Pts',(110.570607330673,21.99325,34.0554521560241));
#106161=CARTESIAN_POINT('Ctrl Pts',(110.58591980247,21.99325,34.0405356739251));
#106162=CARTESIAN_POINT('Ctrl Pts',(110.600726220396,21.99325,34.0250574879875));
#106163=CARTESIAN_POINT('Ctrl Pts',(110.615004560658,21.99325,34.0090521485743));
#106164=CARTESIAN_POINT('Ctrl Pts',(110.621473282823,21.99325,34.0018010191072));
#106165=CARTESIAN_POINT('Ctrl Pts',(110.627832369673,21.99325,33.9944428472011));
#106166=CARTESIAN_POINT('Ctrl Pts',(110.63407242037,21.99325,33.9869901381755));
#106167=CARTESIAN_POINT('Ctrl Pts',(110.660863661377,21.99325,33.9549924296047));
#106168=CARTESIAN_POINT('Ctrl Pts',(110.685505043446,21.99325,33.9212086657911));
#106169=CARTESIAN_POINT('Ctrl Pts',(110.707856824131,21.99325,33.8859124195861));
#106170=CARTESIAN_POINT('Ctrl Pts',(110.720728374224,21.99325,33.8655866384995));
#106171=CARTESIAN_POINT('Ctrl Pts',(110.732839764501,21.99325,33.8447589036181));
#106172=CARTESIAN_POINT('Ctrl Pts',(110.74415655274,21.99325,33.8234800396049));
#106173=CARTESIAN_POINT('Ctrl Pts',(110.748940610787,21.99325,33.8144846145377));
#106174=CARTESIAN_POINT('Ctrl Pts',(110.753582593749,21.99325,33.8054085665864));
#106175=CARTESIAN_POINT('Ctrl Pts',(110.75807957408,21.99325,33.7962557496567));
#106176=CARTESIAN_POINT('Ctrl Pts',(110.761770866658,21.99325,33.7887427692294));
#106177=CARTESIAN_POINT('Ctrl Pts',(110.765360254662,21.99325,33.7811866076814));
#106178=CARTESIAN_POINT('Ctrl Pts',(110.768846556029,21.99325,33.7735900770095));
#106179=CARTESIAN_POINT('Ctrl Pts',(110.785569298044,21.99325,33.7371517977927));
#106180=CARTESIAN_POINT('Ctrl Pts',(110.79992620115,21.99325,33.6997811388704));
#106181=CARTESIAN_POINT('Ctrl Pts',(110.811786822027,21.99325,33.6617216338423));
#106182=CARTESIAN_POINT('Ctrl Pts',(110.823370425106,21.99325,33.6245510502608));
#106183=CARTESIAN_POINT('Ctrl Pts',(110.83257307252,21.99325,33.5867223451475));
#106184=CARTESIAN_POINT('Ctrl Pts',(110.839225035118,21.99325,33.54846478224));
#106185=CARTESIAN_POINT('Ctrl Pts',(110.842386440096,21.99325,33.5302825318116));
#106186=CARTESIAN_POINT('Ctrl Pts',(110.844970999637,21.99325,33.5120035489813));
#106187=CARTESIAN_POINT('Ctrl Pts',(110.846956463004,21.99325,33.4936536749133));
#106188=CARTESIAN_POINT('Ctrl Pts',(110.847833192143,21.99325,33.4855508463484));
#106189=CARTESIAN_POINT('Ctrl Pts',(110.848593070033,21.99325,33.4774342090572));
#106190=CARTESIAN_POINT('Ctrl Pts',(110.849234013381,21.99325,33.4693060637584));
#106191=CARTESIAN_POINT('Ctrl Pts',(110.849865427658,21.99325,33.4612987617171));
#106192=CARTESIAN_POINT('Ctrl Pts',(110.850380715277,21.99325,33.45328873078));
#106193=CARTESIAN_POINT('Ctrl Pts',(110.850778455272,21.99325,33.4452818304454));
#106194=CARTESIAN_POINT('Ctrl Pts',(110.852542333712,21.99325,33.4097732091587));
#106195=CARTESIAN_POINT('Ctrl Pts',(110.851999556645,21.99325,33.3743011239417));
#106196=CARTESIAN_POINT('Ctrl Pts',(110.849028272475,21.99325,33.3390457962148));
#106197=CARTESIAN_POINT('Ctrl Pts',(110.846251958068,21.99325,33.3061038530315));
#106198=CARTESIAN_POINT('Ctrl Pts',(110.841354467676,21.99325,33.2733506949589));
#106199=CARTESIAN_POINT('Ctrl Pts',(110.834425817615,21.99325,33.2409490348578));
#106200=CARTESIAN_POINT('Ctrl Pts',(110.830911409544,21.99325,33.224513992715));
#106201=CARTESIAN_POINT('Ctrl Pts',(110.826874028556,21.99325,33.2081696208379));
#106202=CARTESIAN_POINT('Ctrl Pts',(110.82232328327,21.99325,33.1919389686854));
#106203=CARTESIAN_POINT('Ctrl Pts',(110.819274840855,21.99325,33.1810664180728));
#106204=CARTESIAN_POINT('Ctrl Pts',(110.815996005313,21.99325,33.1702449246969));
#106205=CARTESIAN_POINT('Ctrl Pts',(110.812489369983,21.99325,33.1594818015797));
#106206=CARTESIAN_POINT('Ctrl Pts',(110.809585252903,21.99325,33.1505680233467));
#106207=CARTESIAN_POINT('Ctrl Pts',(110.806523937818,21.99325,33.1416922065324));
#106208=CARTESIAN_POINT('Ctrl Pts',(110.803315104313,21.99325,33.1328799180716));
#106209=CARTESIAN_POINT('Ctrl Pts',(110.790547715166,21.99325,33.0978173584587));
#106210=CARTESIAN_POINT('Ctrl Pts',(110.775425302369,21.99325,33.0636827746753));
#106211=CARTESIAN_POINT('Ctrl Pts',(110.758092822638,21.99325,33.0307063318292));
#106212=CARTESIAN_POINT('Ctrl Pts',(110.740958075622,21.99325,32.9981060914485));
#106213=CARTESIAN_POINT('Ctrl Pts',(110.721662428768,21.99325,32.9666368288481));
#106214=CARTESIAN_POINT('Ctrl Pts',(110.700313079278,21.99325,32.9365590456047));
#106215=CARTESIAN_POINT('Ctrl Pts',(110.690673858058,21.99325,32.9229789406643));
#106216=CARTESIAN_POINT('Ctrl Pts',(110.680615626106,21.99325,32.9096830911525));
#106217=CARTESIAN_POINT('Ctrl Pts',(110.670146809868,21.99325,32.8966987819899));
#106218=CARTESIAN_POINT('Ctrl Pts',(110.665276843094,21.99325,32.8906586383129));
#106219=CARTESIAN_POINT('Ctrl Pts',(110.660316746254,21.99325,32.884684463972));
#106220=CARTESIAN_POINT('Ctrl Pts',(110.655271360203,21.99325,32.8787838850441));
#106221=CARTESIAN_POINT('Ctrl Pts',(110.632244741213,21.99325,32.8518542544048));
#106222=CARTESIAN_POINT('Ctrl Pts',(110.607540668324,21.99325,32.8265654533201));
#106223=CARTESIAN_POINT('Ctrl Pts',(110.581270482762,21.99325,32.8031360739611));
#106224=CARTESIAN_POINT('Ctrl Pts',(110.555959181703,21.99325,32.78056188722));
#106225=CARTESIAN_POINT('Ctrl Pts',(110.529193139856,21.99325,32.7597134486046));
#106226=CARTESIAN_POINT('Ctrl Pts',(110.501054523868,21.99325,32.7408301544696));
#106227=CARTESIAN_POINT('Ctrl Pts',(110.478219674726,21.99325,32.7255061181679));
#106228=CARTESIAN_POINT('Ctrl Pts',(110.454480437898,21.99325,32.7114769174597));
#106229=CARTESIAN_POINT('Ctrl Pts',(110.429877377952,21.99325,32.6988956497206));
#106230=CARTESIAN_POINT('Origin',(110.,21.99325,33.3));
#106231=CARTESIAN_POINT('Origin',(110.,22.7327725593024,33.3));
#106232=CARTESIAN_POINT('Ctrl Pts',(110.429877377952,21.99325,32.6988956497206));
#106233=CARTESIAN_POINT('Ctrl Pts',(110.629392425721,21.9721196880608,32.8415780401524));
#106234=CARTESIAN_POINT('Ctrl Pts',(110.871460562011,21.9298590641823,33.3393357713752));
#106235=CARTESIAN_POINT('Ctrl Pts',(110.441011075278,21.8664681283645,34.0539278279709));
#106236=CARTESIAN_POINT('Ctrl Pts',(109.60727954107,21.8030771925468,34.079572693842));
#106237=CARTESIAN_POINT('Ctrl Pts',(109.273287397513,21.7585120028594,33.5980922637393));
#106238=CARTESIAN_POINT('Ctrl Pts',(109.259905511347,21.7350771251113,33.3271351273468));
#106239=CARTESIAN_POINT('Ctrl Pts',(109.260096259818,21.7327725593024,33.3004698838673));
#106240=CARTESIAN_POINT('Ctrl Pts',(110.562359885163,22.1247415238079,32.5136432603077));
#106241=CARTESIAN_POINT('Ctrl Pts',(110.823362824852,22.1036112118687,32.7002984713361));
#106242=CARTESIAN_POINT('Ctrl Pts',(111.140033150641,22.0613505879902,33.3514585344749));
#106243=CARTESIAN_POINT('Ctrl Pts',(110.576924840359,21.9979596521725,34.2862783865912));
#106244=CARTESIAN_POINT('Ctrl Pts',(109.486248303559,21.9345687163548,34.3198266600429));
#106245=CARTESIAN_POINT('Ctrl Pts',(108.864753649643,21.871177780537,33.4238848870208));
#106246=CARTESIAN_POINT('Ctrl Pts',(109.278620310884,21.8077868447193,32.4145625088781));
#106247=CARTESIAN_POINT('Ctrl Pts',(110.350675199839,21.7443959089015,32.2131476509265));
#106248=CARTESIAN_POINT('Ctrl Pts',(111.102775091905,21.6810049730838,33.0031216845332));
#106249=CARTESIAN_POINT('Ctrl Pts',(110.84890495161,21.6176140372661,34.0639581186772));
#106250=CARTESIAN_POINT('Ctrl Pts',(109.820617769302,21.5542231014483,34.4278636578058));
#106251=CARTESIAN_POINT('Ctrl Pts',(108.955975747213,21.4908321656306,33.7628948884635));
#106252=CARTESIAN_POINT('Ctrl Pts',(109.043732049669,21.4274412298128,32.6756514155529));
#106253=CARTESIAN_POINT('Ctrl Pts',(110.003835112584,21.3640502939951,32.1579646066592));
#106254=CARTESIAN_POINT('Ctrl Pts',(110.960439907255,21.3006593581774,32.6820894055575));
#106255=CARTESIAN_POINT('Ctrl Pts',(111.040891398074,21.2372684223596,33.7698930864614));
#106256=CARTESIAN_POINT('Ctrl Pts',(110.171803802845,21.1738774865419,34.4290505202554));
#106257=CARTESIAN_POINT('Ctrl Pts',(109.145981672175,21.1104865507242,34.0582231421285));
#106258=CARTESIAN_POINT('Ctrl Pts',(108.899247052897,21.0470956149064,32.9957565548576));
#106259=CARTESIAN_POINT('Ctrl Pts',(109.65662563213,20.9837046790887,32.2107423399201));
#106260=CARTESIAN_POINT('Ctrl Pts',(110.727326917525,20.920313743271,32.4195868604602));
#106261=CARTESIAN_POINT('Ctrl Pts',(111.134364726985,20.8569228074532,33.4311635936655));
#106262=CARTESIAN_POINT('Ctrl Pts',(110.507004538604,20.7935318716355,34.3239793577582));
#106263=CARTESIAN_POINT('Ctrl Pts',(109.416540606268,20.7301409358177,34.2807643453944));
#106264=CARTESIAN_POINT('Ctrl Pts',(109.046513639301,20.6878803119393,33.6583741407962));
#106265=CARTESIAN_POINT('Ctrl Pts',(109.033986956687,20.66675,33.3377407293226));
#106266=CARTESIAN_POINT('Ctrl Pts',(110.518199049426,22.080911015872,32.5753940567787));
#106267=CARTESIAN_POINT('Ctrl Pts',(110.758706025142,22.0597807039327,32.7473916609415));
#106268=CARTESIAN_POINT('Ctrl Pts',(111.050508954431,22.0175200800542,33.3474176134417));
#106269=CARTESIAN_POINT('Ctrl Pts',(110.531620251999,21.9541291442365,34.2088282003844));
#106270=CARTESIAN_POINT('Ctrl Pts',(109.526592049396,21.8907382084188,34.2397420046426));
#106271=CARTESIAN_POINT('Ctrl Pts',(108.953901949374,21.827347272601,33.4141564901519));
#106272=CARTESIAN_POINT('Ctrl Pts',(109.335268608168,21.7639563367833,32.4840938901739));
#106273=CARTESIAN_POINT('Ctrl Pts',(110.323137478345,21.7005654009656,32.2984956804072));
#106274=CARTESIAN_POINT('Ctrl Pts',(111.016176685843,21.6371744651478,33.0264348597242));
#106275=CARTESIAN_POINT('Ctrl Pts',(110.782242387097,21.5737835293301,34.0039662346917));
#106276=CARTESIAN_POINT('Ctrl Pts',(109.834704245655,21.5103925935123,34.3392951040379));
#106277=CARTESIAN_POINT('Ctrl Pts',(109.037960584235,21.4470016576946,33.7265448114537));
#106278=CARTESIAN_POINT('Ctrl Pts',(109.118825584946,21.3836107218769,32.7246800820843));
#106279=CARTESIAN_POINT('Ctrl Pts',(110.003533949963,21.3202197860591,32.2476460344097));
#106280=CARTESIAN_POINT('Ctrl Pts',(110.885018757741,21.2568288502414,32.7306125114567));
#106281=CARTESIAN_POINT('Ctrl Pts',(110.959152576969,21.1934379144237,33.7329934569668));
#106282=CARTESIAN_POINT('Ctrl Pts',(110.158312443101,21.1300469786059,34.3403887648936));
#106283=CARTESIAN_POINT('Ctrl Pts',(109.213045778429,21.0666560427882,33.9986816127363));
#106284=CARTESIAN_POINT('Ctrl Pts',(108.985686664552,21.0032651069704,33.0196480968388));
#106285=CARTESIAN_POINT('Ctrl Pts',(109.683590035986,20.9398741711527,32.2962792529735));
#106286=CARTESIAN_POINT('Ctrl Pts',(110.670211597996,20.876483235335,32.4887236909162));
#106287=CARTESIAN_POINT('Ctrl Pts',(111.045285659121,20.8130922995172,33.4208636166092));
#106288=CARTESIAN_POINT('Ctrl Pts',(110.467190631642,20.7497013636995,34.243568600503));
#106289=CARTESIAN_POINT('Ctrl Pts',(109.46235833816,20.6863104278818,34.2037471642329));
#106290=CARTESIAN_POINT('Ctrl Pts',(109.121388742706,20.6440498040033,33.6302318390752));
#106291=CARTESIAN_POINT('Ctrl Pts',(109.109845751831,20.622919492064,33.3347770361571));
#106292=CARTESIAN_POINT('Ctrl Pts',(110.474038213689,22.037080507936,32.6371448532496));
#106293=CARTESIAN_POINT('Ctrl Pts',(110.694049225431,22.0159501959967,32.794484850547));
#106294=CARTESIAN_POINT('Ctrl Pts',(110.960984758221,21.9736895721183,33.3433766924084));
#106295=CARTESIAN_POINT('Ctrl Pts',(110.486315663638,21.9102986363005,34.1313780141776));
#106296=CARTESIAN_POINT('Ctrl Pts',(109.566935795233,21.8469077004828,34.1596573492423));
#106297=CARTESIAN_POINT('Ctrl Pts',(109.043050249104,21.783516764665,33.404428093283));
#106298=CARTESIAN_POINT('Ctrl Pts',(109.391916905451,21.7201258288473,32.5536252714697));
#106299=CARTESIAN_POINT('Ctrl Pts',(110.295599756851,21.6567348930296,32.383843709888));
#106300=CARTESIAN_POINT('Ctrl Pts',(110.929578279781,21.5933439572118,33.0497480349151));
#106301=CARTESIAN_POINT('Ctrl Pts',(110.715579822584,21.5299530213941,33.9439743507063));
#106302=CARTESIAN_POINT('Ctrl Pts',(109.848790722007,21.4665620855764,34.25072655027));
#106303=CARTESIAN_POINT('Ctrl Pts',(109.119945421257,21.4031711497586,33.6901947344439));
#106304=CARTESIAN_POINT('Ctrl Pts',(109.193919120223,21.3397802139409,32.7737087486158));
#106305=CARTESIAN_POINT('Ctrl Pts',(110.003232787343,21.2763892781232,32.3373274621601));
#106306=CARTESIAN_POINT('Ctrl Pts',(110.809597608227,21.2129983423054,32.779135617356));
#106307=CARTESIAN_POINT('Ctrl Pts',(110.877413755863,21.1496074064877,33.6960938274722));
#106308=CARTESIAN_POINT('Ctrl Pts',(110.144821083357,21.0862164706699,34.2517270095317));
#106309=CARTESIAN_POINT('Ctrl Pts',(109.280109884683,21.0228255348522,33.9391400833441));
#106310=CARTESIAN_POINT('Ctrl Pts',(109.072126276207,20.9594345990345,33.0435396388201));
#106311=CARTESIAN_POINT('Ctrl Pts',(109.710554439841,20.8960436632167,32.381816166027));
#106312=CARTESIAN_POINT('Ctrl Pts',(110.613096278466,20.832652727399,32.5578605213723));
#106313=CARTESIAN_POINT('Ctrl Pts',(110.956206591258,20.7692617915813,33.410563639553));
#106314=CARTESIAN_POINT('Ctrl Pts',(110.427376724679,20.7058708557635,34.1631578432478));
#106315=CARTESIAN_POINT('Ctrl Pts',(109.508176070054,20.6424799199458,34.1267299830714));
#106316=CARTESIAN_POINT('Ctrl Pts',(109.19626384611,20.6002192960673,33.6020895373542));
#106317=CARTESIAN_POINT('Ctrl Pts',(109.185704546974,20.5790889841281,33.3318133429916));
#106318=CARTESIAN_POINT('Ctrl Pts',(110.429877377952,21.99325,32.6988956497206));
#106319=CARTESIAN_POINT('Ctrl Pts',(110.629392425721,21.9721196880608,32.8415780401524));
#106320=CARTESIAN_POINT('Ctrl Pts',(110.871460562011,21.9298590641823,33.3393357713752));
#106321=CARTESIAN_POINT('Ctrl Pts',(110.441011075278,21.8664681283645,34.0539278279709));
#106322=CARTESIAN_POINT('Ctrl Pts',(109.60727954107,21.8030771925468,34.079572693842));
#106323=CARTESIAN_POINT('Ctrl Pts',(109.132198548835,21.7396862567291,33.3946996964141));
#106324=CARTESIAN_POINT('Ctrl Pts',(109.448565202734,21.6762953209113,32.6231566527654));
#106325=CARTESIAN_POINT('Ctrl Pts',(110.268062035357,21.6129043850936,32.4691917393687));
#106326=CARTESIAN_POINT('Ctrl Pts',(110.842979873719,21.5495134492758,33.0730612101061));
#106327=CARTESIAN_POINT('Ctrl Pts',(110.648917258071,21.4861225134581,33.8839824667209));
#106328=CARTESIAN_POINT('Ctrl Pts',(109.86287719836,21.4227315776404,34.1621579965021));
#106329=CARTESIAN_POINT('Ctrl Pts',(109.201930258278,21.3593406418226,33.6538446574342));
#106330=CARTESIAN_POINT('Ctrl Pts',(109.269012655501,21.2959497060049,32.8227374151472));
#106331=CARTESIAN_POINT('Ctrl Pts',(110.002931624722,21.2325587701872,32.4270088899107));
#106332=CARTESIAN_POINT('Ctrl Pts',(110.734176458714,21.1691678343694,32.8276587232552));
#106333=CARTESIAN_POINT('Ctrl Pts',(110.795674934758,21.1057768985517,33.6591941979777));
#106334=CARTESIAN_POINT('Ctrl Pts',(110.131329723613,21.042385962734,34.1630652541699));
#106335=CARTESIAN_POINT('Ctrl Pts',(109.347173990936,20.9789950269162,33.8795985539519));
#106336=CARTESIAN_POINT('Ctrl Pts',(109.158565887862,20.9156040910985,33.0674311808014));
#106337=CARTESIAN_POINT('Ctrl Pts',(109.737518843697,20.8522131552808,32.4673530790804));
#106338=CARTESIAN_POINT('Ctrl Pts',(110.555980958936,20.788822219463,32.6269973518284));
#106339=CARTESIAN_POINT('Ctrl Pts',(110.867127523395,20.7254312836453,33.4002636624968));
#106340=CARTESIAN_POINT('Ctrl Pts',(110.387562817717,20.6620403478275,34.0827470859926));
#106341=CARTESIAN_POINT('Ctrl Pts',(109.553993801946,20.5986494120098,34.04971280191));
#106342=CARTESIAN_POINT('Ctrl Pts',(109.271138949515,20.5563887881313,33.5739472356332));
#106343=CARTESIAN_POINT('Ctrl Pts',(109.261563342117,20.5352584761921,33.3288496498261));
#106344=CARTESIAN_POINT('Origin',(110.,22.1,33.3));
#106345=CARTESIAN_POINT('',(109.330384757729,22.2,33.3));
#106346=CARTESIAN_POINT('Origin',(110.,22.2,33.3));
#106347=CARTESIAN_POINT('',(109.480384757729,22.05,33.3));
#106348=CARTESIAN_POINT('',(109.430384757729,22.1,33.3));
#106349=CARTESIAN_POINT('',(109.543134871874,22.,33.1913136141202));
#106350=CARTESIAN_POINT('Ctrl Pts',(109.543134871874,22.,33.1913136141202));
#106351=CARTESIAN_POINT('Ctrl Pts',(109.513345646292,22.0170391114376,33.2429100663472));
#106352=CARTESIAN_POINT('Ctrl Pts',(109.480384757729,22.05,33.3));
#106353=CARTESIAN_POINT('',(109.67744226472,22.,32.9586863858798));
#106354=CARTESIAN_POINT('Origin',(110.,22.,33.3));
#106355=CARTESIAN_POINT('',(109.740192378865,22.05,32.85));
#106356=CARTESIAN_POINT('Ctrl Pts',(109.740192378865,22.05,32.85));
#106357=CARTESIAN_POINT('Ctrl Pts',(109.707231490302,22.0170391114376,32.9070899336529));
#106358=CARTESIAN_POINT('Ctrl Pts',(109.67744226472,22.,32.9586863858798));
#106359=CARTESIAN_POINT('',(109.865692607155,22.,32.85));
#106360=CARTESIAN_POINT('Ctrl Pts',(109.865692607155,22.,32.85));
#106361=CARTESIAN_POINT('Ctrl Pts',(109.80611415599,22.0170391114376,32.85));
#106362=CARTESIAN_POINT('Ctrl Pts',(109.740192378865,22.05,32.85));
#106363=CARTESIAN_POINT('',(110.134307392845,22.,32.85));
#106364=CARTESIAN_POINT('Origin',(110.,22.,33.3));
#106365=CARTESIAN_POINT('',(110.259807621135,22.05,32.85));
#106366=CARTESIAN_POINT('Ctrl Pts',(110.259807621135,22.05,32.85));
#106367=CARTESIAN_POINT('Ctrl Pts',(110.19388584401,22.0170391114376,32.85));
#106368=CARTESIAN_POINT('Ctrl Pts',(110.134307392845,22.,32.85));
#106369=CARTESIAN_POINT('',(110.32255773528,22.,32.9586863858798));
#106370=CARTESIAN_POINT('Ctrl Pts',(110.32255773528,22.,32.9586863858798));
#106371=CARTESIAN_POINT('Ctrl Pts',(110.292768509698,22.0170391114376,32.9070899336528));
#106372=CARTESIAN_POINT('Ctrl Pts',(110.259807621135,22.05,32.85));
#106373=CARTESIAN_POINT('',(110.456865128126,22.,33.1913136141202));
#106374=CARTESIAN_POINT('Origin',(110.,22.,33.3));
#106375=CARTESIAN_POINT('',(110.519615242271,22.05,33.3));
#106376=CARTESIAN_POINT('Ctrl Pts',(110.519615242271,22.05,33.3));
#106377=CARTESIAN_POINT('Ctrl Pts',(110.486654353708,22.0170391114376,33.2429100663471));
#106378=CARTESIAN_POINT('Ctrl Pts',(110.456865128126,22.,33.1913136141202));
#106379=CARTESIAN_POINT('',(110.456865128126,22.,33.4086863858798));
#106380=CARTESIAN_POINT('Ctrl Pts',(110.456865128126,22.,33.4086863858798));
#106381=CARTESIAN_POINT('Ctrl Pts',(110.486654353708,22.0170391114376,33.3570899336528));
#106382=CARTESIAN_POINT('Ctrl Pts',(110.519615242271,22.05,33.3));
#106383=CARTESIAN_POINT('',(110.32255773528,22.,33.6413136141202));
#106384=CARTESIAN_POINT('Origin',(110.,22.,33.3));
#106385=CARTESIAN_POINT('',(110.259807621135,22.05,33.75));
#106386=CARTESIAN_POINT('Ctrl Pts',(110.259807621135,22.05,33.75));
#106387=CARTESIAN_POINT('Ctrl Pts',(110.292768509698,22.0170391114376,33.6929100663471));
#106388=CARTESIAN_POINT('Ctrl Pts',(110.32255773528,22.,33.6413136141202));
#106389=CARTESIAN_POINT('',(110.134307392845,22.,33.75));
#106390=CARTESIAN_POINT('Ctrl Pts',(110.134307392845,22.,33.75));
#106391=CARTESIAN_POINT('Ctrl Pts',(110.19388584401,22.0170391114376,33.75));
#106392=CARTESIAN_POINT('Ctrl Pts',(110.259807621135,22.05,33.75));
#106393=CARTESIAN_POINT('',(109.865692607155,22.,33.75));
#106394=CARTESIAN_POINT('Origin',(110.,22.,33.3));
#106395=CARTESIAN_POINT('',(109.740192378865,22.05,33.75));
#106396=CARTESIAN_POINT('Ctrl Pts',(109.740192378865,22.05,33.75));
#106397=CARTESIAN_POINT('Ctrl Pts',(109.80611415599,22.0170391114376,33.75));
#106398=CARTESIAN_POINT('Ctrl Pts',(109.865692607155,22.,33.75));
#106399=CARTESIAN_POINT('',(109.67744226472,22.,33.6413136141202));
#106400=CARTESIAN_POINT('Ctrl Pts',(109.67744226472,22.,33.6413136141202));
#106401=CARTESIAN_POINT('Ctrl Pts',(109.707231490302,22.0170391114376,33.6929100663472));
#106402=CARTESIAN_POINT('Ctrl Pts',(109.740192378865,22.05,33.75));
#106403=CARTESIAN_POINT('',(109.543134871874,22.,33.4086863858798));
#106404=CARTESIAN_POINT('Origin',(110.,22.,33.3));
#106405=CARTESIAN_POINT('Ctrl Pts',(109.480384757729,22.05,33.3));
#106406=CARTESIAN_POINT('Ctrl Pts',(109.513345646292,22.0170391114376,33.3570899336529));
#106407=CARTESIAN_POINT('Ctrl Pts',(109.543134871874,22.,33.4086863858798));
#106408=CARTESIAN_POINT('Origin',(110.,22.1,33.3));
#106409=CARTESIAN_POINT('',(110.134307392845,22.2,32.85));
#106410=CARTESIAN_POINT('',(110.134307392845,22.1,32.85));
#106411=CARTESIAN_POINT('',(109.865692607155,22.2,32.85));
#106412=CARTESIAN_POINT('',(109.865692607155,22.1,32.85));
#106413=CARTESIAN_POINT('Origin',(110.,22.2,33.3));
#106414=CARTESIAN_POINT('Origin',(110.,22.1,33.3));
#106415=CARTESIAN_POINT('',(110.456865128126,22.2,33.1913136141202));
#106416=CARTESIAN_POINT('',(110.456865128126,22.1,33.1913136141202));
#106417=CARTESIAN_POINT('',(110.32255773528,22.2,32.9586863858798));
#106418=CARTESIAN_POINT('',(110.32255773528,22.1,32.9586863858798));
#106419=CARTESIAN_POINT('Origin',(110.,22.2,33.3));
#106420=CARTESIAN_POINT('Origin',(110.,22.1,33.3));
#106421=CARTESIAN_POINT('',(109.543134871874,22.2,33.1913136141202));
#106422=CARTESIAN_POINT('',(109.543134871874,22.1,33.1913136141202));
#106423=CARTESIAN_POINT('',(109.67744226472,22.2,32.9586863858798));
#106424=CARTESIAN_POINT('Origin',(110.,22.2,33.3));
#106425=CARTESIAN_POINT('',(109.67744226472,22.1,32.9586863858798));
#106426=CARTESIAN_POINT('Origin',(110.,22.1,33.3));
#106427=CARTESIAN_POINT('',(110.32255773528,22.2,33.6413136141202));
#106428=CARTESIAN_POINT('',(110.32255773528,22.1,33.6413136141202));
#106429=CARTESIAN_POINT('',(110.456865128126,22.2,33.4086863858798));
#106430=CARTESIAN_POINT('',(110.456865128126,22.1,33.4086863858798));
#106431=CARTESIAN_POINT('Origin',(110.,22.2,33.3));
#106432=CARTESIAN_POINT('Origin',(110.,22.1,33.3));
#106433=CARTESIAN_POINT('',(109.67744226472,22.2,33.6413136141202));
#106434=CARTESIAN_POINT('',(109.67744226472,22.1,33.6413136141202));
#106435=CARTESIAN_POINT('',(109.543134871874,22.2,33.4086863858798));
#106436=CARTESIAN_POINT('Origin',(110.,22.2,33.3));
#106437=CARTESIAN_POINT('',(109.543134871874,22.1,33.4086863858798));
#106438=CARTESIAN_POINT('Origin',(110.,22.1,33.3));
#106439=CARTESIAN_POINT('',(110.134307392845,22.2,33.75));
#106440=CARTESIAN_POINT('',(110.134307392845,22.1,33.75));
#106441=CARTESIAN_POINT('',(109.865692607155,22.2,33.75));
#106442=CARTESIAN_POINT('Origin',(110.,22.2,33.3));
#106443=CARTESIAN_POINT('',(109.865692607155,22.1,33.75));
#106444=CARTESIAN_POINT('Origin',(110.519615242271,22.2,33.3));
#106445=CARTESIAN_POINT('',(110.549663336987,22.2,33.247955173281));
#106446=CARTESIAN_POINT('',(110.519615242271,21.4,33.3));
#106447=CARTESIAN_POINT('',(110.519615242271,22.2,33.3));
#106448=CARTESIAN_POINT('',(110.259807621135,21.4,33.75));
#106449=CARTESIAN_POINT('',(110.519615242271,21.4,33.3));
#106450=CARTESIAN_POINT('',(110.259807621135,22.2,33.75));
#106451=CARTESIAN_POINT('Origin',(110.259807621135,22.2,32.85));
#106452=CARTESIAN_POINT('',(110.419759526419,22.2,33.127044826719));
#106453=CARTESIAN_POINT('',(110.259807621135,21.4,32.85));
#106454=CARTESIAN_POINT('',(110.259807621135,22.2,32.85));
#106455=CARTESIAN_POINT('',(110.259807621135,21.4,32.85));
#106456=CARTESIAN_POINT('Origin',(109.740192378865,22.2,32.85));
#106457=CARTESIAN_POINT('',(110.250096189432,22.2,32.85));
#106458=CARTESIAN_POINT('',(109.740192378865,21.4,32.85));
#106459=CARTESIAN_POINT('',(109.740192378865,22.2,32.85));
#106460=CARTESIAN_POINT('',(109.740192378865,21.4,32.85));
#106461=CARTESIAN_POINT('Origin',(110.76,22.2,33.3));
#106462=CARTESIAN_POINT('Origin',(110.76,22.2,33.3));
#106463=CARTESIAN_POINT('Origin',(110.76,22.2,33.3));
#106464=CARTESIAN_POINT('',(109.640336663013,22.2,33.022955173281));
#106465=CARTESIAN_POINT('Origin',(110.76,22.2,33.3));
#106466=CARTESIAN_POINT('Origin',(110.76,22.2,33.3));
#106467=CARTESIAN_POINT('',(109.770240473581,22.2,33.802044826719));
#106468=CARTESIAN_POINT('Origin',(110.76,22.2,33.3));
#106469=CARTESIAN_POINT('',(110.509903810568,22.2,33.75));
#106470=CARTESIAN_POINT('Origin',(110.519615242271,21.4,33.3));
#106471=CARTESIAN_POINT('',(109.480384757729,21.4,33.3));
#106472=CARTESIAN_POINT('',(109.480384757729,21.4,33.3));
#106473=CARTESIAN_POINT('Origin',(110.,21.4,33.3));
#106474=CARTESIAN_POINT('Origin',(110.519615242271,21.4,33.3));
#106475=CARTESIAN_POINT('Origin',(110.,21.4,33.3));
#106476=CARTESIAN_POINT('Origin',(110.519615242271,21.4,33.3));
#106477=CARTESIAN_POINT('Origin',(110.,21.4,33.3));
#106478=CARTESIAN_POINT('Origin',(110.519615242271,21.4,33.3));
#106479=CARTESIAN_POINT('Origin',(110.,21.4,33.3));
#106480=CARTESIAN_POINT('Origin',(110.519615242271,21.4,33.3));
#106481=CARTESIAN_POINT('',(109.740192378865,21.4,33.75));
#106482=CARTESIAN_POINT('',(110.259807621135,21.4,33.75));
#106483=CARTESIAN_POINT('Origin',(110.,21.4,33.3));
#106484=CARTESIAN_POINT('Origin',(110.519615242271,21.4,33.3));
#106485=CARTESIAN_POINT('',(109.740192378865,21.4,33.75));
#106486=CARTESIAN_POINT('Origin',(110.,21.4,33.3));
#106487=CARTESIAN_POINT('Origin',(110.,21.4,33.3));
#106488=CARTESIAN_POINT('',(110.,21.0877836638731,33.3));
#106489=CARTESIAN_POINT('',(109.480384757729,21.4,33.3));
#106490=CARTESIAN_POINT('Origin',(109.480384757729,22.2,33.3));
#106491=CARTESIAN_POINT('',(109.480384757729,22.2,33.3));
#106492=CARTESIAN_POINT('Origin',(109.740192378865,22.2,33.75));
#106493=CARTESIAN_POINT('',(109.740192378865,22.2,33.75));
#106494=CARTESIAN_POINT('Origin',(110.259807621135,22.2,33.75));
#106495=CARTESIAN_POINT('Origin',(110.76,22.2,33.3));
#106496=CARTESIAN_POINT('',(109.24,22.2,33.3));
#106497=CARTESIAN_POINT('Origin',(110.,22.2,33.3));
#106498=CARTESIAN_POINT('Origin',(110.,22.08,33.3));
#106499=CARTESIAN_POINT('',(109.12,22.08,33.3));
#106500=CARTESIAN_POINT('Origin',(110.,21.33,33.3));
#106501=CARTESIAN_POINT('Origin',(110.,20.66675,33.3));
#106502=CARTESIAN_POINT('Origin',(110.,20.45,33.3));
#106503=CARTESIAN_POINT('',(109.5,20.2,33.3));
#106504=CARTESIAN_POINT('Origin',(110.,20.2,33.3));
#106505=CARTESIAN_POINT('',(109.25,20.45,33.3));
#106506=CARTESIAN_POINT('Origin',(110.,20.2,33.3));
#106507=CARTESIAN_POINT('',(0.,0.,0.));
#106508=CARTESIAN_POINT('Origin',(98.,10.75,11.7549960127668));
#106509=CARTESIAN_POINT('',(96.5351020985542,10.7510579807298,9.27915105860971));
#106510=CARTESIAN_POINT('',(96.5354401179964,10.7513381115446,9.20784096692389));
#106511=CARTESIAN_POINT('',(96.5365,10.75,11.7549960127668));
#106512=CARTESIAN_POINT('',(98.6347992875354,12.0698446533255,9.1184960127668));
#106513=CARTESIAN_POINT('Ctrl Pts',(96.5351020985542,10.7510579807298,9.27915105860971));
#106514=CARTESIAN_POINT('Ctrl Pts',(96.5346060590799,10.8145630912322,9.27568846090188));
#106515=CARTESIAN_POINT('Ctrl Pts',(96.5383821988364,10.878006616392,9.27222586319404));
#106516=CARTESIAN_POINT('Ctrl Pts',(96.5466319128065,10.9408598239014,9.26876326548621));
#106517=CARTESIAN_POINT('Ctrl Pts',(96.609221767305,11.4177215826278,9.24249284114118));
#106518=CARTESIAN_POINT('Ctrl Pts',(96.9293160773523,11.8606039284948,9.21622241679615));
#106519=CARTESIAN_POINT('Ctrl Pts',(97.3625071015607,12.069892529637,9.18995199245112));
#106520=CARTESIAN_POINT('Ctrl Pts',(97.7552693021089,12.2596486578589,9.16613333255634));
#106521=CARTESIAN_POINT('Ctrl Pts',(98.2410031353653,12.2573780592344,9.14231467266158));
#106522=CARTESIAN_POINT('Ctrl Pts',(98.6355914804955,12.0706490290142,9.1184960127668));
#106523=CARTESIAN_POINT('',(97.3659929054248,12.0690402776368,9.1184960127668));
#106524=CARTESIAN_POINT('Origin',(98.,10.75,9.1184960127668));
#106525=CARTESIAN_POINT('Ctrl Pts',(97.3659929054248,12.0690402776368,9.1184960127668));
#106526=CARTESIAN_POINT('Ctrl Pts',(96.930546199862,11.8597393902289,9.14476643711183));
#106527=CARTESIAN_POINT('Ctrl Pts',(96.6105106946804,11.419616133128,9.17103686145686));
#106528=CARTESIAN_POINT('Ctrl Pts',(96.5472508070897,10.9435820611701,9.19730728580189));
#106529=CARTESIAN_POINT('Ctrl Pts',(96.5387956780449,10.8799567582901,9.20081851284256));
#106530=CARTESIAN_POINT('Ctrl Pts',(96.5349276407975,10.8156899373181,9.20432973988323));
#106531=CARTESIAN_POINT('Ctrl Pts',(96.5354401179964,10.7513381115446,9.20784096692389));
#106532=CARTESIAN_POINT('Origin',(98.,10.75,11.7549960127668));
#106533=CARTESIAN_POINT('',(96.5387662976346,10.750184760568,9.7791510586097));
#106534=CARTESIAN_POINT('',(96.5387723473756,10.7501752126031,9.70784096692389));
#106535=CARTESIAN_POINT('',(96.5365,10.75,11.7549960127668));
#106536=CARTESIAN_POINT('Ctrl Pts',(96.5387662976346,10.750184760568,9.7791510586097));
#106537=CARTESIAN_POINT('Ctrl Pts',(96.538503535619,10.9810513320239,9.76664434030537));
#106538=CARTESIAN_POINT('Ctrl Pts',(96.590063734169,11.2118067540368,9.75413762200105));
#106539=CARTESIAN_POINT('Ctrl Pts',(96.6940778839653,11.415818168987,9.74163090369672));
#106540=CARTESIAN_POINT('Ctrl Pts',(96.9125601257928,11.8443451663622,9.71536047935169));
#106541=CARTESIAN_POINT('Ctrl Pts',(97.3624755610563,12.1548743616133,9.68909005500666));
#106542=CARTESIAN_POINT('Ctrl Pts',(97.8406352022483,12.20717006172,9.66281963066163));
#106543=CARTESIAN_POINT('Ctrl Pts',(98.3187948434403,12.2594657618267,9.63654920631661));
#106544=CARTESIAN_POINT('Ctrl Pts',(98.8251986905609,12.053527966789,9.61027878197158));
#106545=CARTESIAN_POINT('Ctrl Pts',(99.1311396738187,11.6823507781742,9.58400835762655));
#106546=CARTESIAN_POINT('Ctrl Pts',(99.4370806570765,11.3111735895595,9.55773793328152));
#106547=CARTESIAN_POINT('Ctrl Pts',(99.5425587764715,10.7747570073677,9.53146750893649));
#106548=CARTESIAN_POINT('Ctrl Pts',(99.3999470419584,10.3153816915692,9.50519708459146));
#106549=CARTESIAN_POINT('Ctrl Pts',(99.2573353074454,9.85600637577063,9.47892666024643));
#106550=CARTESIAN_POINT('Ctrl Pts',(98.8666337190244,9.47367232636532,9.4526562359014));
#106551=CARTESIAN_POINT('Ctrl Pts',(98.4042727797815,9.3410015425033,9.42638581155638));
#106552=CARTESIAN_POINT('Ctrl Pts',(97.9419118405387,9.20833075864129,9.40011538721135));
#106553=CARTESIAN_POINT('Ctrl Pts',(97.4078915504739,9.32532324032258,9.37384496286631));
#106554=CARTESIAN_POINT('Ctrl Pts',(97.0434241049163,9.63924006695603,9.34757453852129));
#106555=CARTESIAN_POINT('Ctrl Pts',(96.7269956299132,9.91178079436568,9.32476671188409));
#106556=CARTESIAN_POINT('Ctrl Pts',(96.5383694669553,10.3327554018202,9.3019588852469));
#106557=CARTESIAN_POINT('Ctrl Pts',(96.5351020985542,10.7510579807298,9.27915105860971));
#106558=CARTESIAN_POINT('Ctrl Pts',(96.5354401179964,10.7513381115446,9.20784096692389));
#106559=CARTESIAN_POINT('Ctrl Pts',(96.5387619110758,10.3342201403306,9.23060016422825));
#106560=CARTESIAN_POINT('Ctrl Pts',(96.726127496539,9.91353076072674,9.25335936153261));
#106561=CARTESIAN_POINT('Ctrl Pts',(97.0412798458648,9.64082474825794,9.27611855883697));
#106562=CARTESIAN_POINT('Ctrl Pts',(97.4050530422302,9.32604639411874,9.302388983182));
#106563=CARTESIAN_POINT('Ctrl Pts',(97.939083704961,9.20843457265531,9.32865940752703));
#106564=CARTESIAN_POINT('Ctrl Pts',(98.4017442787636,9.34034906364773,9.35492983187206));
#106565=CARTESIAN_POINT('Ctrl Pts',(98.8644048525662,9.47226355464014,9.38120025621709));
#106566=CARTESIAN_POINT('Ctrl Pts',(99.2556953374407,9.85370435808839,9.40747068056212));
#106567=CARTESIAN_POINT('Ctrl Pts',(99.3991207985907,10.3127728125,9.43374110490715));
#106568=CARTESIAN_POINT('Ctrl Pts',(99.5425462597407,10.7718412669117,9.46001152925217));
#106569=CARTESIAN_POINT('Ctrl Pts',(99.4381066971662,11.3085373722868,9.4862819535972));
#106570=CARTESIAN_POINT('Ctrl Pts',(99.1328605939268,11.6802968798121,9.51255237794223));
#106571=CARTESIAN_POINT('Ctrl Pts',(98.8276144906875,12.0520563873375,9.53882280228726));
#106572=CARTESIAN_POINT('Ctrl Pts',(98.3215618467832,12.2588792970132,9.56509322663229));
#106573=CARTESIAN_POINT('Ctrl Pts',(97.8433002185608,12.2074494086105,9.59136365097732));
#106574=CARTESIAN_POINT('Ctrl Pts',(97.3650385903383,12.1560195202078,9.61763407532235));
#106575=CARTESIAN_POINT('Ctrl Pts',(96.9145679777977,11.8463368337266,9.64390449966737));
#106576=CARTESIAN_POINT('Ctrl Pts',(96.6953038636642,11.4182164216731,9.6701749240124));
#106577=CARTESIAN_POINT('Ctrl Pts',(96.5905116021786,11.2136060760883,9.68273027164956));
#106578=CARTESIAN_POINT('Ctrl Pts',(96.5385302134461,10.9819428591635,9.69528561928673));
#106579=CARTESIAN_POINT('Ctrl Pts',(96.5387723473756,10.7501752126031,9.70784096692389));
#106580=CARTESIAN_POINT('Origin',(98.,10.75,11.7549960127668));
#106581=CARTESIAN_POINT('',(96.5357076024386,10.7488070530836,10.2791510586097));
#106582=CARTESIAN_POINT('',(96.5356817146954,10.7488128621349,10.2078409669239));
#106583=CARTESIAN_POINT('',(96.5365,10.75,11.7549960127668));
#106584=CARTESIAN_POINT('Ctrl Pts',(96.5357076024386,10.7488070530836,10.2791510586097));
#106585=CARTESIAN_POINT('Ctrl Pts',(96.5391927502809,11.1445138219629,10.2576002197089));
#106586=CARTESIAN_POINT('Ctrl Pts',(96.7054282825438,11.5428021399452,10.2360493808081));
#106587=CARTESIAN_POINT('Ctrl Pts',(96.9918932170273,11.8141742722173,10.2144985419072));
#106588=CARTESIAN_POINT('Ctrl Pts',(97.3410933304653,12.1449762935684,10.1882281175622));
#106589=CARTESIAN_POINT('Ctrl Pts',(97.8689489900534,12.2871865058065,10.1619576932172));
#106590=CARTESIAN_POINT('Ctrl Pts',(98.3370695803043,12.1765798886882,10.1356872688721));
#106591=CARTESIAN_POINT('Ctrl Pts',(98.8051901705552,12.0659732715699,10.1094168445271));
#106592=CARTESIAN_POINT('Ctrl Pts',(99.2135756914689,11.7025498250952,10.0831464201821));
#106593=CARTESIAN_POINT('Ctrl Pts',(99.377790641522,11.2504390034582,10.0568759958371));
#106594=CARTESIAN_POINT('Ctrl Pts',(99.5420055915751,10.7983281818212,10.030605571492));
#106595=CARTESIAN_POINT('Ctrl Pts',(99.4620499707675,10.2575299850219,10.004335147147));
#106596=CARTESIAN_POINT('Ctrl Pts',(99.1740335407107,9.87228052451059,9.97806472280198));
#106597=CARTESIAN_POINT('Ctrl Pts',(98.8860171106538,9.4870310639993,9.95179429845695));
#106598=CARTESIAN_POINT('Ctrl Pts',(98.3899398713477,9.25733033977605,9.92552387411192));
#106599=CARTESIAN_POINT('Ctrl Pts',(97.9098404039135,9.28691530384111,9.89925344976689));
#106600=CARTESIAN_POINT('Ctrl Pts',(97.4297409364793,9.31650026790617,9.87298302542186));
#106601=CARTESIAN_POINT('Ctrl Pts',(96.965619240917,9.60537092025954,9.84671260107683));
#106602=CARTESIAN_POINT('Ctrl Pts',(96.7270829173316,10.0230686461859,9.8204421767318));
#106603=CARTESIAN_POINT('Ctrl Pts',(96.6021080103892,10.241910513299,9.8066784706911));
#106604=CARTESIAN_POINT('Ctrl Pts',(96.5390554685469,10.4961149441044,9.7929147646504));
#106605=CARTESIAN_POINT('Ctrl Pts',(96.5387662976346,10.750184760568,9.7791510586097));
#106606=CARTESIAN_POINT('Ctrl Pts',(96.5387723473756,10.7501752126031,9.70784096692389));
#106607=CARTESIAN_POINT('Ctrl Pts',(96.5390368470544,10.4969993434167,9.72155604363176));
#106608=CARTESIAN_POINT('Ctrl Pts',(96.6016181491467,10.2436988613999,9.73527112033962));
#106609=CARTESIAN_POINT('Ctrl Pts',(96.7257506472849,10.0254008549467,9.74898619704748));
#106610=CARTESIAN_POINT('Ctrl Pts',(96.9635191607655,9.60726383789951,9.77525662139251));
#106611=CARTESIAN_POINT('Ctrl Pts',(97.4271138034529,9.31754794143095,9.80152704573755));
#106612=CARTESIAN_POINT('Ctrl Pts',(97.9071590987782,9.28708417413698,9.82779747008257));
#106613=CARTESIAN_POINT('Ctrl Pts',(98.3872043941035,9.256620406843,9.8540678944276));
#106614=CARTESIAN_POINT('Ctrl Pts',(98.8837003420666,9.4854087687236,9.88033831877263));
#106615=CARTESIAN_POINT('Ctrl Pts',(99.1724221784704,9.87012895792189,9.90660874311765));
#106616=CARTESIAN_POINT('Ctrl Pts',(99.4611440148742,10.2548491471202,9.93287916746268));
#106617=CARTESIAN_POINT('Ctrl Pts',(99.5420917397186,10.7955011636361,9.95914959180771));
#106618=CARTESIAN_POINT('Ctrl Pts',(99.3787060978683,11.2479126394726,9.98542001615274));
#106619=CARTESIAN_POINT('Ctrl Pts',(99.215320456018,11.700324115309,10.0116904404978));
#106620=CARTESIAN_POINT('Ctrl Pts',(98.807601447473,12.0644950504659,10.0379608648428));
#106621=CARTESIAN_POINT('Ctrl Pts',(98.3396842729412,12.1759595319847,10.0642312891878));
#106622=CARTESIAN_POINT('Ctrl Pts',(97.8717670984094,12.2874240135035,10.0905017135329));
#106623=CARTESIAN_POINT('Ctrl Pts',(97.3436517578907,12.1461820413841,10.1167721378779));
#106624=CARTESIAN_POINT('Ctrl Pts',(96.9938457937009,11.8160208042116,10.1430425622229));
#106625=CARTESIAN_POINT('Ctrl Pts',(96.706236324123,11.5445631733553,10.1646420304566));
#106626=CARTESIAN_POINT('Ctrl Pts',(96.5391654491034,11.1453945765175,10.1862414986902));
#106627=CARTESIAN_POINT('Ctrl Pts',(96.5356817146954,10.7488128621349,10.2078409669239));
#106628=CARTESIAN_POINT('Origin',(98.,10.75,11.7549960127668));
#106629=CARTESIAN_POINT('',(96.5355008698795,10.7511408312974,10.7791510586097));
#106630=CARTESIAN_POINT('',(96.5355258561876,10.7511478400734,10.7078409669239));
#106631=CARTESIAN_POINT('',(96.5365,10.75,11.7549960127668));
#106632=CARTESIAN_POINT('Ctrl Pts',(96.5355008698795,10.7511408312974,10.7791510586097));
#106633=CARTESIAN_POINT('Ctrl Pts',(96.5348195355476,10.8305169224741,10.7748265234574));
#106634=CARTESIAN_POINT('Ctrl Pts',(96.5407253171912,10.9097915622436,10.7705019883051));
#106635=CARTESIAN_POINT('Ctrl Pts',(96.5535773406929,10.9879236072814,10.7661774531528));
#106636=CARTESIAN_POINT('Ctrl Pts',(96.631650035027,11.4625554245303,10.7399070288078));
#106637=CARTESIAN_POINT('Ctrl Pts',(96.966056138436,11.8950226859328,10.7136366044628));
#106638=CARTESIAN_POINT('Ctrl Pts',(97.4057708655159,12.0900141373515,10.6873661801177));
#106639=CARTESIAN_POINT('Ctrl Pts',(97.8454855925959,12.2850055887703,10.6610957557727));
#106640=CARTESIAN_POINT('Ctrl Pts',(98.3905089433467,12.2425212302052,10.6348253314277));
#106641=CARTESIAN_POINT('Ctrl Pts',(98.7946969823958,11.9817478870923,10.6085549070827));
#106642=CARTESIAN_POINT('Ctrl Pts',(99.198885021445,11.7209745439793,10.5822844827376));
#106643=CARTESIAN_POINT('Ctrl Pts',(99.4622377487925,11.2419122163185,10.5560140583926));
#106644=CARTESIAN_POINT('Ctrl Pts',(99.465819567919,10.7609154609234,10.5297436340476));
#106645=CARTESIAN_POINT('Ctrl Pts',(99.4694013870456,10.2799187055283,10.5034732097025));
#106646=CARTESIAN_POINT('Ctrl Pts',(99.2132122979512,9.796987522399,10.4772027853575));
#106647=CARTESIAN_POINT('Ctrl Pts',(98.812952649374,9.5302237317626,10.4509323610125));
#106648=CARTESIAN_POINT('Ctrl Pts',(98.4126930007967,9.2634599411262,10.4246619366675));
#106649=CARTESIAN_POINT('Ctrl Pts',(97.8683627927365,9.21286354298272,10.3983915123224));
#106650=CARTESIAN_POINT('Ctrl Pts',(97.4257929194293,9.40128491809413,10.3721210879774));
#106651=CARTESIAN_POINT('Ctrl Pts',(96.9832230461221,9.58970629320554,10.3458506636324));
#106652=CARTESIAN_POINT('Ctrl Pts',(96.6424135075679,10.0171454415718,10.3195802392873));
#106653=CARTESIAN_POINT('Ctrl Pts',(96.5572810219347,10.490561930987,10.2933098149423));
#106654=CARTESIAN_POINT('Ctrl Pts',(96.5419866348039,10.5756130722684,10.2885902294981));
#106655=CARTESIAN_POINT('Ctrl Pts',(96.534944362868,10.6621481571042,10.2838706440539));
#106656=CARTESIAN_POINT('Ctrl Pts',(96.5357076024386,10.7488070530836,10.2791510586097));
#106657=CARTESIAN_POINT('Ctrl Pts',(96.5356817146954,10.7488128621349,10.2078409669239));
#106658=CARTESIAN_POINT('Ctrl Pts',(96.5349283456612,10.6630507608455,10.2125119230353));
#106659=CARTESIAN_POINT('Ctrl Pts',(96.5418252088114,10.5774096363722,10.2171828791466));
#106660=CARTESIAN_POINT('Ctrl Pts',(96.5568076622876,10.4932072156605,10.221853835258));
#106661=CARTESIAN_POINT('Ctrl Pts',(96.6410720829249,10.0196353665074,10.248124259603));
#106662=CARTESIAN_POINT('Ctrl Pts',(96.9810975120607,9.59157217042678,10.2743946839481));
#106663=CARTESIAN_POINT('Ctrl Pts',(97.4233212663288,9.40233975759363,10.3006651082931));
#106664=CARTESIAN_POINT('Ctrl Pts',(97.8655450205969,9.21310734476048,10.3269355326381));
#106665=CARTESIAN_POINT('Ctrl Pts',(98.4099670999973,9.26270571517481,10.3532059569831));
#106666=CARTESIAN_POINT('Ctrl Pts',(98.8107151614298,9.52873528490133,10.3794763813282));
#106667=CARTESIAN_POINT('Ctrl Pts',(99.2114632228624,9.79476485462785,10.4057468056732));
#106668=CARTESIAN_POINT('Ctrl Pts',(99.4685372663271,10.2772256236666,10.4320172300182));
#106669=CARTESIAN_POINT('Ctrl Pts',(99.4658372583905,10.7582281877286,10.4582876543633));
#106670=CARTESIAN_POINT('Ctrl Pts',(99.4631372504539,11.2392307517907,10.4845580787083));
#106671=CARTESIAN_POINT('Ctrl Pts',(99.200663191116,11.7187751108762,10.5108285030533));
#106672=CARTESIAN_POINT('Ctrl Pts',(98.7969538623296,11.9802890289434,10.5370989273983));
#106673=CARTESIAN_POINT('Ctrl Pts',(98.3932445335432,12.2418029470106,10.5633693517434));
#106674=CARTESIAN_POINT('Ctrl Pts',(97.8482999353083,12.2852864240596,10.5896397760884));
#106675=CARTESIAN_POINT('Ctrl Pts',(97.4082284316461,12.0911014038513,10.6159102004334));
#106676=CARTESIAN_POINT('Ctrl Pts',(96.9681569279837,11.8969163836431,10.6421806247785));
#106677=CARTESIAN_POINT('Ctrl Pts',(96.632958518894,11.4650628661776,10.6684510491235));
#106678=CARTESIAN_POINT('Ctrl Pts',(96.5540158140872,10.9905749299596,10.6947214734685));
#106679=CARTESIAN_POINT('Ctrl Pts',(96.5408744415503,10.9115882427239,10.6990946379536));
#106680=CARTESIAN_POINT('Ctrl Pts',(96.5348342566888,10.8314200988262,10.7034678024388));
#106681=CARTESIAN_POINT('Ctrl Pts',(96.5355258561876,10.7511478400734,10.7078409669239));
#106682=CARTESIAN_POINT('Origin',(98.,10.75,11.7549960127668));
#106683=CARTESIAN_POINT('',(96.5387850105563,10.7499314378747,11.2791510586097));
#106684=CARTESIAN_POINT('',(96.5387834722467,10.7499171729064,11.2078409669239));
#106685=CARTESIAN_POINT('',(96.5365,10.75,11.7549960127668));
#106686=CARTESIAN_POINT('Ctrl Pts',(96.5387850105563,10.7499314378747,11.2791510586097));
#106687=CARTESIAN_POINT('Ctrl Pts',(96.5388896036327,10.9967165449052,11.2657824028609));
#106688=CARTESIAN_POINT('Ctrl Pts',(96.5981895170845,11.2435488522249,11.2524137471121));
#106689=CARTESIAN_POINT('Ctrl Pts',(96.7163984162244,11.4578934427831,11.2390450913634));
#106690=CARTESIAN_POINT('Ctrl Pts',(96.9486878849727,11.8790968499048,11.2127746670183));
#106691=CARTESIAN_POINT('Ctrl Pts',(97.4084557934653,12.1748481713484,11.1865042426733));
#106692=CARTESIAN_POINT('Ctrl Pts',(97.8880613453677,12.2115799293275,11.1602338183283));
#106693=CARTESIAN_POINT('Ctrl Pts',(98.3676668972702,12.2483116873066,11.1339633939832));
#106694=CARTESIAN_POINT('Ctrl Pts',(98.8671100925825,12.0260238818212,11.1076929696382));
#106695=CARTESIAN_POINT('Ctrl Pts',(99.1608319462644,11.6451063315194,11.0814225452932));
#106696=CARTESIAN_POINT('Ctrl Pts',(99.4545537999463,11.2641887812175,11.0551521209481));
#106697=CARTESIAN_POINT('Ctrl Pts',(99.5425543119979,10.7246414860992,11.0288816966031));
#106698=CARTESIAN_POINT('Ctrl Pts',(99.3850906120084,10.2701352807983,11.0026112722581));
#106699=CARTESIAN_POINT('Ctrl Pts',(99.2276269120188,9.8156290754975,10.9763408479131));
#106700=CARTESIAN_POINT('Ctrl Pts',(98.8246989999881,9.44616396001416,10.950070423568));
#106701=CARTESIAN_POINT('Ctrl Pts',(98.3582775419532,9.3285981021577,10.923799999223));
#106702=CARTESIAN_POINT('Ctrl Pts',(97.8918560839184,9.21103224430123,10.897529574878));
#106703=CARTESIAN_POINT('Ctrl Pts',(97.3619410798795,9.34536564407164,10.8712591505329));
#106704=CARTESIAN_POINT('Ctrl Pts',(97.0078532204896,9.67093053050446,10.8449887261879));
#106705=CARTESIAN_POINT('Ctrl Pts',(96.7120539283044,9.94290219068257,10.8230428369952));
#106706=CARTESIAN_POINT('Ctrl Pts',(96.5389584641005,10.3483278490524,10.8010969478024));
#106707=CARTESIAN_POINT('Ctrl Pts',(96.5355008698795,10.7511408312974,10.7791510586097));
#106708=CARTESIAN_POINT('Ctrl Pts',(96.5355258561876,10.7511478400734,10.7078409669239));
#106709=CARTESIAN_POINT('Ctrl Pts',(96.5389888253935,10.3492094918976,10.7297382267838));
#106710=CARTESIAN_POINT('Ctrl Pts',(96.7112306802982,9.94466078244129,10.7516354866437));
#106711=CARTESIAN_POINT('Ctrl Pts',(97.005876554875,9.67275112583176,10.7735327465036));
#106712=CARTESIAN_POINT('Ctrl Pts',(97.3593670009933,9.34653761289245,10.7998031708486));
#106713=CARTESIAN_POINT('Ctrl Pts',(97.8890348937537,9.21123294198437,10.8260735951937));
#106714=CARTESIAN_POINT('Ctrl Pts',(98.3556711437306,9.32794353138054,10.8523440195387));
#106715=CARTESIAN_POINT('Ctrl Pts',(98.8223073937075,9.44465412077671,10.8786144438837));
#106716=CARTESIAN_POINT('Ctrl Pts',(99.2259120009009,9.81337997047714,10.9048848682287));
#106717=CARTESIAN_POINT('Ctrl Pts',(99.3842086892949,10.2675967800744,10.9311552925738));
#106718=CARTESIAN_POINT('Ctrl Pts',(99.5425053776888,10.7218135896718,10.9574257169188));
#106719=CARTESIAN_POINT('Ctrl Pts',(99.4554941472833,11.2615213591659,10.9836961412638));
#106720=CARTESIAN_POINT('Ctrl Pts',(99.1624710883709,11.6429767805759,11.0099665656089));
#106721=CARTESIAN_POINT('Ctrl Pts',(98.8694480294585,12.0244322019858,11.0362369899539));
#106722=CARTESIAN_POINT('Ctrl Pts',(98.3704131420392,12.2476352753116,11.0625074142989));
#106723=CARTESIAN_POINT('Ctrl Pts',(97.8907410107022,12.211782827704,11.0887778386439));
#106724=CARTESIAN_POINT('Ctrl Pts',(97.4110688793651,12.1759303800964,11.115048262989));
#106725=CARTESIAN_POINT('Ctrl Pts',(96.9507595041103,11.8810224115554,11.141318687334));
#106726=CARTESIAN_POINT('Ctrl Pts',(96.7176982190144,11.4602455241283,11.167589111679));
#106727=CARTESIAN_POINT('Ctrl Pts',(96.5986651321274,11.2453390810417,11.1810063967606));
#106728=CARTESIAN_POINT('Ctrl Pts',(96.5389102934636,10.9975994070483,11.1944236818423));
#106729=CARTESIAN_POINT('Ctrl Pts',(96.5387834722467,10.7499171729064,11.2078409669239));
#106730=CARTESIAN_POINT('Origin',(98.,10.75,11.7549960127668));
#106731=CARTESIAN_POINT('',(96.5352653497957,10.7489347653901,11.7791510586097));
#106732=CARTESIAN_POINT('',(96.5352413523044,10.7489434884042,11.7078409669239));
#106733=CARTESIAN_POINT('',(96.5365,10.75,11.7549960127668));
#106734=CARTESIAN_POINT('Ctrl Pts',(96.5352653497957,10.7489347653901,11.7791510586097));
#106735=CARTESIAN_POINT('Ctrl Pts',(96.5386412990586,11.1601452319407,11.7567382822644));
#106736=CARTESIAN_POINT('Ctrl Pts',(96.7200647749387,11.5739666593434,11.7343255059191));
#106737=CARTESIAN_POINT('Ctrl Pts',(97.0269988720097,11.8463644271576,11.7119127295739));
#106738=CARTESIAN_POINT('Ctrl Pts',(97.3867619308914,12.1656468239869,11.6856423052288));
#106739=CARTESIAN_POINT('Ctrl Pts',(97.9189591634772,12.290632740949,11.6593718808838));
#106740=CARTESIAN_POINT('Ctrl Pts',(98.3832391769487,12.1648759258178,11.6331014565388));
#106741=CARTESIAN_POINT('Ctrl Pts',(98.8475191904202,12.0391191106867,11.6068310321937));
#106742=CARTESIAN_POINT('Ctrl Pts',(99.2438819847773,11.6626195634623,11.5805606078487));
#106743=CARTESIAN_POINT('Ctrl Pts',(99.3933218383592,11.2054123482717,11.5542901835037));
#106744=CARTESIAN_POINT('Ctrl Pts',(99.5427616919411,10.7482051330811,11.5280197591587));
#106745=CARTESIAN_POINT('Ctrl Pts',(99.4452786047477,10.2102902499242,11.5017493348136));
#106746=CARTESIAN_POINT('Ctrl Pts',(99.1448979762896,9.834601302112,11.4754789104686));
#106747=CARTESIAN_POINT('Ctrl Pts',(98.8445173478316,9.45891235429976,11.4492084861236));
#106748=CARTESIAN_POINT('Ctrl Pts',(98.3412391781088,9.24544934183213,11.4229380617785));
#106749=CARTESIAN_POINT('Ctrl Pts',(97.8623544067611,9.29061662238126,11.3966676374335));
#106750=CARTESIAN_POINT('Ctrl Pts',(97.3834696354134,9.33578390293038,11.3703972130885));
#106751=CARTESIAN_POINT('Ctrl Pts',(96.9289782624408,9.63958147649625,11.3441267887435));
#106752=CARTESIAN_POINT('Ctrl Pts',(96.7041380904565,10.064808009679,11.3178563643984));
#106753=CARTESIAN_POINT('Ctrl Pts',(96.5937159734788,10.2736426390726,11.3049545958022));
#106754=CARTESIAN_POINT('Ctrl Pts',(96.5386840702901,10.511765057968,11.292052827206));
#106755=CARTESIAN_POINT('Ctrl Pts',(96.5387850105563,10.7499314378747,11.2791510586097));
#106756=CARTESIAN_POINT('Ctrl Pts',(96.5387834722467,10.7499171729064,11.2078409669239));
#106757=CARTESIAN_POINT('Ctrl Pts',(96.5386619833798,10.5126490348939,11.2206941061873));
#106758=CARTESIAN_POINT('Ctrl Pts',(96.5932596645075,10.2754336080251,11.2335472454507));
#106759=CARTESIAN_POINT('Ctrl Pts',(96.7028839945097,10.067184775836,11.2464003847141));
#106760=CARTESIAN_POINT('Ctrl Pts',(96.9269442500378,9.64154672128373,11.2726708090591));
#106761=CARTESIAN_POINT('Ctrl Pts',(97.3808779560309,9.33691641849236,11.2989412334042));
#106762=CARTESIAN_POINT('Ctrl Pts',(97.8596791639475,9.29087127879738,11.3252116577492));
#106763=CARTESIAN_POINT('Ctrl Pts',(98.3384803718641,9.24482613910239,11.3514820820942));
#106764=CARTESIAN_POINT('Ctrl Pts',(98.8421490817041,9.45736616250379,11.3777525064392));
#106765=CARTESIAN_POINT('Ctrl Pts',(99.1432179777445,9.83250383247476,11.4040229307843));
#106766=CARTESIAN_POINT('Ctrl Pts',(99.4442868737849,10.2076415024457,11.4302933551293));
#106767=CARTESIAN_POINT('Ctrl Pts',(99.5427559560256,10.7453768189863,11.4565637794743));
#106768=CARTESIAN_POINT('Ctrl Pts',(99.3941545289882,11.2028572748257,11.4828342038194));
#106769=CARTESIAN_POINT('Ctrl Pts',(99.2455531019507,11.6603377306651,11.5091046281644));
#106770=CARTESIAN_POINT('Ctrl Pts',(98.8498811656352,12.0375633258033,11.5353750525094));
#106771=CARTESIAN_POINT('Ctrl Pts',(98.3858324357713,12.1641710976999,11.5616454768544));
#106772=CARTESIAN_POINT('Ctrl Pts',(97.9217837059074,12.2907788695965,11.5879159011995));
#106773=CARTESIAN_POINT('Ctrl Pts',(97.3893581824952,12.1667688182515,11.6141863255445));
#106774=CARTESIAN_POINT('Ctrl Pts',(97.0290103592619,11.848146474584,11.6404567498895));
#106775=CARTESIAN_POINT('Ctrl Pts',(96.7209103249204,11.575722031597,11.6629181555677));
#106776=CARTESIAN_POINT('Ctrl Pts',(96.5386055516053,11.1610286944639,11.6853795612458));
#106777=CARTESIAN_POINT('Ctrl Pts',(96.5352413523044,10.7489434884042,11.7078409669239));
#106778=CARTESIAN_POINT('Origin',(98.,10.75,11.7549960127668));
#106779=CARTESIAN_POINT('',(96.5359578915487,10.751240120072,12.2791510586097));
#106780=CARTESIAN_POINT('',(96.5359840746412,10.7512441236452,12.2078409669239));
#106781=CARTESIAN_POINT('',(96.5365,10.75,11.7549960127668));
#106782=CARTESIAN_POINT('Ctrl Pts',(96.5359578915487,10.751240120072,12.2791510586097));
#106783=CARTESIAN_POINT('Ctrl Pts',(96.5351035673496,10.8465138711225,12.273964586013));
#106784=CARTESIAN_POINT('Ctrl Pts',(96.5436208912905,10.941635625592,12.2687781134162));
#106785=CARTESIAN_POINT('Ctrl Pts',(96.5620706913964,11.034790195851,12.2635916408195));
#106786=CARTESIAN_POINT('Ctrl Pts',(96.6555222750729,11.5066349891535,12.2373212164744));
#106787=CARTESIAN_POINT('Ctrl Pts',(97.0038020855935,11.9280095818795,12.2110507921294));
#106788=CARTESIAN_POINT('Ctrl Pts',(97.4496196817153,12.1086124014813,12.1847803677844));
#106789=CARTESIAN_POINT('Ctrl Pts',(97.8954372778371,12.289215221083,12.1585099434393));
#106790=CARTESIAN_POINT('Ctrl Pts',(98.43879265956,12.2290462675604,12.1322395190943));
#106791=CARTESIAN_POINT('Ctrl Pts',(98.8342951807105,11.9552790978233,12.1059690947493));
#106792=CARTESIAN_POINT('Ctrl Pts',(99.2297977018609,11.6815119280863,12.0796986704043));
#106793=CARTESIAN_POINT('Ctrl Pts',(99.477447362439,11.1941465421347,12.0534282460592));
#106794=CARTESIAN_POINT('Ctrl Pts',(99.4654004000111,10.7132873338868,12.0271578217142));
#106795=CARTESIAN_POINT('Ctrl Pts',(99.4533534375832,10.2324281256388,12.0008873973692));
#106796=CARTESIAN_POINT('Ctrl Pts',(99.1816098521493,9.75807509509448,11.9746169730242));
#106797=CARTESIAN_POINT('Ctrl Pts',(98.7728947261572,9.5044559845247,11.9483465486791));
#106798=CARTESIAN_POINT('Ctrl Pts',(98.3641796001652,9.25083687395492,11.9220761243341));
#106799=CARTESIAN_POINT('Ctrl Pts',(97.8184929336149,9.21795168335968,11.8958056999891));
#106800=CARTESIAN_POINT('Ctrl Pts',(97.3822782296244,9.42065205209055,11.869535275644));
#106801=CARTESIAN_POINT('Ctrl Pts',(96.9460635256339,9.62335242082142,11.843264851299));
#106802=CARTESIAN_POINT('Ctrl Pts',(96.6193207842032,10.0616383488784,11.816994426954));
#106803=CARTESIAN_POINT('Ctrl Pts',(96.5496138560767,10.5375707512551,11.790724002609));
#106804=CARTESIAN_POINT('Ctrl Pts',(96.5393778283551,10.6074584567573,11.7868663546092));
#106805=CARTESIAN_POINT('Ctrl Pts',(96.5346842872928,10.6781579366151,11.7830087066095));
#106806=CARTESIAN_POINT('Ctrl Pts',(96.5352653497957,10.7489347653901,11.7791510586097));
#106807=CARTESIAN_POINT('Ctrl Pts',(96.5352413523044,10.7489434884042,11.7078409669239));
#106808=CARTESIAN_POINT('Ctrl Pts',(96.5346708493661,10.6790618316311,11.7116499855908));
#106809=CARTESIAN_POINT('Ctrl Pts',(96.5392462443228,10.6092551783963,11.7154590042577));
#106810=CARTESIAN_POINT('Ctrl Pts',(96.5492267123949,10.5402300545035,11.7192680229246));
#106811=CARTESIAN_POINT('Ctrl Pts',(96.6180610118158,10.0641706140802,11.7455384472697));
#106812=CARTESIAN_POINT('Ctrl Pts',(96.943999733712,9.62528636922334,11.7718088716147));
#106813=CARTESIAN_POINT('Ctrl Pts',(97.3798421393641,9.42178661731112,11.7980792959597));
#106814=CARTESIAN_POINT('Ctrl Pts',(97.8156845450163,9.21828686539889,11.8243497203047));
#106815=CARTESIAN_POINT('Ctrl Pts',(98.3614306344244,9.25017160643128,11.8506201446498));
#106816=CARTESIAN_POINT('Ctrl Pts',(98.7706100678667,9.5030410249873,11.8768905689948));
#106817=CARTESIAN_POINT('Ctrl Pts',(99.179789501309,9.75591044354332,11.9031609933398));
#106818=CARTESIAN_POINT('Ctrl Pts',(99.4524022787855,10.229764539623,11.9294314176849));
#106819=CARTESIAN_POINT('Ctrl Pts',(99.4653307725548,10.7106009001884,11.9557018420299));
#106820=CARTESIAN_POINT('Ctrl Pts',(99.4782592663242,11.1914372607538,11.9819722663749));
#106821=CARTESIAN_POINT('Ctrl Pts',(99.2315034763865,11.6792558858049,12.0082426907199));
#106822=CARTESIAN_POINT('Ctrl Pts',(98.8365034745158,11.9537476891712,12.034513115065));
#106823=CARTESIAN_POINT('Ctrl Pts',(98.4415034726451,12.2282394925375,12.06078353941));
#106824=CARTESIAN_POINT('Ctrl Pts',(97.8982592588414,12.2894044742189,12.087053963755));
#106825=CARTESIAN_POINT('Ctrl Pts',(97.4521112735164,12.1096192501782,12.1133243881001));
#106826=CARTESIAN_POINT('Ctrl Pts',(97.0059632881914,11.9298340261375,12.1395948124451));
#106827=CARTESIAN_POINT('Ctrl Pts',(96.6569115313452,11.5090985963747,12.1658652367901));
#106828=CARTESIAN_POINT('Ctrl Pts',(96.562595071327,11.0374258740744,12.1921356611351));
#106829=CARTESIAN_POINT('Ctrl Pts',(96.5437999321489,10.9434321590808,12.1973707630647));
#106830=CARTESIAN_POINT('Ctrl Pts',(96.5351207094314,10.8474156486503,12.2026058649943));
#106831=CARTESIAN_POINT('Ctrl Pts',(96.5359840746412,10.7512441236452,12.2078409669239));
#106832=CARTESIAN_POINT('Origin',(98.,10.75,11.7549960127668));
#106833=CARTESIAN_POINT('',(96.5387213242412,10.7496813739491,12.7791510586097));
#106834=CARTESIAN_POINT('',(96.5387151545458,10.7496675338344,12.7078409669239));
#106835=CARTESIAN_POINT('',(96.5365,10.75,11.7549960127668));
#106836=CARTESIAN_POINT('Ctrl Pts',(96.5387213242412,10.7496813739491,12.7791510586097));
#106837=CARTESIAN_POINT('Ctrl Pts',(96.5392400434179,11.0123491908163,12.7649204654165));
#106838=CARTESIAN_POINT('Ctrl Pts',(96.6068977921477,11.2752662571728,12.7506898722232));
#106839=CARTESIAN_POINT('Ctrl Pts',(96.7400744574238,11.4992221154966,12.73645927903));
#106840=CARTESIAN_POINT('Ctrl Pts',(96.9859255939258,11.9126564223331,12.7101888546849));
#106841=CARTESIAN_POINT('Ctrl Pts',(97.4550593278255,12.1933144229382,12.6839184303399));
#106842=CARTESIAN_POINT('Ctrl Pts',(97.9356050612555,12.2144450977881,12.6576480059949));
#106843=CARTESIAN_POINT('Ctrl Pts',(98.4161507946855,12.2355757726381,12.6313775816499));
#106844=CARTESIAN_POINT('Ctrl Pts',(98.9081085276457,11.9971791217329,12.6051071573048));
#106845=CARTESIAN_POINT('Ctrl Pts',(99.1892998658561,11.6069200553923,12.5788367329598));
#106846=CARTESIAN_POINT('Ctrl Pts',(99.4704912040665,11.2166609890518,12.5525663086148));
#106847=CARTESIAN_POINT('Ctrl Pts',(99.540916147527,10.6745395072759,12.5262958842698));
#106848=CARTESIAN_POINT('Ctrl Pts',(99.3687693201679,10.2253890010137,12.5000254599247));
#106849=CARTESIAN_POINT('Ctrl Pts',(99.1966224928088,9.77623849475159,12.4737550355797));
#106850=CARTESIAN_POINT('Ctrl Pts',(98.7819038946301,9.42005896400319,12.4474846112347));
#106851=CARTESIAN_POINT('Ctrl Pts',(98.311909111808,9.31770852888495,12.4212141868896));
#106852=CARTESIAN_POINT('Ctrl Pts',(97.841914328986,9.21535809376671,12.3949437625446));
#106853=CARTESIAN_POINT('Ctrl Pts',(97.3166433615205,9.36683675427863,12.3686733381996));
#106854=CARTESIAN_POINT('Ctrl Pts',(96.973319556204,9.70373358147408,12.3424029138545));
#106855=CARTESIAN_POINT('Ctrl Pts',(96.6977768984129,9.97411811563489,12.3213189621063));
#106856=CARTESIAN_POINT('Ctrl Pts',(96.5394308743624,10.3639350427664,12.300235010358));
#106857=CARTESIAN_POINT('Ctrl Pts',(96.5359578915487,10.751240120072,12.2791510586097));
#106858=CARTESIAN_POINT('Ctrl Pts',(96.5359840746412,10.7512441236452,12.2078409669239));
#106859=CARTESIAN_POINT('Ctrl Pts',(96.5394531886708,10.3648143916403,12.2288762893393));
#106860=CARTESIAN_POINT('Ctrl Pts',(96.6969909367875,9.97588189162702,12.2499116117548));
#106861=CARTESIAN_POINT('Ctrl Pts',(96.9714030824048,9.70561743447366,12.2709469341702));
#106862=CARTESIAN_POINT('Ctrl Pts',(97.3141087166909,9.36809173201119,12.2972173585153));
#106863=CARTESIAN_POINT('Ctrl Pts',(97.8391011484532,9.21565034192411,12.3234877828603));
#106864=CARTESIAN_POINT('Ctrl Pts',(98.3092828234955,9.31713898191082,12.3497582072053));
#106865=CARTESIAN_POINT('Ctrl Pts',(98.7794644985377,9.41862762189754,12.3760286315503));
#106866=CARTESIAN_POINT('Ctrl Pts',(99.1948354168599,9.77404629195804,12.4022990558954));
#106867=CARTESIAN_POINT('Ctrl Pts',(99.3678053907722,10.2228804926548,12.4285694802404));
#106868=CARTESIAN_POINT('Ctrl Pts',(99.5407753646844,10.6717146933516,12.4548399045854));
#106869=CARTESIAN_POINT('Ctrl Pts',(99.4713443941867,11.2139644246847,12.4811103289305));
#106870=CARTESIAN_POINT('Ctrl Pts',(99.1908689565956,11.6047383753408,12.5073807532755));
#106871=CARTESIAN_POINT('Ctrl Pts',(98.9103935190044,11.9955123259969,12.5336511776205));
#106872=CARTESIAN_POINT('Ctrl Pts',(98.4188736143198,12.234810495976,12.5599216019655));
#106873=CARTESIAN_POINT('Ctrl Pts',(97.9382899039966,12.2145608304758,12.5861920263106));
#106874=CARTESIAN_POINT('Ctrl Pts',(97.4577061936734,12.1943111649755,12.6124624506556));
#106875=CARTESIAN_POINT('Ctrl Pts',(96.9880586777116,11.9145136639958,12.6387328750006));
#106876=CARTESIAN_POINT('Ctrl Pts',(96.7414499895577,11.5015307266915,12.6650032993457));
#106877=CARTESIAN_POINT('Ctrl Pts',(96.607406462557,11.277054898521,12.6792825218717));
#106878=CARTESIAN_POINT('Ctrl Pts',(96.5392583845217,11.0132302528889,12.6935617443978));
#106879=CARTESIAN_POINT('Ctrl Pts',(96.5387151545458,10.7496675338344,12.7078409669239));
#106880=CARTESIAN_POINT('Origin',(98.,10.75,11.7549960127668));
#106881=CARTESIAN_POINT('',(96.5348664968456,10.7491119138617,13.2791510586097));
#106882=CARTESIAN_POINT('',(96.5348456374124,10.749123229052,13.2078409669239));
#106883=CARTESIAN_POINT('',(96.5365,10.75,11.7549960127668));
#106884=CARTESIAN_POINT('Ctrl Pts',(96.5348664968456,10.7491119138617,13.2791510586097));
#106885=CARTESIAN_POINT('Ctrl Pts',(96.5379355734796,11.175832275792,13.25587634482));
#106886=CARTESIAN_POINT('Ctrl Pts',(96.7353719317325,11.6050282494574,13.2326016310302));
#106887=CARTESIAN_POINT('Ctrl Pts',(97.0631318295525,11.8773970516098,13.2093269172405));
#106888=CARTESIAN_POINT('Ctrl Pts',(97.4330780156496,12.1848227014171,13.1830564928955));
#106889=CARTESIAN_POINT('Ctrl Pts',(97.9690548809394,12.292452352062,13.1567860685504));
#106890=CARTESIAN_POINT('Ctrl Pts',(98.4290041376041,12.1516781433137,13.1305156442054));
#106891=CARTESIAN_POINT('Ctrl Pts',(98.8889533942687,12.0109039345654,13.1042452198604));
#106892=CARTESIAN_POINT('Ctrl Pts',(99.2728750423081,11.621725866424,13.0779747955154));
#106893=CARTESIAN_POINT('Ctrl Pts',(99.4073820091069,11.1599049179571,13.0517043711703));
#106894=CARTESIAN_POINT('Ctrl Pts',(99.5418889759057,10.6980839694902,13.0254339468253));
#106895=CARTESIAN_POINT('Ctrl Pts',(99.4269812614638,10.1636201406978,12.9991635224803));
#106896=CARTESIAN_POINT('Ctrl Pts',(99.1145536072369,9.79788845184339,12.9728930981352));
#106897=CARTESIAN_POINT('Ctrl Pts',(98.8021259530099,9.43215676298898,12.9466226737902));
#106898=CARTESIAN_POINT('Ctrl Pts',(98.2921783589979,9.23515721407256,12.9203522494452));
#106899=CARTESIAN_POINT('Ctrl Pts',(97.8150138082797,9.29585892584242,12.8940818251001));
#106900=CARTESIAN_POINT('Ctrl Pts',(97.3378492575615,9.35656063761229,12.8678114007551));
#106901=CARTESIAN_POINT('Ctrl Pts',(96.8934677501372,9.67496361006843,12.8415409764101));
#106902=CARTESIAN_POINT('Ctrl Pts',(96.6825612659772,10.1072704028304,12.8152705520651));
#106903=CARTESIAN_POINT('Ctrl Pts',(96.5859020561848,10.3053981803746,12.8032307209133));
#106904=CARTESIAN_POINT('Ctrl Pts',(96.5382824605045,10.5274505701347,12.7911908897615));
#106905=CARTESIAN_POINT('Ctrl Pts',(96.5387213242412,10.7496813739491,12.7791510586097));
#106906=CARTESIAN_POINT('Ctrl Pts',(96.5387151545458,10.7496675338344,12.7078409669239));
#106907=CARTESIAN_POINT('Ctrl Pts',(96.5382589686252,10.5283365929963,12.7198321687428));
#106908=CARTESIAN_POINT('Ctrl Pts',(96.5854781604418,10.3071903644812,12.7318233705618));
#106909=CARTESIAN_POINT('Ctrl Pts',(96.6813850502399,10.1096866576566,12.7438145723807));
#106910=CARTESIAN_POINT('Ctrl Pts',(96.8914986594218,9.6769938995548,12.7700849967258));
#106911=CARTESIAN_POINT('Ctrl Pts',(97.3352957381316,9.35777675697994,12.7963554210708));
#106912=CARTESIAN_POINT('Ctrl Pts',(97.812348250158,9.29620036345914,12.8226258454158));
#106913=CARTESIAN_POINT('Ctrl Pts',(98.2894007621844,9.23462396993834,12.8488962697608));
#106914=CARTESIAN_POINT('Ctrl Pts',(98.7997087075274,9.43068832547161,12.8751666941059));
#106915=CARTESIAN_POINT('Ctrl Pts',(99.1128063537502,9.79584666845564,12.9014371184509));
#106916=CARTESIAN_POINT('Ctrl Pts',(99.425903999973,10.1610050114397,12.9277075427959));
#106917=CARTESIAN_POINT('Ctrl Pts',(99.5417913470757,10.6952573418744,12.953977967141));
#106918=CARTESIAN_POINT('Ctrl Pts',(99.4081312455337,11.1573241438787,12.980248391486));
#106919=CARTESIAN_POINT('Ctrl Pts',(99.2744711439917,11.6193909458829,13.006518815831));
#106920=CARTESIAN_POINT('Ctrl Pts',(98.8912635938049,12.0092722194565,13.032789240176));
#106921=CARTESIAN_POINT('Ctrl Pts',(98.4315731366753,12.1508894289787,13.0590596645211));
#106922=CARTESIAN_POINT('Ctrl Pts',(97.9718826795457,12.2925066385009,13.0853300888661));
#106923=CARTESIAN_POINT('Ctrl Pts',(97.4357093154733,12.1858597839718,13.1116005132111));
#106924=CARTESIAN_POINT('Ctrl Pts',(97.0652001347814,11.8791128222671,13.1378709375562));
#106925=CARTESIAN_POINT('Ctrl Pts',(96.7362555909916,11.6067774939266,13.1611942806787));
#106926=CARTESIAN_POINT('Ctrl Pts',(96.5378908628165,11.1767192675748,13.1845176238013));
#106927=CARTESIAN_POINT('Ctrl Pts',(96.5348456374124,10.749123229052,13.2078409669239));
#106928=CARTESIAN_POINT('Origin',(98.,10.75,11.7549960127668));
#106929=CARTESIAN_POINT('',(96.5364271352644,10.7512852130388,13.7791510586097));
#106930=CARTESIAN_POINT('',(96.5364532332071,10.7512863178753,13.7078409669239));
#106931=CARTESIAN_POINT('',(96.5365,10.75,11.7549960127668));
#106932=CARTESIAN_POINT('Ctrl Pts',(96.5364271352644,10.7512852130388,13.7791510586097));
#106933=CARTESIAN_POINT('Ctrl Pts',(96.5354273092983,10.8624851060287,13.7731026485685));
#106934=CARTESIAN_POINT('Ctrl Pts',(96.5470462255384,10.9734783641957,13.7670542385273));
#106935=CARTESIAN_POINT('Ctrl Pts',(96.5720796503353,11.0813584317053,13.7610058284861));
#106936=CARTESIAN_POINT('Ctrl Pts',(96.6808088349878,11.5499204393302,13.7347354041411));
#106937=CARTESIAN_POINT('Ctrl Pts',(97.0425997605388,11.959752792851,13.708464979796));
#106938=CARTESIAN_POINT('Ctrl Pts',(97.4940508333205,12.1257751154429,13.682194555451));
#106939=CARTESIAN_POINT('Ctrl Pts',(97.9455019061022,12.2917974380347,13.655924131106));
#106940=CARTESIAN_POINT('Ctrl Pts',(98.4866131261147,12.2140097296976,13.6296537067609));
#106941=CARTESIAN_POINT('Ctrl Pts',(98.8730119243886,11.9275383591108,13.6033832824159));
#106942=CARTESIAN_POINT('Ctrl Pts',(99.2594107226625,11.6410669885239,13.5771128580709));
#106943=CARTESIAN_POINT('Ctrl Pts',(99.4910970991978,11.1459119556874,13.5508424337259));
#106944=CARTESIAN_POINT('Ctrl Pts',(99.4634343896403,10.6656976884966,13.5245720093808));
#106945=CARTESIAN_POINT('Ctrl Pts',(99.4357716800828,10.1854834213057,13.4983015850358));
#106946=CARTESIAN_POINT('Ctrl Pts',(99.1487598844324,9.72020991976056,13.4720311606908));
#106947=CARTESIAN_POINT('Ctrl Pts',(98.7320206410468,9.48000340079889,13.4457607363457));
#106948=CARTESIAN_POINT('Ctrl Pts',(98.3152813976611,9.23979688183723,13.4194903120007));
#106949=CARTESIAN_POINT('Ctrl Pts',(97.7688147065403,9.22465734545908,13.3932198876557));
#106950=CARTESIAN_POINT('Ctrl Pts',(97.3394157966844,9.44142262640037,13.3669494633107));
#106951=CARTESIAN_POINT('Ctrl Pts',(96.9100168868285,9.65818790734167,13.3406790389656));
#106952=CARTESIAN_POINT('Ctrl Pts',(96.5976857582377,10.1068580056024,13.3144086146206));
#106953=CARTESIAN_POINT('Ctrl Pts',(96.5434779473944,10.5848038792176,13.2881381902756));
#106954=CARTESIAN_POINT('Ctrl Pts',(96.5372964366206,10.6393057585798,13.2851424797203));
#106955=CARTESIAN_POINT('Ctrl Pts',(96.5344714730721,10.6941883300987,13.282146769165));
#106956=CARTESIAN_POINT('Ctrl Pts',(96.5348664968456,10.7491119138617,13.2791510586097));
#106957=CARTESIAN_POINT('Ctrl Pts',(96.5348456374124,10.749123229052,13.2078409669239));
#106958=CARTESIAN_POINT('Ctrl Pts',(96.5344608500961,10.6950932278937,13.2107880481463));
#106959=CARTESIAN_POINT('Ctrl Pts',(96.5371945805109,10.6411025386132,13.2137351293688));
#106960=CARTESIAN_POINT('Ctrl Pts',(96.5431774380789,10.5874743274537,13.2166822105912));
#106961=CARTESIAN_POINT('Ctrl Pts',(96.5965089193795,10.1094298632253,13.2429526349363));
#106962=CARTESIAN_POINT('Ctrl Pts',(96.9080168792921,9.66018800364869,13.2692230592813));
#106963=CARTESIAN_POINT('Ctrl Pts',(97.337017785826,9.4426357963421,13.2954934836263));
#106964=CARTESIAN_POINT('Ctrl Pts',(97.7660186923598,9.22508358903551,13.3217639079714));
#106965=CARTESIAN_POINT('Ctrl Pts',(98.3125125455149,9.23922103399892,13.3480343323164));
#106966=CARTESIAN_POINT('Ctrl Pts',(98.7296913544854,9.47866329478746,13.3743047566614));
#106967=CARTESIAN_POINT('Ctrl Pts',(99.1468701634559,9.71810555557601,13.4005751810064));
#106968=CARTESIAN_POINT('Ctrl Pts',(99.4347339282419,10.1828526321897,13.4268456053515));
#106969=CARTESIAN_POINT('Ctrl Pts',(99.4632772457784,10.6630151754182,13.4531160296965));
#106970=CARTESIAN_POINT('Ctrl Pts',(99.4918205633151,11.1431777186466,13.4793864540415));
#106971=CARTESIAN_POINT('Ctrl Pts',(99.2610434336023,11.6387557284899,13.5056568783866));
#106972=CARTESIAN_POINT('Ctrl Pts',(98.8751698558169,11.9259355277118,13.5319273027316));
#106973=CARTESIAN_POINT('Ctrl Pts',(98.4892962780315,12.2131153269336,13.5581977270766));
#106974=CARTESIAN_POINT('Ctrl Pts',(97.9483262521734,12.2918969155339,13.5844681514217));
#106975=CARTESIAN_POINT('Ctrl Pts',(97.4965726934334,12.1267014705973,13.6107385757667));
#106976=CARTESIAN_POINT('Ctrl Pts',(97.0448191346934,11.9615060256606,13.6370090001117));
#106977=CARTESIAN_POINT('Ctrl Pts',(96.6822820430715,11.552333547187,13.6632794244567));
#106978=CARTESIAN_POINT('Ctrl Pts',(96.5726916665336,11.0839736846863,13.6895498488018));
#106979=CARTESIAN_POINT('Ctrl Pts',(96.5472571005748,10.9752731747371,13.6956468881758));
#106980=CARTESIAN_POINT('Ctrl Pts',(96.5354474203,10.8633845572015,13.7017439275498));
#106981=CARTESIAN_POINT('Ctrl Pts',(96.5364532332071,10.7512863178753,13.7078409669239));
#106982=CARTESIAN_POINT('Origin',(98.,10.75,11.7549960127668));
#106983=CARTESIAN_POINT('',(96.5389396828847,10.7491495099393,14.2791510586097));
#106984=CARTESIAN_POINT('',(96.5386021580424,10.7493836819919,14.2078409669239));
#106985=CARTESIAN_POINT('',(96.5365,10.75,11.7549960127668));
#106986=CARTESIAN_POINT('Ctrl Pts',(96.5389396828847,10.7491495099393,14.2791510586097));
#106987=CARTESIAN_POINT('Ctrl Pts',(96.5397654834611,11.0277392116347,14.264058527972));
#106988=CARTESIAN_POINT('Ctrl Pts',(96.6161315948558,11.3070074359605,14.2489659973343));
#106989=CARTESIAN_POINT('Ctrl Pts',(96.7649096360069,11.5399149644685,14.2338734666966));
#106990=CARTESIAN_POINT('Ctrl Pts',(97.0238762976017,11.9453194492387,14.2076030423516));
#106991=CARTESIAN_POINT('Ctrl Pts',(97.5022346449331,12.2102615648714,14.1813326180065));
#106992=CARTESIAN_POINT('Ctrl Pts',(97.9833029979984,12.2156857424005,14.1550621936615));
#106993=CARTESIAN_POINT('Ctrl Pts',(98.4643713510638,12.2211099199297,14.1287917693165));
#106994=CARTESIAN_POINT('Ctrl Pts',(98.948149709863,11.9670161593553,14.1025213449715));
#106995=CARTESIAN_POINT('Ctrl Pts',(99.2164694661934,11.56786814773,14.0762509206264));
#106996=CARTESIAN_POINT('Ctrl Pts',(99.4847892225238,11.1687201361046,14.0499804962814));
#106997=CARTESIAN_POINT('Ctrl Pts',(99.5376503763853,10.6245178734282,14.0237100719364));
#106998=CARTESIAN_POINT('Ctrl Pts',(99.3510239773211,10.1811772819105,13.9974396475913));
#106999=CARTESIAN_POINT('Ctrl Pts',(99.1643975782568,9.73783669039288,13.9711692232463));
#107000=CARTESIAN_POINT('Ctrl Pts',(98.7382836262668,9.39535777003392,13.9448987989013));
#107001=CARTESIAN_POINT('Ctrl Pts',(98.2652009675881,9.30834068501235,13.9186283745563));
#107002=CARTESIAN_POINT('Ctrl Pts',(97.7921183089095,9.22132359999078,13.8923579502112));
#107003=CARTESIAN_POINT('Ctrl Pts',(97.2720669435421,9.3897683503066,13.8660875258662));
#107004=CARTESIAN_POINT('Ctrl Pts',(96.9398749827355,9.737636556329,13.8398171015212));
#107005=CARTESIAN_POINT('Ctrl Pts',(96.6841657298197,10.0054128109353,13.8195950872173));
#107006=CARTESIAN_POINT('Ctrl Pts',(96.5397699137549,10.3795039000482,13.7993730729135));
#107007=CARTESIAN_POINT('Ctrl Pts',(96.5364271352644,10.7512852130388,13.7791510586097));
#107008=CARTESIAN_POINT('Ctrl Pts',(96.5364532332071,10.7512863178753,13.7078409669239));
#107009=CARTESIAN_POINT('Ctrl Pts',(96.5397811846501,10.3803848363914,13.7280143518949));
#107010=CARTESIAN_POINT('Ctrl Pts',(96.6834082335339,10.0071884960508,13.7481877368659));
#107011=CARTESIAN_POINT('Ctrl Pts',(96.9380160986013,9.73958572435502,13.7683611218369));
#107012=CARTESIAN_POINT('Ctrl Pts',(97.2695745686609,9.39110487305198,13.7946315461819));
#107013=CARTESIAN_POINT('Ctrl Pts',(97.7893351702339,9.22169041697355,13.8209019705269));
#107014=CARTESIAN_POINT('Ctrl Pts',(98.2625669313284,9.30784856791217,13.8471723948719));
#107015=CARTESIAN_POINT('Ctrl Pts',(98.7357986924228,9.39400671885079,13.873442819217));
#107016=CARTESIAN_POINT('Ctrl Pts',(99.1625016130387,9.73573747680645,13.899713243562));
#107017=CARTESIAN_POINT('Ctrl Pts',(99.3499600818927,10.1787180107837,13.925983667907));
#107018=CARTESIAN_POINT('Ctrl Pts',(99.5374185507468,10.6216985447609,13.9522540922521));
#107019=CARTESIAN_POINT('Ctrl Pts',(99.485632567839,11.1659288547597,13.9785245165971));
#107020=CARTESIAN_POINT('Ctrl Pts',(99.2180052725653,11.5656030593164,14.0047949409421));
#107021=CARTESIAN_POINT('Ctrl Pts',(98.9503779772916,11.9652772638732,14.0310653652871));
#107022=CARTESIAN_POINT('Ctrl Pts',(98.4669093696519,12.2203953629878,14.0573357896322));
#107023=CARTESIAN_POINT('Ctrl Pts',(97.9859125610385,12.2157814107928,14.0836062139772));
#107024=CARTESIAN_POINT('Ctrl Pts',(97.5049157524252,12.2111674585977,14.1098766383222));
#107025=CARTESIAN_POINT('Ctrl Pts',(97.0263907428381,11.946821455093,14.1361470626673));
#107026=CARTESIAN_POINT('Ctrl Pts',(96.7665130736172,11.5420450822417,14.1624174870123));
#107027=CARTESIAN_POINT('Ctrl Pts',(96.6167305915848,11.3087491242799,14.1775586469828));
#107028=CARTESIAN_POINT('Ctrl Pts',(96.5395801623541,11.0288038634533,14.1926998069534));
#107029=CARTESIAN_POINT('Ctrl Pts',(96.5386021580424,10.7493836819919,14.2078409669239));
#107030=CARTESIAN_POINT('Origin',(98.,10.75,8.19412889803065));
#107031=CARTESIAN_POINT('',(96.8221913621849,10.7510342737659,13.9441288980306));
#107032=CARTESIAN_POINT('',(96.8239417093505,10.7495040187672,14.042863127503));
#107033=CARTESIAN_POINT('',(96.82225,10.7499999999999,8.19412889803065));
#107034=CARTESIAN_POINT('',(97.0688835974449,11.4739959996586,14.3914960127668));
#107035=CARTESIAN_POINT('Ctrl Pts',(96.8221913621849,10.7510342737659,13.9441288980306));
#107036=CARTESIAN_POINT('Ctrl Pts',(96.8248814594635,10.4518436749448,13.9643509123345));
#107037=CARTESIAN_POINT('Ctrl Pts',(97.092042366385,9.75970094281903,14.0108433509833));
#107038=CARTESIAN_POINT('Ctrl Pts',(98.2512181987561,9.38424363867761,14.0836062139772));
#107039=CARTESIAN_POINT('Ctrl Pts',(99.2799623879387,10.2110722313379,14.1624174870123));
#107040=CARTESIAN_POINT('Ctrl Pts',(99.1523425233119,11.5249107312363,14.2412287600474));
#107041=CARTESIAN_POINT('Ctrl Pts',(98.0207166727073,12.1192718941808,14.3175882686322));
#107042=CARTESIAN_POINT('Ctrl Pts',(97.2863392653372,11.7499101701945,14.367677352872));
#107043=CARTESIAN_POINT('Ctrl Pts',(97.0688835974449,11.4739959996586,14.3914960127668));
#107044=CARTESIAN_POINT('',(98.3831331782623,11.8636893777956,14.3914960127668));
#107045=CARTESIAN_POINT('Origin',(98.,10.75,14.3914960127668));
#107046=CARTESIAN_POINT('Ctrl Pts',(96.8239417093505,10.7495040187672,14.042863127503));
#107047=CARTESIAN_POINT('Ctrl Pts',(96.8233632025523,10.5842220536541,14.0539923918774));
#107048=CARTESIAN_POINT('Ctrl Pts',(96.9327137988548,10.0295622300994,14.091392080597));
#107049=CARTESIAN_POINT('Ctrl Pts',(97.7773396251973,9.37952591027267,14.1550621936615));
#107050=CARTESIAN_POINT('Ctrl Pts',(99.0247842083376,9.81167589004277,14.2338734666966));
#107051=CARTESIAN_POINT('Ctrl Pts',(99.3448716997135,11.0936334060014,14.3126847397317));
#107052=CARTESIAN_POINT('Ctrl Pts',(98.7507886462592,11.7372079631681,14.3652255884217));
#107053=CARTESIAN_POINT('Ctrl Pts',(98.3831331782623,11.8636893777956,14.3914960127668));
#107054=CARTESIAN_POINT('Origin',(98.,10.75,8.19412889803065));
#107055=CARTESIAN_POINT('',(96.8209354401503,10.7492853136663,13.4441288980306));
#107056=CARTESIAN_POINT('',(96.8222123644753,10.7510351628818,13.542863127503));
#107057=CARTESIAN_POINT('',(96.82225,10.7499999999999,8.19412889803065));
#107058=CARTESIAN_POINT('Ctrl Pts',(96.8209354401503,10.7492853136663,13.4441288980306));
#107059=CARTESIAN_POINT('Ctrl Pts',(96.8206175452072,10.7050856206175,13.4471246085859));
#107060=CARTESIAN_POINT('Ctrl Pts',(96.8428270438524,10.2736059300338,13.4763907434862));
#107061=CARTESIAN_POINT('Ctrl Pts',(97.3741854288762,9.51029866733518,13.5319273027316));
#107062=CARTESIAN_POINT('Ctrl Pts',(98.6934908176036,9.54684924260553,13.6107385757667));
#107063=CARTESIAN_POINT('Ctrl Pts',(99.3864080892004,10.670134243859,13.6895498488018));
#107064=CARTESIAN_POINT('Ctrl Pts',(98.82706002641,11.8655606324956,13.7683611218369));
#107065=CARTESIAN_POINT('Ctrl Pts',(97.5206840659668,12.0533593482333,13.8471723948719));
#107066=CARTESIAN_POINT('Ctrl Pts',(96.8713488287459,11.3178003010048,13.9057616536032));
#107067=CARTESIAN_POINT('Ctrl Pts',(96.8213867533488,10.8405222641786,13.9380804879894));
#107068=CARTESIAN_POINT('Ctrl Pts',(96.8221913621849,10.7510342737659,13.9441288980306));
#107069=CARTESIAN_POINT('Ctrl Pts',(96.8222123644753,10.7510351628818,13.542863127503));
#107070=CARTESIAN_POINT('Ctrl Pts',(96.824890529704,10.4525526074888,13.5630365124739));
#107071=CARTESIAN_POINT('Ctrl Pts',(97.0909910233665,9.7611248355653,13.60948032179));
#107072=CARTESIAN_POINT('Ctrl Pts',(98.2487444791565,9.38375846460147,13.682194555451));
#107073=CARTESIAN_POINT('Ctrl Pts',(99.2789105838822,10.2087808086717,13.7610058284861));
#107074=CARTESIAN_POINT('Ctrl Pts',(99.1538864471491,11.5226870217249,13.8398171015212));
#107075=CARTESIAN_POINT('Ctrl Pts',(97.986673971616,12.1386050426998,13.9186283745563));
#107076=CARTESIAN_POINT('Ctrl Pts',(96.9945380412469,11.5905309339865,13.9863103832169));
#107077=CARTESIAN_POINT('Ctrl Pts',(96.8247287572344,10.9743670995436,14.0277219675324));
#107078=CARTESIAN_POINT('Ctrl Pts',(96.8239417093505,10.7495040187672,14.042863127503));
#107079=CARTESIAN_POINT('Origin',(98.,10.75,8.19412889803065));
#107080=CARTESIAN_POINT('',(96.8240376082166,10.7497435860393,12.9441288980306));
#107081=CARTESIAN_POINT('',(96.8209186535446,10.749294419553,13.042863127503));
#107082=CARTESIAN_POINT('',(96.82225,10.7499999999999,8.19412889803065));
#107083=CARTESIAN_POINT('Ctrl Pts',(96.8240376082166,10.7497435860393,12.9441288980306));
#107084=CARTESIAN_POINT('Ctrl Pts',(96.8236844331119,10.570903593424,12.9561687291824));
#107085=CARTESIAN_POINT('Ctrl Pts',(96.9456229031997,10.0022988352385,12.9944789846792));
#107086=CARTESIAN_POINT('Ctrl Pts',(97.8247504499228,9.37239678178178,13.0590596645211));
#107087=CARTESIAN_POINT('Ctrl Pts',(99.0558897301026,9.8480022865368,13.1378709375562));
#107088=CARTESIAN_POINT('Ctrl Pts',(99.3333052969297,11.1383298048701,13.2166822105913));
#107089=CARTESIAN_POINT('Ctrl Pts',(98.4064237370152,12.0779016595067,13.2954934836263));
#107090=CARTESIAN_POINT('Ctrl Pts',(97.161629113368,11.8279341345178,13.3713090461061));
#107091=CARTESIAN_POINT('Ctrl Pts',(96.8234052761637,11.0926880511199,13.4208541842409));
#107092=CARTESIAN_POINT('Ctrl Pts',(96.8209354401503,10.7492853136663,13.4441288980306));
#107093=CARTESIAN_POINT('Ctrl Pts',(96.8209186535446,10.749294419553,13.042863127503));
#107094=CARTESIAN_POINT('Ctrl Pts',(96.8206089963791,10.7058138361133,13.0458102087254));
#107095=CARTESIAN_POINT('Ctrl Pts',(96.8424195706642,10.2750588747293,13.0750277142929));
#107096=CARTESIAN_POINT('Ctrl Pts',(97.3719134809519,9.51144811833339,13.1305156442054));
#107097=CARTESIAN_POINT('Ctrl Pts',(98.6912844455304,9.54557939774368,13.2093269172405));
#107098=CARTESIAN_POINT('Ctrl Pts',(99.3862585807745,10.6675934793599,13.2881381902756));
#107099=CARTESIAN_POINT('Ctrl Pts',(98.8291056640969,11.8640410388261,13.3669494633107));
#107100=CARTESIAN_POINT('Ctrl Pts',(97.5230705811704,12.0542392266786,13.4457607363457));
#107101=CARTESIAN_POINT('Ctrl Pts',(96.87185607722,11.3192549760816,13.5043986244099));
#107102=CARTESIAN_POINT('Ctrl Pts',(96.8214029376552,10.8412460965111,13.5367660881289));
#107103=CARTESIAN_POINT('Ctrl Pts',(96.8222123644753,10.7510351628818,13.542863127503));
#107104=CARTESIAN_POINT('Origin',(98.,10.75,8.19412889803065));
#107105=CARTESIAN_POINT('',(96.8218137388258,10.7509979852509,12.4441288980306));
#107106=CARTESIAN_POINT('',(96.8240326431611,10.7497324482223,12.542863127503));
#107107=CARTESIAN_POINT('',(96.82225,10.7499999999999,8.19412889803065));
#107108=CARTESIAN_POINT('Ctrl Pts',(96.8218137388257,10.7509979852509,12.4441288980306));
#107109=CARTESIAN_POINT('Ctrl Pts',(96.8246086178889,10.4393146543342,12.4652128497789));
#107110=CARTESIAN_POINT('Ctrl Pts',(97.1108125884919,9.7347364811699,12.5125672258722));
#107111=CARTESIAN_POINT('Ctrl Pts',(98.2954919596144,9.39309634609896,12.5861920263106));
#107112=CARTESIAN_POINT('Ctrl Pts',(99.2967249538166,10.2530015917544,12.6650032993457));
#107113=CARTESIAN_POINT('Ctrl Pts',(99.1267017686563,11.561816573295,12.7438145723807));
#107114=CARTESIAN_POINT('Ctrl Pts',(97.9389944505958,12.1373648936305,12.8226258454158));
#107115=CARTESIAN_POINT('Ctrl Pts',(96.9794154936065,11.5632993510555,12.8893972872991));
#107116=CARTESIAN_POINT('Ctrl Pts',(96.8244550468982,10.9611252200095,12.9298983048374));
#107117=CARTESIAN_POINT('Ctrl Pts',(96.8240376082166,10.7497435860393,12.9441288980306));
#107118=CARTESIAN_POINT('Ctrl Pts',(96.8240326431611,10.7497324482223,12.542863127503));
#107119=CARTESIAN_POINT('Ctrl Pts',(96.823665528048,10.5716166193381,12.5548543293219));
#107120=CARTESIAN_POINT('Ctrl Pts',(96.9449149417848,10.0037574602552,12.5931159554859));
#107121=CARTESIAN_POINT('Ctrl Pts',(97.8222251896378,9.37272024999355,12.6576480059949));
#107122=CARTESIAN_POINT('Ctrl Pts',(99.0542344468179,9.84606796723849,12.73645927903));
#107123=CARTESIAN_POINT('Ctrl Pts',(99.3340150885336,11.1358848763664,12.8152705520651));
#107124=CARTESIAN_POINT('Ctrl Pts',(98.4088575369805,12.0771544423753,12.8940818251001));
#107125=CARTESIAN_POINT('Ctrl Pts',(97.1628078249773,11.8293105708282,12.9699460169128));
#107126=CARTESIAN_POINT('Ctrl Pts',(96.8233692953073,11.0934018567722,13.0195397843804));
#107127=CARTESIAN_POINT('Ctrl Pts',(96.8209186535446,10.749294419553,13.042863127503));
#107128=CARTESIAN_POINT('Origin',(98.,10.75,8.19412889803065));
#107129=CARTESIAN_POINT('',(96.821256416619,10.7491427536305,11.9441288980306));
#107130=CARTESIAN_POINT('',(96.8218348096404,10.751001207122,12.042863127503));
#107131=CARTESIAN_POINT('',(96.82225,10.7499999999999,8.19412889803065));
#107132=CARTESIAN_POINT('Ctrl Pts',(96.821256416619,10.7491427536305,11.9441288980306));
#107133=CARTESIAN_POINT('Ctrl Pts',(96.820788807215,10.6921851792609,11.9479865460304));
#107134=CARTESIAN_POINT('Ctrl Pts',(96.850287974486,10.2478350064117,11.9781146183752));
#107135=CARTESIAN_POINT('Ctrl Pts',(97.4147916508613,9.49062149767907,12.034513115065));
#107136=CARTESIAN_POINT('Ctrl Pts',(98.7322138678675,9.57001445953124,12.1133243881001));
#107137=CARTESIAN_POINT('Ctrl Pts',(99.3882699138082,10.7152196834265,12.1921356611351));
#107138=CARTESIAN_POINT('Ctrl Pts',(98.7903825456925,11.8918399430189,12.2709469341702));
#107139=CARTESIAN_POINT('Ctrl Pts',(97.478588625315,12.0371026386346,12.3497582072053));
#107140=CARTESIAN_POINT('Ctrl Pts',(96.8626988373633,11.2919537648761,12.4074855284921));
#107141=CARTESIAN_POINT('Ctrl Pts',(96.8211262223751,10.8276694306214,12.4389424254339));
#107142=CARTESIAN_POINT('Ctrl Pts',(96.8218137388257,10.7509979852509,12.4441288980306));
#107143=CARTESIAN_POINT('Ctrl Pts',(96.8218348096404,10.751001207122,12.042863127503));
#107144=CARTESIAN_POINT('Ctrl Pts',(96.8246265753037,10.440022309364,12.0638984499184));
#107145=CARTESIAN_POINT('Ctrl Pts',(97.1097348020618,9.73614113337312,12.1112041966789));
#107146=CARTESIAN_POINT('Ctrl Pts',(98.2930039044064,9.39255677692249,12.1847803677844));
#107147=CARTESIAN_POINT('Ctrl Pts',(99.2958117603423,10.2506251171967,12.2635916408195));
#107148=CARTESIAN_POINT('Ctrl Pts',(99.1281882710963,11.5597497248036,12.3424029138546));
#107149=CARTESIAN_POINT('Ctrl Pts',(97.941537978492,12.1374745345601,12.4212141868896));
#107150=CARTESIAN_POINT('Ctrl Pts',(96.9802084953429,11.5647522740104,12.4880342581058));
#107151=CARTESIAN_POINT('Ctrl Pts',(96.824469806881,10.9618342537341,12.5285839049769));
#107152=CARTESIAN_POINT('Ctrl Pts',(96.8240326431611,10.7497324482223,12.542863127503));
#107153=CARTESIAN_POINT('Origin',(98.,10.75,8.19412889803065));
#107154=CARTESIAN_POINT('',(96.824088859708,10.7499448247057,11.4441288980306));
#107155=CARTESIAN_POINT('',(96.8212371046644,10.7491497734663,11.542863127503));
#107156=CARTESIAN_POINT('',(96.82225,10.7499999999999,8.19412889803065));
#107157=CARTESIAN_POINT('Ctrl Pts',(96.824088859708,10.7499448247057,11.4441288980306));
#107158=CARTESIAN_POINT('Ctrl Pts',(96.824007628141,10.5582806949243,11.4570306666269));
#107159=CARTESIAN_POINT('Ctrl Pts',(96.9584708630627,9.97645980746022,11.4962028595682));
#107160=CARTESIAN_POINT('Ctrl Pts',(97.8695993014189,9.36743040615582,11.5616454768545));
#107161=CARTESIAN_POINT('Ctrl Pts',(99.0846369462246,9.88278277294862,11.6404567498895));
#107162=CARTESIAN_POINT('Ctrl Pts',(99.3199851647595,11.1814419877856,11.7192680229246));
#107163=CARTESIAN_POINT('Ctrl Pts',(98.3630676087894,12.0904047655311,11.7980792959597));
#107164=CARTESIAN_POINT('Ctrl Pts',(97.1411032137602,11.8034278121455,11.8730329209951));
#107165=CARTESIAN_POINT('Ctrl Pts',(96.8239732080398,11.0800639199987,11.9217161216854));
#107166=CARTESIAN_POINT('Ctrl Pts',(96.821256416619,10.7491427536305,11.9441288980306));
#107167=CARTESIAN_POINT('Ctrl Pts',(96.8212371046644,10.7491497734663,11.542863127503));
#107168=CARTESIAN_POINT('Ctrl Pts',(96.8207779930583,10.6929125877714,11.5466721461699));
#107169=CARTESIAN_POINT('Ctrl Pts',(96.8498547297939,10.2492897535191,11.5767515891818));
#107170=CARTESIAN_POINT('Ctrl Pts',(97.412483782776,9.49169634572781,11.6331014565388));
#107171=CARTESIAN_POINT('Ctrl Pts',(98.7300494612188,9.56867397555541,11.7119127295739));
#107172=CARTESIAN_POINT('Ctrl Pts',(99.388203951153,10.7126746485813,11.790724002609));
#107173=CARTESIAN_POINT('Ctrl Pts',(98.7924746072532,11.89038913916,11.869535275644));
#107174=CARTESIAN_POINT('Ctrl Pts',(97.4809490736544,12.0380564924405,11.9483465486791));
#107175=CARTESIAN_POINT('Ctrl Pts',(96.8631742202878,11.2934111401974,12.0061224992988));
#107176=CARTESIAN_POINT('Ctrl Pts',(96.8211400174464,10.8283951350857,12.0376280255734));
#107177=CARTESIAN_POINT('Ctrl Pts',(96.8218348096404,10.751001207122,12.042863127503));
#107178=CARTESIAN_POINT('Origin',(98.,10.75,8.19412889803065));
#107179=CARTESIAN_POINT('',(96.821445951145,10.7509180827198,10.9441288980306));
#107180=CARTESIAN_POINT('',(96.8240876217551,10.7499333449883,11.042863127503));
#107181=CARTESIAN_POINT('',(96.82225,10.7499999999999,8.19412889803065));
#107182=CARTESIAN_POINT('Ctrl Pts',(96.821445951145,10.7509180827198,10.9441288980306));
#107183=CARTESIAN_POINT('Ctrl Pts',(96.8242284462551,10.4267547825223,10.9660747872234));
#107184=CARTESIAN_POINT('Ctrl Pts',(97.1302745778463,9.70993094798344,11.0142911007611));
#107185=CARTESIAN_POINT('Ctrl Pts',(98.3394198147195,9.4034127530893,11.0887778386439));
#107186=CARTESIAN_POINT('Ctrl Pts',(99.3121871841641,10.2953926774361,11.167589111679));
#107187=CARTESIAN_POINT('Ctrl Pts',(99.0997322410784,11.5979929374135,11.2464003847141));
#107188=CARTESIAN_POINT('Ctrl Pts',(97.8939531704686,12.1346505313534,11.3252116577492));
#107189=CARTESIAN_POINT('Ctrl Pts',(96.9656710215615,11.5375217036545,11.391121162188));
#107190=CARTESIAN_POINT('Ctrl Pts',(96.8241730308702,10.9485448655703,11.4307602422819));
#107191=CARTESIAN_POINT('Ctrl Pts',(96.824088859708,10.7499448247057,11.4441288980306));
#107192=CARTESIAN_POINT('Ctrl Pts',(96.8240876217551,10.7499333449883,11.042863127503));
#107193=CARTESIAN_POINT('Ctrl Pts',(96.8239898537243,10.5589920743739,11.0557162667664));
#107194=CARTESIAN_POINT('Ctrl Pts',(96.9577306106451,9.97791664978809,11.0948398303748));
#107195=CARTESIAN_POINT('Ctrl Pts',(97.8670648684311,9.36767165887723,11.1602338183283));
#107196=CARTESIAN_POINT('Ctrl Pts',(99.0830453734138,9.88079570239144,11.2390450913633));
#107197=CARTESIAN_POINT('Ctrl Pts',(99.3207740272075,11.1790213991231,11.3178563643984));
#107198=CARTESIAN_POINT('Ctrl Pts',(98.3655243729628,12.0897370356262,11.3966676374335));
#107199=CARTESIAN_POINT('Ctrl Pts',(97.1422426640937,11.8048160075092,11.4716698918017));
#107200=CARTESIAN_POINT('Ctrl Pts',(96.8239444403164,11.0807748854833,11.5204017218248));
#107201=CARTESIAN_POINT('Ctrl Pts',(96.8212371046644,10.7491497734663,11.542863127503));
#107202=CARTESIAN_POINT('Origin',(98.,10.75,8.19412889803065));
#107203=CARTESIAN_POINT('',(96.8216123189423,10.7490399772936,10.4441288980306));
#107204=CARTESIAN_POINT('',(96.8214660588487,10.7509237230245,10.542863127503));
#107205=CARTESIAN_POINT('',(96.82225,10.7499999999999,8.19412889803065));
#107206=CARTESIAN_POINT('Ctrl Pts',(96.8216123189423,10.7490399772936,10.4441288980306));
#107207=CARTESIAN_POINT('Ctrl Pts',(96.8209981027453,10.679301326976,10.4488484834748));
#107208=CARTESIAN_POINT('Ctrl Pts',(96.858210790406,10.2220336847976,10.4798384932641));
#107209=CARTESIAN_POINT('Ctrl Pts',(97.45601597308,9.47227374775156,10.5370989273983));
#107210=CARTESIAN_POINT('Ctrl Pts',(98.7701633646951,9.59442593343006,10.6159102004334));
#107211=CARTESIAN_POINT('Ctrl Pts',(99.3886670196609,10.7603409336293,10.6947214734685));
#107212=CARTESIAN_POINT('Ctrl Pts',(98.7528685749049,11.9169155624013,10.7735327465036));
#107213=CARTESIAN_POINT('Ctrl Pts',(97.4370477658578,12.0194832835491,10.8523440195387));
#107214=CARTESIAN_POINT('Ctrl Pts',(96.8545215587298,11.266137244336,10.909209403381));
#107215=CARTESIAN_POINT('Ctrl Pts',(96.8208976480979,10.8147959039589,10.9398043628784));
#107216=CARTESIAN_POINT('Ctrl Pts',(96.821445951145,10.7509180827198,10.9441288980306));
#107217=CARTESIAN_POINT('Ctrl Pts',(96.8214660588487,10.7509237230245,10.542863127503));
#107218=CARTESIAN_POINT('Ctrl Pts',(96.824252879472,10.4274642836231,10.5647603873629));
#107219=CARTESIAN_POINT('Ctrl Pts',(97.1291582504351,9.71132548914857,10.6129280715678));
#107220=CARTESIAN_POINT('Ctrl Pts',(98.3369506025399,9.40279263495737,10.6873661801177));
#107221=CARTESIAN_POINT('Ctrl Pts',(99.311351681027,10.2929877893503,10.7661774531528));
#107222=CARTESIAN_POINT('Ctrl Pts',(99.1012851078598,11.595975474055,10.8449887261879));
#107223=CARTESIAN_POINT('Ctrl Pts',(97.8964917932208,12.1348427503298,10.923799999223));
#107224=CARTESIAN_POINT('Ctrl Pts',(96.9664306987752,11.5389773547356,10.9897581329947));
#107225=CARTESIAN_POINT('Ctrl Pts',(96.8241896809885,10.9492553478996,11.0294458424213));
#107226=CARTESIAN_POINT('Ctrl Pts',(96.8240876217551,10.7499333449883,11.042863127503));
#107227=CARTESIAN_POINT('Origin',(98.,10.75,8.19412889803065));
#107228=CARTESIAN_POINT('',(96.8240738005051,10.7501486858619,9.94412889803064));
#107229=CARTESIAN_POINT('',(96.8215914858097,10.7490446521211,10.042863127503));
#107230=CARTESIAN_POINT('',(96.82225,10.7499999999999,8.19412889803065));
#107231=CARTESIAN_POINT('Ctrl Pts',(96.8240738005051,10.7501486858619,9.94412889803064));
#107232=CARTESIAN_POINT('Ctrl Pts',(96.8243065104756,10.5456862831697,9.95789260407134));
#107233=CARTESIAN_POINT('Ctrl Pts',(96.9718968717623,9.95065676196432,9.99792673445707));
#107234=CARTESIAN_POINT('Ctrl Pts',(97.9145860709853,9.36392434555335,10.0642312891878));
#107235=CARTESIAN_POINT('Ctrl Pts',(99.1122388935191,9.91847855386342,10.1430425622229));
#107236=CARTESIAN_POINT('Ctrl Pts',(99.3052714847173,11.2240987990573,10.221853835258));
#107237=CARTESIAN_POINT('Ctrl Pts',(98.319328101206,12.101492644125,10.3006651082931));
#107238=CARTESIAN_POINT('Ctrl Pts',(97.1212697594882,11.778722341383,10.374756795884));
#107239=CARTESIAN_POINT('Ctrl Pts',(96.8244169877987,11.0674845601755,10.4225780591298));
#107240=CARTESIAN_POINT('Ctrl Pts',(96.8216123189423,10.7490399772936,10.4441288980306));
#107241=CARTESIAN_POINT('Ctrl Pts',(96.8215914858097,10.7490446521211,10.042863127503));
#107242=CARTESIAN_POINT('Ctrl Pts',(96.8209852129159,10.6800276963346,10.0475340836143));
#107243=CARTESIAN_POINT('Ctrl Pts',(96.857751171539,10.2234899964845,10.0784754640707));
#107244=CARTESIAN_POINT('Ctrl Pts',(97.4536744407203,9.47327310866837,10.1356872688721));
#107245=CARTESIAN_POINT('Ctrl Pts',(98.7680436324125,9.59301580922626,10.2144985419072));
#107246=CARTESIAN_POINT('Ctrl Pts',(99.388683785519,10.7577951137743,10.2933098149423));
#107247=CARTESIAN_POINT('Ctrl Pts',(98.7550066620784,11.9155334853073,10.3721210879774));
#107248=CARTESIAN_POINT('Ctrl Pts',(97.4393759810305,12.0205133249269,10.4509323610125));
#107249=CARTESIAN_POINT('Ctrl Pts',(96.8549702624813,11.2675930892139,10.5078463741877));
#107250=CARTESIAN_POINT('Ctrl Pts',(96.8209094949199,10.8155227341254,10.5384899630178));
#107251=CARTESIAN_POINT('Ctrl Pts',(96.8214660588487,10.7509237230245,10.542863127503));
#107252=CARTESIAN_POINT('Origin',(98.,10.75,8.19412889803065));
#107253=CARTESIAN_POINT('',(96.8211250403637,10.7508514088176,9.44412889803064));
#107254=CARTESIAN_POINT('',(96.8240786690275,10.7501410021477,9.54286312750296));
#107255=CARTESIAN_POINT('',(96.82225,10.7499999999999,8.19412889803065));
#107256=CARTESIAN_POINT('Ctrl Pts',(96.8211250403636,10.7508514088176,9.44412889803065));
#107257=CARTESIAN_POINT('Ctrl Pts',(96.8237544514565,10.4142228729031,9.46693672466784));
#107258=CARTESIAN_POINT('Ctrl Pts',(97.1503930402075,9.68523305769091,9.51601497565005));
#107259=CARTESIAN_POINT('Ctrl Pts',(98.383005853651,9.41519382008176,9.59136365097731));
#107260=CARTESIAN_POINT('Ctrl Pts',(99.3262558620476,10.3382425252825,9.6701749240124));
#107261=CARTESIAN_POINT('Ctrl Pts',(99.0716056636518,11.6332844720055,9.74898619704748));
#107262=CARTESIAN_POINT('Ctrl Pts',(97.8490218626003,12.130469107685,9.82779747008258));
#107263=CARTESIAN_POINT('Ctrl Pts',(96.9525116359327,11.5117026075794,9.89284503707695));
#107264=CARTESIAN_POINT('Ctrl Pts',(96.8238623430648,10.9359383028979,9.93162217972631));
#107265=CARTESIAN_POINT('Ctrl Pts',(96.8240738005051,10.7501486858619,9.94412889803064));
#107266=CARTESIAN_POINT('Ctrl Pts',(96.8240786690275,10.7501410021477,9.54286312750296));
#107267=CARTESIAN_POINT('Ctrl Pts',(96.8242915248503,10.5463980025343,9.55657820421082));
#107268=CARTESIAN_POINT('Ctrl Pts',(96.9711196599306,9.95210488068972,9.59656370526371));
#107269=CARTESIAN_POINT('Ctrl Pts',(97.9120477433836,9.36408725039594,9.66281963066163));
#107270=CARTESIAN_POINT('Ctrl Pts',(99.1107114318979,9.91643879095944,9.74163090369672));
#107271=CARTESIAN_POINT('Ctrl Pts',(99.3061392069621,11.2217061208911,9.8204421767318));
#107272=CARTESIAN_POINT('Ctrl Pts',(98.321804948717,12.10090458802,9.89925344976689));
#107273=CARTESIAN_POINT('Ctrl Pts',(97.1223704965245,11.7801214664973,9.97339376669061));
#107274=CARTESIAN_POINT('Ctrl Pts',(96.8243950172063,11.0681933464253,10.0212636592693));
#107275=CARTESIAN_POINT('Ctrl Pts',(96.8215914858097,10.7490446521211,10.042863127503));
#107276=CARTESIAN_POINT('Origin',(98.,10.75,14.3914960127668));
#107277=CARTESIAN_POINT('',(97.7682422725578,9.30496691879707,14.3914960127668));
#107278=CARTESIAN_POINT('Ctrl Pts',(97.0688835974449,11.4739959996586,14.3914960127668));
#107279=CARTESIAN_POINT('Ctrl Pts',(97.0429761988506,11.4480386702715,14.3914960127668));
#107280=CARTESIAN_POINT('Ctrl Pts',(97.0184141797121,11.420872235244,14.3914960127668));
#107281=CARTESIAN_POINT('Ctrl Pts',(96.995310961042,11.3925593864603,14.3914960127668));
#107282=CARTESIAN_POINT('Ctrl Pts',(96.9647247406936,11.35507616631,14.3914960127668));
#107283=CARTESIAN_POINT('Ctrl Pts',(96.9366933909,11.3155851478366,14.3914960127668));
#107284=CARTESIAN_POINT('Ctrl Pts',(96.9112006310938,11.2743888078016,14.3914960127668));
#107285=CARTESIAN_POINT('Ctrl Pts',(96.9032600996146,11.2615568964134,14.3914960127668));
#107286=CARTESIAN_POINT('Ctrl Pts',(96.8955661051928,11.2485592386644,14.3914960127668));
#107287=CARTESIAN_POINT('Ctrl Pts',(96.8881188327785,11.2354042386312,14.3914960127668));
#107288=CARTESIAN_POINT('Ctrl Pts',(96.8811800017753,11.2231473589306,14.3914960127668));
#107289=CARTESIAN_POINT('Ctrl Pts',(96.8744542741059,11.2107513797533,14.3914960127668));
#107290=CARTESIAN_POINT('Ctrl Pts',(96.8679528845086,11.1982449409067,14.3914960127668));
#107291=CARTESIAN_POINT('Ctrl Pts',(96.8446356339814,11.1533905657889,14.3914960127668));
#107292=CARTESIAN_POINT('Ctrl Pts',(96.8241681434784,11.1070628521453,14.3914960127668));
#107293=CARTESIAN_POINT('Ctrl Pts',(96.8065305355175,11.0595945690794,14.3914960127668));
#107294=CARTESIAN_POINT('Ctrl Pts',(96.7939104221224,11.0256299228364,14.3914960127668));
#107295=CARTESIAN_POINT('Ctrl Pts',(96.7827398306571,10.991080304713,14.3914960127668));
#107296=CARTESIAN_POINT('Ctrl Pts',(96.7730236186375,10.9560568345071,14.3914960127668));
#107297=CARTESIAN_POINT('Ctrl Pts',(96.7696110617776,10.9437557872194,14.3914960127668));
#107298=CARTESIAN_POINT('Ctrl Pts',(96.766378010274,10.931396221671,14.3914960127668));
#107299=CARTESIAN_POINT('Ctrl Pts',(96.7633249962767,10.9189827643307,14.3914960127668));
#107300=CARTESIAN_POINT('Ctrl Pts',(96.7610658690711,10.9097972253134,14.3914960127668));
#107301=CARTESIAN_POINT('Ctrl Pts',(96.7589059318967,10.900584374175,14.3914960127668));
#107302=CARTESIAN_POINT('Ctrl Pts',(96.7568470780902,10.8913548727577,14.3914960127668));
#107303=CARTESIAN_POINT('Ctrl Pts',(96.7454259124535,10.8401556743983,14.3914960127668));
#107304=CARTESIAN_POINT('Ctrl Pts',(96.7370933376322,10.7883715386039,14.3914960127668));
#107305=CARTESIAN_POINT('Ctrl Pts',(96.7318320440446,10.736340937265,14.3914960127668));
#107306=CARTESIAN_POINT('Ctrl Pts',(96.7264686405729,10.6833005388905,14.3914960127668));
#107307=CARTESIAN_POINT('Ctrl Pts',(96.7242964061771,10.6300029496301,14.3914960127668));
#107308=CARTESIAN_POINT('Ctrl Pts',(96.7253427957507,10.5767796518361,14.3914960127668));
#107309=CARTESIAN_POINT('Ctrl Pts',(96.7259617653546,10.5452965365773,14.3914960127668));
#107310=CARTESIAN_POINT('Ctrl Pts',(96.7277078521842,10.5138389806834,14.3914960127668));
#107311=CARTESIAN_POINT('Ctrl Pts',(96.7305951134011,10.482473675579,14.3914960127668));
#107312=CARTESIAN_POINT('Ctrl Pts',(96.7320811103492,10.4663307830031,14.3914960127668));
#107313=CARTESIAN_POINT('Ctrl Pts',(96.7338694964227,10.4502123161242,14.3914960127668));
#107314=CARTESIAN_POINT('Ctrl Pts',(96.7359628745836,10.4341273667755,14.3914960127668));
#107315=CARTESIAN_POINT('Ctrl Pts',(96.7374537227486,10.4226720943033,14.3914960127668));
#107316=CARTESIAN_POINT('Ctrl Pts',(96.7390997168083,10.4112319328867,14.3914960127668));
#107317=CARTESIAN_POINT('Ctrl Pts',(96.7408980733302,10.3998319062154,14.3914960127668));
#107318=CARTESIAN_POINT('Ctrl Pts',(96.7494385785201,10.3456924818211,14.3914960127668));
#107319=CARTESIAN_POINT('Ctrl Pts',(96.7614239701143,10.2923517591577,14.3914960127668));
#107320=CARTESIAN_POINT('Ctrl Pts',(96.7768661020469,10.2401573800707,14.3914960127668));
#107321=CARTESIAN_POINT('Ctrl Pts',(96.7802201578377,10.2288206773286,14.3914960127668));
#107322=CARTESIAN_POINT('Ctrl Pts',(96.7837374792372,10.2175380043515,14.3914960127668));
#107323=CARTESIAN_POINT('Ctrl Pts',(96.7874185073135,10.2063128612481,14.3914960127668));
#107324=CARTESIAN_POINT('Ctrl Pts',(96.8037952935392,10.1563725279636,14.3914960127668));
#107325=CARTESIAN_POINT('Ctrl Pts',(96.8234081998674,10.1075702746358,14.3914960127668));
#107326=CARTESIAN_POINT('Ctrl Pts',(96.8460023865325,10.0600579930232,14.3914960127668));
#107327=CARTESIAN_POINT('Ctrl Pts',(96.8569215707814,10.0370965399424,14.3914960127668));
#107328=CARTESIAN_POINT('Ctrl Pts',(96.8685378258048,10.0144364777629,14.3914960127668));
#107329=CARTESIAN_POINT('Ctrl Pts',(96.8808264862297,9.99209596216232,14.3914960127668));
#107330=CARTESIAN_POINT('Ctrl Pts',(96.8886074358317,9.97795036614436,14.3914960127668));
#107331=CARTESIAN_POINT('Ctrl Pts',(96.8966580166366,9.96393289812474,14.3914960127668));
#107332=CARTESIAN_POINT('Ctrl Pts',(96.9049724672611,9.95004837447309,14.3914960127668));
#107333=CARTESIAN_POINT('Ctrl Pts',(96.910186650653,9.94134107005839,14.3914960127668));
#107334=CARTESIAN_POINT('Ctrl Pts',(96.9155049177142,9.93268578036605,14.3914960127668));
#107335=CARTESIAN_POINT('Ctrl Pts',(96.9209173591067,9.92409670769064,14.3914960127668));
#107336=CARTESIAN_POINT('Ctrl Pts',(96.9501434809259,9.87771740006923,14.3914960127668));
#107337=CARTESIAN_POINT('Ctrl Pts',(96.9821663853327,9.83317419115088,14.3914960127668));
#107338=CARTESIAN_POINT('Ctrl Pts',(97.0166886585068,9.79062429455657,14.3914960127668));
#107339=CARTESIAN_POINT('Ctrl Pts',(97.0519654053717,9.74714448302404,14.3914960127668));
#107340=CARTESIAN_POINT('Ctrl Pts',(97.0898524425345,9.70574520992445,14.3914960127668));
#107341=CARTESIAN_POINT('Ctrl Pts',(97.130085198549,9.66660954170395,14.3914960127668));
#107342=CARTESIAN_POINT('Ctrl Pts',(97.1526979511723,9.64461340542393,14.3914960127668));
#107343=CARTESIAN_POINT('Ctrl Pts',(97.1760526165578,9.62333268371835,14.3914960127668));
#107344=CARTESIAN_POINT('Ctrl Pts',(97.2001083672487,9.60280352273155,14.3914960127668));
#107345=CARTESIAN_POINT('Ctrl Pts',(97.2158596822888,9.58936136138041,14.3914960127668));
#107346=CARTESIAN_POINT('Ctrl Pts',(97.2319116681868,9.57624148376674,14.3914960127668));
#107347=CARTESIAN_POINT('Ctrl Pts',(97.2482537342435,9.56345483580649,14.3914960127668));
#107348=CARTESIAN_POINT('Ctrl Pts',(97.2564933326357,9.5570078637034,14.3914960127668));
#107349=CARTESIAN_POINT('Ctrl Pts',(97.2648087003651,9.55064411016295,14.3914960127668));
#107350=CARTESIAN_POINT('Ctrl Pts',(97.2731919630714,9.54436995193093,14.3914960127668));
#107351=CARTESIAN_POINT('Ctrl Pts',(97.3197937996518,9.50949244577978,14.3914960127668));
#107352=CARTESIAN_POINT('Ctrl Pts',(97.3683447994762,9.47748800785936,14.3914960127668));
#107353=CARTESIAN_POINT('Ctrl Pts',(97.4185523047113,9.44853887199522,14.3914960127668));
#107354=CARTESIAN_POINT('Ctrl Pts',(97.4688918883076,9.41951358109408,14.3914960127668));
#107355=CARTESIAN_POINT('Ctrl Pts',(97.5208974737716,9.39355880028942,14.3914960127668));
#107356=CARTESIAN_POINT('Ctrl Pts',(97.5743161192772,9.37088902478583,14.3914960127668));
#107357=CARTESIAN_POINT('Ctrl Pts',(97.6265065651117,9.34874047198558,14.3914960127668));
#107358=CARTESIAN_POINT('Ctrl Pts',(97.6800466921163,9.32972692287584,14.3914960127668));
#107359=CARTESIAN_POINT('Ctrl Pts',(97.7347284624306,9.31408912061954,14.3914960127668));
#107360=CARTESIAN_POINT('Ctrl Pts',(97.7458529634341,9.3109077542173,14.3914960127668));
#107361=CARTESIAN_POINT('Ctrl Pts',(97.7570247849795,9.30786626056828,14.3914960127668));
#107362=CARTESIAN_POINT('Ctrl Pts',(97.7682422725578,9.30496691879707,14.3914960127668));
#107363=CARTESIAN_POINT('',(96.5365,10.75,14.3914960127668));
#107364=CARTESIAN_POINT('Origin',(98.,10.75,14.3914960127668));
#107365=CARTESIAN_POINT('',(98.9846501585944,9.66583019221064,14.3914960127668));
#107366=CARTESIAN_POINT('Origin',(98.,10.75,14.3914960127668));
#107367=CARTESIAN_POINT('Ctrl Pts',(98.985638815547,9.6652849966315,14.3914960127668));
#107368=CARTESIAN_POINT('Ctrl Pts',(99.016139412943,9.69833171151842,14.3914960127668));
#107369=CARTESIAN_POINT('Ctrl Pts',(99.0449589200137,9.73279368715152,14.3914960127668));
#107370=CARTESIAN_POINT('Ctrl Pts',(99.0719485462807,9.76863256666571,14.3914960127668));
#107371=CARTESIAN_POINT('Ctrl Pts',(99.1063284484702,9.81428481690756,14.3914960127668));
#107372=CARTESIAN_POINT('Ctrl Pts',(99.1377406776653,9.8621714511127,14.3914960127668));
#107373=CARTESIAN_POINT('Ctrl Pts',(99.1661298440887,9.91196072331448,14.3914960127668));
#107374=CARTESIAN_POINT('Ctrl Pts',(99.1769248568896,9.93089315066194,14.3914960127668));
#107375=CARTESIAN_POINT('Ctrl Pts',(99.1872822730401,9.95010081750062,14.3914960127668));
#107376=CARTESIAN_POINT('Ctrl Pts',(99.1971972321457,9.9695657815029,14.3914960127668));
#107377=CARTESIAN_POINT('Ctrl Pts',(99.2030514614112,9.98105875496862,14.3914960127668));
#107378=CARTESIAN_POINT('Ctrl Pts',(99.2087516966422,9.99264230536428,14.3914960127668));
#107379=CARTESIAN_POINT('Ctrl Pts',(99.2142900149449,10.0042976336629,14.3914960127668));
#107380=CARTESIAN_POINT('Ctrl Pts',(99.238975512711,10.0562479848257,14.3914960127668));
#107381=CARTESIAN_POINT('Ctrl Pts',(99.260484301343,10.1096920623883,14.3914960127668));
#107382=CARTESIAN_POINT('Ctrl Pts',(99.2787659465126,10.1642873542009,14.3914960127668));
#107383=CARTESIAN_POINT('Ctrl Pts',(99.2910846217951,10.2010751632604,14.3914960127668));
#107384=CARTESIAN_POINT('Ctrl Pts',(99.3019369735001,10.2383860468379,14.3914960127668));
#107385=CARTESIAN_POINT('Ctrl Pts',(99.3112942427666,10.2761157654541,14.3914960127668));
#107386=CARTESIAN_POINT('Ctrl Pts',(99.3153448835169,10.2924484722911,14.3914960127668));
#107387=CARTESIAN_POINT('Ctrl Pts',(99.3191152218517,10.3088596507996,14.3914960127668));
#107388=CARTESIAN_POINT('Ctrl Pts',(99.3226022941674,10.3253407262825,14.3914960127668));
#107389=CARTESIAN_POINT('Ctrl Pts',(99.3249788512658,10.3365731336955,14.3914960127668));
#107390=CARTESIAN_POINT('Ctrl Pts',(99.327224111217,10.3478400238607,14.3914960127668));
#107391=CARTESIAN_POINT('Ctrl Pts',(99.3293340464886,10.3591211859305,14.3914960127668));
#107392=CARTESIAN_POINT('Ctrl Pts',(99.339673988808,10.4144056141612,14.3914960127668));
#107393=CARTESIAN_POINT('Ctrl Pts',(99.3467877541545,10.4701190818833,14.3914960127668));
#107394=CARTESIAN_POINT('Ctrl Pts',(99.3506248509382,10.5259436282514,14.3914960127668));
#107395=CARTESIAN_POINT('Ctrl Pts',(99.3543694449217,10.5804223845209,14.3914960127668));
#107396=CARTESIAN_POINT('Ctrl Pts',(99.3549932689645,10.6350079682248,14.3914960127668));
#107397=CARTESIAN_POINT('Ctrl Pts',(99.3524014399336,10.6893967205018,14.3914960127668));
#107398=CARTESIAN_POINT('Ctrl Pts',(99.3508330094634,10.7223097619436,14.3914960127668));
#107399=CARTESIAN_POINT('Ctrl Pts',(99.3480860911869,10.7551504957268,14.3914960127668));
#107400=CARTESIAN_POINT('Ctrl Pts',(99.3441311915637,10.7878477780733,14.3914960127668));
#107401=CARTESIAN_POINT('Ctrl Pts',(99.3411589614533,10.8124208030236,14.3914960127668));
#107402=CARTESIAN_POINT('Ctrl Pts',(99.3375043339722,10.8369127499246,14.3914960127668));
#107403=CARTESIAN_POINT('Ctrl Pts',(99.3331524064438,10.8612918325753,14.3914960127668));
#107404=CARTESIAN_POINT('Ctrl Pts',(99.331461276709,10.8707653799422,14.3914960127668));
#107405=CARTESIAN_POINT('Ctrl Pts',(99.3296656034321,10.8802171964784,14.3914960127668));
#107406=CARTESIAN_POINT('Ctrl Pts',(99.3277664602594,10.8896377701555,14.3914960127668));
#107407=CARTESIAN_POINT('Ctrl Pts',(99.3173475530846,10.9413200677745,14.3914960127668));
#107408=CARTESIAN_POINT('Ctrl Pts',(99.3038056233175,10.9921354570883,14.3914960127668));
#107409=CARTESIAN_POINT('Ctrl Pts',(99.2870604116319,11.0418039394557,14.3914960127668));
#107410=CARTESIAN_POINT('Ctrl Pts',(99.2833577555898,11.0527865003091,14.3914960127668));
#107411=CARTESIAN_POINT('Ctrl Pts',(99.2794982983791,11.0637129030486,14.3914960127668));
#107412=CARTESIAN_POINT('Ctrl Pts',(99.2754808601922,11.074579962025,14.3914960127668));
#107413=CARTESIAN_POINT('Ctrl Pts',(99.2565155778308,11.1258805253043,14.3914960127668));
#107414=CARTESIAN_POINT('Ctrl Pts',(99.2340328831329,11.1758617007157,14.3914960127668));
#107415=CARTESIAN_POINT('Ctrl Pts',(99.2082809266655,11.2242819327261,14.3914960127668));
#107416=CARTESIAN_POINT('Ctrl Pts',(99.1972654713244,11.2449937921917,14.3914960127668));
#107417=CARTESIAN_POINT('Ctrl Pts',(99.1856513303607,11.2654195472256,14.3914960127668));
#107418=CARTESIAN_POINT('Ctrl Pts',(99.1734560041558,11.285537825985,14.3914960127668));
#107419=CARTESIAN_POINT('Ctrl Pts',(99.1644844946234,11.3003378671345,14.3914960127668));
#107420=CARTESIAN_POINT('Ctrl Pts',(99.1551984345818,11.3149714760779,14.3914960127668));
#107421=CARTESIAN_POINT('Ctrl Pts',(99.1456045021247,11.3294295540173,14.3914960127668));
#107422=CARTESIAN_POINT('Ctrl Pts',(99.140099525536,11.337725566203,14.3914960127668));
#107423=CARTESIAN_POINT('Ctrl Pts',(99.1344983585284,11.3459559325157,14.3914960127668));
#107424=CARTESIAN_POINT('Ctrl Pts',(99.1288044719674,11.3541169102581,14.3914960127668));
#107425=CARTESIAN_POINT('Ctrl Pts',(99.0987571404528,11.3971833818293,14.3914960127668));
#107426=CARTESIAN_POINT('Ctrl Pts',(99.066115553153,11.4383434819937,14.3914960127668));
#107427=CARTESIAN_POINT('Ctrl Pts',(99.0311189048726,11.4773986149495,14.3914960127668));
#107428=CARTESIAN_POINT('Ctrl Pts',(98.996294801149,11.5162611937342,14.3914960127668));
#107429=CARTESIAN_POINT('Ctrl Pts',(98.9591377847492,11.5530401413719,14.3914960127668));
#107430=CARTESIAN_POINT('Ctrl Pts',(98.9198553772279,11.5874972110253,14.3914960127668));
#107431=CARTESIAN_POINT('Ctrl Pts',(98.9002209306982,11.6047198186599,14.3914960127668));
#107432=CARTESIAN_POINT('Ctrl Pts',(98.8800551562504,11.6213616305313,14.3914960127668));
#107433=CARTESIAN_POINT('Ctrl Pts',(98.859382499797,11.6373881384408,14.3914960127668));
#107434=CARTESIAN_POINT('Ctrl Pts',(98.8441369891611,11.6492072434185,14.3914960127668));
#107435=CARTESIAN_POINT('Ctrl Pts',(98.8286157834736,11.6606916398438,14.3914960127668));
#107436=CARTESIAN_POINT('Ctrl Pts',(98.8128285365262,11.6718262543508,14.3914960127668));
#107437=CARTESIAN_POINT('Ctrl Pts',(98.8051889947957,11.6772143598555,14.3914960127668));
#107438=CARTESIAN_POINT('Ctrl Pts',(98.7974879290995,11.6825198806233,14.3914960127668));
#107439=CARTESIAN_POINT('Ctrl Pts',(98.7897372384311,11.6877341666513,14.3914960127668));
#107440=CARTESIAN_POINT('Ctrl Pts',(98.7478945384241,11.715883891025,14.3914960127668));
#107441=CARTESIAN_POINT('Ctrl Pts',(98.7045253466422,11.7414367511671,14.3914960127668));
#107442=CARTESIAN_POINT('Ctrl Pts',(98.6598266413956,11.7641882725167,14.3914960127668));
#107443=CARTESIAN_POINT('Ctrl Pts',(98.6160321815113,11.7864795353968,14.3914960127668));
#107444=CARTESIAN_POINT('Ctrl Pts',(98.57096057418,11.8060819970254,14.3914960127668));
#107445=CARTESIAN_POINT('Ctrl Pts',(98.5247867566208,11.8227547930337,14.3914960127668));
#107446=CARTESIAN_POINT('Ctrl Pts',(98.4786129390616,11.8394275890421,14.3914960127668));
#107447=CARTESIAN_POINT('Ctrl Pts',(98.431336115872,11.8531711940639,14.3914960127668));
#107448=CARTESIAN_POINT('Ctrl Pts',(98.3831331782623,11.8636893777956,14.3914960127668));
#107449=CARTESIAN_POINT('Ctrl Pts',(97.4897834946116,11.8114961988294,8.95351817334586));
#107450=CARTESIAN_POINT('Ctrl Pts',(97.1393582418089,11.6430615420855,8.97978859769089));
#107451=CARTESIAN_POINT('Ctrl Pts',(96.6242618069232,10.9346841371649,9.03232944638095));
#107452=CARTESIAN_POINT('Ctrl Pts',(97.0914565134647,9.69872289948882,9.11114071941605));
#107453=CARTESIAN_POINT('Ctrl Pts',(98.3807382620766,9.41477895129228,9.18995199245111));
#107454=CARTESIAN_POINT('Ctrl Pts',(99.3254100117742,10.3356711404167,9.2687632654862));
#107455=CARTESIAN_POINT('Ctrl Pts',(99.0732671457231,11.6313879250538,9.3475745385213));
#107456=CARTESIAN_POINT('Ctrl Pts',(97.8515312358663,12.1307094457997,9.42638581155637));
#107457=CARTESIAN_POINT('Ctrl Pts',(96.7639840600833,11.3830590515328,9.50519708459147));
#107458=CARTESIAN_POINT('Ctrl Pts',(96.7928159215348,10.0635328883854,9.58400835762655));
#107459=CARTESIAN_POINT('Ctrl Pts',(97.9120477433836,9.36408725039594,9.66281963066163));
#107460=CARTESIAN_POINT('Ctrl Pts',(99.1107114318979,9.91643879095944,9.74163090369672));
#107461=CARTESIAN_POINT('Ctrl Pts',(99.3061392069621,11.2217061208911,9.8204421767318));
#107462=CARTESIAN_POINT('Ctrl Pts',(98.321804948717,12.10090458802,9.89925344976689));
#107463=CARTESIAN_POINT('Ctrl Pts',(97.0468042470516,11.7599116273157,9.97806472280198));
#107464=CARTESIAN_POINT('Ctrl Pts',(96.632769181073,10.5067232539037,10.0568759958371));
#107465=CARTESIAN_POINT('Ctrl Pts',(97.4536744407203,9.47327310866837,10.1356872688721));
#107466=CARTESIAN_POINT('Ctrl Pts',(98.7680436324125,9.59301580922626,10.2144985419072));
#107467=CARTESIAN_POINT('Ctrl Pts',(99.388683785519,10.7577951137743,10.2933098149423));
#107468=CARTESIAN_POINT('Ctrl Pts',(98.7550066620784,11.9155334853073,10.3721210879774));
#107469=CARTESIAN_POINT('Ctrl Pts',(97.4393759810305,12.0205133249269,10.4509323610125));
#107470=CARTESIAN_POINT('Ctrl Pts',(96.6301243384503,10.977912408914,10.5297436340476));
#107471=CARTESIAN_POINT('Ctrl Pts',(97.0582016567961,9.7294514859898,10.6085549070827));
#107472=CARTESIAN_POINT('Ctrl Pts',(98.3369506025399,9.40279263495737,10.6873661801177));
#107473=CARTESIAN_POINT('Ctrl Pts',(99.311351681027,10.2929877893503,10.7661774531528));
#107474=CARTESIAN_POINT('Ctrl Pts',(99.1012851078598,11.595975474055,10.8449887261879));
#107475=CARTESIAN_POINT('Ctrl Pts',(97.8964917932208,12.1348427503298,10.923799999223));
#107476=CARTESIAN_POINT('Ctrl Pts',(96.7851914173279,11.4228621696346,11.0026112722581));
#107477=CARTESIAN_POINT('Ctrl Pts',(96.7711569308156,10.1031243526508,11.0814225452932));
#107478=CARTESIAN_POINT('Ctrl Pts',(97.8670648684311,9.36767165887723,11.1602338183283));
#107479=CARTESIAN_POINT('Ctrl Pts',(99.0830453734138,9.88079570239144,11.2390450913633));
#107480=CARTESIAN_POINT('Ctrl Pts',(99.3207740272075,11.1790213991231,11.3178563643984));
#107481=CARTESIAN_POINT('Ctrl Pts',(98.3655243729628,12.0897370356262,11.3966676374335));
#107482=CARTESIAN_POINT('Ctrl Pts',(97.0801178266041,11.7903461822508,11.4754789104686));
#107483=CARTESIAN_POINT('Ctrl Pts',(96.625587309158,10.5512711719255,11.5542901835037));
#107484=CARTESIAN_POINT('Ctrl Pts',(97.412483782776,9.49169634572781,11.6331014565388));
#107485=CARTESIAN_POINT('Ctrl Pts',(98.7300494612188,9.56867397555541,11.7119127295739));
#107486=CARTESIAN_POINT('Ctrl Pts',(99.388203951153,10.7126746485813,11.790724002609));
#107487=CARTESIAN_POINT('Ctrl Pts',(98.7924746072532,11.89038913916,11.869535275644));
#107488=CARTESIAN_POINT('Ctrl Pts',(97.4809490736544,12.0380564924405,11.9483465486791));
#107489=CARTESIAN_POINT('Ctrl Pts',(96.6382520323991,11.0222973826287,12.0271578217142));
#107490=CARTESIAN_POINT('Ctrl Pts',(97.0255426748034,9.76058789514945,12.1059690947493));
#107491=CARTESIAN_POINT('Ctrl Pts',(98.2930039044064,9.39255677692249,12.1847803677844));
#107492=CARTESIAN_POINT('Ctrl Pts',(99.2958117603423,10.2506251171967,12.2635916408195));
#107493=CARTESIAN_POINT('Ctrl Pts',(99.1281882710963,11.5597497248036,12.3424029138546));
#107494=CARTESIAN_POINT('Ctrl Pts',(97.941537978492,12.1374745345601,12.4212141868896));
#107495=CARTESIAN_POINT('Ctrl Pts',(96.807693027503,11.4619743498409,12.5000254599247));
#107496=CARTESIAN_POINT('Ctrl Pts',(96.7507895706755,10.1433891731248,12.5788367329598));
#107497=CARTESIAN_POINT('Ctrl Pts',(97.8222251896378,9.37272024999355,12.6576480059949));
#107498=CARTESIAN_POINT('Ctrl Pts',(99.0542344468179,9.84606796723849,12.73645927903));
#107499=CARTESIAN_POINT('Ctrl Pts',(99.3340150885336,11.1358848763664,12.8152705520651));
#107500=CARTESIAN_POINT('Ctrl Pts',(98.4088575369805,12.0771544423753,12.8940818251001));
#107501=CARTESIAN_POINT('Ctrl Pts',(97.1144027787922,11.8196826290748,12.9728930981352));
#107502=CARTESIAN_POINT('Ctrl Pts',(96.6198564263835,10.5960287813665,13.0517043711703));
#107503=CARTESIAN_POINT('Ctrl Pts',(97.3719134809519,9.51144811833339,13.1305156442054));
#107504=CARTESIAN_POINT('Ctrl Pts',(98.6912844455304,9.54557939774368,13.2093269172405));
#107505=CARTESIAN_POINT('Ctrl Pts',(99.3862585807745,10.6675934793599,13.2881381902756));
#107506=CARTESIAN_POINT('Ctrl Pts',(98.8291056640969,11.8640410388261,13.3669494633107));
#107507=CARTESIAN_POINT('Ctrl Pts',(97.5230705811704,12.0542392266786,13.4457607363457));
#107508=CARTESIAN_POINT('Ctrl Pts',(96.6478166153533,11.0663959334999,13.5245720093808));
#107509=CARTESIAN_POINT('Ctrl Pts',(96.9939141781605,9.79276675085979,13.6033832824159));
#107510=CARTESIAN_POINT('Ctrl Pts',(98.2487444791565,9.38375846460147,13.682194555451));
#107511=CARTESIAN_POINT('Ctrl Pts',(99.2789105838822,10.2087808086717,13.7610058284861));
#107512=CARTESIAN_POINT('Ctrl Pts',(99.1538864471491,11.5226870217249,13.8398171015212));
#107513=CARTESIAN_POINT('Ctrl Pts',(97.986673971616,12.1386050426998,13.9186283745563));
#107514=CARTESIAN_POINT('Ctrl Pts',(96.8313965612137,11.5004085842898,13.9974396475913));
#107515=CARTESIAN_POINT('Ctrl Pts',(96.731856377117,10.1841450230525,14.0762509206264));
#107516=CARTESIAN_POINT('Ctrl Pts',(97.7773396251973,9.37952591027267,14.1550621936615));
#107517=CARTESIAN_POINT('Ctrl Pts',(99.0247842083376,9.81167589004277,14.2338734666966));
#107518=CARTESIAN_POINT('Ctrl Pts',(99.3448716997135,11.0936334060014,14.3126847397317));
#107519=CARTESIAN_POINT('Ctrl Pts',(98.7507886462592,11.7372079631681,14.3652255884217));
#107520=CARTESIAN_POINT('Ctrl Pts',(98.3831331782623,11.8636893777956,14.3914960127668));
#107521=CARTESIAN_POINT('Ctrl Pts',(97.4485199648826,11.8973442250985,9.00851078648618));
#107522=CARTESIAN_POINT('Ctrl Pts',(97.0697542278266,11.7152874914666,9.03478121083121));
#107523=CARTESIAN_POINT('Ctrl Pts',(96.5129996011151,10.9496203834523,9.08732205952127));
#107524=CARTESIAN_POINT('Ctrl Pts',(97.0179784688096,9.6137013381866,9.16613333255634));
#107525=CARTESIAN_POINT('Ctrl Pts',(98.4115302972817,9.30679355125881,9.24494460559144));
#107526=CARTESIAN_POINT('Ctrl Pts',(99.4326019486213,10.30216248079,9.32375587862652));
#107527=CARTESIAN_POINT('Ctrl Pts',(99.1600671420125,11.7026697759231,9.40256715166161));
#107528=CARTESIAN_POINT('Ctrl Pts',(97.8395238915373,12.2423736994294,9.48137842469669));
#107529=CARTESIAN_POINT('Ctrl Pts',(96.6640218284744,11.4342574167704,9.56018969773178));
#107530=CARTESIAN_POINT('Ctrl Pts',(96.695185453716,10.0080151703796,9.63900097076685));
#107531=CARTESIAN_POINT('Ctrl Pts',(97.9049346443025,9.2520021819181,9.71781224380195));
#107532=CARTESIAN_POINT('Ctrl Pts',(99.2005397179419,9.84902490417435,9.79662351683703));
#107533=CARTESIAN_POINT('Ctrl Pts',(99.4117726261623,11.2598551406448,9.87543478987212));
#107534=CARTESIAN_POINT('Ctrl Pts',(98.3478307787874,12.210158387221,9.9542460629072));
#107535=CARTESIAN_POINT('Ctrl Pts',(96.9697149704917,11.841587774632,10.0330573359423));
#107536=CARTESIAN_POINT('Ctrl Pts',(96.5221950053118,10.4870483567985,10.1118686089774));
#107537=CARTESIAN_POINT('Ctrl Pts',(97.4094906075456,9.37001839722762,10.1906798820125));
#107538=CARTESIAN_POINT('Ctrl Pts',(98.8301588147409,9.49944523468055,10.2694911550476));
#107539=CARTESIAN_POINT('Ctrl Pts',(99.5009929602766,10.7584255400846,10.3483024280826));
#107540=CARTESIAN_POINT('Ctrl Pts',(98.8160674853117,12.0097954801921,10.4271137011177));
#107541=CARTESIAN_POINT('Ctrl Pts',(97.3940357663781,12.1232655169875,10.5059249741528));
#107542=CARTESIAN_POINT('Ctrl Pts',(96.5193362622349,10.99634472218,10.5847362471879));
#107543=CARTESIAN_POINT('Ctrl Pts',(96.9820341406084,9.64691508526005,10.663547520223));
#107544=CARTESIAN_POINT('Ctrl Pts',(98.3642013305314,9.293837846997,10.742358793258));
#107545=CARTESIAN_POINT('Ctrl Pts',(99.417406656716,10.2560271329594,10.8211700662932));
#107546=CARTESIAN_POINT('Ctrl Pts',(99.1903510441992,11.6643933589234,10.8999813393282));
#107547=CARTESIAN_POINT('Ctrl Pts',(97.8881206136871,12.2468412830989,10.9787926123633));
#107548=CARTESIAN_POINT('Ctrl Pts',(96.6869443211705,11.4772795940945,11.0576038853984));
#107549=CARTESIAN_POINT('Ctrl Pts',(96.6717748018918,10.0508085764589,11.1364151584335));
#107550=CARTESIAN_POINT('Ctrl Pts',(97.8563137996289,9.25587647781848,11.2152264314686));
#107551=CARTESIAN_POINT('Ctrl Pts',(99.1706361794572,9.81049919689602,11.2940377045037));
#107552=CARTESIAN_POINT('Ctrl Pts',(99.4275910308938,11.2137183112577,11.3728489775388));
#107553=CARTESIAN_POINT('Ctrl Pts',(98.3950859917484,12.1980876640647,11.4516602505738));
#107554=CARTESIAN_POINT('Ctrl Pts',(97.0057227707638,11.8744837104693,11.5304715236089));
#107555=CARTESIAN_POINT('Ctrl Pts',(96.5144323027452,10.535199067596,11.609282796644));
#107556=CARTESIAN_POINT('Ctrl Pts',(97.3649686737201,9.38993160527404,11.6880940696791));
#107557=CARTESIAN_POINT('Ctrl Pts',(98.78909188209,9.4731347661915,11.7669053427142));
#107558=CARTESIAN_POINT('Ctrl Pts',(99.5004743195226,10.7096559776218,11.8457166157493));
#107559=CARTESIAN_POINT('Ctrl Pts',(98.8565656336517,11.9826175963921,11.9245278887844));
#107560=CARTESIAN_POINT('Ctrl Pts',(97.4389710641154,12.1422274802604,12.0033391618194));
#107561=CARTESIAN_POINT('Ctrl Pts',(96.5281212797658,11.0443193106231,12.0821504348545));
#107562=CARTESIAN_POINT('Ctrl Pts',(96.9467338781784,9.68056963746572,12.1609617078896));
#107563=CARTESIAN_POINT('Ctrl Pts',(98.3167004630095,9.28277416856067,12.2397729809247));
#107564=CARTESIAN_POINT('Ctrl Pts',(99.4006099519555,10.210238398804,12.3185842539598));
#107565=CARTESIAN_POINT('Ctrl Pts',(99.2194299886273,11.6252378685416,12.3973955269949));
#107566=CARTESIAN_POINT('Ctrl Pts',(97.9368098888729,12.2496859116918,12.4762068000299));
#107567=CARTESIAN_POINT('Ctrl Pts',(96.7112657389187,11.5195549542326,12.555018073065));
#107568=CARTESIAN_POINT('Ctrl Pts',(96.6497602406877,10.0943297961264,12.6338293461001));
#107569=CARTESIAN_POINT('Ctrl Pts',(97.807847732039,9.26133337146405,12.7126406191352));
#107570=CARTESIAN_POINT('Ctrl Pts',(99.1394951821687,9.7729628718273,12.7914518921703));
#107571=CARTESIAN_POINT('Ctrl Pts',(99.4419029570818,11.1670931416807,12.8702631652054));
#107572=CARTESIAN_POINT('Ctrl Pts',(98.4419237058598,12.1844874592602,12.9490744382405));
#107573=CARTESIAN_POINT('Ctrl Pts',(97.0427805029951,11.9061927291974,13.0278857112756));
#107574=CARTESIAN_POINT('Ctrl Pts',(96.5082379374112,10.5835764285116,13.1066969843106));
#107575=CARTESIAN_POINT('Ctrl Pts',(97.3211172670363,9.41128079357963,13.1855082573457));
#107576=CARTESIAN_POINT('Ctrl Pts',(98.7471917632435,9.44817242481657,13.2643195303808));
#107577=CARTESIAN_POINT('Ctrl Pts',(99.4983716181923,10.6609288891744,13.3431308034159));
#107578=CARTESIAN_POINT('Ctrl Pts',(98.8961592106945,11.9541386053284,13.421942076451));
#107579=CARTESIAN_POINT('Ctrl Pts',(97.4844991295521,12.1597189858305,13.5007533494861));
#107580=CARTESIAN_POINT('Ctrl Pts',(96.538459394052,11.0919843119044,13.5795646225211));
#107581=CARTESIAN_POINT('Ctrl Pts',(96.9125474411364,9.71535094361666,13.6583758955562));
#107582=CARTESIAN_POINT('Ctrl Pts',(98.2688615767066,9.27326429669935,13.7371871685913));
#107583=CARTESIAN_POINT('Ctrl Pts',(99.3823419004731,10.1650099507019,13.8159984416264));
#107584=CARTESIAN_POINT('Ctrl Pts',(99.2472064930764,11.5851777360694,13.8948097146615));
#107585=CARTESIAN_POINT('Ctrl Pts',(97.9855962350814,12.2509078491674,13.9736209876966));
#107586=CARTESIAN_POINT('Ctrl Pts',(96.7368862852262,11.561097540056,14.0524322607317));
#107587=CARTESIAN_POINT('Ctrl Pts',(96.6292958336403,10.1383817570332,14.1312435337667));
#107588=CARTESIAN_POINT('Ctrl Pts',(97.759332067821,9.26868943644842,14.2100548068018));
#107589=CARTESIAN_POINT('Ctrl Pts',(99.1076631689353,9.73578935090167,14.2888660798369));
#107590=CARTESIAN_POINT('Ctrl Pts',(99.4536375917939,11.1214246027084,14.367677352872));
#107591=CARTESIAN_POINT('Ctrl Pts',(98.8115083393657,11.8170479618875,14.4202182015621));
#107592=CARTESIAN_POINT('Ctrl Pts',(98.4141189012336,11.9537585038707,14.4464886259071));
#107593=CARTESIAN_POINT('Ctrl Pts',(97.4072564351537,11.9831922513677,9.06350339962649));
#107594=CARTESIAN_POINT('Ctrl Pts',(97.0001502138443,11.7875134408477,9.08977382397152));
#107595=CARTESIAN_POINT('Ctrl Pts',(96.401737395307,10.9645566297397,9.14231467266158));
#107596=CARTESIAN_POINT('Ctrl Pts',(96.9445004241546,9.52867977688438,9.22112594569665));
#107597=CARTESIAN_POINT('Ctrl Pts',(98.4423223324868,9.19880815122535,9.29993721873175));
#107598=CARTESIAN_POINT('Ctrl Pts',(99.5397938854681,10.2686538211633,9.37874849176682));
#107599=CARTESIAN_POINT('Ctrl Pts',(99.2468671383022,11.7739516267925,9.45755976480192));
#107600=CARTESIAN_POINT('Ctrl Pts',(97.8275165472081,12.3540379530592,9.536371037837));
#107601=CARTESIAN_POINT('Ctrl Pts',(96.5640595968658,11.4854557820079,9.61518231087209));
#107602=CARTESIAN_POINT('Ctrl Pts',(96.597554985897,9.95249745237383,9.69399358390716));
#107603=CARTESIAN_POINT('Ctrl Pts',(97.8978215452215,9.13991711344024,9.77280485694227));
#107604=CARTESIAN_POINT('Ctrl Pts',(99.2903680039858,9.78161101738929,9.85161612997734));
#107605=CARTESIAN_POINT('Ctrl Pts',(99.5174060453627,11.2980041603985,9.93042740301244));
#107606=CARTESIAN_POINT('Ctrl Pts',(98.3738566088577,12.3194121864219,10.0092386760475));
#107607=CARTESIAN_POINT('Ctrl Pts',(96.8926256939319,11.9232639219484,10.0880499490826));
#107608=CARTESIAN_POINT('Ctrl Pts',(96.4116208295505,10.4673734596933,10.1668612221177));
#107609=CARTESIAN_POINT('Ctrl Pts',(97.3653067743711,9.26676368578688,10.2456724951528));
#107610=CARTESIAN_POINT('Ctrl Pts',(98.8922739970692,9.40587466013485,10.3244837681879));
#107611=CARTESIAN_POINT('Ctrl Pts',(99.6133021350342,10.7590559663949,10.4032950412229));
#107612=CARTESIAN_POINT('Ctrl Pts',(98.8771283085448,12.1040574750769,10.482106314258));
#107613=CARTESIAN_POINT('Ctrl Pts',(97.3486955517258,12.226017709048,10.5609175872931));
#107614=CARTESIAN_POINT('Ctrl Pts',(96.4085481860195,11.0147770354461,10.6397288603282));
#107615=CARTESIAN_POINT('Ctrl Pts',(96.9058666244206,9.5643786845303,10.7185401333633));
#107616=CARTESIAN_POINT('Ctrl Pts',(98.3914520585228,9.18488305903664,10.7973514063984));
#107617=CARTESIAN_POINT('Ctrl Pts',(99.5234616324051,10.2190664765685,10.8761626794335));
#107618=CARTESIAN_POINT('Ctrl Pts',(99.2794169805385,11.7328112437917,10.9549739524685));
#107619=CARTESIAN_POINT('Ctrl Pts',(97.8797494341536,12.3588398158681,11.0337852255036));
#107620=CARTESIAN_POINT('Ctrl Pts',(96.5886972250129,11.5316970185545,11.1125964985387));
#107621=CARTESIAN_POINT('Ctrl Pts',(96.5723926729683,9.99849280026701,11.1914077715738));
#107622=CARTESIAN_POINT('Ctrl Pts',(97.8455627308264,9.14408129675973,11.2702190446089));
#107623=CARTESIAN_POINT('Ctrl Pts',(99.2582269855007,9.74020269140061,11.349030317644));
#107624=CARTESIAN_POINT('Ctrl Pts',(99.5344080345801,11.2484152233922,11.4278415906791));
#107625=CARTESIAN_POINT('Ctrl Pts',(98.424647610534,12.3064382925031,11.5066528637141));
#107626=CARTESIAN_POINT('Ctrl Pts',(96.9313277149234,11.9586212386879,11.5854641367492));
#107627=CARTESIAN_POINT('Ctrl Pts',(96.4032772963324,10.5191269632665,11.6642754097843));
#107628=CARTESIAN_POINT('Ctrl Pts',(97.3174535646642,9.28816686482028,11.7430866828194));
#107629=CARTESIAN_POINT('Ctrl Pts',(98.8481343029613,9.37759555682758,11.8218979558545));
#107630=CARTESIAN_POINT('Ctrl Pts',(99.6127446878923,10.7066373066622,11.9007092288896));
#107631=CARTESIAN_POINT('Ctrl Pts',(98.9206566600503,12.074846053624,11.9795205019247));
#107632=CARTESIAN_POINT('Ctrl Pts',(97.3969930545765,12.2463984680804,12.0583317749597));
#107633=CARTESIAN_POINT('Ctrl Pts',(96.4179905271324,11.0663412386175,12.1371430479948));
#107634=CARTESIAN_POINT('Ctrl Pts',(96.8679250815535,9.60055137978199,12.2159543210299));
#107635=CARTESIAN_POINT('Ctrl Pts',(98.3403970216125,9.17299156019885,12.294765594065));
#107636=CARTESIAN_POINT('Ctrl Pts',(99.5054081435689,10.1698516804113,12.3735768671001));
#107637=CARTESIAN_POINT('Ctrl Pts',(99.3106717061581,11.6907260122797,12.4523881401352));
#107638=CARTESIAN_POINT('Ctrl Pts',(97.9320817992542,12.3618972888235,12.5311994131703));
#107639=CARTESIAN_POINT('Ctrl Pts',(96.6148384503341,11.5771355586244,12.6100106862053));
#107640=CARTESIAN_POINT('Ctrl Pts',(96.5487309106999,10.0452704191281,12.6888219592404));
#107641=CARTESIAN_POINT('Ctrl Pts',(97.7934702744402,9.14994649293456,12.7676332322755));
#107642=CARTESIAN_POINT('Ctrl Pts',(99.2247559175195,9.6998577764161,12.8464445053106));
#107643=CARTESIAN_POINT('Ctrl Pts',(99.5497908256302,11.1983014069949,12.9252557783457));
#107644=CARTESIAN_POINT('Ctrl Pts',(98.4749898747389,12.2918204761452,13.0040670513808));
#107645=CARTESIAN_POINT('Ctrl Pts',(96.9711582271979,11.99270282932,13.0828783244159));
#107646=CARTESIAN_POINT('Ctrl Pts',(96.3966194484392,10.5711240756567,13.1616895974509));
#107647=CARTESIAN_POINT('Ctrl Pts',(97.2703210531204,9.31111346882587,13.240500870486));
#107648=CARTESIAN_POINT('Ctrl Pts',(98.8030990809567,9.35076545188944,13.3193121435211));
#107649=CARTESIAN_POINT('Ctrl Pts',(99.6104846556101,10.6542642989889,13.3981234165562));
#107650=CARTESIAN_POINT('Ctrl Pts',(98.963212757292,12.0442361718308,13.4769346895913));
#107651=CARTESIAN_POINT('Ctrl Pts',(97.4459276779337,12.2651987449824,13.5557459626264));
#107652=CARTESIAN_POINT('Ctrl Pts',(96.4291021727508,11.1175726903089,13.6345572356614));
#107653=CARTESIAN_POINT('Ctrl Pts',(96.8311807041122,9.63793513637353,13.7133685086966));
#107654=CARTESIAN_POINT('Ctrl Pts',(98.2889786742568,9.16277012879724,13.7921797817316));
#107655=CARTESIAN_POINT('Ctrl Pts',(99.4857732170638,10.121239092732,13.8709910547667));
#107656=CARTESIAN_POINT('Ctrl Pts',(99.3405265390038,11.647668450414,13.9498023278018));
#107657=CARTESIAN_POINT('Ctrl Pts',(97.9845184985468,12.3632106556349,14.0286136008369));
#107658=CARTESIAN_POINT('Ctrl Pts',(96.6423760092385,11.6217864958221,14.107424873872));
#107659=CARTESIAN_POINT('Ctrl Pts',(96.5267352901637,10.0926184910139,14.1862361469071));
#107660=CARTESIAN_POINT('Ctrl Pts',(97.7413245104446,9.15785296262414,14.2650474199421));
#107661=CARTESIAN_POINT('Ctrl Pts',(99.1905421295333,9.65990281176058,14.3438586929772));
#107662=CARTESIAN_POINT('Ctrl Pts',(99.5624034838743,11.1492157994153,14.4226699660123));
#107663=CARTESIAN_POINT('Ctrl Pts',(98.8722280324722,11.8968879606069,14.4752108147024));
#107664=CARTESIAN_POINT('Ctrl Pts',(98.4451046242049,12.0438276299459,14.5014812390474));
#107665=CARTESIAN_POINT('Ctrl Pts',(97.3659929054248,12.0690402776369,9.1184960127668));
#107666=CARTESIAN_POINT('Ctrl Pts',(96.930546199862,11.8597393902289,9.14476643711183));
#107667=CARTESIAN_POINT('Ctrl Pts',(96.2904751894988,10.9794928760271,9.19730728580189));
#107668=CARTESIAN_POINT('Ctrl Pts',(96.8710223794995,9.44365821558217,9.27611855883696));
#107669=CARTESIAN_POINT('Ctrl Pts',(98.4731143676917,9.09082275119189,9.35492983187206));
#107670=CARTESIAN_POINT('Ctrl Pts',(99.6469858223152,10.2351451615366,9.43374110490715));
#107671=CARTESIAN_POINT('Ctrl Pts',(99.3336671345917,11.8452334776618,9.51255237794222));
#107672=CARTESIAN_POINT('Ctrl Pts',(97.815509202879,12.4657022066889,9.59136365097732));
#107673=CARTESIAN_POINT('Ctrl Pts',(96.464097365257,11.5366541472455,9.6701749240124));
#107674=CARTESIAN_POINT('Ctrl Pts',(96.4999245180781,9.89697973436806,9.74898619704748));
#107675=CARTESIAN_POINT('Ctrl Pts',(97.8907084461403,9.02783204496239,9.82779747008258));
#107676=CARTESIAN_POINT('Ctrl Pts',(99.3801962900298,9.71419713060421,9.90660874311765));
#107677=CARTESIAN_POINT('Ctrl Pts',(99.623039464563,11.3361531801521,9.98542001615274));
#107678=CARTESIAN_POINT('Ctrl Pts',(98.399882438928,12.4286659856228,10.0642312891878));
#107679=CARTESIAN_POINT('Ctrl Pts',(96.8155364173721,12.0049400692647,10.1430425622229));
#107680=CARTESIAN_POINT('Ctrl Pts',(96.3010466537892,10.447698562588,10.221853835258));
#107681=CARTESIAN_POINT('Ctrl Pts',(97.3211229411965,9.16350897434615,10.3006651082931));
#107682=CARTESIAN_POINT('Ctrl Pts',(98.9543891793977,9.31230408558914,10.3794763813282));
#107683=CARTESIAN_POINT('Ctrl Pts',(99.7256113097918,10.7596863927053,10.4582876543633));
#107684=CARTESIAN_POINT('Ctrl Pts',(98.9381891317781,12.1983194699616,10.5370989273983));
#107685=CARTESIAN_POINT('Ctrl Pts',(97.3033553370735,12.3287699011085,10.6159102004334));
#107686=CARTESIAN_POINT('Ctrl Pts',(96.2977601098042,11.0332093487121,10.6947214734685));
#107687=CARTESIAN_POINT('Ctrl Pts',(96.8296991082329,9.48184228380054,10.7735327465036));
#107688=CARTESIAN_POINT('Ctrl Pts',(98.4187027865141,9.07592827107629,10.8523440195387));
#107689=CARTESIAN_POINT('Ctrl Pts',(99.6295166080943,10.1821058201776,10.9311552925738));
#107690=CARTESIAN_POINT('Ctrl Pts',(99.3684829168778,11.8012291286601,11.0099665656089));
#107691=CARTESIAN_POINT('Ctrl Pts',(97.8713782546199,12.4708383486373,11.0887778386439));
#107692=CARTESIAN_POINT('Ctrl Pts',(96.4904501288555,11.5861144430144,11.167589111679));
#107693=CARTESIAN_POINT('Ctrl Pts',(96.4730105440447,9.94617702407511,11.2464003847141));
#107694=CARTESIAN_POINT('Ctrl Pts',(97.8348116620241,9.03228611570099,11.3252116577492));
#107695=CARTESIAN_POINT('Ctrl Pts',(99.3458177915441,9.66990618590519,11.4040229307843));
#107696=CARTESIAN_POINT('Ctrl Pts',(99.6412250382663,11.2831121355268,11.4828342038194));
#107697=CARTESIAN_POINT('Ctrl Pts',(98.4542092293196,12.4147889209416,11.5616454768544));
#107698=CARTESIAN_POINT('Ctrl Pts',(96.856932659083,12.0427587669064,11.6404567498895));
#107699=CARTESIAN_POINT('Ctrl Pts',(96.2921222899196,10.503054858937,11.7192680229246));
#107700=CARTESIAN_POINT('Ctrl Pts',(97.2699384556081,9.18640212436651,11.7980792959597));
#107701=CARTESIAN_POINT('Ctrl Pts',(98.9071767238326,9.28205634746367,11.8768905689948));
#107702=CARTESIAN_POINT('Ctrl Pts',(99.7250150562619,10.7036186357026,11.9557018420299));
#107703=CARTESIAN_POINT('Ctrl Pts',(98.9847476864488,12.1670745108561,12.034513115065));
#107704=CARTESIAN_POINT('Ctrl Pts',(97.3550150450377,12.3505694559004,12.1133243881001));
#107705=CARTESIAN_POINT('Ctrl Pts',(96.3078597744989,11.0883631666119,12.1921356611351));
#107706=CARTESIAN_POINT('Ctrl Pts',(96.7891162849286,9.52053312209826,12.2709469341702));
#107707=CARTESIAN_POINT('Ctrl Pts',(98.3640935802155,9.06320895183703,12.3497582072053));
#107708=CARTESIAN_POINT('Ctrl Pts',(99.6102063351822,10.1294649620185,12.4285694802404));
#107709=CARTESIAN_POINT('Ctrl Pts',(99.401913423689,11.7562141560178,12.5073807532755));
#107710=CARTESIAN_POINT('Ctrl Pts',(97.9273537096352,12.4741086659552,12.5861920263106));
#107711=CARTESIAN_POINT('Ctrl Pts',(96.5184111617498,11.6347161630161,12.6650032993457));
#107712=CARTESIAN_POINT('Ctrl Pts',(96.447701580712,9.99621104212966,12.7438145723807));
#107713=CARTESIAN_POINT('Ctrl Pts',(97.7790928168414,9.03855961440507,12.8226258454158));
#107714=CARTESIAN_POINT('Ctrl Pts',(99.3100166528703,9.62675268100489,12.9014371184509));
#107715=CARTESIAN_POINT('Ctrl Pts',(99.6576786941785,11.2295096723092,12.980248391486));
#107716=CARTESIAN_POINT('Ctrl Pts',(98.5080560436181,12.3991534930301,13.0590596645211));
#107717=CARTESIAN_POINT('Ctrl Pts',(96.8995359514008,12.0792129294426,13.1378709375562));
#107718=CARTESIAN_POINT('Ctrl Pts',(96.285000959467,10.5586717228019,13.2166822105912));
#107719=CARTESIAN_POINT('Ctrl Pts',(97.2195248392047,9.2109461440721,13.2954934836263));
#107720=CARTESIAN_POINT('Ctrl Pts',(98.85900639867,9.25335847896233,13.3743047566614));
#107721=CARTESIAN_POINT('Ctrl Pts',(99.7225976930278,10.6475997088034,13.4531160296965));
#107722=CARTESIAN_POINT('Ctrl Pts',(99.0302663038896,12.1343337383332,13.5319273027316));
#107723=CARTESIAN_POINT('Ctrl Pts',(97.4073562263153,12.3706785041343,13.6107385757667));
#107724=CARTESIAN_POINT('Ctrl Pts',(96.3197449514496,11.1431610687133,13.6895498488018));
#107725=CARTESIAN_POINT('Ctrl Pts',(96.7498139670879,9.56051932913041,13.7683611218369));
#107726=CARTESIAN_POINT('Ctrl Pts',(98.3090957718069,9.05227596089513,13.8471723948719));
#107727=CARTESIAN_POINT('Ctrl Pts',(99.5892045336545,10.0774682347621,13.925983667907));
#107728=CARTESIAN_POINT('Ctrl Pts',(99.4338465849312,11.7101591647585,14.0047949409421));
#107729=CARTESIAN_POINT('Ctrl Pts',(97.9834407620123,12.4755134621025,14.0836062139772));
#107730=CARTESIAN_POINT('Ctrl Pts',(96.547865733251,11.6824754515883,14.1624174870123));
#107731=CARTESIAN_POINT('Ctrl Pts',(96.4241747466871,10.0468552249946,14.2412287600474));
#107732=CARTESIAN_POINT('Ctrl Pts',(97.7233169530683,9.04701648879988,14.3200400330824));
#107733=CARTESIAN_POINT('Ctrl Pts',(99.2734210901312,9.58401627261947,14.3988513061175));
#107734=CARTESIAN_POINT('Ctrl Pts',(99.6711693759547,11.1770069961223,14.4776625791526));
#107735=CARTESIAN_POINT('Ctrl Pts',(98.9329477255787,11.9767279593263,14.5302034278427));
#107736=CARTESIAN_POINT('Ctrl Pts',(98.4760903471762,12.1338967560211,14.5564738521877));
#107737=CARTESIAN_POINT('Ctrl Pts',(96.5386021580424,10.7493836819919,14.2078409669239));
#107738=CARTESIAN_POINT('Ctrl Pts',(96.5378832918151,10.5440004037554,14.2189702312984));
#107739=CARTESIAN_POINT('Ctrl Pts',(96.5783184588143,10.3389008126099,14.2300994956729));
#107740=CARTESIAN_POINT('Ctrl Pts',(96.6613136121779,10.1528188067278,14.2412287600474));
#107741=CARTESIAN_POINT('Ctrl Pts',(96.8572221488142,9.71357564626303,14.2674991843924));
#107742=CARTESIAN_POINT('Ctrl Pts',(97.2902695509412,9.38029606753146,14.2937696087374));
#107743=CARTESIAN_POINT('Ctrl Pts',(97.7651439415152,9.30315624213561,14.3200400330824));
#107744=CARTESIAN_POINT('Ctrl Pts',(98.195699285931,9.23321571733423,14.3438586929772));
#107745=CARTESIAN_POINT('Ctrl Pts',(98.6606386832877,9.37383596121387,14.367677352872));
#107746=CARTESIAN_POINT('Ctrl Pts',(98.9856388155471,9.66528499663154,14.3914960127668));
#107747=CARTESIAN_POINT('',(97.3153355754606,9.7917048010816,9.1184960127668));
#107748=CARTESIAN_POINT('Ctrl Pts',(97.3138573448686,9.79064797878732,9.1184960127668));
#107749=CARTESIAN_POINT('Ctrl Pts',(97.2816262023953,9.80814453001893,9.1184960127668));
#107750=CARTESIAN_POINT('Ctrl Pts',(97.2503400185293,9.8271834909513,9.1184960127668));
#107751=CARTESIAN_POINT('Ctrl Pts',(97.2201253783783,9.84773709665585,9.1184960127668));
#107752=CARTESIAN_POINT('Ctrl Pts',(97.1801243676892,9.8749479122531,9.1184960127668));
#107753=CARTESIAN_POINT('Ctrl Pts',(97.1419999996926,9.90481142917744,9.1184960127668));
#107754=CARTESIAN_POINT('Ctrl Pts',(97.1058228801383,9.93703307814226,9.1184960127668));
#107755=CARTESIAN_POINT('Ctrl Pts',(97.0945544245732,9.947069483032,9.1184960127668));
#107756=CARTESIAN_POINT('Ctrl Pts',(97.0834750376363,9.95733502451731,9.1184960127668));
#107757=CARTESIAN_POINT('Ctrl Pts',(97.0725872918701,9.96782169999479,9.1184960127668));
#107758=CARTESIAN_POINT('Ctrl Pts',(97.0624427997589,9.97759250094279,9.1184960127668));
#107759=CARTESIAN_POINT('Ctrl Pts',(97.0524629268139,9.98755737105614,9.1184960127668));
#107760=CARTESIAN_POINT('Ctrl Pts',(97.0426666047809,9.99769206046759,9.1184960127668));
#107761=CARTESIAN_POINT('Ctrl Pts',(97.0075321550023,10.0340400628046,9.1184960127668));
#107762=CARTESIAN_POINT('Ctrl Pts',(96.9747093356107,10.0726125260596,9.1184960127668));
#107763=CARTESIAN_POINT('Ctrl Pts',(96.9442739384259,10.1130848201818,9.1184960127668));
#107764=CARTESIAN_POINT('Ctrl Pts',(96.9224967199919,10.1420436664974,9.1184960127668));
#107765=CARTESIAN_POINT('Ctrl Pts',(96.9019421721014,10.1719763617394,9.1184960127668));
#107766=CARTESIAN_POINT('Ctrl Pts',(96.8826466217712,10.2027777804103,9.1184960127668));
#107767=CARTESIAN_POINT('Ctrl Pts',(96.8758695774648,10.2135959522408,9.1184960127668));
#107768=CARTESIAN_POINT('Ctrl Pts',(96.869247914313,10.2245213776691,9.1184960127668));
#107769=CARTESIAN_POINT('Ctrl Pts',(96.8627834610163,10.2355497738227,9.1184960127668));
#107770=CARTESIAN_POINT('Ctrl Pts',(96.8579999807869,10.2437104198265,9.1184960127668));
#107771=CARTESIAN_POINT('Ctrl Pts',(96.8533037921159,10.2519255162684,9.1184960127668));
#107772=CARTESIAN_POINT('Ctrl Pts',(96.8486997486209,10.2601853832081,9.1184960127668));
#107773=CARTESIAN_POINT('Ctrl Pts',(96.8231595708657,10.3060056431825,9.1184960127668));
#107774=CARTESIAN_POINT('Ctrl Pts',(96.8004131575191,10.3532668875542,9.1184960127668));
#107775=CARTESIAN_POINT('Ctrl Pts',(96.7805403871832,10.4016397520554,9.1184960127668));
#107776=CARTESIAN_POINT('Ctrl Pts',(96.7602819368002,10.4509514111153,9.1184960127668));
#107777=CARTESIAN_POINT('Ctrl Pts',(96.743008985931,10.5014191405875,9.1184960127668));
#107778=CARTESIAN_POINT('Ctrl Pts',(96.7288423286544,10.5527330349271,9.1184960127668));
#107779=CARTESIAN_POINT('Ctrl Pts',(96.7204623441663,10.5830866765937,9.1184960127668));
#107780=CARTESIAN_POINT('Ctrl Pts',(96.7131700098127,10.6137370708059,9.1184960127668));
#107781=CARTESIAN_POINT('Ctrl Pts',(96.7069978078214,10.6446242994682,9.1184960127668));
#107782=CARTESIAN_POINT('Ctrl Pts',(96.7038211368344,10.6605211484857,9.1184960127668));
#107783=CARTESIAN_POINT('Ctrl Pts',(96.7009412741981,10.6764807723151,9.1184960127668));
#107784=CARTESIAN_POINT('Ctrl Pts',(96.6983633062362,10.6924951981886,9.1184960127668));
#107785=CARTESIAN_POINT('Ctrl Pts',(96.6965273501873,10.7039002204718,9.1184960127668));
#107786=CARTESIAN_POINT('Ctrl Pts',(96.6948444111156,10.7153349782316,9.1184960127668));
#107787=CARTESIAN_POINT('Ctrl Pts',(96.6933189532335,10.7267746925458,9.1184960127668));
#107788=CARTESIAN_POINT('Ctrl Pts',(96.6860744472355,10.7811026946108,9.1184960127668));
#107789=CARTESIAN_POINT('Ctrl Pts',(96.6823595818324,10.8356469910512,9.1184960127668));
#107790=CARTESIAN_POINT('Ctrl Pts',(96.6822848029741,10.8900777405499,9.1184960127668));
#107791=CARTESIAN_POINT('Ctrl Pts',(96.6822685608941,10.9019001808453,9.1184960127668));
#107792=CARTESIAN_POINT('Ctrl Pts',(96.6824242116089,10.9137173667906,9.1184960127668));
#107793=CARTESIAN_POINT('Ctrl Pts',(96.6827531754784,10.925526069197,9.1184960127668));
#107794=CARTESIAN_POINT('Ctrl Pts',(96.6842167271888,10.9780626794681,9.1184960127668));
#107795=CARTESIAN_POINT('Ctrl Pts',(96.6891065426952,11.0304307823436,9.1184960127668));
#107796=CARTESIAN_POINT('Ctrl Pts',(96.6972216454077,11.0824121493641,9.1184960127668));
#107797=CARTESIAN_POINT('Ctrl Pts',(96.701143463069,11.1075333894095,9.1184960127668));
#107798=CARTESIAN_POINT('Ctrl Pts',(96.7058193396968,11.1325644201795,9.1184960127668));
#107799=CARTESIAN_POINT('Ctrl Pts',(96.7112308078138,11.1574808086853,9.1184960127668));
#107800=CARTESIAN_POINT('Ctrl Pts',(96.7146572466834,11.1732573928251,9.1184960127668));
#107801=CARTESIAN_POINT('Ctrl Pts',(96.7183786513777,11.188988014253,9.1184960127668));
#107802=CARTESIAN_POINT('Ctrl Pts',(96.7223908722737,11.2046664142087,9.1184960127668));
#107803=CARTESIAN_POINT('Ctrl Pts',(96.7249070283208,11.2144986995884,9.1184960127668));
#107804=CARTESIAN_POINT('Ctrl Pts',(96.7275377758382,11.2243107938145,9.1184960127668));
#107805=CARTESIAN_POINT('Ctrl Pts',(96.730277664453,11.234086259318,9.1184960127668));
#107806=CARTESIAN_POINT('Ctrl Pts',(96.7450725356843,11.2868718917602,9.1184960127668));
#107807=CARTESIAN_POINT('Ctrl Pts',(96.7630715066882,11.3386947259173,9.1184960127668));
#107808=CARTESIAN_POINT('Ctrl Pts',(96.7840343095851,11.3893192975371,9.1184960127668));
#107809=CARTESIAN_POINT('Ctrl Pts',(96.8054552476105,11.4410502524366,9.1184960127668));
#107810=CARTESIAN_POINT('Ctrl Pts',(96.8299711992107,11.4915309516225,9.1184960127668));
#107811=CARTESIAN_POINT('Ctrl Pts',(96.8573807452556,11.540510511024,9.1184960127668));
#107812=CARTESIAN_POINT('Ctrl Pts',(96.872786221314,11.5680393664262,9.1184960127668));
#107813=CARTESIAN_POINT('Ctrl Pts',(96.8891067425656,11.5950939415267,9.1184960127668));
#107814=CARTESIAN_POINT('Ctrl Pts',(96.906313477585,11.6216279524499,9.1184960127668));
#107815=CARTESIAN_POINT('Ctrl Pts',(96.9175801783897,11.6390020075443,9.1184960127668));
#107816=CARTESIAN_POINT('Ctrl Pts',(96.9292269360609,11.6561528433843,9.1184960127668));
#107817=CARTESIAN_POINT('Ctrl Pts',(96.9412467190239,11.6730669493708,9.1184960127668));
#107818=CARTESIAN_POINT('Ctrl Pts',(96.9473070401079,11.6815949663442,9.1184960127668));
#107819=CARTESIAN_POINT('Ctrl Pts',(96.9534637066899,11.6900648121644,9.1184960127668));
#107820=CARTESIAN_POINT('Ctrl Pts',(96.9597109884959,11.6984681301698,9.1184960127668));
#107821=CARTESIAN_POINT('Ctrl Pts',(96.994439093181,11.7451814554931,9.1184960127668));
#107822=CARTESIAN_POINT('Ctrl Pts',(97.0318543947935,11.7896964276675,9.1184960127668));
#107823=CARTESIAN_POINT('Ctrl Pts',(97.0717283155403,11.8317549554711,9.1184960127668));
#107824=CARTESIAN_POINT('Ctrl Pts',(97.1117071183608,11.8739241116134,9.1184960127668));
#107825=CARTESIAN_POINT('Ctrl Pts',(97.1541579759603,11.9136249543042,9.1184960127668));
#107826=CARTESIAN_POINT('Ctrl Pts',(97.1988995745023,11.950579789157,9.1184960127668));
#107827=CARTESIAN_POINT('Ctrl Pts',(97.2426124503278,11.9866849387207,9.1184960127668));
#107828=CARTESIAN_POINT('Ctrl Pts',(97.2885125610699,12.0201697994727,9.1184960127668));
#107829=CARTESIAN_POINT('Ctrl Pts',(97.3364691156415,12.0507443169141,9.1184960127668));
#107830=CARTESIAN_POINT('Ctrl Pts',(97.3462254661903,12.0569644407883,9.1184960127668));
#107831=CARTESIAN_POINT('Ctrl Pts',(97.3560670415472,12.0630639797634,9.1184960127668));
#107832=CARTESIAN_POINT('Ctrl Pts',(97.3659929054248,12.0690402776369,9.1184960127668));
#107833=CARTESIAN_POINT('Ctrl Pts',(97.3138573448685,9.79064797878733,9.1184960127668));
#107834=CARTESIAN_POINT('Ctrl Pts',(97.6009341668568,9.58815735646046,9.14231467266158));
#107835=CARTESIAN_POINT('Ctrl Pts',(98.4101263498954,9.44342727335157,9.19240375690137));
#107836=CARTESIAN_POINT('Ctrl Pts',(99.3254100117742,10.3356711404167,9.2687632654862));
#107837=CARTESIAN_POINT('Ctrl Pts',(99.0732671457231,11.6313879250538,9.3475745385213));
#107838=CARTESIAN_POINT('Ctrl Pts',(97.8515312358663,12.1307094457997,9.42638581155637));
#107839=CARTESIAN_POINT('Ctrl Pts',(96.9532436972502,11.513168388854,9.4914820078836));
#107840=CARTESIAN_POINT('Ctrl Pts',(96.8238838120166,10.9366557583736,9.5303077798658));
#107841=CARTESIAN_POINT('Ctrl Pts',(96.8240786690275,10.7501410021477,9.54286312750296));
#107842=CARTESIAN_POINT('Origin',(98.,10.75,9.1184960127668));
#107843=CARTESIAN_POINT('',(96.5365,10.75,9.1184960127668));
#107844=CARTESIAN_POINT('Origin',(98.,10.75,9.1184960127668));
#107845=CARTESIAN_POINT('Origin',(98.,10.75,9.1184960127668));
#107846=CARTESIAN_POINT('',(98.6846644245394,9.7917048010816,9.1184960127668));
#107847=CARTESIAN_POINT('Ctrl Pts',(98.6355914804955,12.0706490290142,9.1184960127668));
#107848=CARTESIAN_POINT('Ctrl Pts',(98.6742459232636,12.0476662825293,9.1184960127668));
#107849=CARTESIAN_POINT('Ctrl Pts',(98.7116923833512,12.0228478308923,9.1184960127668));
#107850=CARTESIAN_POINT('Ctrl Pts',(98.7477773097589,11.9961880312021,9.1184960127668));
#107851=CARTESIAN_POINT('Ctrl Pts',(98.7937429792402,11.9622282684151,9.1184960127668));
#107852=CARTESIAN_POINT('Ctrl Pts',(98.837500916529,11.9252809487968,9.1184960127668));
#107853=CARTESIAN_POINT('Ctrl Pts',(98.8789034740481,11.8856482730193,9.1184960127668));
#107854=CARTESIAN_POINT('Ctrl Pts',(98.8946468210008,11.8705779246444,9.1184960127668));
#107855=CARTESIAN_POINT('Ctrl Pts',(98.9100491720406,11.8551190301289,9.1184960127668));
#107856=CARTESIAN_POINT('Ctrl Pts',(98.9251007544373,11.8392874023257,9.1184960127668));
#107857=CARTESIAN_POINT('Ctrl Pts',(98.9339879045998,11.8299396772894,9.1184960127668));
#107858=CARTESIAN_POINT('Ctrl Pts',(98.9427532639398,11.8204612402146,9.1184960127668));
#107859=CARTESIAN_POINT('Ctrl Pts',(98.9513838800037,11.8108678523316,9.1184960127668));
#107860=CARTESIAN_POINT('Ctrl Pts',(98.9898523430754,11.7681081136552,9.1184960127668));
#107861=CARTESIAN_POINT('Ctrl Pts',(99.0257016044828,11.7230111787601,9.1184960127668));
#107862=CARTESIAN_POINT('Ctrl Pts',(99.0587856979425,11.6758909804124,9.1184960127668));
#107863=CARTESIAN_POINT('Ctrl Pts',(99.0810786704322,11.6441400942423,9.1184960127668));
#107864=CARTESIAN_POINT('Ctrl Pts',(99.1021152266029,11.6114698985822,9.1184960127668));
#107865=CARTESIAN_POINT('Ctrl Pts',(99.1218380897891,11.5779721130894,9.1184960127668));
#107866=CARTESIAN_POINT('Ctrl Pts',(99.130375855498,11.5634713663365,9.1184960127668));
#107867=CARTESIAN_POINT('Ctrl Pts',(99.1386673115564,11.5488155114193,9.1184960127668));
#107868=CARTESIAN_POINT('Ctrl Pts',(99.14670717331,11.5340119227266,9.1184960127668));
#107869=CARTESIAN_POINT('Ctrl Pts',(99.1521866210255,11.5239227579214,9.1184960127668));
#107870=CARTESIAN_POINT('Ctrl Pts',(99.1575500455029,11.5137631182504,9.1184960127668));
#107871=CARTESIAN_POINT('Ctrl Pts',(99.1627878257323,11.5035512284172,9.1184960127668));
#107872=CARTESIAN_POINT('Ctrl Pts',(99.188456039613,11.4535069423098,9.1184960127668));
#107873=CARTESIAN_POINT('Ctrl Pts',(99.2111541768037,11.4021318913227,9.1184960127668));
#107874=CARTESIAN_POINT('Ctrl Pts',(99.2307432138167,11.3497164587869,9.1184960127668));
#107875=CARTESIAN_POINT('Ctrl Pts',(99.2498600002804,11.2985646522673,9.1184960127668));
#107876=CARTESIAN_POINT('Ctrl Pts',(99.2660159096322,11.2464209738408,9.1184960127668));
#107877=CARTESIAN_POINT('Ctrl Pts',(99.2790334447493,11.1935494452341,9.1184960127668));
#107878=CARTESIAN_POINT('Ctrl Pts',(99.2869109368667,11.1615545209964,9.1184960127668));
#107879=CARTESIAN_POINT('Ctrl Pts',(99.2936382121067,11.1292930152132,9.1184960127668));
#107880=CARTESIAN_POINT('Ctrl Pts',(99.2991667226112,11.0968247150207,9.1184960127668));
#107881=CARTESIAN_POINT('Ctrl Pts',(99.3033215590753,11.0724238429494,9.1184960127668));
#107882=CARTESIAN_POINT('Ctrl Pts',(99.3067991965717,11.0479061914403,9.1184960127668));
#107883=CARTESIAN_POINT('Ctrl Pts',(99.3095762909331,11.0232979807197,9.1184960127668));
#107884=CARTESIAN_POINT('Ctrl Pts',(99.3106554499975,11.0137354055235,9.1184960127668));
#107885=CARTESIAN_POINT('Ctrl Pts',(99.3116282087408,11.0041638628727,9.1184960127668));
#107886=CARTESIAN_POINT('Ctrl Pts',(99.3124928851242,10.9945927765962,9.1184960127668));
#107887=CARTESIAN_POINT('Ctrl Pts',(99.3172366087752,10.9420845906342,9.1184960127668));
#107888=CARTESIAN_POINT('Ctrl Pts',(99.3187397604984,10.8895172404699,9.1184960127668));
#107889=CARTESIAN_POINT('Ctrl Pts',(99.3168456041743,10.8371362369631,9.1184960127668));
#107890=CARTESIAN_POINT('Ctrl Pts',(99.3164267682064,10.825553746108,9.1184960127668));
#107891=CARTESIAN_POINT('Ctrl Pts',(99.3158416245084,10.8139803933148,9.1184960127668));
#107892=CARTESIAN_POINT('Ctrl Pts',(99.3150881341521,10.8024188959489,9.1184960127668));
#107893=CARTESIAN_POINT('Ctrl Pts',(99.3115311410324,10.7478406704473,9.1184960127668));
#107894=CARTESIAN_POINT('Ctrl Pts',(99.304226566631,10.6935245877712,9.1184960127668));
#107895=CARTESIAN_POINT('Ctrl Pts',(99.2933434227707,10.6397729100594,9.1184960127668));
#107896=CARTESIAN_POINT('Ctrl Pts',(99.2886881485009,10.6167805830786,9.1184960127668));
#107897=CARTESIAN_POINT('Ctrl Pts',(99.2833774775542,10.5938918575654,9.1184960127668));
#107898=CARTESIAN_POINT('Ctrl Pts',(99.2774220930974,10.5711322064764,9.1184960127668));
#107899=CARTESIAN_POINT('Ctrl Pts',(99.2730409956331,10.5543889969661,9.1184960127668));
#107900=CARTESIAN_POINT('Ctrl Pts',(99.2683109576553,10.5377156641035,9.1184960127668));
#107901=CARTESIAN_POINT('Ctrl Pts',(99.2632357869822,10.5211228325942,9.1184960127668));
#107902=CARTESIAN_POINT('Ctrl Pts',(99.2603236688996,10.5116019144236,9.1184960127668));
#107903=CARTESIAN_POINT('Ctrl Pts',(99.2573006399554,10.5021165033124,9.1184960127668));
#107904=CARTESIAN_POINT('Ctrl Pts',(99.2541689602905,10.4926711758706,9.1184960127668));
#107905=CARTESIAN_POINT('Ctrl Pts',(99.2376426939,10.4428269982574,9.1184960127668));
#107906=CARTESIAN_POINT('Ctrl Pts',(99.2180864219794,10.3940707106807,9.1184960127668));
#107907=CARTESIAN_POINT('Ctrl Pts',(99.1956728157365,10.3466608440923,9.1184960127668));
#107908=CARTESIAN_POINT('Ctrl Pts',(99.1733697042633,10.2994846990314,9.1184960127668));
#107909=CARTESIAN_POINT('Ctrl Pts',(99.1482365664014,10.2536408379213,9.1184960127668));
#107910=CARTESIAN_POINT('Ctrl Pts',(99.1204044127404,10.2094167710738,9.1184960127668));
#107911=CARTESIAN_POINT('Ctrl Pts',(99.1064931374631,10.1873123671065,9.1184960127668));
#107912=CARTESIAN_POINT('Ctrl Pts',(99.0919070356358,10.1656132292874,9.1184960127668));
#107913=CARTESIAN_POINT('Ctrl Pts',(99.076659703857,10.1443594016445,9.1184960127668));
#107914=CARTESIAN_POINT('Ctrl Pts',(99.0654152076224,10.1286852765996,9.1184960127668));
#107915=CARTESIAN_POINT('Ctrl Pts',(99.0538110530504,10.1132533986003,9.1184960127668));
#107916=CARTESIAN_POINT('Ctrl Pts',(99.0418521973943,10.0980809672068,9.1184960127668));
#107917=CARTESIAN_POINT('Ctrl Pts',(99.0360652404285,10.0907389430143,9.1184960127668));
#107918=CARTESIAN_POINT('Ctrl Pts',(99.0301957732572,10.083458542508,9.1184960127668));
#107919=CARTESIAN_POINT('Ctrl Pts',(99.0242527358895,10.0762514482787,9.1184960127668));
#107920=CARTESIAN_POINT('Ctrl Pts',(98.9921687683648,10.0373433676301,9.1184960127668));
#107921=CARTESIAN_POINT('Ctrl Pts',(98.9578814680878,10.0004893575788,9.1184960127668));
#107922=CARTESIAN_POINT('Ctrl Pts',(98.9215213654119,9.96594155220527,9.1184960127668));
#107923=CARTESIAN_POINT('Ctrl Pts',(98.8858968563399,9.93209267622934,9.1184960127668));
#107924=CARTESIAN_POINT('Ctrl Pts',(98.8482818182359,9.90045705616418,9.1184960127668));
#107925=CARTESIAN_POINT('Ctrl Pts',(98.8087752824265,9.87131542359124,9.1184960127668));
#107926=CARTESIAN_POINT('Ctrl Pts',(98.769268746617,9.84217379101829,9.1184960127668));
#107927=CARTESIAN_POINT('Ctrl Pts',(98.7278700859694,9.81552546429294,9.1184960127668));
#107928=CARTESIAN_POINT('Ctrl Pts',(98.6846644245395,9.79170480108161,9.1184960127668));
#107929=CARTESIAN_POINT('Origin',(98.,10.75,9.1184960127668));
#107930=CARTESIAN_POINT('Origin',(98.,10.75,8.19412889803065));
#107931=CARTESIAN_POINT('Ctrl Pts',(98.6846644245394,9.79170480108159,9.1184960127668));
#107932=CARTESIAN_POINT('Ctrl Pts',(99.0010205619527,10.0177288832392,9.14476643711183));
#107933=CARTESIAN_POINT('Ctrl Pts',(99.3870316775812,10.8039329633741,9.19730728580188));
#107934=CARTESIAN_POINT('Ctrl Pts',(98.7148371953222,11.9414877424438,9.27611855883697));
#107935=CARTESIAN_POINT('Ctrl Pts',(97.3959638426784,12.0001663543762,9.35492983187205));
#107936=CARTESIAN_POINT('Ctrl Pts',(96.8468201417438,11.2403713725409,9.41093327826995));
#107937=CARTESIAN_POINT('Ctrl Pts',(96.8207258531474,10.8019570759813,9.44066630032281));
#107938=CARTESIAN_POINT('Ctrl Pts',(96.8211250403636,10.7508514088176,9.44412889803065));
#107939=CARTESIAN_POINT('Ctrl Pts',(98.8507802040446,9.55919972522428,8.95351817334586));
#107940=CARTESIAN_POINT('Ctrl Pts',(99.2438918211996,9.840062594456,8.97978859769089));
#107941=CARTESIAN_POINT('Ctrl Pts',(99.7235583614009,10.8170183756298,9.03232944638095));
#107942=CARTESIAN_POINT('Ctrl Pts',(98.8882736025083,12.2305708436141,9.11114071941604));
#107943=CARTESIAN_POINT('Ctrl Pts',(97.2494103873996,12.3034862743618,9.18995199245111));
#107944=CARTESIAN_POINT('Ctrl Pts',(96.2891274572576,10.9748392367607,9.26876326548621));
#107945=CARTESIAN_POINT('Ctrl Pts',(96.8738712604091,9.44231572200386,9.34757453852128));
#107946=CARTESIAN_POINT('Ctrl Pts',(98.4759321306034,9.09133827696001,9.42638581155638));
#107947=CARTESIAN_POINT('Ctrl Pts',(99.6480368958664,10.2383404251759,9.50519708459146));
#107948=CARTESIAN_POINT('Ctrl Pts',(99.3316025376815,11.8475901717513,9.58400835762655));
#107949=CARTESIAN_POINT('Ctrl Pts',(97.8123909963197,12.4654035568644,9.66281963066163));
#107950=CARTESIAN_POINT('Ctrl Pts',(96.4626446905293,11.5338159711112,9.74163090369672));
#107951=CARTESIAN_POINT('Ctrl Pts',(96.5014975453548,9.89424157261291,9.8204421767318));
#107952=CARTESIAN_POINT('Ctrl Pts',(97.8938626320415,9.02762961555281,9.89925344976689));
#107953=CARTESIAN_POINT('Ctrl Pts',(99.38209434996,9.71673178822254,9.97806472280197));
#107954=CARTESIAN_POINT('Ctrl Pts',(99.6219612123826,11.3391263786206,10.0568759958371));
#107955=CARTESIAN_POINT('Ctrl Pts',(98.3968046496415,12.4293967180445,10.1356872688721));
#107956=CARTESIAN_POINT('Ctrl Pts',(96.8132376708772,12.0027660813303,10.2144985419073));
#107957=CARTESIAN_POINT('Ctrl Pts',(96.3016039690137,10.4445845899381,10.2933098149423));
#107958=CARTESIAN_POINT('Ctrl Pts',(97.3240325846763,9.16226714483924,10.3721210879774));
#107959=CARTESIAN_POINT('Ctrl Pts',(98.9570232088569,9.31405633926968,10.4509323610125));
#107960=CARTESIAN_POINT('Ctrl Pts',(99.72559047614,10.7628498886576,10.5297436340476));
#107961=CARTESIAN_POINT('Ctrl Pts',(98.9355322940975,12.2000368716401,10.6085549070827));
#107962=CARTESIAN_POINT('Ctrl Pts',(97.3004622418451,12.3274899473353,10.6873661801177));
#107963=CARTESIAN_POINT('Ctrl Pts',(96.2972439316179,11.0300881631277,10.7661774531528));
#107964=CARTESIAN_POINT('Ctrl Pts',(96.8320260758406,9.47969904384205,10.8449887261879));
#107965=CARTESIAN_POINT('Ctrl Pts',(98.4217710879573,9.07669884453082,10.923799999223));
#107966=CARTESIAN_POINT('Ctrl Pts',(99.6305548240495,10.1850941909808,11.0026112722581));
#107967=CARTESIAN_POINT('Ctrl Pts',(99.3665532878948,11.8037360763359,11.0814225452932));
#107968=CARTESIAN_POINT('Ctrl Pts',(97.8682237019579,12.470599492792,11.1602338183283));
#107969=CARTESIAN_POINT('Ctrl Pts',(96.48891997648,11.5833455284612,11.2390450913634));
#107970=CARTESIAN_POINT('Ctrl Pts',(96.4744868894682,9.94337905006212,11.3178563643984));
#107971=CARTESIAN_POINT('Ctrl Pts',(97.8379610083861,9.03198632936451,11.3966676374335));
#107972=CARTESIAN_POINT('Ctrl Pts',(99.3477955175543,9.67237536676738,11.4754789104686));
#107973=CARTESIAN_POINT('Ctrl Pts',(99.6402447791345,11.286120016238,11.5542901835037));
#107974=CARTESIAN_POINT('Ctrl Pts',(98.451156396063,12.4156186579111,11.6331014565388));
#107975=CARTESIAN_POINT('Ctrl Pts',(96.8545646983056,12.0406609070249,11.7119127295739));
#107976=CARTESIAN_POINT('Ctrl Pts',(96.2925780427725,10.4999242769354,11.790724002609));
#107977=CARTESIAN_POINT('Ctrl Pts',(97.2728062670646,9.18506649276444,11.869535275644));
#107978=CARTESIAN_POINT('Ctrl Pts',(98.9098662667154,9.28372206455016,11.9483465486791));
#107979=CARTESIAN_POINT('Ctrl Pts',(99.7250970230171,10.7067811561831,12.0271578217142));
#107980=CARTESIAN_POINT('Ctrl Pts',(98.9821480412829,12.1688773140378,12.1059690947493));
#107981=CARTESIAN_POINT('Ctrl Pts',(97.3520818961143,12.3493841746056,12.1847803677844));
#107982=CARTESIAN_POINT('Ctrl Pts',(96.3072424645522,11.0852603964275,12.2635916408195));
#107983=CARTESIAN_POINT('Ctrl Pts',(96.7913723940551,9.51831541479055,12.3424029138545));
#107984=CARTESIAN_POINT('Ctrl Pts',(98.3671852964514,9.06387943325478,12.4212141868896));
#107985=CARTESIAN_POINT('Ctrl Pts',(99.6113410909875,10.1324180255,12.5000254599247));
#107986=CARTESIAN_POINT('Ctrl Pts',(99.4000662606059,11.7587824708276,12.5788367329598));
#107987=CARTESIAN_POINT('Ctrl Pts',(97.9241930617252,12.4739724235433,12.6576480059949));
#107988=CARTESIAN_POINT('Ctrl Pts',(96.5167918600261,11.6319984217279,12.73645927903));
#107989=CARTESIAN_POINT('Ctrl Pts',(96.4490862427128,9.99336658252459,12.8152705520651));
#107990=CARTESIAN_POINT('Ctrl Pts',(97.7822307649859,9.03815766515614,12.8940818251002));
#107991=CARTESIAN_POINT('Ctrl Pts',(99.3120735470219,9.6291563119054,12.9728930981352));
#107992=CARTESIAN_POINT('Ctrl Pts',(99.6567966903475,11.2325477982826,13.0517043711703));
#107993=CARTESIAN_POINT('Ctrl Pts',(98.5050317462293,12.4000820027069,13.1305156442054));
#107994=CARTESIAN_POINT('Ctrl Pts',(96.8971011503598,12.0771930507722,13.2093269172405));
#107995=CARTESIAN_POINT('Ctrl Pts',(96.2853546296468,10.5555281038632,13.2881381902756));
#107996=CARTESIAN_POINT('Ctrl Pts',(97.2223480154194,9.20951780908093,13.3669494633107));
#107997=CARTESIAN_POINT('Ctrl Pts',(98.861748088782,9.25493641821538,13.4457607363457));
#107998=CARTESIAN_POINT('Ctrl Pts',(99.7227834757332,10.6507569228509,13.5245720093808));
#107999=CARTESIAN_POINT('Ctrl Pts',(99.0277243461271,12.1362220213605,13.6033832824159));
#108000=CARTESIAN_POINT('Ctrl Pts',(97.4043906860898,12.3695851463718,13.682194555451));
#108001=CARTESIAN_POINT('Ctrl Pts',(96.3190179094369,11.1400880858094,13.7610058284861));
#108002=CARTESIAN_POINT('Ctrl Pts',(96.7520155781748,9.55821310062242,13.8398171015212));
#108003=CARTESIAN_POINT('Ctrl Pts',(98.3121696742768,9.05287884967496,13.9186283745563));
#108004=CARTESIAN_POINT('Ctrl Pts',(99.5905115302468,10.0803156107518,13.9974396475913));
#108005=CARTESIAN_POINT('Ctrl Pts',(99.4319280686622,11.712922398781,14.0762509206264));
#108006=CARTESIAN_POINT('Ctrl Pts',(97.9805929922645,12.4752036805041,14.1550621936615));
#108007=CARTESIAN_POINT('Ctrl Pts',(96.5455179502704,11.680377333606,14.2338734666966));
#108008=CARTESIAN_POINT('Ctrl Pts',(96.4267930226957,10.042776771883,14.3126847397317));
#108009=CARTESIAN_POINT('Ctrl Pts',(97.2912023327567,9.38147568097394,14.3652255884217));
#108010=CARTESIAN_POINT('Ctrl Pts',(97.7682422725578,9.30496691879707,14.3914960127668));
#108011=CARTESIAN_POINT('Ctrl Pts',(98.7954082775428,9.63670141717672,9.00851078648618));
#108012=CARTESIAN_POINT('Ctrl Pts',(99.162934734784,9.89928469071707,9.0347812108312));
#108013=CARTESIAN_POINT('Ctrl Pts',(99.6113828001277,10.8126565715445,9.08732205952127));
#108014=CARTESIAN_POINT('Ctrl Pts',(98.8304614667797,12.1342098098907,9.16613333255634));
#108015=CARTESIAN_POINT('Ctrl Pts',(97.2982615391592,12.2023796343666,9.24494460559143));
#108016=CARTESIAN_POINT('Ctrl Pts',(96.4004773784714,10.9602058665513,9.32375587862652));
#108017=CARTESIAN_POINT('Ctrl Pts',(96.9471638893438,9.52742465776002,9.4025671516616));
#108018=CARTESIAN_POINT('Ctrl Pts',(98.4449567049526,9.19929012466724,9.48137842469669));
#108019=CARTESIAN_POINT('Ctrl Pts',(99.5407765512603,10.2716411252115,9.56018969773177));
#108020=CARTESIAN_POINT('Ctrl Pts',(99.2449369130049,11.7761549385027,9.63900097076687));
#108021=CARTESIAN_POINT('Ctrl Pts',(97.8246012850799,12.3537587404712,9.71781224380194));
#108022=CARTESIAN_POINT('Ctrl Pts',(96.5627014675891,11.4828023248875,9.79662351683703));
#108023=CARTESIAN_POINT('Ctrl Pts',(96.5990256347329,9.94993750032636,9.87543478987212));
#108024=CARTESIAN_POINT('Ctrl Pts',(97.9007704450228,9.13972785888631,9.9542460629072));
#108025=CARTESIAN_POINT('Ctrl Pts',(99.2921425311463,9.78398071010284,10.0330573359423));
#108026=CARTESIAN_POINT('Ctrl Pts',(99.5163979698276,11.3007838520995,10.1118686089774));
#108027=CARTESIAN_POINT('Ctrl Pts',(98.3709791334962,12.3200953600714,10.1906798820125));
#108028=CARTESIAN_POINT('Ctrl Pts',(96.8904765583723,11.9212314252,10.2694911550475));
#108029=CARTESIAN_POINT('Ctrl Pts',(96.412141872636,10.4644621559158,10.3483024280826));
#108030=CARTESIAN_POINT('Ctrl Pts',(97.3680270474777,9.26560267914335,10.4271137011177));
#108031=CARTESIAN_POINT('Ctrl Pts',(98.8947365941362,9.40751287065647,10.5059249741528));
#108032=CARTESIAN_POINT('Ctrl Pts',(99.6132826573136,10.7620135703149,10.5847362471879));
#108033=CARTESIAN_POINT('Ctrl Pts',(98.8746443877,12.1056631018939,10.663547520223));
#108034=CARTESIAN_POINT('Ctrl Pts',(97.3459907498493,12.2248210594066,10.7423587932581));
#108035=CARTESIAN_POINT('Ctrl Pts',(96.4080656026213,11.0118589881787,10.8211700662931));
#108036=CARTESIAN_POINT('Ctrl Pts',(96.9080421443586,9.56237493456568,10.8999813393282));
#108037=CARTESIAN_POINT('Ctrl Pts',(98.3943206635447,9.18560348071698,10.9787926123633));
#108038=CARTESIAN_POINT('Ctrl Pts',(99.5244322774211,10.2218603531326,11.0576038853984));
#108039=CARTESIAN_POINT('Ctrl Pts',(99.2776129389559,11.7351550300284,11.1364151584335));
#108040=CARTESIAN_POINT('Ctrl Pts',(97.8768001914615,12.3586165056458,11.2152264314686));
#108041=CARTESIAN_POINT('Ctrl Pts',(96.5872666606209,11.5291083152149,11.2940377045037));
#108042=CARTESIAN_POINT('Ctrl Pts',(96.5737729323643,9.99587692876494,11.3728489775387));
#108043=CARTESIAN_POINT('Ctrl Pts',(97.8485071060636,9.14380102162829,11.4516602505738));
#108044=CARTESIAN_POINT('Ctrl Pts',(99.2600759937777,9.74251116882779,11.5304715236089));
#108045=CARTESIAN_POINT('Ctrl Pts',(99.5334915743428,11.2512273400872,11.609282796644));
#108046=CARTESIAN_POINT('Ctrl Pts',(98.4217934669718,12.3072140271177,11.6880940696791));
#108047=CARTESIAN_POINT('Ctrl Pts',(96.9291138698029,11.9566599152967,11.7669053427142));
#108048=CARTESIAN_POINT('Ctrl Pts',(96.4037033871018,10.5162001311355,11.8457166157493));
#108049=CARTESIAN_POINT('Ctrl Pts',(97.3201347283301,9.28691816106932,11.9245278887843));
#108050=CARTESIAN_POINT('Ctrl Pts',(98.8506488004328,9.37915286287718,12.0033391618194));
#108051=CARTESIAN_POINT('Ctrl Pts',(99.6128213199474,10.7095939985976,12.0821504348545));
#108052=CARTESIAN_POINT('Ctrl Pts',(98.9182262094195,12.0765315236982,12.1609617078896));
#108053=CARTESIAN_POINT('Ctrl Pts',(97.3942508058477,12.2452903292819,12.2397729809247));
#108054=CARTESIAN_POINT('Ctrl Pts',(96.4174133940031,11.0634404082077,12.3185842539598));
#108055=CARTESIAN_POINT('Ctrl Pts',(96.8700343547427,9.59847800907903,12.3973955269949));
#108056=CARTESIAN_POINT('Ctrl Pts',(98.3432875175056,9.17361840420285,12.4762068000299));
#108057=CARTESIAN_POINT('Ctrl Pts',(99.506469045264,10.1726125475848,12.555018073065));
#108058=CARTESIAN_POINT('Ctrl Pts',(99.3089447632893,11.6931271716501,12.6338293461001));
#108059=CARTESIAN_POINT('Ctrl Pts',(97.9291268580154,12.3617699135724,12.7126406191352));
#108060=CARTESIAN_POINT('Ctrl Pts',(96.6133245387638,11.5745946980042,12.7914518921703));
#108061=CARTESIAN_POINT('Ctrl Pts',(96.5500254537696,10.0426110874884,12.8702631652054));
#108062=CARTESIAN_POINT('Ctrl Pts',(97.7964039932982,9.14957070403135,12.9490744382404));
#108063=CARTESIAN_POINT('Ctrl Pts',(99.2266789413822,9.70210497011587,13.0278857112755));
#108064=CARTESIAN_POINT('Ctrl Pts',(99.5489662258748,11.2011418004784,13.1066969843106));
#108065=CARTESIAN_POINT('Ctrl Pts',(98.4721624098248,12.2926885549735,13.1855082573457));
#108066=CARTESIAN_POINT('Ctrl Pts',(96.9688818920255,11.9908144118339,13.2643195303808));
#108067=CARTESIAN_POINT('Ctrl Pts',(96.3969501004541,10.5681850550808,13.3431308034159));
#108068=CARTESIAN_POINT('Ctrl Pts',(97.2729604865715,9.30977809516568,13.421942076451));
#108069=CARTESIAN_POINT('Ctrl Pts',(98.8056623317227,9.35224069301209,13.5007533494861));
#108070=CARTESIAN_POINT('Ctrl Pts',(99.6106583468889,10.6572160298536,13.5795646225211));
#108071=CARTESIAN_POINT('Ctrl Pts',(98.9608362395547,12.0460015584055,13.6583758955562));
#108072=CARTESIAN_POINT('Ctrl Pts',(97.4431551460489,12.2641765469923,13.7371871685913));
#108073=CARTESIAN_POINT('Ctrl Pts',(96.4284224493248,11.1146997085129,13.8159984416264));
#108074=CARTESIAN_POINT('Ctrl Pts',(96.8332390261959,9.63577900575786,13.8948097146615));
#108075=CARTESIAN_POINT('Ctrl Pts',(98.29185251577,9.16333377934252,13.9736209876966));
#108076=CARTESIAN_POINT('Ctrl Pts',(99.4869951494774,10.1239011509472,14.0524322607317));
#108077=CARTESIAN_POINT('Ctrl Pts',(99.3387328868789,11.6502518429328,14.1312435337667));
#108078=CARTESIAN_POINT('Ctrl Pts',(97.9818560722007,12.3629210357702,14.2100548068018));
#108079=CARTESIAN_POINT('Ctrl Pts',(96.6401810286692,11.6198249311283,14.2888660798369));
#108080=CARTESIAN_POINT('Ctrl Pts',(96.5291831590731,10.0888054787351,14.367677352872));
#108081=CARTESIAN_POINT('Ctrl Pts',(97.337333509938,9.47054431191841,14.4202182015621));
#108082=CARTESIAN_POINT('Ctrl Pts',(97.7833259237631,9.39901502333043,14.4464886259071));
#108083=CARTESIAN_POINT('Ctrl Pts',(98.7400363510412,9.71420310912915,9.06350339962649));
#108084=CARTESIAN_POINT('Ctrl Pts',(99.0819776483683,9.95850678697813,9.08977382397152));
#108085=CARTESIAN_POINT('Ctrl Pts',(99.4992072388545,10.8082947674593,9.14231467266157));
#108086=CARTESIAN_POINT('Ctrl Pts',(98.7726493310509,12.0378487761672,9.22112594569666));
#108087=CARTESIAN_POINT('Ctrl Pts',(97.3471126909189,12.1012729943714,9.29993721873174));
#108088=CARTESIAN_POINT('Ctrl Pts',(96.5118272996849,10.9455724963419,9.37874849176683));
#108089=CARTESIAN_POINT('Ctrl Pts',(97.0204565182787,9.61253359351617,9.45755976480191));
#108090=CARTESIAN_POINT('Ctrl Pts',(98.4139812793017,9.3072419723745,9.536371037837));
#108091=CARTESIAN_POINT('Ctrl Pts',(99.4335162066539,10.304941825247,9.61518231087208));
#108092=CARTESIAN_POINT('Ctrl Pts',(99.1582712883284,11.7047197052541,9.69399358390718));
#108093=CARTESIAN_POINT('Ctrl Pts',(97.8368115738402,12.2421139240781,9.77280485694225));
#108094=CARTESIAN_POINT('Ctrl Pts',(96.6627582446489,11.4317886786638,9.85161612997734));
#108095=CARTESIAN_POINT('Ctrl Pts',(96.6965537241111,10.0056334280398,9.93042740301242));
#108096=CARTESIAN_POINT('Ctrl Pts',(97.907678258004,9.25182610221983,10.0092386760475));
#108097=CARTESIAN_POINT('Ctrl Pts',(99.2021907123328,9.85122963198313,10.0880499490826));
#108098=CARTESIAN_POINT('Ctrl Pts',(99.4108347272724,11.2624413255784,10.1668612221177));
#108099=CARTESIAN_POINT('Ctrl Pts',(98.3451536173513,12.2107940020982,10.2456724951528));
#108100=CARTESIAN_POINT('Ctrl Pts',(96.9677154458671,11.8396967690697,10.3244837681879));
#108101=CARTESIAN_POINT('Ctrl Pts',(96.5226797762587,10.4843397218936,10.4032950412229));
#108102=CARTESIAN_POINT('Ctrl Pts',(97.4120215102787,9.36893821344744,10.482106314258));
#108103=CARTESIAN_POINT('Ctrl Pts',(98.8324499794158,9.50096940204327,10.5609175872931));
#108104=CARTESIAN_POINT('Ctrl Pts',(99.5009748384872,10.7611772519721,10.6397288603282));
#108105=CARTESIAN_POINT('Ctrl Pts',(98.8137564813025,12.0112893321476,10.7185401333633));
#108106=CARTESIAN_POINT('Ctrl Pts',(97.3915192578535,12.1221521714779,10.7973514063984));
#108107=CARTESIAN_POINT('Ctrl Pts',(96.5188872736248,10.9936298132297,10.8761626794335));
#108108=CARTESIAN_POINT('Ctrl Pts',(96.9840582128766,9.64505082528932,10.9549739524685));
#108109=CARTESIAN_POINT('Ctrl Pts',(98.3668702391322,9.29450811690314,11.0337852255036));
#108110=CARTESIAN_POINT('Ctrl Pts',(99.4183097307926,10.2586265152843,11.1125964985387));
#108111=CARTESIAN_POINT('Ctrl Pts',(99.1886725900172,11.6665739837209,11.1914077715738));
#108112=CARTESIAN_POINT('Ctrl Pts',(97.885376680965,12.2466335184996,11.2702190446089));
#108113=CARTESIAN_POINT('Ctrl Pts',(96.685613344762,11.4748711019686,11.349030317644));
#108114=CARTESIAN_POINT('Ctrl Pts',(96.67305897526,10.0483748074678,11.4278415906791));
#108115=CARTESIAN_POINT('Ctrl Pts',(97.8590532037414,9.25561571389206,11.5066528637141));
#108116=CARTESIAN_POINT('Ctrl Pts',(99.1723564700011,9.8126469708882,11.5854641367492));
#108117=CARTESIAN_POINT('Ctrl Pts',(99.4267383695512,11.2163346639364,11.6642754097843));
#108118=CARTESIAN_POINT('Ctrl Pts',(98.3924305378805,12.1988093963244,11.7430866828194));
#108119=CARTESIAN_POINT('Ctrl Pts',(97.0036630413004,11.8726589235686,11.8218979558545));
#108120=CARTESIAN_POINT('Ctrl Pts',(96.514828731431,10.5324759853356,11.9007092288896));
#108121=CARTESIAN_POINT('Ctrl Pts',(97.3674631895958,9.3887698293742,11.9795205019247));
#108122=CARTESIAN_POINT('Ctrl Pts',(98.7914313341501,9.47458366120421,12.0583317749597));
#108123=CARTESIAN_POINT('Ctrl Pts',(99.5005456168779,10.712406841012,12.1371430479948));
#108124=CARTESIAN_POINT('Ctrl Pts',(98.8543043775559,11.9841857333585,12.2159543210299));
#108125=CARTESIAN_POINT('Ctrl Pts',(97.4364197155815,12.1411964839582,12.294765594065));
#108126=CARTESIAN_POINT('Ctrl Pts',(96.5275843234539,11.0416204199878,12.3735768671001));
#108127=CARTESIAN_POINT('Ctrl Pts',(96.9486963154304,9.67864060336751,12.4523881401352));
#108128=CARTESIAN_POINT('Ctrl Pts',(98.31938973856,9.2833573751509,12.5311994131703));
#108129=CARTESIAN_POINT('Ctrl Pts',(99.4015969995403,10.2128070696696,12.6100106862053));
#108130=CARTESIAN_POINT('Ctrl Pts',(99.2178232659729,11.6274718724726,12.6888219592404));
#108131=CARTESIAN_POINT('Ctrl Pts',(97.9340606543056,12.2495674036014,12.7676332322755));
#108132=CARTESIAN_POINT('Ctrl Pts',(96.7098572175013,11.5171909742806,12.8464445053106));
#108133=CARTESIAN_POINT('Ctrl Pts',(96.6509646648264,10.0918555924522,12.9252557783457));
#108134=CARTESIAN_POINT('Ctrl Pts',(97.8105772216106,9.26098374290656,13.0040670513808));
#108135=CARTESIAN_POINT('Ctrl Pts',(99.1412843357424,9.77505362832634,13.0828783244159));
#108136=CARTESIAN_POINT('Ctrl Pts',(99.4411357614023,11.1697358026742,13.1616895974509));
#108137=CARTESIAN_POINT('Ctrl Pts',(98.4392930734199,12.1852951072401,13.240500870486));
#108138=CARTESIAN_POINT('Ctrl Pts',(97.0406626336916,11.9044357728958,13.3193121435211));
#108139=CARTESIAN_POINT('Ctrl Pts',(96.5085455712611,10.5808420062985,13.3981234165562));
#108140=CARTESIAN_POINT('Ctrl Pts',(97.3235729577238,9.41003838125043,13.4769346895913));
#108141=CARTESIAN_POINT('Ctrl Pts',(98.7495765746631,9.44954496780881,13.5557459626264));
#108142=CARTESIAN_POINT('Ctrl Pts',(99.4985332180447,10.6636751368563,13.6345572356615));
#108143=CARTESIAN_POINT('Ctrl Pts',(98.8939481329824,11.9557810954505,13.7133685086965));
#108144=CARTESIAN_POINT('Ctrl Pts',(97.4819196060078,12.1587679476128,13.7921797817316));
#108145=CARTESIAN_POINT('Ctrl Pts',(96.5378269892129,11.0893113312165,13.8709910547667));
#108146=CARTESIAN_POINT('Ctrl Pts',(96.914462474217,9.7133449108933,13.9498023278018));
#108147=CARTESIAN_POINT('Ctrl Pts',(98.271535357263,9.27378870901005,14.0286136008369));
#108148=CARTESIAN_POINT('Ctrl Pts',(99.3834787687081,10.1674866911426,14.107424873872));
#108149=CARTESIAN_POINT('Ctrl Pts',(99.2455377050953,11.5875812870845,14.1862361469071));
#108150=CARTESIAN_POINT('Ctrl Pts',(97.9831191521371,12.2506383910364,14.2650474199421));
#108151=CARTESIAN_POINT('Ctrl Pts',(96.7348441070681,11.5592725286507,14.3438586929772));
#108152=CARTESIAN_POINT('Ctrl Pts',(96.6315732954504,10.1348341855873,14.4226699660123));
#108153=CARTESIAN_POINT('Ctrl Pts',(97.3834646871194,9.55961294286288,14.4752108147024));
#108154=CARTESIAN_POINT('Ctrl Pts',(97.7984095749683,9.4930631278638,14.5014812390474));
#108155=CARTESIAN_POINT('Ctrl Pts',(98.6846644245394,9.79170480108159,9.1184960127668));
#108156=CARTESIAN_POINT('Ctrl Pts',(99.0010205619527,10.0177288832392,9.14476643711183));
#108157=CARTESIAN_POINT('Ctrl Pts',(99.3870316775812,10.8039329633741,9.19730728580188));
#108158=CARTESIAN_POINT('Ctrl Pts',(98.7148371953222,11.9414877424438,9.27611855883697));
#108159=CARTESIAN_POINT('Ctrl Pts',(97.3959638426784,12.0001663543762,9.35492983187205));
#108160=CARTESIAN_POINT('Ctrl Pts',(96.6231772208986,10.9309391261325,9.43374110490715));
#108161=CARTESIAN_POINT('Ctrl Pts',(97.0937491472135,9.69764252927232,9.51255237794222));
#108162=CARTESIAN_POINT('Ctrl Pts',(98.383005853651,9.41519382008176,9.59136365097731));
#108163=CARTESIAN_POINT('Ctrl Pts',(99.3262558620476,10.3382425252825,9.6701749240124));
#108164=CARTESIAN_POINT('Ctrl Pts',(99.0716056636518,11.6332844720055,9.74898619704748));
#108165=CARTESIAN_POINT('Ctrl Pts',(97.8490218626003,12.130469107685,9.82779747008258));
#108166=CARTESIAN_POINT('Ctrl Pts',(96.7628150217088,11.3807750324401,9.90660874311765));
#108167=CARTESIAN_POINT('Ctrl Pts',(96.7940818134893,10.0613293557532,9.98542001615274));
#108168=CARTESIAN_POINT('Ctrl Pts',(97.9145860709853,9.36392434555335,10.0642312891878));
#108169=CARTESIAN_POINT('Ctrl Pts',(99.1122388935191,9.91847855386342,10.1430425622229));
#108170=CARTESIAN_POINT('Ctrl Pts',(99.3052714847173,11.2240987990573,10.221853835258));
#108171=CARTESIAN_POINT('Ctrl Pts',(98.319328101206,12.101492644125,10.3006651082931));
#108172=CARTESIAN_POINT('Ctrl Pts',(97.0449543333623,11.7581621129394,10.3794763813282));
#108173=CARTESIAN_POINT('Ctrl Pts',(96.6332176798809,10.5042172878713,10.4582876543632));
#108174=CARTESIAN_POINT('Ctrl Pts',(97.45601597308,9.47227374775156,10.5370989273983));
#108175=CARTESIAN_POINT('Ctrl Pts',(98.7701633646951,9.59442593343006,10.6159102004334));
#108176=CARTESIAN_POINT('Ctrl Pts',(99.3886670196609,10.7603409336293,10.6947214734685));
#108177=CARTESIAN_POINT('Ctrl Pts',(98.7528685749049,11.9169155624013,10.7735327465036));
#108178=CARTESIAN_POINT('Ctrl Pts',(97.4370477658578,12.0194832835491,10.8523440195387));
#108179=CARTESIAN_POINT('Ctrl Pts',(96.629708944628,10.9754006382806,10.9311552925738));
#108180=CARTESIAN_POINT('Ctrl Pts',(97.0600742813947,9.72772671601295,11.0099665656089));
#108181=CARTESIAN_POINT('Ctrl Pts',(98.3394198147195,9.4034127530893,11.0887778386439));
#108182=CARTESIAN_POINT('Ctrl Pts',(99.3121871841641,10.2953926774361,11.167589111679));
#108183=CARTESIAN_POINT('Ctrl Pts',(99.0997322410784,11.5979929374135,11.2464003847141));
#108184=CARTESIAN_POINT('Ctrl Pts',(97.8939531704686,12.1346505313534,11.3252116577492));
#108185=CARTESIAN_POINT('Ctrl Pts',(96.7839600289029,11.4206338887223,11.4040229307843));
#108186=CARTESIAN_POINT('Ctrl Pts',(96.772345018156,10.1008726861706,11.4828342038194));
#108187=CARTESIAN_POINT('Ctrl Pts',(97.8695993014189,9.36743040615582,11.5616454768545));
#108188=CARTESIAN_POINT('Ctrl Pts',(99.0846369462246,9.88278277294862,11.6404567498895));
#108189=CARTESIAN_POINT('Ctrl Pts',(99.3199851647595,11.1814419877856,11.7192680229246));
#108190=CARTESIAN_POINT('Ctrl Pts',(98.3630676087894,12.0904047655311,11.7980792959597));
#108191=CARTESIAN_POINT('Ctrl Pts',(97.0782122127977,11.7886579318405,11.8768905689948));
#108192=CARTESIAN_POINT('Ctrl Pts',(96.6259540757604,10.5487518395358,11.9557018420299));
#108193=CARTESIAN_POINT('Ctrl Pts',(97.4147916508613,9.49062149767907,12.034513115065));
#108194=CARTESIAN_POINT('Ctrl Pts',(98.7322138678675,9.57001445953124,12.1133243881001));
#108195=CARTESIAN_POINT('Ctrl Pts',(99.3882699138082,10.7152196834265,12.1921356611351));
#108196=CARTESIAN_POINT('Ctrl Pts',(98.7903825456925,11.8918399430189,12.2709469341702));
#108197=CARTESIAN_POINT('Ctrl Pts',(97.478588625315,12.0371026386346,12.3497582072053));
#108198=CARTESIAN_POINT('Ctrl Pts',(96.6377552529049,11.019800431768,12.4285694802404));
#108199=CARTESIAN_POINT('Ctrl Pts',(97.0273582761178,9.758803197656,12.5073807532755));
#108200=CARTESIAN_POINT('Ctrl Pts',(98.2954919596144,9.39309634609896,12.5861920263106));
#108201=CARTESIAN_POINT('Ctrl Pts',(99.2967249538166,10.2530015917544,12.6650032993457));
#108202=CARTESIAN_POINT('Ctrl Pts',(99.1267017686563,11.561816573295,12.7438145723807));
#108203=CARTESIAN_POINT('Ctrl Pts',(97.9389944505958,12.1373648936305,12.8226258454158));
#108204=CARTESIAN_POINT('Ctrl Pts',(96.8063898962389,11.4597872505569,12.9014371184509));
#108205=CARTESIAN_POINT('Ctrl Pts',(96.7519038758833,10.141100097416,12.980248391486));
#108206=CARTESIAN_POINT('Ctrl Pts',(97.8247504499228,9.37239678178178,13.0590596645211));
#108207=CARTESIAN_POINT('Ctrl Pts',(99.0558897301026,9.8480022865368,13.1378709375562));
#108208=CARTESIAN_POINT('Ctrl Pts',(99.3333052969297,11.1383298048701,13.2166822105913));
#108209=CARTESIAN_POINT('Ctrl Pts',(98.4064237370152,12.0779016595067,13.2954934836263));
#108210=CARTESIAN_POINT('Ctrl Pts',(97.1124433753578,11.8180571339576,13.3743047566614));
#108211=CARTESIAN_POINT('Ctrl Pts',(96.620141042068,10.5934989575161,13.4531160296965));
#108212=CARTESIAN_POINT('Ctrl Pts',(97.3741854288762,9.51029866733518,13.5319273027316));
#108213=CARTESIAN_POINT('Ctrl Pts',(98.6934908176036,9.54684924260553,13.6107385757667));
#108214=CARTESIAN_POINT('Ctrl Pts',(99.3864080892004,10.670134243859,13.6895498488018));
#108215=CARTESIAN_POINT('Ctrl Pts',(98.82706002641,11.8655606324956,13.7683611218369));
#108216=CARTESIAN_POINT('Ctrl Pts',(97.5206840659668,12.0533593482333,13.8471723948719));
#108217=CARTESIAN_POINT('Ctrl Pts',(96.6472315291008,11.06392295392,13.925983667907));
#108218=CARTESIAN_POINT('Ctrl Pts',(96.9956859222381,9.79091081602872,14.0047949409421));
#108219=CARTESIAN_POINT('Ctrl Pts',(98.2512181987561,9.38424363867761,14.0836062139772));
#108220=CARTESIAN_POINT('Ctrl Pts',(99.2799623879387,10.2110722313379,14.1624174870123));
#108221=CARTESIAN_POINT('Ctrl Pts',(99.1523425233119,11.5249107312363,14.2412287600474));
#108222=CARTESIAN_POINT('Ctrl Pts',(97.9843822320735,12.1383557463025,14.3200400330825));
#108223=CARTESIAN_POINT('Ctrl Pts',(96.829507185467,11.4987201261731,14.3988513061175));
#108224=CARTESIAN_POINT('Ctrl Pts',(96.7339634318277,10.1808628924395,14.4776625791526));
#108225=CARTESIAN_POINT('Ctrl Pts',(97.4295958643008,9.64868157380735,14.5302034278427));
#108226=CARTESIAN_POINT('Ctrl Pts',(97.8134932261736,9.58711123239716,14.5564738521877));
#108227=CARTESIAN_POINT('Ctrl Pts',(97.7682422725578,9.30496691879707,14.3914960127668));
#108228=CARTESIAN_POINT('Ctrl Pts',(97.2912023327567,9.38147568097394,14.3652255884217));
#108229=CARTESIAN_POINT('Ctrl Pts',(96.8589976777262,9.71212622642846,14.3389551640767));
#108230=CARTESIAN_POINT('Ctrl Pts',(96.6626828381401,10.1503849261096,14.3126847397317));
#108231=CARTESIAN_POINT('Ctrl Pts',(96.5791521581158,10.3368611358961,14.3015068460244));
#108232=CARTESIAN_POINT('Ctrl Pts',(96.5383280749783,10.542819229865,14.290328952317));
#108233=CARTESIAN_POINT('Ctrl Pts',(96.5389396828847,10.7491495099393,14.2791510586097));
#108234=CARTESIAN_POINT('Origin',(98.,10.75,8.95499601276678));
#108235=CARTESIAN_POINT('',(96.9839745962156,10.75,8.85499601276677));
#108236=CARTESIAN_POINT('Origin',(98.,10.75,8.85499601276678));
#108237=CARTESIAN_POINT('',(97.1339745962156,10.75,9.00499601276677));
#108238=CARTESIAN_POINT('',(97.0839745962156,10.75,8.95499601276678));
#108239=CARTESIAN_POINT('',(97.189703570316,10.6534745854044,9.05499601276678));
#108240=CARTESIAN_POINT('Ctrl Pts',(97.189703570316,10.6534745854044,9.05499601276678));
#108241=CARTESIAN_POINT('Ctrl Pts',(97.1626673723677,10.7003026538944,9.03368878891887));
#108242=CARTESIAN_POINT('Ctrl Pts',(97.1339745962156,10.75,9.00499601276677));
#108243=CARTESIAN_POINT('',(97.5112583240073,10.0965254145956,9.05499601276678));
#108244=CARTESIAN_POINT('Origin',(98.,10.75,9.05499601276678));
#108245=CARTESIAN_POINT('',(97.5669872981078,10.,9.00499601276675));
#108246=CARTESIAN_POINT('Ctrl Pts',(97.5669872981078,10.,9.00499601276675));
#108247=CARTESIAN_POINT('Ctrl Pts',(97.5382945219557,10.0496973461057,9.03368878891888));
#108248=CARTESIAN_POINT('Ctrl Pts',(97.5112583240073,10.0965254145956,9.05499601276678));
#108249=CARTESIAN_POINT('',(97.6784452463086,10.,9.05499601276678));
#108250=CARTESIAN_POINT('Ctrl Pts',(97.6784452463086,10.,9.05499601276678));
#108251=CARTESIAN_POINT('Ctrl Pts',(97.624372850412,10.,9.03368878891888));
#108252=CARTESIAN_POINT('Ctrl Pts',(97.5669872981078,10.,9.00499601276675));
#108253=CARTESIAN_POINT('',(98.3215547536914,10.,9.05499601276678));
#108254=CARTESIAN_POINT('Origin',(98.,10.75,9.05499601276678));
#108255=CARTESIAN_POINT('',(98.4330127018922,10.,9.00499601276676));
#108256=CARTESIAN_POINT('Ctrl Pts',(98.4330127018922,10.,9.00499601276676));
#108257=CARTESIAN_POINT('Ctrl Pts',(98.375627149588,10.,9.03368878891888));
#108258=CARTESIAN_POINT('Ctrl Pts',(98.3215547536914,10.,9.05499601276678));
#108259=CARTESIAN_POINT('',(98.4887416759926,10.0965254145956,9.05499601276678));
#108260=CARTESIAN_POINT('Ctrl Pts',(98.4887416759927,10.0965254145956,9.05499601276678));
#108261=CARTESIAN_POINT('Ctrl Pts',(98.4617054780443,10.0496973461056,9.03368878891889));
#108262=CARTESIAN_POINT('Ctrl Pts',(98.4330127018922,10.,9.00499601276676));
#108263=CARTESIAN_POINT('',(98.810296429684,10.6534745854044,9.05499601276678));
#108264=CARTESIAN_POINT('Origin',(98.,10.75,9.05499601276678));
#108265=CARTESIAN_POINT('',(98.8660254037844,10.75,9.00499601276677));
#108266=CARTESIAN_POINT('Ctrl Pts',(98.8660254037844,10.75,9.00499601276677));
#108267=CARTESIAN_POINT('Ctrl Pts',(98.8373326276323,10.7003026538944,9.03368878891888));
#108268=CARTESIAN_POINT('Ctrl Pts',(98.810296429684,10.6534745854044,9.05499601276678));
#108269=CARTESIAN_POINT('',(98.810296429684,10.8465254145956,9.05499601276678));
#108270=CARTESIAN_POINT('Ctrl Pts',(98.810296429684,10.8465254145956,9.05499601276678));
#108271=CARTESIAN_POINT('Ctrl Pts',(98.8373326276323,10.7996973461057,9.03368878891894));
#108272=CARTESIAN_POINT('Ctrl Pts',(98.8660254037844,10.75,9.00499601276677));
#108273=CARTESIAN_POINT('',(98.4887416759926,11.4034745854044,9.05499601276678));
#108274=CARTESIAN_POINT('Origin',(98.,10.75,9.05499601276678));
#108275=CARTESIAN_POINT('',(98.4330127018922,11.5,9.00499601276676));
#108276=CARTESIAN_POINT('Ctrl Pts',(98.4330127018922,11.5,9.00499601276676));
#108277=CARTESIAN_POINT('Ctrl Pts',(98.4617054780443,11.4503026538943,9.03368878891891));
#108278=CARTESIAN_POINT('Ctrl Pts',(98.4887416759926,11.4034745854044,9.05499601276678));
#108279=CARTESIAN_POINT('',(98.3215547536914,11.5,9.05499601276678));
#108280=CARTESIAN_POINT('Ctrl Pts',(98.3215547536914,11.5,9.05499601276678));
#108281=CARTESIAN_POINT('Ctrl Pts',(98.375627149588,11.5,9.03368878891889));
#108282=CARTESIAN_POINT('Ctrl Pts',(98.4330127018922,11.5,9.00499601276676));
#108283=CARTESIAN_POINT('',(97.6784452463086,11.5,9.05499601276678));
#108284=CARTESIAN_POINT('Origin',(98.,10.75,9.05499601276678));
#108285=CARTESIAN_POINT('',(97.5669872981078,11.5,9.00499601276675));
#108286=CARTESIAN_POINT('Ctrl Pts',(97.5669872981078,11.5,9.00499601276675));
#108287=CARTESIAN_POINT('Ctrl Pts',(97.624372850412,11.5,9.03368878891888));
#108288=CARTESIAN_POINT('Ctrl Pts',(97.6784452463086,11.5,9.05499601276678));
#108289=CARTESIAN_POINT('',(97.5112583240073,11.4034745854044,9.05499601276678));
#108290=CARTESIAN_POINT('Ctrl Pts',(97.5112583240073,11.4034745854043,9.05499601276678));
#108291=CARTESIAN_POINT('Ctrl Pts',(97.5382945219557,11.4503026538943,9.03368878891889));
#108292=CARTESIAN_POINT('Ctrl Pts',(97.5669872981078,11.5,9.00499601276675));
#108293=CARTESIAN_POINT('',(97.189703570316,10.8465254145956,9.05499601276678));
#108294=CARTESIAN_POINT('Origin',(98.,10.75,9.05499601276678));
#108295=CARTESIAN_POINT('Ctrl Pts',(97.1339745962156,10.75,9.00499601276677));
#108296=CARTESIAN_POINT('Ctrl Pts',(97.1626673723677,10.7996973461056,9.03368878891887));
#108297=CARTESIAN_POINT('Ctrl Pts',(97.189703570316,10.8465254145956,9.05499601276678));
#108298=CARTESIAN_POINT('Origin',(98.,10.75,8.95499601276678));
#108299=CARTESIAN_POINT('',(98.810296429684,10.6534745854044,8.85499601276678));
#108300=CARTESIAN_POINT('',(98.810296429684,10.6534745854044,8.95499601276678));
#108301=CARTESIAN_POINT('',(98.4887416759926,10.0965254145956,8.85499601276678));
#108302=CARTESIAN_POINT('',(98.4887416759926,10.0965254145956,8.95499601276678));
#108303=CARTESIAN_POINT('Origin',(98.,10.75,8.85499601276678));
#108304=CARTESIAN_POINT('Origin',(98.,10.75,8.95499601276678));
#108305=CARTESIAN_POINT('',(98.4887416759926,11.4034745854044,8.85499601276678));
#108306=CARTESIAN_POINT('',(98.4887416759926,11.4034745854044,8.95499601276678));
#108307=CARTESIAN_POINT('',(98.810296429684,10.8465254145956,8.85499601276678));
#108308=CARTESIAN_POINT('',(98.810296429684,10.8465254145956,8.95499601276678));
#108309=CARTESIAN_POINT('Origin',(98.,10.75,8.85499601276678));
#108310=CARTESIAN_POINT('Origin',(98.,10.75,8.95499601276678));
#108311=CARTESIAN_POINT('',(97.6784452463086,10.,8.85499601276678));
#108312=CARTESIAN_POINT('',(97.6784452463086,10.,8.95499601276678));
#108313=CARTESIAN_POINT('',(98.3215547536914,10.,8.85499601276678));
#108314=CARTESIAN_POINT('Origin',(98.,10.75,8.85499601276678));
#108315=CARTESIAN_POINT('',(98.3215547536914,10.,8.95499601276678));
#108316=CARTESIAN_POINT('Origin',(98.,10.75,8.95499601276678));
#108317=CARTESIAN_POINT('',(97.6784452463086,11.5,8.85499601276678));
#108318=CARTESIAN_POINT('',(97.6784452463086,11.5,8.95499601276678));
#108319=CARTESIAN_POINT('',(98.3215547536914,11.5,8.85499601276678));
#108320=CARTESIAN_POINT('',(98.3215547536914,11.5,8.95499601276678));
#108321=CARTESIAN_POINT('Origin',(98.,10.75,8.85499601276678));
#108322=CARTESIAN_POINT('Origin',(98.,10.75,8.95499601276678));
#108323=CARTESIAN_POINT('',(97.189703570316,10.6534745854044,8.85499601276678));
#108324=CARTESIAN_POINT('',(97.189703570316,10.6534745854044,8.95499601276678));
#108325=CARTESIAN_POINT('',(97.5112583240073,10.0965254145956,8.85499601276678));
#108326=CARTESIAN_POINT('Origin',(98.,10.75,8.85499601276678));
#108327=CARTESIAN_POINT('',(97.5112583240073,10.0965254145956,8.95499601276678));
#108328=CARTESIAN_POINT('Origin',(98.,10.75,8.95499601276678));
#108329=CARTESIAN_POINT('',(97.5112583240073,11.4034745854044,8.85499601276678));
#108330=CARTESIAN_POINT('',(97.5112583240073,11.4034745854044,8.95499601276678));
#108331=CARTESIAN_POINT('',(97.189703570316,10.8465254145956,8.85499601276678));
#108332=CARTESIAN_POINT('Origin',(98.,10.75,8.85499601276678));
#108333=CARTESIAN_POINT('',(97.189703570316,10.8465254145956,8.95499601276678));
#108334=CARTESIAN_POINT('Origin',(98.4330127018922,11.5,8.854996));
#108335=CARTESIAN_POINT('',(98.8165063509461,11.5,8.85499601276678));
#108336=CARTESIAN_POINT('',(98.4330127018922,11.5,10.354996));
#108337=CARTESIAN_POINT('',(98.4330127018922,11.5,8.854996));
#108338=CARTESIAN_POINT('',(97.5669872981078,11.5,10.354996));
#108339=CARTESIAN_POINT('',(98.4330127018922,11.5,10.354996));
#108340=CARTESIAN_POINT('',(97.5669872981078,11.5,8.854996));
#108341=CARTESIAN_POINT('Origin',(98.8660254037844,10.75,8.854996));
#108342=CARTESIAN_POINT('',(98.9077722283114,10.6776923788647,8.85499601276678));
#108343=CARTESIAN_POINT('',(98.8660254037844,10.75,10.354996));
#108344=CARTESIAN_POINT('',(98.8660254037844,10.75,8.854996));
#108345=CARTESIAN_POINT('',(98.8660254037844,10.75,10.354996));
#108346=CARTESIAN_POINT('Origin',(98.4330127018922,10.,8.854996));
#108347=CARTESIAN_POINT('',(98.6912658773653,10.4473076211353,8.85499601276678));
#108348=CARTESIAN_POINT('',(98.4330127018922,10.,10.354996));
#108349=CARTESIAN_POINT('',(98.4330127018922,10.,8.854996));
#108350=CARTESIAN_POINT('',(98.4330127018922,10.,10.354996));
#108351=CARTESIAN_POINT('Origin',(99.2,10.75,8.85499601276678));
#108352=CARTESIAN_POINT('Origin',(99.2,10.75,8.85499601276678));
#108353=CARTESIAN_POINT('Origin',(99.2,10.75,8.85499601276678));
#108354=CARTESIAN_POINT('',(98.3834936490539,10.,8.85499601276678));
#108355=CARTESIAN_POINT('Origin',(99.2,10.75,8.85499601276678));
#108356=CARTESIAN_POINT('Origin',(99.2,10.75,8.85499601276678));
#108357=CARTESIAN_POINT('',(97.3922277716886,10.3026923788647,8.85499601276678));
#108358=CARTESIAN_POINT('Origin',(99.2,10.75,8.85499601276678));
#108359=CARTESIAN_POINT('',(97.6087341226347,11.5723076211353,8.85499601276678));
#108360=CARTESIAN_POINT('Origin',(98.8660254037844,10.75,10.3549960127668));
#108361=CARTESIAN_POINT('',(97.5669872981078,10.,10.354996));
#108362=CARTESIAN_POINT('',(97.5669872981078,10.,10.354996));
#108363=CARTESIAN_POINT('Origin',(98.,10.75,10.3549960127668));
#108364=CARTESIAN_POINT('Origin',(98.8660254037844,10.75,10.3549960127668));
#108365=CARTESIAN_POINT('Origin',(98.,10.75,10.3549960127668));
#108366=CARTESIAN_POINT('Origin',(98.8660254037844,10.75,10.3549960127668));
#108367=CARTESIAN_POINT('Origin',(98.,10.75,10.3549960127668));
#108368=CARTESIAN_POINT('Origin',(98.8660254037844,10.75,10.3549960127668));
#108369=CARTESIAN_POINT('Origin',(98.,10.75,10.3549960127668));
#108370=CARTESIAN_POINT('Origin',(98.8660254037844,10.75,10.3549960127668));
#108371=CARTESIAN_POINT('',(97.1339745962156,10.75,10.354996));
#108372=CARTESIAN_POINT('',(97.5669872981078,11.5,10.354996));
#108373=CARTESIAN_POINT('Origin',(98.,10.75,10.3549960127668));
#108374=CARTESIAN_POINT('Origin',(98.8660254037844,10.75,10.3549960127668));
#108375=CARTESIAN_POINT('',(97.1339745962156,10.75,10.354996));
#108376=CARTESIAN_POINT('Origin',(98.,10.75,10.3549960127668));
#108377=CARTESIAN_POINT('Origin',(98.,10.75,10.3549960127668));
#108378=CARTESIAN_POINT('',(98.,10.75,10.8753565729783));
#108379=CARTESIAN_POINT('',(97.1339745962156,10.75,10.3549960127668));
#108380=CARTESIAN_POINT('Origin',(97.5669872981078,10.,8.854996));
#108381=CARTESIAN_POINT('',(97.5669872981078,10.,8.854996));
#108382=CARTESIAN_POINT('Origin',(97.1339745962156,10.75,8.854996));
#108383=CARTESIAN_POINT('',(97.1339745962156,10.75,8.854996));
#108384=CARTESIAN_POINT('Origin',(97.5669872981078,11.5,8.854996));
#108385=CARTESIAN_POINT('Origin',(99.2,10.75,8.85499601276678));
#108386=CARTESIAN_POINT('',(96.8,10.75,8.85499601276678));
#108387=CARTESIAN_POINT('Origin',(98.,10.75,8.85499601276678));
#108388=CARTESIAN_POINT('Origin',(98.,10.75,9.00499601276678));
#108389=CARTESIAN_POINT('',(96.65,10.75,9.00499601276678));
#108390=CARTESIAN_POINT('Origin',(98.,10.75,11.7549960127668));
#108391=CARTESIAN_POINT('Origin',(98.,10.75,14.3914960127668));
#108392=CARTESIAN_POINT('Origin',(98.,10.75,14.6049960127668));
#108393=CARTESIAN_POINT('',(97.,10.75,14.8549960127668));
#108394=CARTESIAN_POINT('Origin',(98.,10.75,14.8549960127668));
#108395=CARTESIAN_POINT('',(96.75,10.75,14.6049960127668));
#108396=CARTESIAN_POINT('Origin',(98.,10.75,14.8549960127668));
#108397=CARTESIAN_POINT('',(0.,0.,0.));
#108398=CARTESIAN_POINT('Origin',(110.,24.53,42.));
#108399=CARTESIAN_POINT('',(109.032306318989,25.5642640831103,42.0006908675261));
#108400=CARTESIAN_POINT('',(109.032548003746,25.6222359168897,42.0006735849849));
#108401=CARTESIAN_POINT('',(109.03325,24.53,42.));
#108402=CARTESIAN_POINT('',(110.425646355462,25.69325,42.8688267550426));
#108403=CARTESIAN_POINT('Ctrl Pts',(109.032306318989,25.5642640831103,42.0006908675261));
#108404=CARTESIAN_POINT('Ctrl Pts',(109.031974852187,25.5670559984264,42.0429741926217));
#108405=CARTESIAN_POINT('Ctrl Pts',(109.034508923572,25.5698479137424,42.0852164196326));
#108406=CARTESIAN_POINT('Ctrl Pts',(109.040044285781,25.5726398290584,42.1270598791021));
#108407=CARTESIAN_POINT('Ctrl Pts',(109.081696521971,25.5936483036209,42.4419215974445));
#108408=CARTESIAN_POINT('Ctrl Pts',(109.293287593117,25.6146567781833,42.7342043338243));
#108409=CARTESIAN_POINT('Ctrl Pts',(109.579443943085,25.6356652527458,42.8722111754205));
#108410=CARTESIAN_POINT('Ctrl Pts',(109.84089781557,25.6548601684972,42.9983045616719));
#108411=CARTESIAN_POINT('Ctrl Pts',(110.164598917808,25.6740550842486,42.9956081516571));
#108412=CARTESIAN_POINT('Ctrl Pts',(110.426173582409,25.69325,42.8693912864047));
#108413=CARTESIAN_POINT('',(109.574880871485,25.69325,42.8682622236805));
#108414=CARTESIAN_POINT('Origin',(110.,25.69325,42.));
#108415=CARTESIAN_POINT('Ctrl Pts',(109.574880871485,25.69325,42.8682622236805));
#108416=CARTESIAN_POINT('Ctrl Pts',(109.288354036607,25.6722415254375,42.7279727638635));
#108417=CARTESIAN_POINT('Ctrl Pts',(109.079161047597,25.6512330508751,42.4357219166886));
#108418=CARTESIAN_POINT('Ctrl Pts',(109.039553457205,25.6302245763126,42.1210844078894));
#108419=CARTESIAN_POINT('Ctrl Pts',(109.034533077624,25.6275616898383,42.0812031702488));
#108420=CARTESIAN_POINT('Ctrl Pts',(109.032237310398,25.624898803364,42.0409622614609));
#108421=CARTESIAN_POINT('Ctrl Pts',(109.032548003746,25.6222359168897,42.0006735849849));
#108422=CARTESIAN_POINT('Origin',(110.,24.53,42.));
#108423=CARTESIAN_POINT('',(109.034715906394,25.1642640831103,42.0001041586162));
#108424=CARTESIAN_POINT('',(109.034710481353,25.2222359168897,42.0001372498462));
#108425=CARTESIAN_POINT('',(109.03325,24.53,42.));
#108426=CARTESIAN_POINT('Ctrl Pts',(109.034715906394,25.1642640831103,42.0001041586162));
#108427=CARTESIAN_POINT('Ctrl Pts',(109.034566524345,25.1743384843849,42.1536664781764));
#108428=CARTESIAN_POINT('Ctrl Pts',(109.069123406379,25.1844128856595,42.3071651928001));
#108429=CARTESIAN_POINT('Ctrl Pts',(109.138750317064,25.1944872869341,42.4426393893168));
#108430=CARTESIAN_POINT('Ctrl Pts',(109.283945564119,25.2154957614966,42.7251481095688));
#108431=CARTESIAN_POINT('Ctrl Pts',(109.581646719205,25.236504236059,42.9292752143365));
#108432=CARTESIAN_POINT('Ctrl Pts',(109.897499355924,25.2575127106215,42.962898308317));
#108433=CARTESIAN_POINT('Ctrl Pts',(110.213351992642,25.278521185184,42.9965214022976));
#108434=CARTESIAN_POINT('Ctrl Pts',(110.547356110992,25.2995296597464,42.8596404854909));
#108435=CARTESIAN_POINT('Ctrl Pts',(110.748769062449,25.3205381343089,42.614026335183));
#108436=CARTESIAN_POINT('Ctrl Pts',(110.950182013906,25.3415466088713,42.3684121848753));
#108437=CARTESIAN_POINT('Ctrl Pts',(111.019003798469,25.3625550834338,42.0140648010663));
#108438=CARTESIAN_POINT('Ctrl Pts',(110.924180524676,25.3835635579963,41.7109157798489));
#108439=CARTESIAN_POINT('Ctrl Pts',(110.829357250883,25.4045720325587,41.4077667586315));
#108440=CARTESIAN_POINT('Ctrl Pts',(110.570888918734,25.4255805071212,41.1558161000056));
#108441=CARTESIAN_POINT('Ctrl Pts',(110.265412196082,25.4465889816837,41.068749323821));
#108442=CARTESIAN_POINT('Ctrl Pts',(109.959935473431,25.4675974562461,40.9816825476364));
#108443=CARTESIAN_POINT('Ctrl Pts',(109.607450360277,25.4886059308086,41.0594996538931));
#108444=CARTESIAN_POINT('Ctrl Pts',(109.367064504317,25.509614405371,41.2671285571739));
#108445=CARTESIAN_POINT('Ctrl Pts',(109.15862465905,25.5278309646175,41.4471646757718));
#108446=CARTESIAN_POINT('Ctrl Pts',(109.034469058168,25.5460475238639,41.7248025938681));
#108447=CARTESIAN_POINT('Ctrl Pts',(109.032306318989,25.5642640831103,42.0006908675261));
#108448=CARTESIAN_POINT('Ctrl Pts',(109.032548003746,25.6222359168897,42.0006735849849));
#108449=CARTESIAN_POINT('Ctrl Pts',(109.034688482602,25.6038903288015,41.7231103203184));
#108450=CARTESIAN_POINT('Ctrl Pts',(109.160540193731,25.5855447407134,41.4432798433115));
#108451=CARTESIAN_POINT('Ctrl Pts',(109.371468464982,25.5671991526252,41.2631720502119));
#108452=CARTESIAN_POINT('Ctrl Pts',(109.613013254922,25.5461906780628,41.056921371757));
#108453=CARTESIAN_POINT('Ctrl Pts',(109.966125026575,25.5251822035003,40.9814441852706));
#108454=CARTESIAN_POINT('Ctrl Pts',(110.271108162041,25.5041737289379,41.0704195389749));
#108455=CARTESIAN_POINT('Ctrl Pts',(110.576091297507,25.4831652543754,41.1593948926792));
#108456=CARTESIAN_POINT('Ctrl Pts',(110.832945796785,25.462156779813,41.412822786574));
#108457=CARTESIAN_POINT('Ctrl Pts',(110.925903746015,25.4411483052505,41.7165193527544));
#108458=CARTESIAN_POINT('Ctrl Pts',(111.018861695245,25.420139830688,42.0202159189348));
#108459=CARTESIAN_POINT('Ctrl Pts',(110.947923094426,25.3991313561256,42.3741811574008));
#108460=CARTESIAN_POINT('Ctrl Pts',(110.745030040548,25.3781228815631,42.6185773842525));
#108461=CARTESIAN_POINT('Ctrl Pts',(110.542136986669,25.3571144070006,42.8629736111042));
#108462=CARTESIAN_POINT('Ctrl Pts',(110.207289479731,25.3361059324382,42.9978008263417));
#108463=CARTESIAN_POINT('Ctrl Pts',(109.891642598199,25.3150974578757,42.9622525435628));
#108464=CARTESIAN_POINT('Ctrl Pts',(109.575995716666,25.2940889833133,42.926704260784));
#108465=CARTESIAN_POINT('Ctrl Pts',(109.27954946054,25.2730805087508,42.7207804799889));
#108466=CARTESIAN_POINT('Ctrl Pts',(109.136076806743,25.2520720341883,42.4373967098996));
#108467=CARTESIAN_POINT('Ctrl Pts',(109.068157121679,25.2421266617554,42.3032433649439));
#108468=CARTESIAN_POINT('Ctrl Pts',(109.034519705577,25.2321812893226,42.1517307884195));
#108469=CARTESIAN_POINT('Ctrl Pts',(109.034710481353,25.2222359168897,42.0001372498462));
#108470=CARTESIAN_POINT('Origin',(110.,24.53,42.));
#108471=CARTESIAN_POINT('',(109.032641470368,24.7642640831103,41.9992259658271));
#108472=CARTESIAN_POINT('',(109.032697715776,24.8222359168897,41.9992128726693));
#108473=CARTESIAN_POINT('',(109.03325,24.53,42.));
#108474=CARTESIAN_POINT('Ctrl Pts',(109.032641470368,24.7642640831103,41.9992259658271));
#108475=CARTESIAN_POINT('Ctrl Pts',(109.03493584802,24.7816209703435,42.2623534561074));
#108476=CARTESIAN_POINT('Ctrl Pts',(109.146410049054,24.7989778575767,42.5271931796135));
#108477=CARTESIAN_POINT('Ctrl Pts',(109.337910161716,24.8163347448098,42.7066241744067));
#108478=CARTESIAN_POINT('Ctrl Pts',(109.569698568907,24.8373432193723,42.9238043311475));
#108479=CARTESIAN_POINT('Ctrl Pts',(109.918727023337,24.8583516939348,43.0158584732588));
#108480=CARTESIAN_POINT('Ctrl Pts',(110.227475156868,24.8793601684972,42.9412415806255));
#108481=CARTESIAN_POINT('Ctrl Pts',(110.5362232904,24.9003686430597,42.8666246879923));
#108482=CARTESIAN_POINT('Ctrl Pts',(110.804691103032,24.9213771176221,42.6253367606144));
#108483=CARTESIAN_POINT('Ctrl Pts',(110.911716082052,24.9423855921846,42.3262736383281));
#108484=CARTESIAN_POINT('Ctrl Pts',(111.018741061072,24.963394066747,42.0272105160418));
#108485=CARTESIAN_POINT('Ctrl Pts',(110.964323206479,24.9844025413095,41.6703721988471));
#108486=CARTESIAN_POINT('Ctrl Pts',(110.773021965262,25.005411015872,41.4168038702247));
#108487=CARTESIAN_POINT('Ctrl Pts',(110.581720724044,25.0264194904344,41.1632355416022));
#108488=CARTESIAN_POINT('Ctrl Pts',(110.253536096201,25.0474279649969,41.012937201552));
#108489=CARTESIAN_POINT('Ctrl Pts',(109.936581269547,25.0684364395594,41.033739887542));
#108490=CARTESIAN_POINT('Ctrl Pts',(109.619626442893,25.0894449141218,41.054542573532));
#108491=CARTESIAN_POINT('Ctrl Pts',(109.313901417428,25.1104533886843,41.2464462855623));
#108492=CARTESIAN_POINT('Ctrl Pts',(109.157383574207,25.1314618632467,41.5228433094456));
#108493=CARTESIAN_POINT('Ctrl Pts',(109.075922278026,25.1423959365346,41.6666969389274));
#108494=CARTESIAN_POINT('Ctrl Pts',(109.03487803556,25.1533300098225,41.8334380103697));
#108495=CARTESIAN_POINT('Ctrl Pts',(109.034715906394,25.1642640831103,42.0001041586162));
#108496=CARTESIAN_POINT('Ctrl Pts',(109.034710481353,25.2222359168897,42.0001372498462));
#108497=CARTESIAN_POINT('Ctrl Pts',(109.03492269783,25.2111728147601,41.8315065815894));
#108498=CARTESIAN_POINT('Ctrl Pts',(109.076994075968,25.2001097126305,41.6627757305176));
#108499=CARTESIAN_POINT('Ctrl Pts',(109.160299591046,25.1890466105009,41.5177277634241));
#108500=CARTESIAN_POINT('Ctrl Pts',(109.318494080615,25.1680381359385,41.2422863464211));
#108501=CARTESIAN_POINT('Ctrl Pts',(109.62538211122,25.147029661376,41.0522472717984));
#108502=CARTESIAN_POINT('Ctrl Pts',(109.942458023974,25.1260211868136,41.0333727242458));
#108503=CARTESIAN_POINT('Ctrl Pts',(110.259533936729,25.1050127122511,41.0144981766932));
#108504=CARTESIAN_POINT('Ctrl Pts',(110.586797731632,25.0840042376886,41.1667881562108));
#108505=CARTESIAN_POINT('Ctrl Pts',(110.776553416921,25.0629957631262,41.4215146740517));
#108506=CARTESIAN_POINT('Ctrl Pts',(110.966309102209,25.0419872885637,41.6762411918927));
#108507=CARTESIAN_POINT('Ctrl Pts',(111.018556677882,25.0209788140013,42.033404248057));
#108508=CARTESIAN_POINT('Ctrl Pts',(110.909715401718,24.9999703394388,42.3318112002329));
#108509=CARTESIAN_POINT('Ctrl Pts',(110.800874125554,24.9789618648763,42.6302181524088));
#108510=CARTESIAN_POINT('Ctrl Pts',(110.530943997553,24.9579533903139,42.8698690005962));
#108511=CARTESIAN_POINT('Ctrl Pts',(110.221747852986,24.9369449157514,42.9426071642036));
#108512=CARTESIAN_POINT('Ctrl Pts',(109.912551708419,24.915936441189,43.015345327811));
#108513=CARTESIAN_POINT('Ctrl Pts',(109.564089547287,24.8949279666265,42.9211708068382));
#108514=CARTESIAN_POINT('Ctrl Pts',(109.33362599082,24.873919492064,42.7025853689385));
#108515=CARTESIAN_POINT('Ctrl Pts',(109.144635900016,24.8566916336726,42.523335849447));
#108516=CARTESIAN_POINT('Ctrl Pts',(109.034996446688,24.8394637752811,42.2604235985598));
#108517=CARTESIAN_POINT('Ctrl Pts',(109.032697715776,24.8222359168897,41.9992128726693));
#108518=CARTESIAN_POINT('Origin',(110.,24.53,42.));
#108519=CARTESIAN_POINT('',(109.032632519022,24.3642640831103,42.0007718204176));
#108520=CARTESIAN_POINT('',(109.032577150836,24.4222359168897,42.0007573162032));
#108521=CARTESIAN_POINT('',(109.03325,24.53,42.));
#108522=CARTESIAN_POINT('Ctrl Pts',(109.032632519022,24.3642640831103,42.0007718204176));
#108523=CARTESIAN_POINT('Ctrl Pts',(109.032153349384,24.3678949817396,42.0558143102464));
#108524=CARTESIAN_POINT('Ctrl Pts',(109.03645356453,24.3715258803689,42.1107819869543));
#108525=CARTESIAN_POINT('Ctrl Pts',(109.045800826623,24.3751567789982,42.1648775768284));
#108526=CARTESIAN_POINT('Ctrl Pts',(109.099884329895,24.3961652535606,42.477876076607));
#108527=CARTESIAN_POINT('Ctrl Pts',(109.322933370855,24.4171737281231,42.7616787669617));
#108528=CARTESIAN_POINT('Ctrl Pts',(109.61428345485,24.4381822026855,42.8882023557283));
#108529=CARTESIAN_POINT('Ctrl Pts',(109.905633538845,24.459190677248,43.0147259444948));
#108530=CARTESIAN_POINT('Ctrl Pts',(110.265284665876,24.4801991518105,42.9839704316732));
#108531=CARTESIAN_POINT('Ctrl Pts',(110.530922326302,24.5012076263729,42.8098161254884));
#108532=CARTESIAN_POINT('Ctrl Pts',(110.796559986728,24.5222161009354,42.6356618193037));
#108533=CARTESIAN_POINT('Ctrl Pts',(110.968184180549,24.5432245754978,42.3181087197559));
#108534=CARTESIAN_POINT('Ctrl Pts',(110.968339017755,24.5642330500603,42.000472032944));
#108535=CARTESIAN_POINT('Ctrl Pts',(110.96849385496,24.5852415246228,41.6828353461321));
#108536=CARTESIAN_POINT('Ctrl Pts',(110.79717933555,24.6062499991852,41.3651150720561));
#108537=CARTESIAN_POINT('Ctrl Pts',(110.531711589679,24.6272584737477,41.1907018710498));
#108538=CARTESIAN_POINT('Ctrl Pts',(110.266243843807,24.6482669483101,41.0162886700435));
#108539=CARTESIAN_POINT('Ctrl Pts',(109.906622871474,24.6692754228726,40.9851825421069));
#108540=CARTESIAN_POINT('Ctrl Pts',(109.615149574554,24.6902838974351,41.1114220215978));
#108541=CARTESIAN_POINT('Ctrl Pts',(109.323676277635,24.7112923719975,41.2376615010887));
#108542=CARTESIAN_POINT('Ctrl Pts',(109.100350656129,24.73230084656,41.5212465880071));
#108543=CARTESIAN_POINT('Ctrl Pts',(109.045962025352,24.7533093211224,41.8341922171514));
#108544=CARTESIAN_POINT('Ctrl Pts',(109.036508467246,24.7569609084517,41.8885868515997));
#108545=CARTESIAN_POINT('Ctrl Pts',(109.032158773197,24.760612495781,41.9438685162689));
#108546=CARTESIAN_POINT('Ctrl Pts',(109.032641470368,24.7642640831103,41.9992259658271));
#108547=CARTESIAN_POINT('Ctrl Pts',(109.032697715776,24.8222359168897,41.9992128726693));
#108548=CARTESIAN_POINT('Ctrl Pts',(109.032193264262,24.8184553007187,41.9418907452229));
#108549=CARTESIAN_POINT('Ctrl Pts',(109.036858057582,24.8146746845477,41.8846505587128));
#108550=CARTESIAN_POINT('Ctrl Pts',(109.046987895688,24.8108940683766,41.8283944448405));
#108551=CARTESIAN_POINT('Ctrl Pts',(109.103278308826,24.7898855938142,41.5157853134692));
#108552=CARTESIAN_POINT('Ctrl Pts',(109.328324086905,24.7688771192517,41.2335634055532));
#108553=CARTESIAN_POINT('Ctrl Pts',(109.620559550287,24.7478686446893,41.109098523204));
#108554=CARTESIAN_POINT('Ctrl Pts',(109.91279501367,24.7268601701268,40.9846336408548));
#108555=CARTESIAN_POINT('Ctrl Pts',(110.272220162357,24.7058516955644,41.0179257840723));
#108556=CARTESIAN_POINT('Ctrl Pts',(110.536622489988,24.6848432210019,41.1939498668055));
#108557=CARTESIAN_POINT('Ctrl Pts',(110.80102481762,24.6638347464394,41.3699739495386));
#108558=CARTESIAN_POINT('Ctrl Pts',(110.970404324194,24.642826271877,41.6887299717873));
#108559=CARTESIAN_POINT('Ctrl Pts',(110.968318164027,24.6218177973145,42.0063598196718));
#108560=CARTESIAN_POINT('Ctrl Pts',(110.966232003859,24.600809322752,42.3239896675563));
#108561=CARTESIAN_POINT('Ctrl Pts',(110.792680176949,24.5798008481896,42.6404933410765));
#108562=CARTESIAN_POINT('Ctrl Pts',(110.525988538177,24.5587923736271,42.8130292538006));
#108563=CARTESIAN_POINT('Ctrl Pts',(110.259296899404,24.5377838990647,42.9855651665247));
#108564=CARTESIAN_POINT('Ctrl Pts',(109.89946544877,24.5167754245022,43.0141333184527));
#108565=CARTESIAN_POINT('Ctrl Pts',(109.608890078749,24.4957669499397,42.8858405848606));
#108566=CARTESIAN_POINT('Ctrl Pts',(109.318314708729,24.4747584753773,42.7575478512684));
#108567=CARTESIAN_POINT('Ctrl Pts',(109.096995419324,24.4537500008148,42.4723942321562));
#108568=CARTESIAN_POINT('Ctrl Pts',(109.044816044342,24.4327415262524,42.1590726976564));
#108569=CARTESIAN_POINT('Ctrl Pts',(109.036118345885,24.4292396564648,42.1068456208073));
#108570=CARTESIAN_POINT('Ctrl Pts',(109.032120205872,24.4257377866772,42.0538358974429));
#108571=CARTESIAN_POINT('Ctrl Pts',(109.032577150836,24.4222359168897,42.0007573162032));
#108572=CARTESIAN_POINT('Origin',(110.,24.53,42.));
#108573=CARTESIAN_POINT('',(109.034717052885,23.9642640831103,41.9999017201984));
#108574=CARTESIAN_POINT('',(109.034721981614,24.0222359168897,41.9999322711442));
#108575=CARTESIAN_POINT('',(109.03325,24.53,42.));
#108576=CARTESIAN_POINT('Ctrl Pts',(109.034717052885,23.9642640831103,41.9999017201984));
#108577=CARTESIAN_POINT('Ctrl Pts',(109.034871038885,23.9751774676982,42.1662525240113));
#108578=CARTESIAN_POINT('Ctrl Pts',(109.075751609479,23.986090852286,42.3326741490512));
#108579=CARTESIAN_POINT('Ctrl Pts',(109.156918704901,23.9970042368738,42.4763345202534));
#108580=CARTESIAN_POINT('Ctrl Pts',(109.313166919719,24.0180127114363,42.7528834890671));
#108581=CARTESIAN_POINT('Ctrl Pts',(109.618704861746,24.0390211859988,42.9450861065659));
#108582=CARTESIAN_POINT('Ctrl Pts',(109.935639297263,24.0600296605612,42.9661980378269));
#108583=CARTESIAN_POINT('Ctrl Pts',(110.25257373278,24.0810381351237,42.987309969088));
#108584=CARTESIAN_POINT('Ctrl Pts',(110.580904661786,24.1020466096862,42.8373312141113));
#108585=CARTESIAN_POINT('Ctrl Pts',(110.772453004619,24.1230550842486,42.5839493950286));
#108586=CARTESIAN_POINT('Ctrl Pts',(110.964001347452,24.1440635588111,42.330567575946));
#108587=CARTESIAN_POINT('Ctrl Pts',(111.018767104112,24.1650720333735,41.9737826927573));
#108588=CARTESIAN_POINT('Ctrl Pts',(110.912033751289,24.186080507936,41.6746154258864));
#108589=CARTESIAN_POINT('Ctrl Pts',(110.805300398467,24.2070889824985,41.3754481590154));
#108590=CARTESIAN_POINT('Ctrl Pts',(110.537067936161,24.2280974570609,41.1338985084622));
#108591=CARTESIAN_POINT('Ctrl Pts',(110.228392691396,24.2491059316234,41.0589806166415));
#108592=CARTESIAN_POINT('Ctrl Pts',(109.91971744663,24.2701144061858,40.9840627248208));
#108593=CARTESIAN_POINT('Ctrl Pts',(109.570599419405,24.2911228807483,41.0757765917327));
#108594=CARTESIAN_POINT('Ctrl Pts',(109.338599388585,24.3121313553108,41.2927306797899));
#108595=CARTESIAN_POINT('Ctrl Pts',(109.14669596694,24.329508931244,41.4721885518035));
#108596=CARTESIAN_POINT('Ctrl Pts',(109.034925837462,24.3468865071771,41.7373370225303));
#108597=CARTESIAN_POINT('Ctrl Pts',(109.032632519022,24.3642640831103,42.0007718204176));
#108598=CARTESIAN_POINT('Ctrl Pts',(109.032577150836,24.4222359168897,42.0007573162032));
#108599=CARTESIAN_POINT('Ctrl Pts',(109.03486151758,24.4047293121148,41.7354060038618));
#108600=CARTESIAN_POINT('Ctrl Pts',(109.148488100179,24.3872227073399,41.4683337841834));
#108601=CARTESIAN_POINT('Ctrl Pts',(109.342912081085,24.369716102565,41.288722292881));
#108602=CARTESIAN_POINT('Ctrl Pts',(109.57622695337,24.3487076280025,41.0731828724926));
#108603=CARTESIAN_POINT('Ctrl Pts',(109.925896158499,24.3276991534401,40.983593481603));
#108604=CARTESIAN_POINT('Ctrl Pts',(110.234110139142,24.3066906788776,41.0603868046682));
#108605=CARTESIAN_POINT('Ctrl Pts',(110.542324119785,24.2856822043151,41.1371801277335));
#108606=CARTESIAN_POINT('Ctrl Pts',(110.809082875943,24.2646737297527,41.3803561647535));
#108607=CARTESIAN_POINT('Ctrl Pts',(110.913995235129,24.2436652551902,41.6801668807872));
#108608=CARTESIAN_POINT('Ctrl Pts',(111.018907594316,24.2226567806277,41.9799775968209));
#108609=CARTESIAN_POINT('Ctrl Pts',(110.961973556532,24.2016483060653,42.3364229918684));
#108610=CARTESIAN_POINT('Ctrl Pts',(110.768888098739,24.1806398315028,42.5886353606882));
#108611=CARTESIAN_POINT('Ctrl Pts',(110.575802640947,24.1596313569404,42.8408477295081));
#108612=CARTESIAN_POINT('Ctrl Pts',(110.246565763145,24.1386228823779,42.9888270721004));
#108613=CARTESIAN_POINT('Ctrl Pts',(109.929765653102,24.1176144078154,42.9657886280353));
#108614=CARTESIAN_POINT('Ctrl Pts',(109.612965543059,24.096605933253,42.9427501839702));
#108615=CARTESIAN_POINT('Ctrl Pts',(109.308602200776,24.0755974586905,42.7486939532477));
#108616=CARTESIAN_POINT('Ctrl Pts',(109.154038237157,24.0545889841281,42.4711997629087));
#108617=CARTESIAN_POINT('Ctrl Pts',(109.07469536225,24.0438046283819,42.3287526729402));
#108618=CARTESIAN_POINT('Ctrl Pts',(109.034826328108,24.0330202726358,42.1643187312172));
#108619=CARTESIAN_POINT('Ctrl Pts',(109.034721981614,24.0222359168897,41.9999322711442));
#108620=CARTESIAN_POINT('Origin',(110.,24.53,42.));
#108621=CARTESIAN_POINT('',(109.032328989546,23.5642640831103,41.9994138103573));
#108622=CARTESIAN_POINT('',(109.032351030732,23.6222359168897,41.9993265593643));
#108623=CARTESIAN_POINT('',(109.03325,24.53,42.));
#108624=CARTESIAN_POINT('Ctrl Pts',(109.032328989546,23.5642640831103,41.9994138103573));
#108625=CARTESIAN_POINT('Ctrl Pts',(109.034503741766,23.5824599536567,42.2750214683126));
#108626=CARTESIAN_POINT('Ctrl Pts',(109.158321797255,23.6006558242031,42.5522194353554));
#108627=CARTESIAN_POINT('Ctrl Pts',(109.366343274976,23.6188516947496,42.7322146822975));
#108628=CARTESIAN_POINT('Ctrl Pts',(109.606519413403,23.639860169312,42.9400324702457));
#108629=CARTESIAN_POINT('Ctrl Pts',(109.958942128383,23.6608686438745,43.018275090416));
#108630=CARTESIAN_POINT('Ctrl Pts',(110.264507194704,23.6818771184369,42.9315276900637));
#108631=CARTESIAN_POINT('Ctrl Pts',(110.570072261024,23.7028855929994,42.8447802897114));
#108632=CARTESIAN_POINT('Ctrl Pts',(110.828779678684,23.7238940675619,42.5930428688364));
#108633=CARTESIAN_POINT('Ctrl Pts',(110.923896771461,23.7449025421243,42.2899762255731));
#108634=CARTESIAN_POINT('Ctrl Pts',(111.019013864237,23.7659110166868,41.9869095823098));
#108635=CARTESIAN_POINT('Ctrl Pts',(110.95054063213,23.7869194912492,41.6325137166583));
#108636=CARTESIAN_POINT('Ctrl Pts',(110.749368036451,23.8079279658117,41.3867081653265));
#108637=CARTESIAN_POINT('Ctrl Pts',(110.548195440771,23.8289364403742,41.1409026139947));
#108638=CARTESIAN_POINT('Ctrl Pts',(110.21432348152,23.8499449149366,41.0036873769827));
#108639=CARTESIAN_POINT('Ctrl Pts',(109.898437833994,23.8709533894991,41.0370002203453));
#108640=CARTESIAN_POINT('Ctrl Pts',(109.582552186467,23.8919618640615,41.0703130637079));
#108641=CARTESIAN_POINT('Ctrl Pts',(109.284652850666,23.912970338624,41.2741539874452));
#108642=CARTESIAN_POINT('Ctrl Pts',(109.13918242657,23.9339788131865,41.5565221093782));
#108643=CARTESIAN_POINT('Ctrl Pts',(109.069280301334,23.9440739031611,41.6922069535301));
#108644=CARTESIAN_POINT('Ctrl Pts',(109.034574612883,23.9541689931357,41.8460240374021));
#108645=CARTESIAN_POINT('Ctrl Pts',(109.034717052885,23.9642640831103,41.9999017201984));
#108646=CARTESIAN_POINT('Ctrl Pts',(109.034721981614,24.0222359168897,41.9999322711442));
#108647=CARTESIAN_POINT('Ctrl Pts',(109.034623055819,24.0120117980733,41.8440855298878));
#108648=CARTESIAN_POINT('Ctrl Pts',(109.070264656034,24.001787679257,41.688281465168));
#108649=CARTESIAN_POINT('Ctrl Pts',(109.141894615443,23.9915635604407,41.5512957262226));
#108650=CARTESIAN_POINT('Ctrl Pts',(109.2890795423,23.9705550858782,41.2698180298312));
#108651=CARTESIAN_POINT('Ctrl Pts',(109.588213980968,23.9495466113158,41.0677947870039));
#108652=CARTESIAN_POINT('Ctrl Pts',(109.904295637963,23.9285381367533,41.0364018162067));
#108653=CARTESIAN_POINT('Ctrl Pts',(110.220377294958,23.9075296621908,41.0050088454096));
#108654=CARTESIAN_POINT('Ctrl Pts',(110.553406170279,23.8865211876284,41.1442461466425));
#108655=CARTESIAN_POINT('Ctrl Pts',(110.753081882588,23.8655127130659,41.3912733291643));
#108656=CARTESIAN_POINT('Ctrl Pts',(110.952757594896,23.8445042385035,41.638300511686));
#108657=CARTESIAN_POINT('Ctrl Pts',(111.019080144193,23.823495763941,41.9931175754965));
#108658=CARTESIAN_POINT('Ctrl Pts',(110.922119084851,23.8024872893785,42.2955939150102));
#108659=CARTESIAN_POINT('Ctrl Pts',(110.825158025509,23.7814788148161,42.5980702545239));
#108660=CARTESIAN_POINT('Ctrl Pts',(110.564913357529,23.7604703402536,42.8482058697408));
#108661=CARTESIAN_POINT('Ctrl Pts',(110.258832885919,23.7394618656911,42.9331070807446));
#108662=CARTESIAN_POINT('Ctrl Pts',(109.95275241431,23.7184533911287,43.0180082917484));
#108663=CARTESIAN_POINT('Ctrl Pts',(109.600836139072,23.6974449165662,42.9376750985392));
#108664=CARTESIAN_POINT('Ctrl Pts',(109.361915079957,23.6764364420038,42.7283727071308));
#108665=CARTESIAN_POINT('Ctrl Pts',(109.156448046066,23.6583696002991,42.5483770980853));
#108666=CARTESIAN_POINT('Ctrl Pts',(109.034548144198,23.6403027585944,42.2730005837007));
#108667=CARTESIAN_POINT('Ctrl Pts',(109.032351030732,23.6222359168897,41.9993265593643));
#108668=CARTESIAN_POINT('Origin',(110.,26.4327725593024,42.));
#108669=CARTESIAN_POINT('',(109.26029596408,23.4327725593024,41.9995519067537));
#108670=CARTESIAN_POINT('',(109.261,23.36675,42.));
#108671=CARTESIAN_POINT('',(109.261,26.4327725593024,42.));
#108672=CARTESIAN_POINT('',(109.624043822086,23.36675,41.3637783780095));
#108673=CARTESIAN_POINT('Ctrl Pts',(109.26029596408,23.4327725593024,41.9995519067537));
#108674=CARTESIAN_POINT('Ctrl Pts',(109.260038998003,23.4299599552863,41.9669864411116));
#108675=CARTESIAN_POINT('Ctrl Pts',(109.275412450265,23.4079524355189,41.7124017577352));
#108676=CARTESIAN_POINT('Ctrl Pts',(109.433281110202,23.3859449157514,41.4766714936968));
#108677=CARTESIAN_POINT('Ctrl Pts',(109.623765654177,23.36675,41.3626306739548));
#108678=CARTESIAN_POINT('Origin',(110.,23.36675,42.));
#108679=CARTESIAN_POINT('Origin',(110.,26.4327725593024,42.));
#108680=CARTESIAN_POINT('',(109.262121439961,23.8327725593024,41.9999248732626));
#108681=CARTESIAN_POINT('',(109.260312812734,23.7537274406976,41.9994852106234));
#108682=CARTESIAN_POINT('',(109.261,26.4327725593024,42.));
#108683=CARTESIAN_POINT('Ctrl Pts',(109.262121439961,23.8327725593024,41.9999248732626));
#108684=CARTESIAN_POINT('Ctrl Pts',(109.262012556422,23.8226774693278,41.8822981780607));
#108685=CARTESIAN_POINT('Ctrl Pts',(109.343751851955,23.7915739047907,41.5200261518318));
#108686=CARTESIAN_POINT('Ctrl Pts',(109.908615127961,23.7394618656911,41.1335121918162));
#108687=CARTESIAN_POINT('Ctrl Pts',(110.674267192777,23.6764364420038,41.4481811139323));
#108688=CARTESIAN_POINT('Ctrl Pts',(110.831293472147,23.6134110183164,42.2608996390416));
#108689=CARTESIAN_POINT('Ctrl Pts',(110.23801253607,23.550385594629,42.8381966259357));
#108690=CARTESIAN_POINT('Ctrl Pts',(109.465885790711,23.4901727749577,42.6667740215107));
#108691=CARTESIAN_POINT('Ctrl Pts',(109.261958381344,23.4509684298488,42.2102310474094));
#108692=CARTESIAN_POINT('Ctrl Pts',(109.26029596408,23.4327725593024,41.9995519067537));
#108693=CARTESIAN_POINT('',(109.276407492811,23.36675,42.1501162334309));
#108694=CARTESIAN_POINT('Origin',(110.,23.36675,42.));
#108695=CARTESIAN_POINT('Ctrl Pts',(109.260312812734,23.7537274406976,41.9994852106234));
#108696=CARTESIAN_POINT('Ctrl Pts',(109.26003935578,23.7507858078399,41.9654232168984));
#108697=CARTESIAN_POINT('Ctrl Pts',(109.277562880338,23.7268357004196,41.6883790874115));
#108698=CARTESIAN_POINT('Ctrl Pts',(109.627143274457,23.6818771184369,41.2124713920096));
#108699=CARTESIAN_POINT('Ctrl Pts',(110.453854470857,23.6188516947496,41.2562957542224));
#108700=CARTESIAN_POINT('Ctrl Pts',(110.870694764692,23.5558262710622,41.9711141768508));
#108701=CARTESIAN_POINT('Ctrl Pts',(110.502088724856,23.4928008473748,42.7126144441227));
#108702=CARTESIAN_POINT('Ctrl Pts',(109.679417589571,23.4297754236874,42.8095875279876));
#108703=CARTESIAN_POINT('Ctrl Pts',(109.325945901895,23.3877584745625,42.3889020117039));
#108704=CARTESIAN_POINT('Ctrl Pts',(109.276407492811,23.36675,42.1501162334309));
#108705=CARTESIAN_POINT('Origin',(110.,26.4327725593024,42.));
#108706=CARTESIAN_POINT('',(109.26052798713,24.2327725593024,42.0005899925406));
#108707=CARTESIAN_POINT('',(109.262125207564,24.1537274406976,41.9999482269207));
#108708=CARTESIAN_POINT('',(109.261,26.4327725593024,42.));
#108709=CARTESIAN_POINT('Ctrl Pts',(109.26052798713,24.2327725593024,42.0005899925406));
#108710=CARTESIAN_POINT('Ctrl Pts',(109.262281038411,24.2153949833692,41.7992159913627));
#108711=CARTESIAN_POINT('Ctrl Pts',(109.451010737328,24.1770089328736,41.3514989556746));
#108712=CARTESIAN_POINT('Ctrl Pts',(110.205502368947,24.1176144078154,41.1532927913056));
#108713=CARTESIAN_POINT('Ctrl Pts',(110.820626619199,24.0545889841281,41.7072266679816));
#108714=CARTESIAN_POINT('Ctrl Pts',(110.695035015874,23.9915635604407,42.525423808948));
#108715=CARTESIAN_POINT('Ctrl Pts',(109.942089921891,23.9285381367533,42.8693626760629));
#108716=CARTESIAN_POINT('Ctrl Pts',(109.353645406068,23.8756078030405,42.4991939976866));
#108717=CARTESIAN_POINT('Ctrl Pts',(109.262239149456,23.8436859438902,42.1270862324741));
#108718=CARTESIAN_POINT('Ctrl Pts',(109.262121439961,23.8327725593024,41.9999248732626));
#108719=CARTESIAN_POINT('Ctrl Pts',(109.262125207564,24.1537274406976,41.9999482269206));
#108720=CARTESIAN_POINT('Ctrl Pts',(109.262049587019,24.1435033218813,41.8808163502323));
#108721=CARTESIAN_POINT('Ctrl Pts',(109.345277616316,24.1122707285025,41.5169924706903));
#108722=CARTESIAN_POINT('Ctrl Pts',(109.913887232595,24.0600296605612,41.1329766445788));
#108723=CARTESIAN_POINT('Ctrl Pts',(110.677605894697,23.9970042368739,41.452282666646));
#108724=CARTESIAN_POINT('Ctrl Pts',(110.82970011946,23.9339788131865,42.2659671046784));
#108725=CARTESIAN_POINT('Ctrl Pts',(110.232893883192,23.8709533894991,42.839590749815));
#108726=CARTESIAN_POINT('Ctrl Pts',(109.463528899382,23.8108695986695,42.663965039265));
#108727=CARTESIAN_POINT('Ctrl Pts',(109.261992323312,23.7717942824023,42.2086862491387));
#108728=CARTESIAN_POINT('Ctrl Pts',(109.260312812734,23.7537274406976,41.9994852106234));
#108729=CARTESIAN_POINT('Origin',(110.,26.4327725593024,42.));
#108730=CARTESIAN_POINT('',(109.260534829689,24.6327725593024,41.9994083152275));
#108731=CARTESIAN_POINT('',(109.260485662754,24.5537274406976,42.0005789052745));
#108732=CARTESIAN_POINT('',(109.261,26.4327725593024,42.));
#108733=CARTESIAN_POINT('Ctrl Pts',(109.260534829689,24.6327725593024,41.9994083152275));
#108734=CARTESIAN_POINT('Ctrl Pts',(109.260165847833,24.6291209719731,41.9570921474246));
#108735=CARTESIAN_POINT('Ctrl Pts',(109.282620247005,24.6044609100813,41.6717119456296));
#108736=CARTESIAN_POINT('Ctrl Pts',(109.653720613876,24.5587923736271,41.2004783760763));
#108737=CARTESIAN_POINT('Ctrl Pts',(110.478421617924,24.4957669499397,41.271812522066));
#108738=CARTESIAN_POINT('Ctrl Pts',(110.871288739239,24.4327415262524,42.0004247254552));
#108739=CARTESIAN_POINT('Ctrl Pts',(110.4777114569,24.369716102565,42.7286535557603));
#108740=CARTESIAN_POINT('Ctrl Pts',(109.652941300575,24.3066906788776,42.7991836534335));
#108741=CARTESIAN_POINT('Ctrl Pts',(109.282468435015,24.2610428311234,42.32780213349));
#108742=CARTESIAN_POINT('Ctrl Pts',(109.260161701779,24.2364034579317,42.042665399816));
#108743=CARTESIAN_POINT('Ctrl Pts',(109.26052798713,24.2327725593024,42.0005899925406));
#108744=CARTESIAN_POINT('Ctrl Pts',(109.260485662754,24.5537274406976,42.0005789052745));
#108745=CARTESIAN_POINT('Ctrl Pts',(109.262231871209,24.5362208359227,41.7977398881343));
#108746=CARTESIAN_POINT('Ctrl Pts',(109.453322360428,24.4977057565854,41.3485935708913));
#108747=CARTESIAN_POINT('Ctrl Pts',(110.210646810159,24.4381822026855,41.1545580791696));
#108748=CARTESIAN_POINT('Ctrl Pts',(110.822391482929,24.3751567789981,41.7122216675569));
#108749=CARTESIAN_POINT('Ctrl Pts',(110.691827467654,24.3121313553108,42.5296402771459));
#108750=CARTESIAN_POINT('Ctrl Pts',(109.93680480607,24.2491059316234,42.8689939906469));
#108751=CARTESIAN_POINT('Ctrl Pts',(109.352051429389,24.1963046267523,42.49616645061));
#108752=CARTESIAN_POINT('Ctrl Pts',(109.262204971784,24.1645117964438,42.1256080086574));
#108753=CARTESIAN_POINT('Ctrl Pts',(109.262125207564,24.1537274406976,41.9999482269206));
#108754=CARTESIAN_POINT('Origin',(110.,26.4327725593024,42.));
#108755=CARTESIAN_POINT('',(109.262120563564,25.0327725593024,42.0000796206024));
#108756=CARTESIAN_POINT('',(109.260577824628,24.9537274406976,41.9993983065969));
#108757=CARTESIAN_POINT('',(109.261,26.4327725593024,42.));
#108758=CARTESIAN_POINT('Ctrl Pts',(109.262120563564,25.0327725593024,42.0000796206024));
#108759=CARTESIAN_POINT('Ctrl Pts',(109.262244497832,25.0218384860145,41.872677206789));
#108760=CARTESIAN_POINT('Ctrl Pts',(109.353902434325,24.9898959381642,41.5003194382249));
#108761=CARTESIAN_POINT('Ctrl Pts',(109.942937403792,24.9369449157514,41.1305819691232));
#108762=CARTESIAN_POINT('Ctrl Pts',(110.695546992547,24.873919492064,41.4752537248938));
#108763=CARTESIAN_POINT('Ctrl Pts',(110.820340769253,24.8108940683766,42.2935734034257));
#108764=CARTESIAN_POINT('Ctrl Pts',(110.204676801728,24.7478686446893,42.8469070832775));
#108765=CARTESIAN_POINT('Ctrl Pts',(109.450641491291,24.6884948083312,42.6480348344885));
#108766=CARTESIAN_POINT('Ctrl Pts',(109.262288690651,24.6501294465356,42.2005474052893));
#108767=CARTESIAN_POINT('Ctrl Pts',(109.260534829689,24.6327725593024,41.9994083152275));
#108768=CARTESIAN_POINT('Ctrl Pts',(109.260577824628,24.9537274406976,41.9993983065969));
#108769=CARTESIAN_POINT('Ctrl Pts',(109.260192213384,24.9499468245266,41.9555803058905));
#108770=CARTESIAN_POINT('Ctrl Pts',(109.28357308373,24.9251577337931,41.6686811256762));
#108771=CARTESIAN_POINT('Ctrl Pts',(109.658588394334,24.8793601684972,41.1983877597661));
#108772=CARTESIAN_POINT('Ctrl Pts',(110.482840325691,24.8163347448098,41.2747349865707));
#108773=CARTESIAN_POINT('Ctrl Pts',(110.871269977697,24.7533093211224,42.0057224200596));
#108774=CARTESIAN_POINT('Ctrl Pts',(110.473272149655,24.6902838974351,42.7315446535164));
#108775=CARTESIAN_POINT('Ctrl Pts',(109.64808846612,24.6272584737477,42.7970585845476));
#108776=CARTESIAN_POINT('Ctrl Pts',(109.281527690817,24.5817396548352,42.3247719981271));
#108777=CARTESIAN_POINT('Ctrl Pts',(109.26013636632,24.5572293104852,42.0411530677117));
#108778=CARTESIAN_POINT('Ctrl Pts',(109.260485662754,24.5537274406976,42.0005789052745));
#108779=CARTESIAN_POINT('Origin',(110.,26.4327725593024,42.));
#108780=CARTESIAN_POINT('',(109.260278634324,25.4327725593024,42.0005281107854));
#108781=CARTESIAN_POINT('',(109.262116416571,25.3537274406976,42.0001049160966));
#108782=CARTESIAN_POINT('',(109.261,26.4327725593024,42.));
#108783=CARTESIAN_POINT('Ctrl Pts',(109.260278634324,25.4327725593024,42.0005281107854));
#108784=CARTESIAN_POINT('Ctrl Pts',(109.261931868618,25.414556000056,41.7896344627551));
#108785=CARTESIAN_POINT('Ctrl Pts',(109.466290765521,25.3753309662471,41.3326451825462));
#108786=CARTESIAN_POINT('Ctrl Pts',(110.238819563989,25.3150974578757,41.1620962618873));
#108787=CARTESIAN_POINT('Ctrl Pts',(110.831552217079,25.2520720341883,41.7398822563778));
#108788=CARTESIAN_POINT('Ctrl Pts',(110.673726619585,25.1890466105009,42.5524896004734));
#108789=CARTESIAN_POINT('Ctrl Pts',(109.907771480839,25.1260211868136,42.866391842584));
#108790=CARTESIAN_POINT('Ctrl Pts',(109.343508090084,25.073929836414,42.4794889021236));
#108791=CARTESIAN_POINT('Ctrl Pts',(109.262006373407,25.042846960577,42.1174652468295));
#108792=CARTESIAN_POINT('Ctrl Pts',(109.262120563564,25.0327725593024,42.0000796206024));
#108793=CARTESIAN_POINT('Ctrl Pts',(109.262116416571,25.3537274406976,42.0001049160966));
#108794=CARTESIAN_POINT('Ctrl Pts',(109.262278638424,25.342664338568,41.8712007900642));
#108795=CARTESIAN_POINT('Ctrl Pts',(109.355509647679,25.310592761876,41.4972898740467));
#108796=CARTESIAN_POINT('Ctrl Pts',(109.948226154444,25.2575127106215,41.130252762051));
#108797=CARTESIAN_POINT('Ctrl Pts',(110.698724042524,25.1944872869341,41.479491846189));
#108798=CARTESIAN_POINT('Ctrl Pts',(110.818540825836,25.1314618632468,42.298556232552));
#108799=CARTESIAN_POINT('Ctrl Pts',(110.19952340274,25.0684364395593,42.8481356795978));
#108800=CARTESIAN_POINT('Ctrl Pts',(109.448347483645,25.009191632043,42.6451247354048));
#108801=CARTESIAN_POINT('Ctrl Pts',(109.262335013295,24.9709552990891,42.1990721896413));
#108802=CARTESIAN_POINT('Ctrl Pts',(109.260577824628,24.9537274406976,41.9993983065969));
#108803=CARTESIAN_POINT('Origin',(110.,23.36675,42.));
#108804=CARTESIAN_POINT('',(110.966013043313,23.36675,41.9622592706773));
#108805=CARTESIAN_POINT('Ctrl Pts',(109.623765654177,23.36675,41.3626306739548));
#108806=CARTESIAN_POINT('Ctrl Pts',(109.640283077264,23.36675,41.3490485696045));
#108807=CARTESIAN_POINT('Ctrl Pts',(109.657385440225,23.36675,41.3362594125259));
#108808=CARTESIAN_POINT('Ctrl Pts',(109.675032430314,23.36675,41.32431606363));
#108809=CARTESIAN_POINT('Ctrl Pts',(109.702587947937,23.36675,41.3056666985359));
#108810=CARTESIAN_POINT('Ctrl Pts',(109.731469510825,23.36675,41.2890775093067));
#108811=CARTESIAN_POINT('Ctrl Pts',(109.761429487403,23.36675,41.2745065051108));
#108812=CARTESIAN_POINT('Ctrl Pts',(109.770540279536,23.36675,41.2700754806055));
#108813=CARTESIAN_POINT('Ctrl Pts',(109.779751057641,23.36675,41.2658313065101));
#108814=CARTESIAN_POINT('Ctrl Pts',(109.789055479984,23.36675,41.2617733906582));
#108815=CARTESIAN_POINT('Ctrl Pts',(109.797186423754,23.36675,41.2582272612589));
#108816=CARTESIAN_POINT('Ctrl Pts',(109.805387488184,23.36675,41.254824141658));
#108817=CARTESIAN_POINT('Ctrl Pts',(109.813642892422,23.36675,41.2515677867019));
#108818=CARTESIAN_POINT('Ctrl Pts',(109.846811880316,23.36675,41.2384842362177));
#108819=CARTESIAN_POINT('Ctrl Pts',(109.880903278198,23.36675,41.2277454904922));
#108820=CARTESIAN_POINT('Ctrl Pts',(109.91562914288,23.36675,41.2193032636084));
#108821=CARTESIAN_POINT('Ctrl Pts',(109.941043992756,23.36675,41.2131246434118));
#108822=CARTESIAN_POINT('Ctrl Pts',(109.966799726391,23.36675,41.2081768283695));
#108823=CARTESIAN_POINT('Ctrl Pts',(109.992794303592,23.36675,41.2044543970879));
#108824=CARTESIAN_POINT('Ctrl Pts',(110.001231861349,23.36675,41.2032461362768));
#108825=CARTESIAN_POINT('Ctrl Pts',(110.009690500122,23.36675,41.20216776691));
#108826=CARTESIAN_POINT('Ctrl Pts',(110.0181571196,23.36675,41.2012197872153));
#108827=CARTESIAN_POINT('Ctrl Pts',(110.055685764639,23.36675,41.1970178275597));
#108828=CARTESIAN_POINT('Ctrl Pts',(110.093422889363,23.36675,41.1953662362226));
#108829=CARTESIAN_POINT('Ctrl Pts',(110.131060990144,23.36675,41.1962158968578));
#108830=CARTESIAN_POINT('Ctrl Pts',(110.168976618814,23.36675,41.1970718225414));
#108831=CARTESIAN_POINT('Ctrl Pts',(110.206793073989,23.36675,41.2004656411429));
#108832=CARTESIAN_POINT('Ctrl Pts',(110.244219876593,23.36675,41.2063948015286));
#108833=CARTESIAN_POINT('Ctrl Pts',(110.264234048366,23.36675,41.2095654499991));
#108834=CARTESIAN_POINT('Ctrl Pts',(110.284137081409,23.36675,41.2134619553918));
#108835=CARTESIAN_POINT('Ctrl Pts',(110.303885271042,23.36675,41.2180900338887));
#108836=CARTESIAN_POINT('Ctrl Pts',(110.311643364417,23.36675,41.2199081785287));
#108837=CARTESIAN_POINT('Ctrl Pts',(110.31937791337,23.36675,41.2218395140319));
#108838=CARTESIAN_POINT('Ctrl Pts',(110.327071396012,23.36675,41.2238802066803));
#108839=CARTESIAN_POINT('Ctrl Pts',(110.366741777769,23.36675,41.2344027567634));
#108840=CARTESIAN_POINT('Ctrl Pts',(110.405415001551,23.36675,41.2478495563126));
#108841=CARTESIAN_POINT('Ctrl Pts',(110.442737999354,23.36675,41.2641904381727));
#108842=CARTESIAN_POINT('Ctrl Pts',(110.477160799849,23.36675,41.2792615457821));
#108843=CARTESIAN_POINT('Ctrl Pts',(110.510436743391,23.36675,41.2967944343093));
#108844=CARTESIAN_POINT('Ctrl Pts',(110.542458466816,23.36675,41.3165519498535));
#108845=CARTESIAN_POINT('Ctrl Pts',(110.557087770437,23.36675,41.3255782814429));
#108846=CARTESIAN_POINT('Ctrl Pts',(110.57145516249,23.36675,41.3350696364183));
#108847=CARTESIAN_POINT('Ctrl Pts',(110.585549426311,23.36675,41.3450067176969));
#108848=CARTESIAN_POINT('Ctrl Pts',(110.592366803798,23.36675,41.3498132712743));
#108849=CARTESIAN_POINT('Ctrl Pts',(110.599120267254,23.36675,41.3547241379346));
#108850=CARTESIAN_POINT('Ctrl Pts',(110.605808473246,23.36675,41.3597372899822));
#108851=CARTESIAN_POINT('Ctrl Pts',(110.612060773751,23.36675,41.3644237085989));
#108852=CARTESIAN_POINT('Ctrl Pts',(110.618252318128,23.36675,41.3691968134977));
#108853=CARTESIAN_POINT('Ctrl Pts',(110.624375787699,23.36675,41.3740493717938));
#108854=CARTESIAN_POINT('Ctrl Pts',(110.655391774354,23.36675,41.3986280655561));
#108855=CARTESIAN_POINT('Ctrl Pts',(110.684712587694,23.36675,41.4252784641286));
#108856=CARTESIAN_POINT('Ctrl Pts',(110.712226150003,23.36675,41.4537232719963));
#108857=CARTESIAN_POINT('Ctrl Pts',(110.740390836705,23.36675,41.4828412427224));
#108858=CARTESIAN_POINT('Ctrl Pts',(110.766662646556,23.36675,41.5138401512147));
#108859=CARTESIAN_POINT('Ctrl Pts',(110.790902143872,23.36675,41.5464736475016));
#108860=CARTESIAN_POINT('Ctrl Pts',(110.802327249331,23.36675,41.5618552014886));
#108861=CARTESIAN_POINT('Ctrl Pts',(110.813300488072,23.36675,41.5776005713721));
#108862=CARTESIAN_POINT('Ctrl Pts',(110.823804900303,23.36675,41.5936871406374));
#108863=CARTESIAN_POINT('Ctrl Pts',(110.829218563341,23.36675,41.6019776821278));
#108864=CARTESIAN_POINT('Ctrl Pts',(110.834507674679,23.36675,41.6103588780924));
#108865=CARTESIAN_POINT('Ctrl Pts',(110.839669716296,23.36675,41.6188278067615));
#108866=CARTESIAN_POINT('Ctrl Pts',(110.844131071638,23.36675,41.6261471782345));
#108867=CARTESIAN_POINT('Ctrl Pts',(110.848493088426,23.36675,41.6335249163995));
#108868=CARTESIAN_POINT('Ctrl Pts',(110.852752219124,23.36675,41.6409543603531));
#108869=CARTESIAN_POINT('Ctrl Pts',(110.873798952144,23.36675,41.6776673739833));
#108870=CARTESIAN_POINT('Ctrl Pts',(110.892355271488,23.36675,41.7156717003438));
#108871=CARTESIAN_POINT('Ctrl Pts',(110.90828352324,23.36675,41.7546923358551));
#108872=CARTESIAN_POINT('Ctrl Pts',(110.924103863858,23.36675,41.7934486133495));
#108873=CARTESIAN_POINT('Ctrl Pts',(110.937332486947,23.36675,41.8332084462172));
#108874=CARTESIAN_POINT('Ctrl Pts',(110.947800034903,23.36675,41.8737389314944));
#108875=CARTESIAN_POINT('Ctrl Pts',(110.955324313756,23.36675,41.9028730395555));
#108876=CARTESIAN_POINT('Ctrl Pts',(110.961421269866,23.36675,41.9324061480694));
#108877=CARTESIAN_POINT('Ctrl Pts',(110.966013043313,23.36675,41.9622592706773));
#108878=CARTESIAN_POINT('',(109.03325,23.36675,42.));
#108879=CARTESIAN_POINT('Origin',(110.,23.36675,42.));
#108880=CARTESIAN_POINT('',(110.622527742627,23.36675,42.7406037150629));
#108881=CARTESIAN_POINT('Origin',(110.,23.36675,42.));
#108882=CARTESIAN_POINT('Ctrl Pts',(110.622830835844,23.36675,42.7413141620339));
#108883=CARTESIAN_POINT('Ctrl Pts',(110.599989634549,23.36675,42.7566319918816));
#108884=CARTESIAN_POINT('Ctrl Pts',(110.576498629828,23.36675,42.77088175598));
#108885=CARTESIAN_POINT('Ctrl Pts',(110.552388008497,23.36675,42.7839885195071));
#108886=CARTESIAN_POINT('Ctrl Pts',(110.519529732011,23.36675,42.8018505917406));
#108887=CARTESIAN_POINT('Ctrl Pts',(110.485520388848,23.36675,42.817590950745));
#108888=CARTESIAN_POINT('Ctrl Pts',(110.450577637721,23.36675,42.8312003669318));
#108889=CARTESIAN_POINT('Ctrl Pts',(110.435562109163,23.36675,42.8370485778143));
#108890=CARTESIAN_POINT('Ctrl Pts',(110.420374190204,23.36675,42.8425028947487));
#108891=CARTESIAN_POINT('Ctrl Pts',(110.405031249077,23.36675,42.8475608039096));
#108892=CARTESIAN_POINT('Ctrl Pts',(110.394627168308,23.36675,42.8509905827894));
#108893=CARTESIAN_POINT('Ctrl Pts',(110.384150292893,23.36675,42.8542383301765));
#108894=CARTESIAN_POINT('Ctrl Pts',(110.373624138033,23.36675,42.8572982649821));
#108895=CARTESIAN_POINT('Ctrl Pts',(110.333558504764,23.36675,42.8689452744911));
#108896=CARTESIAN_POINT('Ctrl Pts',(110.292721046436,23.36675,42.8778954764353));
#108897=CARTESIAN_POINT('Ctrl Pts',(110.251418895275,23.36675,42.8841357112893));
#108898=CARTESIAN_POINT('Ctrl Pts',(110.227354637757,23.36675,42.8877715175191));
#108899=CARTESIAN_POINT('Ctrl Pts',(110.203132624234,23.36675,42.8904863918268));
#108900=CARTESIAN_POINT('Ctrl Pts',(110.178815468667,23.36675,42.8922697532124));
#108901=CARTESIAN_POINT('Ctrl Pts',(110.168535476505,23.36675,42.8930236629784));
#108902=CARTESIAN_POINT('Ctrl Pts',(110.158238509494,23.36675,42.8936110274913));
#108903=CARTESIAN_POINT('Ctrl Pts',(110.147929448515,23.36675,42.894030741929));
#108904=CARTESIAN_POINT('Ctrl Pts',(110.139394679409,23.36675,42.8943782193398));
#108905=CARTESIAN_POINT('Ctrl Pts',(110.130860584535,23.36675,42.8946104043804));
#108906=CARTESIAN_POINT('Ctrl Pts',(110.122331803943,23.36675,42.8947273289625));
#108907=CARTESIAN_POINT('Ctrl Pts',(110.082232323714,23.36675,42.8952770693291));
#108908=CARTESIAN_POINT('Ctrl Pts',(110.042234507434,23.36675,42.8932833778413));
#108909=CARTESIAN_POINT('Ctrl Pts',(110.002614476038,23.36675,42.8887284438273));
#108910=CARTESIAN_POINT('Ctrl Pts',(109.96391576674,23.36675,42.8842794300059));
#108911=CARTESIAN_POINT('Ctrl Pts',(109.925576454932,23.36675,42.8773865373935));
#108912=CARTESIAN_POINT('Ctrl Pts',(109.88787553385,23.36675,42.8679900813404));
#108913=CARTESIAN_POINT('Ctrl Pts',(109.869444813718,23.36675,42.8633964680603));
#108914=CARTESIAN_POINT('Ctrl Pts',(109.851167090035,23.36675,42.8582038996012));
#108915=CARTESIAN_POINT('Ctrl Pts',(109.833077994259,23.36675,42.8524019136406));
#108916=CARTESIAN_POINT('Ctrl Pts',(109.825786637571,23.36675,42.8500632478684));
#108917=CARTESIAN_POINT('Ctrl Pts',(109.818525954487,23.36675,42.8476255425698));
#108918=CARTESIAN_POINT('Ctrl Pts',(109.811298392462,23.36675,42.8450880116248));
#108919=CARTESIAN_POINT('Ctrl Pts',(109.80372490632,23.36675,42.8424290298855));
#108920=CARTESIAN_POINT('Ctrl Pts',(109.79619589683,23.36675,42.8396632494703));
#108921=CARTESIAN_POINT('Ctrl Pts',(109.788717112427,23.36675,42.8367917024267));
#108922=CARTESIAN_POINT('Ctrl Pts',(109.754009543215,23.36675,42.823465416711));
#108923=CARTESIAN_POINT('Ctrl Pts',(109.720357321898,23.36675,42.8078559975844));
#108924=CARTESIAN_POINT('Ctrl Pts',(109.6880062221,23.36675,42.7899211270859));
#108925=CARTESIAN_POINT('Ctrl Pts',(109.657136500616,23.36675,42.7728075062018));
#108926=CARTESIAN_POINT('Ctrl Pts',(109.627451293261,23.36675,42.7535752657674));
#108927=CARTESIAN_POINT('Ctrl Pts',(109.599088885777,23.36675,42.7324037129303));
#108928=CARTESIAN_POINT('Ctrl Pts',(109.584394257825,23.36675,42.7214346831588));
#108929=CARTESIAN_POINT('Ctrl Pts',(109.570055217726,23.36675,42.7099447409629));
#108930=CARTESIAN_POINT('Ctrl Pts',(109.556094587763,23.36675,42.6979572564491));
#108931=CARTESIAN_POINT('Ctrl Pts',(109.549550462915,23.36675,42.692338054774));
#108932=CARTESIAN_POINT('Ctrl Pts',(109.543089524179,23.36675,42.6866095167489));
#108933=CARTESIAN_POINT('Ctrl Pts',(109.536714326725,23.36675,42.6807740087885));
#108934=CARTESIAN_POINT('Ctrl Pts',(109.531161622462,23.36675,42.6756913662265));
#108935=CARTESIAN_POINT('Ctrl Pts',(109.525677396191,23.36675,42.6705306180132));
#108936=CARTESIAN_POINT('Ctrl Pts',(109.52026864601,23.36675,42.6652991990941));
#108937=CARTESIAN_POINT('Ctrl Pts',(109.493456603764,23.36675,42.6393662163564));
#108938=CARTESIAN_POINT('Ctrl Pts',(109.468451235971,23.36675,42.6116582827426));
#108939=CARTESIAN_POINT('Ctrl Pts',(109.445404251841,23.36675,42.5824010814883));
#108940=CARTESIAN_POINT('Ctrl Pts',(109.422626821305,23.36675,42.5534860674685));
#108941=CARTESIAN_POINT('Ctrl Pts',(109.401761820652,23.36675,42.5230565668517));
#108942=CARTESIAN_POINT('Ctrl Pts',(109.3830039642,23.36675,42.4913162448205));
#108943=CARTESIAN_POINT('Ctrl Pts',(109.374367167512,23.36675,42.4767018506383));
#108944=CARTESIAN_POINT('Ctrl Pts',(109.366177803065,23.36675,42.4618094753382));
#108945=CARTESIAN_POINT('Ctrl Pts',(109.358458731183,23.36675,42.4466590557636));
#108946=CARTESIAN_POINT('Ctrl Pts',(109.353454535735,23.36675,42.4368371935207));
#108947=CARTESIAN_POINT('Ctrl Pts',(109.348645687868,23.36675,42.4269012311359));
#108948=CARTESIAN_POINT('Ctrl Pts',(109.344052541533,23.36675,42.4168877708613));
#108949=CARTESIAN_POINT('Ctrl Pts',(109.329326840271,23.36675,42.3847844556495));
#108950=CARTESIAN_POINT('Ctrl Pts',(109.316787386093,23.36675,42.351837783171));
#108951=CARTESIAN_POINT('Ctrl Pts',(109.306593405068,23.36675,42.318236792011));
#108952=CARTESIAN_POINT('Ctrl Pts',(109.296770659685,23.36675,42.2858594528769));
#108953=CARTESIAN_POINT('Ctrl Pts',(109.289125656932,23.36675,42.2528736472171));
#108954=CARTESIAN_POINT('Ctrl Pts',(109.283848189441,23.36675,42.219452110081));
#108955=CARTESIAN_POINT('Ctrl Pts',(109.280227872688,23.36675,42.1965250999214));
#108956=CARTESIAN_POINT('Ctrl Pts',(109.277722664731,23.36675,42.1733931203794));
#108957=CARTESIAN_POINT('Ctrl Pts',(109.276407492811,23.36675,42.1501162334309));
#108958=CARTESIAN_POINT('Ctrl Pts',(109.675031770393,25.824741523808,42.6637142832168));
#108959=CARTESIAN_POINT('Ctrl Pts',(109.456005826793,25.8037330492455,42.5564746547661));
#108960=CARTESIAN_POINT('Ctrl Pts',(109.136184530949,25.7617161001206,42.1096717045468));
#108961=CARTESIAN_POINT('Ctrl Pts',(109.434256215294,25.6986906764332,41.3367908296269));
#108962=CARTESIAN_POINT('Ctrl Pts',(110.244029991095,25.6356652527458,41.163702727801));
#108963=CARTESIAN_POINT('Ctrl Pts',(110.833061721015,25.5726398290584,41.7448763929315));
#108964=CARTESIAN_POINT('Ctrl Pts',(110.670381733412,25.509614405371,42.5566073819969));
#108965=CARTESIAN_POINT('Ctrl Pts',(109.902492493296,25.4465889816836,42.8657999717889));
#108966=CARTESIAN_POINT('Ctrl Pts',(109.222666943948,25.3835635579963,42.3935651416645));
#108967=CARTESIAN_POINT('Ctrl Pts',(109.244454999697,25.3205381343089,41.5660599805031));
#108968=CARTESIAN_POINT('Ctrl Pts',(109.948226154444,25.2575127106215,41.130252762051));
#108969=CARTESIAN_POINT('Ctrl Pts',(110.698724042524,25.1944872869341,41.479491846189));
#108970=CARTESIAN_POINT('Ctrl Pts',(110.818540825836,25.1314618632468,42.298556232552));
#108971=CARTESIAN_POINT('Ctrl Pts',(110.19952340274,25.0684364395593,42.8481356795978));
#108972=CARTESIAN_POINT('Ctrl Pts',(109.400412348972,25.005411015872,42.632169904582));
#108973=CARTESIAN_POINT('Ctrl Pts',(109.142502032814,24.9423855921846,41.8455933143042));
#108974=CARTESIAN_POINT('Ctrl Pts',(109.658588394334,24.8793601684972,41.1983877597661));
#108975=CARTESIAN_POINT('Ctrl Pts',(110.482840325691,24.8163347448098,41.2747349865707));
#108976=CARTESIAN_POINT('Ctrl Pts',(110.871269977697,24.7533093211224,42.0057224200596));
#108977=CARTESIAN_POINT('Ctrl Pts',(110.473272149655,24.6902838974351,42.7315446535164));
#108978=CARTESIAN_POINT('Ctrl Pts',(109.64808846612,24.6272584737477,42.7970585845476));
#108979=CARTESIAN_POINT('Ctrl Pts',(109.140547876918,24.5642330500603,42.1431298816027));
#108980=CARTESIAN_POINT('Ctrl Pts',(109.408767702043,24.5012076263729,41.3600090019544));
#108981=CARTESIAN_POINT('Ctrl Pts',(110.210646810159,24.4381822026855,41.1545580791696));
#108982=CARTESIAN_POINT('Ctrl Pts',(110.822391482929,24.3751567789981,41.7122216675569));
#108983=CARTESIAN_POINT('Ctrl Pts',(110.691827467654,24.3121313553108,42.5296402771459));
#108984=CARTESIAN_POINT('Ctrl Pts',(109.93680480607,24.2491059316234,42.8689939906469));
#108985=CARTESIAN_POINT('Ctrl Pts',(109.238823394285,24.186080507936,42.4239744266317));
#108986=CARTESIAN_POINT('Ctrl Pts',(109.227897007069,24.1230550842486,41.5962665637389));
#108987=CARTESIAN_POINT('Ctrl Pts',(109.913887232595,24.0600296605612,41.1329766445788));
#108988=CARTESIAN_POINT('Ctrl Pts',(110.677605894697,23.9970042368739,41.452282666646));
#108989=CARTESIAN_POINT('Ctrl Pts',(110.82970011946,23.9339788131865,42.2659671046784));
#108990=CARTESIAN_POINT('Ctrl Pts',(110.232893883192,23.8709533894991,42.839590749815));
#108991=CARTESIAN_POINT('Ctrl Pts',(109.425861680241,23.8079279658117,42.6553666077465));
#108992=CARTESIAN_POINT('Ctrl Pts',(109.137082167534,23.7449025421243,41.8796250880568));
#108993=CARTESIAN_POINT('Ctrl Pts',(109.627143274457,23.6818771184369,41.2124713920096));
#108994=CARTESIAN_POINT('Ctrl Pts',(110.453854470857,23.6188516947496,41.2562957542224));
#108995=CARTESIAN_POINT('Ctrl Pts',(110.870694764692,23.5558262710622,41.9711141768508));
#108996=CARTESIAN_POINT('Ctrl Pts',(110.502088724856,23.4928008473748,42.7126144441227));
#108997=CARTESIAN_POINT('Ctrl Pts',(109.679417589571,23.4297754236874,42.8095875279876));
#108998=CARTESIAN_POINT('Ctrl Pts',(109.325945901895,23.3877584745625,42.3889020117039));
#108999=CARTESIAN_POINT('Ctrl Pts',(109.276407492811,23.36675,42.1501162334309));
#109000=CARTESIAN_POINT('Ctrl Pts',(109.641648137424,25.780911015872,42.731896930038));
#109001=CARTESIAN_POINT('Ctrl Pts',(109.400121896731,25.7599025413095,42.6136406911319));
#109002=CARTESIAN_POINT('Ctrl Pts',(109.047445706828,25.7178855921846,42.1209381595358));
#109003=CARTESIAN_POINT('Ctrl Pts',(109.376137971286,25.6548601684972,41.268660072499));
#109004=CARTESIAN_POINT('Ctrl Pts',(110.269098926806,25.5918347448098,41.0777908181288));
#109005=CARTESIAN_POINT('Ctrl Pts',(110.918641246031,25.5288093211224,41.7186678221105));
#109006=CARTESIAN_POINT('Ctrl Pts',(110.739249320144,25.4657838974351,42.6137870532869));
#109007=CARTESIAN_POINT('Ctrl Pts',(109.892475653128,25.4027584737477,42.954742661719));
#109008=CARTESIAN_POINT('Ctrl Pts',(109.142812364103,25.3397330500603,42.4339956608409));
#109009=CARTESIAN_POINT('Ctrl Pts',(109.166838683135,25.2767076263729,41.5214817940167));
#109010=CARTESIAN_POINT('Ctrl Pts',(109.942907483571,25.2136822026855,41.0409045737592));
#109011=CARTESIAN_POINT('Ctrl Pts',(110.770503203861,25.1506567789981,41.4260206093688));
#109012=CARTESIAN_POINT('Ctrl Pts',(110.902628635076,25.0876313553108,42.3292265897751));
#109013=CARTESIAN_POINT('Ctrl Pts',(110.22002022501,25.0246059316234,42.9352637359931));
#109014=CARTESIAN_POINT('Ctrl Pts',(109.338817361366,24.961580507936,42.6971120316765));
#109015=CARTESIAN_POINT('Ctrl Pts',(109.054412198792,24.8985550842486,41.8297312833312));
#109016=CARTESIAN_POINT('Ctrl Pts',(109.623515551217,24.8355296605612,41.1160390057232));
#109017=CARTESIAN_POINT('Ctrl Pts',(110.532441987476,24.7725042368739,41.2002293001437));
#109018=CARTESIAN_POINT('Ctrl Pts',(110.960774595388,24.7094788131865,42.0063102780518));
#109019=CARTESIAN_POINT('Ctrl Pts',(110.521890883116,24.6464533894991,42.8066954405431));
#109020=CARTESIAN_POINT('Ctrl Pts',(109.611936976792,24.5834279658117,42.8789395464919));
#109021=CARTESIAN_POINT('Ctrl Pts',(109.052257294585,24.5204025421243,42.1578334587498));
#109022=CARTESIAN_POINT('Ctrl Pts',(109.348031050775,24.4573771184369,41.2942634224304));
#109023=CARTESIAN_POINT('Ctrl Pts',(110.232286327982,24.3943516947496,41.0677067496842));
#109024=CARTESIAN_POINT('Ctrl Pts',(110.906874865986,24.3313262710621,41.6826585122958));
#109025=CARTESIAN_POINT('Ctrl Pts',(110.762898151352,24.2683008473748,42.5840496470692));
#109026=CARTESIAN_POINT('Ctrl Pts',(109.930312832495,24.2052754236874,42.9582647986622));
#109027=CARTESIAN_POINT('Ctrl Pts',(109.160628549021,24.14225,42.4675288585962));
#109028=CARTESIAN_POINT('Ctrl Pts',(109.148579705924,24.0792245763127,41.554791466712));
#109029=CARTESIAN_POINT('Ctrl Pts',(109.905040961609,24.0161991526252,41.0439082777781));
#109030=CARTESIAN_POINT('Ctrl Pts',(110.747215611665,23.9531737289379,41.3960162603891));
#109031=CARTESIAN_POINT('Ctrl Pts',(110.914934310803,23.8901483052505,42.2932896162213));
#109032=CARTESIAN_POINT('Ctrl Pts',(110.256818818644,23.8271228815631,42.9258409948626));
#109033=CARTESIAN_POINT('Ctrl Pts',(109.366881074771,23.7640974578757,42.722691706941));
#109034=CARTESIAN_POINT('Ctrl Pts',(109.048435556643,23.7010720341883,41.867259104207));
#109035=CARTESIAN_POINT('Ctrl Pts',(109.588840108358,23.638046610501,41.1315694341973));
#109036=CARTESIAN_POINT('Ctrl Pts',(110.500478447283,23.5750211868136,41.1798958255007));
#109037=CARTESIAN_POINT('Ctrl Pts',(110.960140291376,23.5119957631262,41.9681467676392));
#109038=CARTESIAN_POINT('Ctrl Pts',(110.553667753763,23.4489703394388,42.7858205513166));
#109039=CARTESIAN_POINT('Ctrl Pts',(109.646484507038,23.3859449157514,42.892755574672));
#109040=CARTESIAN_POINT('Ctrl Pts',(109.25670105713,23.3439279666265,42.4288534926085));
#109041=CARTESIAN_POINT('Ctrl Pts',(109.202073621132,23.322919492064,42.1655375109067));
#109042=CARTESIAN_POINT('Ctrl Pts',(109.608264504454,25.737080507936,42.8000795768593));
#109043=CARTESIAN_POINT('Ctrl Pts',(109.344237966669,25.7160720333735,42.6708067274977));
#109044=CARTESIAN_POINT('Ctrl Pts',(108.958706882707,25.6740550842486,42.1322046145248));
#109045=CARTESIAN_POINT('Ctrl Pts',(109.318019727278,25.6110296605612,41.2005293153711));
#109046=CARTESIAN_POINT('Ctrl Pts',(110.294167862517,25.5480042368739,40.9918789084566));
#109047=CARTESIAN_POINT('Ctrl Pts',(111.004220771048,25.4849788131864,41.6924592512897));
#109048=CARTESIAN_POINT('Ctrl Pts',(110.808116906876,25.4219533894991,42.6709667245769));
#109049=CARTESIAN_POINT('Ctrl Pts',(109.882458812961,25.3589279658117,43.043685351649));
#109050=CARTESIAN_POINT('Ctrl Pts',(109.062957784258,25.2959025421243,42.4744261800173));
#109051=CARTESIAN_POINT('Ctrl Pts',(109.089222366572,25.2328771184369,41.4769036075303));
#109052=CARTESIAN_POINT('Ctrl Pts',(109.937588812698,25.1698516947495,40.9515563854674));
#109053=CARTESIAN_POINT('Ctrl Pts',(110.842282365199,25.1068262710622,41.3725493725486));
#109054=CARTESIAN_POINT('Ctrl Pts',(110.986716444315,25.0438008473748,42.3598969469982));
#109055=CARTESIAN_POINT('Ctrl Pts',(110.240517047281,24.9807754236874,43.0223917923884));
#109056=CARTESIAN_POINT('Ctrl Pts',(109.277222373761,24.91775,42.762054158771));
#109057=CARTESIAN_POINT('Ctrl Pts',(108.96632236477,24.8547245763126,41.8138692523581));
#109058=CARTESIAN_POINT('Ctrl Pts',(109.5884427081,24.7916991526252,41.0336902516802));
#109059=CARTESIAN_POINT('Ctrl Pts',(110.58204364926,24.7286737289379,41.1257236137168));
#109060=CARTESIAN_POINT('Ctrl Pts',(111.050279213078,24.6656483052505,42.0068981360439));
#109061=CARTESIAN_POINT('Ctrl Pts',(110.570509616578,24.6026228815631,42.8818462275699));
#109062=CARTESIAN_POINT('Ctrl Pts',(109.575785487463,24.5395974578757,42.9608205084363));
#109063=CARTESIAN_POINT('Ctrl Pts',(108.963966712252,24.4765720341883,42.1725370358968));
#109064=CARTESIAN_POINT('Ctrl Pts',(109.287294399508,24.4135466105009,41.2285178429063));
#109065=CARTESIAN_POINT('Ctrl Pts',(110.253925845805,24.3505211868136,40.9808554201988));
#109066=CARTESIAN_POINT('Ctrl Pts',(110.991358249043,24.2874957631262,41.6530953570346));
#109067=CARTESIAN_POINT('Ctrl Pts',(110.83396883505,24.2244703394388,42.6384590169925));
#109068=CARTESIAN_POINT('Ctrl Pts',(109.923820858919,24.1614449157514,43.0475356066774));
#109069=CARTESIAN_POINT('Ctrl Pts',(109.082433703756,24.098419492064,42.5110832905607));
#109070=CARTESIAN_POINT('Ctrl Pts',(109.069262404778,24.0353940683767,41.5133163696852));
#109071=CARTESIAN_POINT('Ctrl Pts',(109.896194690623,23.9723686446893,40.9548399109774));
#109072=CARTESIAN_POINT('Ctrl Pts',(110.816825328633,23.9093432210019,41.3397498541323));
#109073=CARTESIAN_POINT('Ctrl Pts',(111.000168502146,23.8463177973145,42.3206121277642));
#109074=CARTESIAN_POINT('Ctrl Pts',(110.280743754096,23.7832923736271,43.0120912399101));
#109075=CARTESIAN_POINT('Ctrl Pts',(109.307900469302,23.7202669499397,42.7900168061355));
#109076=CARTESIAN_POINT('Ctrl Pts',(108.959788945753,23.6572415262524,41.8548931203572));
#109077=CARTESIAN_POINT('Ctrl Pts',(109.550536942258,23.594216102565,41.050667476385));
#109078=CARTESIAN_POINT('Ctrl Pts',(110.54710242371,23.5311906788776,41.1034958967791));
#109079=CARTESIAN_POINT('Ctrl Pts',(111.04958581806,23.4681652551902,41.9651793584275));
#109080=CARTESIAN_POINT('Ctrl Pts',(110.605246782669,23.4051398315028,42.8590266585105));
#109081=CARTESIAN_POINT('Ctrl Pts',(109.613551424506,23.3421144078155,42.9759236213563));
#109082=CARTESIAN_POINT('Ctrl Pts',(109.187456212365,23.3000974586905,42.4688049735131));
#109083=CARTESIAN_POINT('Ctrl Pts',(109.127739749453,23.2790889841281,42.1809587883825));
#109084=CARTESIAN_POINT('Ctrl Pts',(109.574880871485,25.69325,42.8682622236805));
#109085=CARTESIAN_POINT('Ctrl Pts',(109.288354036607,25.6722415254375,42.7279727638635));
#109086=CARTESIAN_POINT('Ctrl Pts',(108.869968058586,25.6302245763126,42.1434710695137));
#109087=CARTESIAN_POINT('Ctrl Pts',(109.259901483269,25.5671991526252,41.1323985582433));
#109088=CARTESIAN_POINT('Ctrl Pts',(110.319236798229,25.5041737289379,40.9059669987843));
#109089=CARTESIAN_POINT('Ctrl Pts',(111.089800296064,25.4411483052505,41.6662506804688));
#109090=CARTESIAN_POINT('Ctrl Pts',(110.876984493608,25.3781228815631,42.7281463958668));
#109091=CARTESIAN_POINT('Ctrl Pts',(109.872441972793,25.3150974578757,43.1326280415791));
#109092=CARTESIAN_POINT('Ctrl Pts',(108.983103204413,25.2520720341883,42.5148566991937));
#109093=CARTESIAN_POINT('Ctrl Pts',(109.01160605001,25.1890466105009,41.4323254210439));
#109094=CARTESIAN_POINT('Ctrl Pts',(109.932270141825,25.1260211868136,40.8622081971757));
#109095=CARTESIAN_POINT('Ctrl Pts',(110.914061526536,25.0629957631262,41.3190781357284));
#109096=CARTESIAN_POINT('Ctrl Pts',(111.070804253555,24.9999703394388,42.3905673042213));
#109097=CARTESIAN_POINT('Ctrl Pts',(110.261013869551,24.9369449157514,43.1095198487837));
#109098=CARTESIAN_POINT('Ctrl Pts',(109.215627386155,24.873919492064,42.8269962858655));
#109099=CARTESIAN_POINT('Ctrl Pts',(108.878232530748,24.8108940683766,41.7980072213851));
#109100=CARTESIAN_POINT('Ctrl Pts',(109.553369864983,24.7478686446893,40.9513414976373));
#109101=CARTESIAN_POINT('Ctrl Pts',(110.631645311045,24.6848432210019,41.0512179272898));
#109102=CARTESIAN_POINT('Ctrl Pts',(111.139783830769,24.6218177973145,42.0074859940361));
#109103=CARTESIAN_POINT('Ctrl Pts',(110.619128350039,24.5587923736271,42.9569970145966));
#109104=CARTESIAN_POINT('Ctrl Pts',(109.539633998135,24.4957669499397,43.0427014703807));
#109105=CARTESIAN_POINT('Ctrl Pts',(108.875676129919,24.4327415262524,42.1872406130439));
#109106=CARTESIAN_POINT('Ctrl Pts',(109.22655774824,24.369716102565,41.1627722633822));
#109107=CARTESIAN_POINT('Ctrl Pts',(110.275565363628,24.3066906788776,40.8940040907134));
#109108=CARTESIAN_POINT('Ctrl Pts',(111.0758416321,24.2436652551902,41.6235322017735));
#109109=CARTESIAN_POINT('Ctrl Pts',(110.905039518748,24.1806398315029,42.6928683869158));
#109110=CARTESIAN_POINT('Ctrl Pts',(109.917328885343,24.1176144078154,43.1368064146927));
#109111=CARTESIAN_POINT('Ctrl Pts',(109.004238858492,24.0545889841281,42.5546377225252));
#109112=CARTESIAN_POINT('Ctrl Pts',(108.989945103632,23.9915635604407,41.4718412726584));
#109113=CARTESIAN_POINT('Ctrl Pts',(109.887348419636,23.9285381367533,40.8657715441766));
#109114=CARTESIAN_POINT('Ctrl Pts',(110.8864350456,23.8655127130659,41.2834834478755));
#109115=CARTESIAN_POINT('Ctrl Pts',(111.085402693489,23.8024872893785,42.347934639307));
#109116=CARTESIAN_POINT('Ctrl Pts',(110.304668689548,23.7394618656911,43.0983414849576));
#109117=CARTESIAN_POINT('Ctrl Pts',(109.248919863833,23.6764364420038,42.85734190533));
#109118=CARTESIAN_POINT('Ctrl Pts',(108.871142334862,23.6134110183164,41.8425271365074));
#109119=CARTESIAN_POINT('Ctrl Pts',(109.512233776159,23.550385594629,40.9697655185727));
#109120=CARTESIAN_POINT('Ctrl Pts',(110.593726400136,23.4873601709416,41.0270959680575));
#109121=CARTESIAN_POINT('Ctrl Pts',(111.139031344744,23.4243347472542,41.9622119492159));
#109122=CARTESIAN_POINT('Ctrl Pts',(110.656825811576,23.3613093235668,42.9322327657045));
#109123=CARTESIAN_POINT('Ctrl Pts',(109.580618341973,23.2982838998795,43.0590916680407));
#109124=CARTESIAN_POINT('Ctrl Pts',(109.1182113676,23.2562669507545,42.5087564544177));
#109125=CARTESIAN_POINT('Ctrl Pts',(109.053405877774,23.2352584761921,42.1963800658584));
#109126=CARTESIAN_POINT('Ctrl Pts',(109.032351030732,23.6222359168897,41.9993265593643));
#109127=CARTESIAN_POINT('Ctrl Pts',(109.031993297971,23.6192942840319,41.954767110875));
#109128=CARTESIAN_POINT('Ctrl Pts',(109.034808906072,23.6163526511741,41.9102527956804));
#109129=CARTESIAN_POINT('Ctrl Pts',(109.040953829907,23.6134110183164,41.8662026616554));
#109130=CARTESIAN_POINT('Ctrl Pts',(109.084839481961,23.5924025437539,41.5516065971958));
#109131=CARTESIAN_POINT('Ctrl Pts',(109.29853662906,23.5713940691915,41.2606860578843));
#109132=CARTESIAN_POINT('Ctrl Pts',(109.585633973272,23.550385594629,41.1247808631426));
#109133=CARTESIAN_POINT('Ctrl Pts',(109.872731317485,23.5293771200665,40.988875668401));
#109134=CARTESIAN_POINT('Ctrl Pts',(110.23322885881,23.5083686455041,41.0079858182292));
#109135=CARTESIAN_POINT('Ctrl Pts',(110.504361786908,23.4873601709416,41.1733935566698));
#109136=CARTESIAN_POINT('Ctrl Pts',(110.775494715005,23.4663516963791,41.3388012951103));
#109137=CARTESIAN_POINT('Ctrl Pts',(110.957263029875,23.4453432218167,41.6505066221631));
#109138=CARTESIAN_POINT('Ctrl Pts',(110.967779598448,23.4243347472542,41.9680294217709));
#109139=CARTESIAN_POINT('Ctrl Pts',(110.977388323116,23.4051398315028,42.2581420317798));
#109140=CARTESIAN_POINT('Ctrl Pts',(110.844035779942,23.3859449157514,42.5531110784096));
#109141=CARTESIAN_POINT('Ctrl Pts',(110.622830835844,23.36675,42.7413141620339));
#109142=CARTESIAN_POINT('',(109.570122622048,25.69325,41.3988956497206));
#109143=CARTESIAN_POINT('Ctrl Pts',(109.569185414382,25.69325,41.3981772519775));
#109144=CARTESIAN_POINT('Ctrl Pts',(109.550084409071,25.69325,41.4077923726575));
#109145=CARTESIAN_POINT('Ctrl Pts',(109.531472121902,25.69325,41.4182631075653));
#109146=CARTESIAN_POINT('Ctrl Pts',(109.513413199996,25.69325,41.4295739604689));
#109147=CARTESIAN_POINT('Ctrl Pts',(109.48521445685,25.69325,41.4472356922968));
#109148=CARTESIAN_POINT('Ctrl Pts',(109.45836378626,25.69325,41.4669432559766));
#109149=CARTESIAN_POINT('Ctrl Pts',(109.432922911696,25.69325,41.4884531863265));
#109150=CARTESIAN_POINT('Ctrl Pts',(109.425186378529,25.69325,41.4949943250419));
#109151=CARTESIAN_POINT('Ctrl Pts',(109.417580311137,25.69325,41.5017024633166));
#109152=CARTESIAN_POINT('Ctrl Pts',(109.410106732163,25.69325,41.5085715615065));
#109153=CARTESIAN_POINT('Ctrl Pts',(109.40357572132,25.69325,41.5145743287101));
#109154=CARTESIAN_POINT('Ctrl Pts',(109.397147155321,25.69325,41.5206990539363));
#109155=CARTESIAN_POINT('Ctrl Pts',(109.390830849284,25.69325,41.5269328221212));
#109156=CARTESIAN_POINT('Ctrl Pts',(109.365452869772,25.69325,41.5519791768034));
#109157=CARTESIAN_POINT('Ctrl Pts',(109.341846493619,25.69325,41.5788172817074));
#109158=CARTESIAN_POINT('Ctrl Pts',(109.320083986518,25.69325,41.6071642569862));
#109159=CARTESIAN_POINT('Ctrl Pts',(109.304156647206,25.69325,41.6279105750294));
#109160=CARTESIAN_POINT('Ctrl Pts',(109.289217175643,25.69325,41.6494663352333));
#109161=CARTESIAN_POINT('Ctrl Pts',(109.275301872763,25.69325,41.6717360185875));
#109162=CARTESIAN_POINT('Ctrl Pts',(109.270785129208,25.69325,41.6789644957281));
#109163=CARTESIAN_POINT('Ctrl Pts',(109.2663786605,25.69325,41.6862647740979));
#109164=CARTESIAN_POINT('Ctrl Pts',(109.262088219408,25.69325,41.6936250734435));
#109165=CARTESIAN_POINT('Ctrl Pts',(109.243070595941,25.69325,41.7262500177269));
#109166=CARTESIAN_POINT('Ctrl Pts',(109.226301260004,25.69325,41.7600968636462));
#109167=CARTESIAN_POINT('Ctrl Pts',(109.211859626931,25.69325,41.7948645052217));
#109168=CARTESIAN_POINT('Ctrl Pts',(109.197311505628,25.69325,41.8298885128565));
#109169=CARTESIAN_POINT('Ctrl Pts',(109.185124660238,25.69325,41.8658479950781));
#109170=CARTESIAN_POINT('Ctrl Pts',(109.175414211212,25.69325,41.9024762449533));
#109171=CARTESIAN_POINT('Ctrl Pts',(109.170221505687,25.69325,41.9220633634251));
#109172=CARTESIAN_POINT('Ctrl Pts',(109.16573761097,25.69325,41.9418423280385));
#109173=CARTESIAN_POINT('Ctrl Pts',(109.161985426801,25.69325,41.9617754774395));
#109174=CARTESIAN_POINT('Ctrl Pts',(109.160511365131,25.69325,41.9696063008185));
#109175=CARTESIAN_POINT('Ctrl Pts',(109.159150350403,25.69325,41.9774613586946));
#109176=CARTESIAN_POINT('Ctrl Pts',(109.157905961237,25.69325,41.9853230748385));
#109177=CARTESIAN_POINT('Ctrl Pts',(109.151489485606,25.69325,42.0258606425495));
#109178=CARTESIAN_POINT('Ctrl Pts',(109.148150748735,25.69325,42.0666685999508));
#109179=CARTESIAN_POINT('Ctrl Pts',(109.148004920988,25.69325,42.1074118288423));
#109180=CARTESIAN_POINT('Ctrl Pts',(109.14787042491,25.69325,42.1449890703042));
#109181=CARTESIAN_POINT('Ctrl Pts',(109.15045121736,25.69325,42.182512788659));
#109182=CARTESIAN_POINT('Ctrl Pts',(109.155573806821,25.69325,42.2197888984577));
#109183=CARTESIAN_POINT('Ctrl Pts',(109.157914090747,25.69325,42.2368186997458));
#109184=CARTESIAN_POINT('Ctrl Pts',(109.160785591051,25.69325,42.2537969833136));
#109185=CARTESIAN_POINT('Ctrl Pts',(109.164175193823,25.69325,42.2707056877841));
#109186=CARTESIAN_POINT('Ctrl Pts',(109.165814744614,25.69325,42.2788844277844));
#109187=CARTESIAN_POINT('Ctrl Pts',(109.167575544834,25.69325,42.2870468896487));
#109188=CARTESIAN_POINT('Ctrl Pts',(109.169456283132,25.69325,42.2951910247737));
#109189=CARTESIAN_POINT('Ctrl Pts',(109.171214441329,25.69325,42.3028043529732));
#109190=CARTESIAN_POINT('Ctrl Pts',(109.173076450049,25.69325,42.3103971639544));
#109191=CARTESIAN_POINT('Ctrl Pts',(109.175038653318,25.69325,42.3179598395574));
#109192=CARTESIAN_POINT('Ctrl Pts',(109.184977396073,25.69325,42.3562654975615));
#109193=CARTESIAN_POINT('Ctrl Pts',(109.197496367751,25.69325,42.3938584158793));
#109194=CARTESIAN_POINT('Ctrl Pts',(109.212387269368,25.69325,42.4305239662854));
#109195=CARTESIAN_POINT('Ctrl Pts',(109.227630572578,25.69325,42.4680572276404));
#109196=CARTESIAN_POINT('Ctrl Pts',(109.245359567467,25.69325,42.5046197943016));
#109197=CARTESIAN_POINT('Ctrl Pts',(109.265405320073,25.69325,42.5399845289048));
#109198=CARTESIAN_POINT('Ctrl Pts',(109.274853740721,25.69325,42.5566534410285));
#109199=CARTESIAN_POINT('Ctrl Pts',(109.284817619868,25.69325,42.573056179039));
#109200=CARTESIAN_POINT('Ctrl Pts',(109.295283129801,25.69325,42.5891680866639));
#109201=CARTESIAN_POINT('Ctrl Pts',(109.300676937784,25.69325,42.5974719855196));
#109202=CARTESIAN_POINT('Ctrl Pts',(109.306204030372,25.69325,42.6056986184729));
#109203=CARTESIAN_POINT('Ctrl Pts',(109.311862753256,25.69325,42.6138445007638));
#109204=CARTESIAN_POINT('Ctrl Pts',(109.316753006447,25.69325,42.6208841504675));
#109205=CARTESIAN_POINT('Ctrl Pts',(109.321736800868,25.69325,42.627856548227));
#109206=CARTESIAN_POINT('Ctrl Pts',(109.326809480733,25.69325,42.6347557588421));
#109207=CARTESIAN_POINT('Ctrl Pts',(109.351877367358,25.69325,42.6688498933249));
#109208=CARTESIAN_POINT('Ctrl Pts',(109.379133279473,25.69325,42.701188413472));
#109209=CARTESIAN_POINT('Ctrl Pts',(109.408381355878,25.69325,42.7315342256809));
#109210=CARTESIAN_POINT('Ctrl Pts',(109.437431291085,25.69325,42.7616744600759));
#109211=CARTESIAN_POINT('Ctrl Pts',(109.46844702927,25.69325,42.7898500743276));
#109212=CARTESIAN_POINT('Ctrl Pts',(109.501284033797,25.69325,42.8158120012212));
#109213=CARTESIAN_POINT('Ctrl Pts',(109.524887847922,25.69325,42.8344738890984));
#109214=CARTESIAN_POINT('Ctrl Pts',(109.549433713551,25.69325,42.8519916790737));
#109215=CARTESIAN_POINT('Ctrl Pts',(109.574880871485,25.69325,42.8682622236805));
#109216=CARTESIAN_POINT('Ctrl Pts',(109.569185414382,25.69325,41.3981772519775));
#109217=CARTESIAN_POINT('Ctrl Pts',(109.750509183194,25.6740550842486,41.2700703592373));
#109218=CARTESIAN_POINT('Ctrl Pts',(110.2609794001,25.6338516939347,41.1804260207118));
#109219=CARTESIAN_POINT('Ctrl Pts',(110.833061721015,25.5726398290584,41.7448763929315));
#109220=CARTESIAN_POINT('Ctrl Pts',(110.670381733412,25.509614405371,42.5566073819969));
#109221=CARTESIAN_POINT('Ctrl Pts',(109.902492493296,25.4465889816836,42.8657999717889));
#109222=CARTESIAN_POINT('Ctrl Pts',(109.341999413969,25.3946266601259,42.4764583909146));
#109223=CARTESIAN_POINT('Ctrl Pts',(109.261970584351,25.3636728131305,42.1159855729423));
#109224=CARTESIAN_POINT('Ctrl Pts',(109.262116416571,25.3537274406976,42.0001049160966));
#109225=CARTESIAN_POINT('Origin',(110.,25.69325,42.));
#109226=CARTESIAN_POINT('',(109.03325,25.69325,42.));
#109227=CARTESIAN_POINT('Origin',(110.,25.69325,42.));
#109228=CARTESIAN_POINT('Origin',(110.,25.69325,42.));
#109229=CARTESIAN_POINT('',(110.429877377952,25.69325,41.3988956497206));
#109230=CARTESIAN_POINT('Ctrl Pts',(110.426173582409,25.69325,42.8693912864046));
#109231=CARTESIAN_POINT('Ctrl Pts',(110.449419070301,25.69325,42.8546942308));
#109232=CARTESIAN_POINT('Ctrl Pts',(110.471950440779,25.69325,42.8389709957552));
#109233=CARTESIAN_POINT('Ctrl Pts',(110.493686951989,25.69325,42.822218891079));
#109234=CARTESIAN_POINT('Ctrl Pts',(110.523309759522,25.69325,42.7993888992837));
#109235=CARTESIAN_POINT('Ctrl Pts',(110.551457457952,25.69325,42.7746482345848));
#109236=CARTESIAN_POINT('Ctrl Pts',(110.578033597365,25.69325,42.74819223656));
#109237=CARTESIAN_POINT('Ctrl Pts',(110.589453845591,25.69325,42.7368236152635));
#109238=CARTESIAN_POINT('Ctrl Pts',(110.600583540201,25.69325,42.7251380560519));
#109239=CARTESIAN_POINT('Ctrl Pts',(110.611413359326,25.69325,42.7131504275406));
#109240=CARTESIAN_POINT('Ctrl Pts',(110.618757077373,25.69325,42.7050215970571));
#109241=CARTESIAN_POINT('Ctrl Pts',(110.625963742205,25.69325,42.6967525850163));
#109242=CARTESIAN_POINT('Ctrl Pts',(110.63301855821,25.69325,42.6883625609957));
#109243=CARTESIAN_POINT('Ctrl Pts',(110.659871269647,25.69325,42.6564276538559));
#109244=CARTESIAN_POINT('Ctrl Pts',(110.684569543192,25.69325,42.6226963939833));
#109245=CARTESIAN_POINT('Ctrl Pts',(110.706977156713,25.69325,42.5874443647455));
#109246=CARTESIAN_POINT('Ctrl Pts',(110.720032713102,25.69325,42.5669051468971));
#109247=CARTESIAN_POINT('Ctrl Pts',(110.732309766148,25.69325,42.5458492713409));
#109248=CARTESIAN_POINT('Ctrl Pts',(110.743773320964,25.69325,42.5243297266878));
#109249=CARTESIAN_POINT('Ctrl Pts',(110.748619502021,25.69325,42.5152324081565));
#109250=CARTESIAN_POINT('Ctrl Pts',(110.753320223074,25.69325,42.506052222641));
#109251=CARTESIAN_POINT('Ctrl Pts',(110.757872500094,25.69325,42.4967931874958));
#109252=CARTESIAN_POINT('Ctrl Pts',(110.761641280016,25.69325,42.4891277344492));
#109253=CARTESIAN_POINT('Ctrl Pts',(110.765304340218,25.69325,42.4814162803775));
#109254=CARTESIAN_POINT('Ctrl Pts',(110.768859833744,25.69325,42.4736630819417));
#109255=CARTESIAN_POINT('Ctrl Pts',(110.785576590795,25.69325,42.4372101018857));
#109256=CARTESIAN_POINT('Ctrl Pts',(110.799925999391,25.69325,42.3998216825895));
#109257=CARTESIAN_POINT('Ctrl Pts',(110.811780122533,25.69325,42.3617431637988));
#109258=CARTESIAN_POINT('Ctrl Pts',(110.82335859233,25.69325,42.3245501150637));
#109259=CARTESIAN_POINT('Ctrl Pts',(110.832556552458,25.69325,42.2866976047657));
#109260=CARTESIAN_POINT('Ctrl Pts',(110.839206606164,25.69325,42.2484166683166));
#109261=CARTESIAN_POINT('Ctrl Pts',(110.842457594823,25.69325,42.2297023998639));
#109262=CARTESIAN_POINT('Ctrl Pts',(110.845098911729,25.69325,42.2108858786613));
#109263=CARTESIAN_POINT('Ctrl Pts',(110.847106580664,25.69325,42.1919954630283));
#109264=CARTESIAN_POINT('Ctrl Pts',(110.847915830519,25.69325,42.1843811268934));
#109265=CARTESIAN_POINT('Ctrl Pts',(110.848622095913,25.69325,42.1767547989806));
#109266=CARTESIAN_POINT('Ctrl Pts',(110.849223668255,25.69325,42.169118399868));
#109267=CARTESIAN_POINT('Ctrl Pts',(110.84985403338,25.69325,42.1611165032625));
#109268=CARTESIAN_POINT('Ctrl Pts',(110.850368736194,25.69325,42.1531121018745));
#109269=CARTESIAN_POINT('Ctrl Pts',(110.850766396287,25.69325,42.1451108704563));
#109270=CARTESIAN_POINT('Ctrl Pts',(110.852611860866,25.69325,42.1079786829481));
#109271=CARTESIAN_POINT('Ctrl Pts',(110.851942434401,25.69325,42.0708885503444));
#109272=CARTESIAN_POINT('Ctrl Pts',(110.84862003613,25.69325,42.0340481470865));
#109273=CARTESIAN_POINT('Ctrl Pts',(110.845449780298,25.69325,41.9988947748077));
#109274=CARTESIAN_POINT('Ctrl Pts',(110.83986288333,25.69325,41.9639681123482));
#109275=CARTESIAN_POINT('Ctrl Pts',(110.831967424511,25.69325,41.9294671381188));
#109276=CARTESIAN_POINT('Ctrl Pts',(110.827876755529,25.69325,41.9115920445548));
#109277=CARTESIAN_POINT('Ctrl Pts',(110.823165875913,25.69325,41.8938315458871));
#109278=CARTESIAN_POINT('Ctrl Pts',(110.81784693204,25.69325,41.8762159653178));
#109279=CARTESIAN_POINT('Ctrl Pts',(110.815353851674,25.69325,41.8679592400915));
#109280=CARTESIAN_POINT('Ctrl Pts',(110.812727157518,25.69325,41.8597343826867));
#109281=CARTESIAN_POINT('Ctrl Pts',(110.809967980466,25.69325,41.8515446861299));
#109282=CARTESIAN_POINT('Ctrl Pts',(110.807564665586,25.69325,41.8444112477094));
#109283=CARTESIAN_POINT('Ctrl Pts',(110.805062231827,25.69325,41.8373088525883));
#109284=CARTESIAN_POINT('Ctrl Pts',(110.802464650691,25.69325,41.8302469111839));
#109285=CARTESIAN_POINT('Ctrl Pts',(110.789587578002,25.69325,41.795238521446));
#109286=CARTESIAN_POINT('Ctrl Pts',(110.774356602264,25.69325,41.7611648311545));
#109287=CARTESIAN_POINT('Ctrl Pts',(110.756916792691,25.69325,41.7282558485766));
#109288=CARTESIAN_POINT('Ctrl Pts',(110.739680949625,25.69325,41.6957317515235));
#109289=CARTESIAN_POINT('Ctrl Pts',(110.720286663262,25.69325,41.6643443970474));
#109290=CARTESIAN_POINT('Ctrl Pts',(110.698841475826,25.69325,41.6343542232482));
#109291=CARTESIAN_POINT('Ctrl Pts',(110.688967574082,25.69325,41.6205459956318));
#109292=CARTESIAN_POINT('Ctrl Pts',(110.678658532674,25.69325,41.6070345771449));
#109293=CARTESIAN_POINT('Ctrl Pts',(110.667923341888,25.69325,41.593848935211));
#109294=CARTESIAN_POINT('Ctrl Pts',(110.660962643681,25.69325,41.5852993643663));
#109295=CARTESIAN_POINT('Ctrl Pts',(110.653818546487,25.69325,41.5768823611315));
#109296=CARTESIAN_POINT('Ctrl Pts',(110.646516304445,25.69325,41.568631352059));
#109297=CARTESIAN_POINT('Ctrl Pts',(110.623108630693,25.69325,41.5421823618229));
#109298=CARTESIAN_POINT('Ctrl Pts',(110.598045622719,25.69325,41.5173919238667));
#109299=CARTESIAN_POINT('Ctrl Pts',(110.571435793576,25.69325,41.4944821051126));
#109300=CARTESIAN_POINT('Ctrl Pts',(110.545795023515,25.69325,41.4724066009192));
#109301=CARTESIAN_POINT('Ctrl Pts',(110.518717190311,25.69325,41.4520768475516));
#109302=CARTESIAN_POINT('Ctrl Pts',(110.490283536382,25.69325,41.433736275871));
#109303=CARTESIAN_POINT('Ctrl Pts',(110.470778285431,25.69325,41.421154795696));
#109304=CARTESIAN_POINT('Ctrl Pts',(110.450634687248,25.69325,41.4095103157974));
#109305=CARTESIAN_POINT('Ctrl Pts',(110.429877377952,25.69325,41.3988956497206));
#109306=CARTESIAN_POINT('Origin',(110.,25.69325,42.));
#109307=CARTESIAN_POINT('Origin',(110.,26.4327725593024,42.));
#109308=CARTESIAN_POINT('Ctrl Pts',(110.429877377952,25.69325,41.3988956497206));
#109309=CARTESIAN_POINT('Ctrl Pts',(110.628242021973,25.6722415254375,41.5407553335017));
#109310=CARTESIAN_POINT('Ctrl Pts',(110.870079721089,25.6302245763126,42.0341450801484));
#109311=CARTESIAN_POINT('Ctrl Pts',(110.448745988018,25.5671991526252,42.74735500798));
#109312=CARTESIAN_POINT('Ctrl Pts',(109.621520902912,25.5041737289379,42.7846640236677));
#109313=CARTESIAN_POINT('Ctrl Pts',(109.276538443787,25.4593648644969,42.3081202044508));
#109314=CARTESIAN_POINT('Ctrl Pts',(109.260025255512,25.4355644746184,42.0328501974113));
#109315=CARTESIAN_POINT('Ctrl Pts',(109.260278634324,25.4327725593024,42.0005281107854));
#109316=CARTESIAN_POINT('Ctrl Pts',(110.562359885163,25.824741523808,41.2136432603077));
#109317=CARTESIAN_POINT('Ctrl Pts',(110.821857881925,25.8037330492455,41.3992222174057));
#109318=CARTESIAN_POINT('Ctrl Pts',(111.138226752859,25.7617161001206,42.0446681410466));
#109319=CARTESIAN_POINT('Ctrl Pts',(110.587043550631,25.6986906764332,42.9776799106423));
#109320=CARTESIAN_POINT('Ctrl Pts',(109.504878664263,25.6356652527458,43.026487070204));
#109321=CARTESIAN_POINT('Ctrl Pts',(108.870105450825,25.5726398290584,42.1496388610647));
#109322=CARTESIAN_POINT('Ctrl Pts',(109.254965247123,25.509614405371,41.1373167601497));
#109323=CARTESIAN_POINT('Ctrl Pts',(110.312420586585,25.4465889816837,40.9038654413797));
#109324=CARTESIAN_POINT('Ctrl Pts',(111.087825583033,25.3835635579963,41.6597174172574));
#109325=CARTESIAN_POINT('Ctrl Pts',(110.881360229342,25.3205381343089,42.7227595686842));
#109326=CARTESIAN_POINT('Ctrl Pts',(109.879347874292,25.2575127106215,43.1334023191043));
#109327=CARTESIAN_POINT('Ctrl Pts',(108.986244409033,25.1944872869341,42.521021004801));
#109328=CARTESIAN_POINT('Ctrl Pts',(109.008176391962,25.1314618632468,41.4383499975927));
#109329=CARTESIAN_POINT('Ctrl Pts',(109.925351468358,25.0684364395594,40.8626388615017));
#109330=CARTESIAN_POINT('Ctrl Pts',(110.909905351887,25.005411015872,41.3135338816524));
#109331=CARTESIAN_POINT('Ctrl Pts',(111.073158915664,24.9423855921846,42.3840488332365));
#109332=CARTESIAN_POINT('Ctrl Pts',(110.267755477768,24.8793601684972,43.1079126153701));
#109333=CARTESIAN_POINT('Ctrl Pts',(109.220670114476,24.8163347448098,42.8317501890362));
#109334=CARTESIAN_POINT('Ctrl Pts',(108.877025034624,24.7533093211225,41.8048316749255));
#109335=CARTESIAN_POINT('Ctrl Pts',(109.547001899141,24.6902838974351,40.9540764141702));
#109336=CARTESIAN_POINT('Ctrl Pts',(110.625864816141,24.6272584737477,41.0473947979801));
#109337=CARTESIAN_POINT('Ctrl Pts',(111.13980837437,24.5642330500603,42.0005556202081));
#109338=CARTESIAN_POINT('Ctrl Pts',(110.624935792907,24.5012076263729,42.9532149188515));
#109339=CARTESIAN_POINT('Ctrl Pts',(109.545982411814,24.4381822026855,43.0454814573164));
#109340=CARTESIAN_POINT('Ctrl Pts',(108.876835288936,24.3751567789982,42.1940733862523));
#109341=CARTESIAN_POINT('Ctrl Pts',(109.221481392179,24.3121313553107,41.1674904586446));
#109342=CARTESIAN_POINT('Ctrl Pts',(110.268835473856,24.2491059316234,40.8923488579089));
#109343=CARTESIAN_POINT('Ctrl Pts',(111.073532860772,24.186080507936,41.6169978095687));
#109344=CARTESIAN_POINT('Ctrl Pts',(110.909235590793,24.1230550842486,42.6873524591346));
#109345=CARTESIAN_POINT('Ctrl Pts',(109.924242803773,24.0600296605612,43.1372887240647));
#109346=CARTESIAN_POINT('Ctrl Pts',(109.007628977691,23.9970042368738,42.5606808715683));
#109347=CARTESIAN_POINT('Ctrl Pts',(108.986753514865,23.9339788131865,41.4779949111826));
#109348=CARTESIAN_POINT('Ctrl Pts',(109.880451522268,23.8709533894991,40.8664721399706));
#109349=CARTESIAN_POINT('Ctrl Pts',(110.882067400023,23.8079279658117,41.2781178510068));
#109350=CARTESIAN_POINT('Ctrl Pts',(111.087487096344,23.7449025421243,42.3413054479614));
#109351=CARTESIAN_POINT('Ctrl Pts',(110.311364843364,23.6818771184369,43.0965177105864));
#109352=CARTESIAN_POINT('Ctrl Pts',(109.254096698422,23.6188516947495,42.8617898500753));
#109353=CARTESIAN_POINT('Ctrl Pts',(108.870308012805,23.5558262710622,41.8496109828972));
#109354=CARTESIAN_POINT('Ctrl Pts',(109.505739682273,23.4928008473748,40.9722914438752));
#109355=CARTESIAN_POINT('Ctrl Pts',(110.588140085362,23.4297754236874,41.0244762310742));
#109356=CARTESIAN_POINT('Ctrl Pts',(110.95355858955,23.3877584745625,41.643474631426));
#109357=CARTESIAN_POINT('Ctrl Pts',(110.966013043313,23.36675,41.9622592706773));
#109358=CARTESIAN_POINT('Ctrl Pts',(110.518199049426,25.780911015872,41.2753940567787));
#109359=CARTESIAN_POINT('Ctrl Pts',(110.757319261941,25.7599025413095,41.4463999227711));
#109360=CARTESIAN_POINT('Ctrl Pts',(111.048844408936,25.7178855921846,42.0411604540805));
#109361=CARTESIAN_POINT('Ctrl Pts',(110.540944363094,25.6548601684972,42.9009049430882));
#109362=CARTESIAN_POINT('Ctrl Pts',(109.54375941048,25.5918347448098,42.9458793880253));
#109363=CARTESIAN_POINT('Ctrl Pts',(108.958833485847,25.5288093211224,42.1378880635102));
#109364=CARTESIAN_POINT('Ctrl Pts',(109.313471122468,25.4657838974351,41.2050613021292));
#109365=CARTESIAN_POINT('Ctrl Pts',(110.287886912386,25.4027584737477,40.9899423815489));
#109366=CARTESIAN_POINT('Ctrl Pts',(111.002401127715,25.3397330500603,41.6864390302975));
#109367=CARTESIAN_POINT('Ctrl Pts',(110.81214902609,25.2767076263729,42.6660029126139));
#109368=CARTESIAN_POINT('Ctrl Pts',(109.888822409808,25.2136822026855,43.0443988269308));
#109369=CARTESIAN_POINT('Ctrl Pts',(109.065852317263,25.1506567789981,42.4801064168023));
#109370=CARTESIAN_POINT('Ctrl Pts',(109.086062031728,25.0876313553108,41.4824550878601));
#109371=CARTESIAN_POINT('Ctrl Pts',(109.931213446836,25.0246059316234,40.9519532307089));
#109372=CARTESIAN_POINT('Ctrl Pts',(110.838452565441,24.961580507936,41.3674404960662));
#109373=CARTESIAN_POINT('Ctrl Pts',(110.988886200194,24.8985550842486,42.353890356633));
#109374=CARTESIAN_POINT('Ctrl Pts',(110.246729252421,24.8355296605612,43.0209107713392));
#109375=CARTESIAN_POINT('Ctrl Pts',(109.281869108159,24.7725042368738,42.7664347487973));
#109376=CARTESIAN_POINT('Ctrl Pts',(108.965209690555,24.7094788131865,41.8201577971686));
#109377=CARTESIAN_POINT('Ctrl Pts',(109.582574804053,24.6464533894991,41.0362104014723));
#109378=CARTESIAN_POINT('Ctrl Pts',(110.576717083402,24.5834279658117,41.1222007060087));
#109379=CARTESIAN_POINT('Ctrl Pts',(111.050301829327,24.5204025421243,42.0005119886239));
#109380=CARTESIAN_POINT('Ctrl Pts',(110.575861014238,24.4573771184369,42.8783611311544));
#109381=CARTESIAN_POINT('Ctrl Pts',(109.581635374735,24.3943516947495,42.9633821893555));
#109382=CARTESIAN_POINT('Ctrl Pts',(108.965034845162,24.3313262710622,42.1788332470509));
#109383=CARTESIAN_POINT('Ctrl Pts',(109.282616678079,24.2683008473748,41.2328655290846));
#109384=CARTESIAN_POINT('Ctrl Pts',(110.247724438886,24.2052754236874,40.9793301690411));
#109385=CARTESIAN_POINT('Ctrl Pts',(110.989230780248,24.14225,41.6470740957064));
#109386=CARTESIAN_POINT('Ctrl Pts',(110.837835399153,24.0792245763126,42.6333762424057));
#109387=CARTESIAN_POINT('Ctrl Pts',(109.930191843146,24.0161991526253,43.0479800413974));
#109388=CARTESIAN_POINT('Ctrl Pts',(109.085557604648,23.9531737289379,42.5166518849293));
#109389=CARTESIAN_POINT('Ctrl Pts',(109.066321444178,23.8901483052505,41.5189867770486));
#109390=CARTESIAN_POINT('Ctrl Pts',(109.889839390833,23.8271228815631,40.9554854905858));
#109391=CARTESIAN_POINT('Ctrl Pts',(110.812800664274,23.7640974578757,41.3348056053153));
#109392=CARTESIAN_POINT('Ctrl Pts',(111.002089221612,23.7010720341883,42.3145035116548));
#109393=CARTESIAN_POINT('Ctrl Pts',(110.286914074266,23.638046610501,43.0104106823695));
#109394=CARTESIAN_POINT('Ctrl Pts',(109.31267077891,23.5750211868136,42.7941154639518));
#109395=CARTESIAN_POINT('Ctrl Pts',(108.959020141099,23.5119957631262,41.8614206884898));
#109396=CARTESIAN_POINT('Ctrl Pts',(109.544552814714,23.4489703394388,41.05299504655));
#109397=CARTESIAN_POINT('Ctrl Pts',(110.54195478946,23.3859449157514,41.1010818817501));
#109398=CARTESIAN_POINT('Ctrl Pts',(110.878677814179,23.3439279666265,41.6714717532923));
#109399=CARTESIAN_POINT('Ctrl Pts',(110.890154248169,23.322919492064,41.9652229638428));
#109400=CARTESIAN_POINT('Ctrl Pts',(110.474038213689,25.737080507936,41.3371448532496));
#109401=CARTESIAN_POINT('Ctrl Pts',(110.692780641957,25.7160720333735,41.4935776281364));
#109402=CARTESIAN_POINT('Ctrl Pts',(110.959462065013,25.6740550842486,42.0376527671144));
#109403=CARTESIAN_POINT('Ctrl Pts',(110.494845175556,25.6110296605612,42.8241299755341));
#109404=CARTESIAN_POINT('Ctrl Pts',(109.582640156696,25.5480042368739,42.8652717058465));
#109405=CARTESIAN_POINT('Ctrl Pts',(109.04756152087,25.4849788131864,42.1261372659557));
#109406=CARTESIAN_POINT('Ctrl Pts',(109.371976997812,25.4219533894991,41.2728058441086));
#109407=CARTESIAN_POINT('Ctrl Pts',(110.263353238187,25.3589279658117,41.0760193217181));
#109408=CARTESIAN_POINT('Ctrl Pts',(110.916976672397,25.2959025421243,41.7131606433377));
#109409=CARTESIAN_POINT('Ctrl Pts',(110.742937822837,25.2328771184369,42.6092462565436));
#109410=CARTESIAN_POINT('Ctrl Pts',(109.898296945324,25.1698516947496,42.9553953347574));
#109411=CARTESIAN_POINT('Ctrl Pts',(109.145460225492,25.1068262710622,42.4391918288035));
#109412=CARTESIAN_POINT('Ctrl Pts',(109.163947671494,25.0438008473748,41.5265601781276));
#109413=CARTESIAN_POINT('Ctrl Pts',(109.937075425314,24.9807754236874,41.041267599916));
#109414=CARTESIAN_POINT('Ctrl Pts',(110.766999778994,24.91775,41.42134711048));
#109415=CARTESIAN_POINT('Ctrl Pts',(110.904613484723,24.8547245763126,42.3237318800293));
#109416=CARTESIAN_POINT('Ctrl Pts',(110.225703027074,24.7916991526253,42.9339089273083));
#109417=CARTESIAN_POINT('Ctrl Pts',(109.343068101842,24.7286737289379,42.7011193085583));
#109418=CARTESIAN_POINT('Ctrl Pts',(109.053394346486,24.6656483052505,41.8354839194118));
#109419=CARTESIAN_POINT('Ctrl Pts',(109.618147708964,24.6026228815631,41.1183443887743));
#109420=CARTESIAN_POINT('Ctrl Pts',(110.527569350663,24.5395974578757,41.1970066140373));
#109421=CARTESIAN_POINT('Ctrl Pts',(110.960795284283,24.4765720341883,42.0004683570396));
#109422=CARTESIAN_POINT('Ctrl Pts',(110.526786235569,24.4135466105009,42.8035073434574));
#109423=CARTESIAN_POINT('Ctrl Pts',(109.617288337655,24.3505211868136,42.8812829213945));
#109424=CARTESIAN_POINT('Ctrl Pts',(109.053234401388,24.2874957631262,42.1635931078495));
#109425=CARTESIAN_POINT('Ctrl Pts',(109.343751963979,24.2244703394388,41.2982405995246));
#109426=CARTESIAN_POINT('Ctrl Pts',(110.226613403917,24.1614449157514,41.0663114801734));
#109427=CARTESIAN_POINT('Ctrl Pts',(110.904928699723,24.098419492064,41.677150381844));
#109428=CARTESIAN_POINT('Ctrl Pts',(110.766435207513,24.0353940683767,42.5794000256769));
#109429=CARTESIAN_POINT('Ctrl Pts',(109.936140882519,23.9723686446893,42.9586713587301));
#109430=CARTESIAN_POINT('Ctrl Pts',(109.163486231604,23.9093432210019,42.4726228982903));
#109431=CARTESIAN_POINT('Ctrl Pts',(109.145889373491,23.8463177973145,41.5599786429147));
#109432=CARTESIAN_POINT('Ctrl Pts',(109.899227259397,23.7832923736271,41.044498841201));
#109433=CARTESIAN_POINT('Ctrl Pts',(110.743533928526,23.7202669499398,41.3914933596238));
#109434=CARTESIAN_POINT('Ctrl Pts',(110.91669134688,23.6572415262523,42.2877015753482));
#109435=CARTESIAN_POINT('Ctrl Pts',(110.262463305168,23.594216102565,42.9243036541526));
#109436=CARTESIAN_POINT('Ctrl Pts',(109.371244859398,23.5311906788776,42.7264410778283));
#109437=CARTESIAN_POINT('Ctrl Pts',(109.047732269392,23.4681652551902,41.8732303940826));
#109438=CARTESIAN_POINT('Ctrl Pts',(109.583365947155,23.4051398315028,41.1336986492247));
#109439=CARTESIAN_POINT('Ctrl Pts',(110.495769493557,23.3421144078154,41.177687532426));
#109440=CARTESIAN_POINT('Ctrl Pts',(110.803797038808,23.3000974586905,41.6994688751586));
#109441=CARTESIAN_POINT('Ctrl Pts',(110.814295453026,23.2790889841281,41.9681866570083));
#109442=CARTESIAN_POINT('Ctrl Pts',(110.429877377952,25.69325,41.3988956497206));
#109443=CARTESIAN_POINT('Ctrl Pts',(110.628242021973,25.6722415254375,41.5407553335017));
#109444=CARTESIAN_POINT('Ctrl Pts',(110.870079721089,25.6302245763126,42.0341450801484));
#109445=CARTESIAN_POINT('Ctrl Pts',(110.448745988018,25.5671991526252,42.74735500798));
#109446=CARTESIAN_POINT('Ctrl Pts',(109.621520902912,25.5041737289379,42.7846640236677));
#109447=CARTESIAN_POINT('Ctrl Pts',(109.136289555893,25.4411483052505,42.1143864684012));
#109448=CARTESIAN_POINT('Ctrl Pts',(109.430482873156,25.3781228815631,41.3405503860881));
#109449=CARTESIAN_POINT('Ctrl Pts',(110.238819563989,25.3150974578757,41.1620962618873));
#109450=CARTESIAN_POINT('Ctrl Pts',(110.831552217079,25.2520720341883,41.7398822563778));
#109451=CARTESIAN_POINT('Ctrl Pts',(110.673726619585,25.1890466105009,42.5524896004734));
#109452=CARTESIAN_POINT('Ctrl Pts',(109.907771480839,25.1260211868136,42.866391842584));
#109453=CARTESIAN_POINT('Ctrl Pts',(109.225068133722,25.0629957631262,42.3982772408048));
#109454=CARTESIAN_POINT('Ctrl Pts',(109.24183331126,24.9999703394388,41.5706652683951));
#109455=CARTESIAN_POINT('Ctrl Pts',(109.942937403792,24.9369449157514,41.1305819691232));
#109456=CARTESIAN_POINT('Ctrl Pts',(110.695546992547,24.873919492064,41.4752537248938));
#109457=CARTESIAN_POINT('Ctrl Pts',(110.820340769253,24.8108940683766,42.2935734034257));
#109458=CARTESIAN_POINT('Ctrl Pts',(110.204676801728,24.7478686446893,42.8469070832775));
#109459=CARTESIAN_POINT('Ctrl Pts',(109.404267095524,24.6848432210019,42.6358038683194));
#109460=CARTESIAN_POINT('Ctrl Pts',(109.141579002417,24.6218177973145,41.850810041655));
#109461=CARTESIAN_POINT('Ctrl Pts',(109.653720613876,24.5587923736271,41.2004783760763));
#109462=CARTESIAN_POINT('Ctrl Pts',(110.478421617924,24.4957669499397,41.271812522066));
#109463=CARTESIAN_POINT('Ctrl Pts',(110.871288739239,24.4327415262524,42.0004247254552));
#109464=CARTESIAN_POINT('Ctrl Pts',(110.4777114569,24.369716102565,42.7286535557603));
#109465=CARTESIAN_POINT('Ctrl Pts',(109.652941300575,24.3066906788776,42.7991836534335));
#109466=CARTESIAN_POINT('Ctrl Pts',(109.141433957614,24.2436652551902,42.148352968648));
#109467=CARTESIAN_POINT('Ctrl Pts',(109.404887249879,24.1806398315028,41.3636156699646));
#109468=CARTESIAN_POINT('Ctrl Pts',(110.205502368947,24.1176144078154,41.1532927913056));
#109469=CARTESIAN_POINT('Ctrl Pts',(110.820626619199,24.0545889841281,41.7072266679816));
#109470=CARTESIAN_POINT('Ctrl Pts',(110.695035015874,23.9915635604407,42.525423808948));
#109471=CARTESIAN_POINT('Ctrl Pts',(109.942089921891,23.9285381367533,42.8693626760629));
#109472=CARTESIAN_POINT('Ctrl Pts',(109.241414858561,23.8655127130659,42.4285939116513));
#109473=CARTESIAN_POINT('Ctrl Pts',(109.225457302804,23.8024872893785,41.6009705087809));
#109474=CARTESIAN_POINT('Ctrl Pts',(109.908615127961,23.7394618656911,41.1335121918162));
#109475=CARTESIAN_POINT('Ctrl Pts',(110.674267192777,23.6764364420038,41.4481811139323));
#109476=CARTESIAN_POINT('Ctrl Pts',(110.831293472147,23.6134110183164,42.2608996390416));
#109477=CARTESIAN_POINT('Ctrl Pts',(110.23801253607,23.550385594629,42.8381966259357));
#109478=CARTESIAN_POINT('Ctrl Pts',(109.429818939885,23.4873601709416,42.6587666917049));
#109479=CARTESIAN_POINT('Ctrl Pts',(109.136444397686,23.4243347472542,41.8850400996752));
#109480=CARTESIAN_POINT('Ctrl Pts',(109.622179079596,23.3613093235668,41.2144022518994));
#109481=CARTESIAN_POINT('Ctrl Pts',(110.449584197655,23.2982838998795,41.254293183102));
#109482=CARTESIAN_POINT('Ctrl Pts',(110.728916263437,23.2562669507545,41.7274659970249));
#109483=CARTESIAN_POINT('Ctrl Pts',(110.738436657883,23.2352584761921,41.9711503501738));
#109484=CARTESIAN_POINT('Ctrl Pts',(110.966013043313,23.36675,41.9622592706773));
#109485=CARTESIAN_POINT('Ctrl Pts',(110.95355858955,23.3877584745625,41.643474631426));
#109486=CARTESIAN_POINT('Ctrl Pts',(110.770849337456,23.4087669491249,41.3339754312501));
#109487=CARTESIAN_POINT('Ctrl Pts',(110.499094644228,23.4297754236874,41.170528366629));
#109488=CARTESIAN_POINT('Ctrl Pts',(110.227339950999,23.4507838982499,41.0070813020079));
#109489=CARTESIAN_POINT('Ctrl Pts',(109.866539816636,23.4717923728123,40.9896863729416));
#109490=CARTESIAN_POINT('Ctrl Pts',(109.58023447121,23.4928008473748,41.1272088315787));
#109491=CARTESIAN_POINT('Ctrl Pts',(109.293929125784,23.5138093219372,41.2647312902159));
#109492=CARTESIAN_POINT('Ctrl Pts',(109.082118569294,23.5348177964997,41.5571711365565));
#109493=CARTESIAN_POINT('Ctrl Pts',(109.040178071986,23.5558262710622,41.8720875375898));
#109494=CARTESIAN_POINT('Ctrl Pts',(109.034563099285,23.5586388750782,41.9142483870906));
#109495=CARTESIAN_POINT('Ctrl Pts',(109.031992829932,23.5614514790943,41.9568121000603));
#109496=CARTESIAN_POINT('Ctrl Pts',(109.032328989546,23.5642640831103,41.9994138103573));
#109497=CARTESIAN_POINT('Origin',(110.,25.8,42.));
#109498=CARTESIAN_POINT('',(109.330384757729,25.9,42.));
#109499=CARTESIAN_POINT('Origin',(110.,25.9,42.));
#109500=CARTESIAN_POINT('',(109.480384757729,25.75,42.));
#109501=CARTESIAN_POINT('',(109.430384757729,25.8,42.));
#109502=CARTESIAN_POINT('',(109.543134871874,25.7,41.8913136141202));
#109503=CARTESIAN_POINT('Ctrl Pts',(109.543134871874,25.7,41.8913136141202));
#109504=CARTESIAN_POINT('Ctrl Pts',(109.513345646292,25.7170391114376,41.9429100663472));
#109505=CARTESIAN_POINT('Ctrl Pts',(109.480384757729,25.75,42.));
#109506=CARTESIAN_POINT('',(109.67744226472,25.7,41.6586863858798));
#109507=CARTESIAN_POINT('Origin',(110.,25.7,42.));
#109508=CARTESIAN_POINT('',(109.740192378865,25.75,41.55));
#109509=CARTESIAN_POINT('Ctrl Pts',(109.740192378865,25.75,41.55));
#109510=CARTESIAN_POINT('Ctrl Pts',(109.707231490302,25.7170391114376,41.6070899336529));
#109511=CARTESIAN_POINT('Ctrl Pts',(109.67744226472,25.7,41.6586863858798));
#109512=CARTESIAN_POINT('',(109.865692607155,25.7,41.55));
#109513=CARTESIAN_POINT('Ctrl Pts',(109.865692607155,25.7,41.55));
#109514=CARTESIAN_POINT('Ctrl Pts',(109.80611415599,25.7170391114376,41.55));
#109515=CARTESIAN_POINT('Ctrl Pts',(109.740192378865,25.75,41.55));
#109516=CARTESIAN_POINT('',(110.134307392845,25.7,41.55));
#109517=CARTESIAN_POINT('Origin',(110.,25.7,42.));
#109518=CARTESIAN_POINT('',(110.259807621135,25.75,41.55));
#109519=CARTESIAN_POINT('Ctrl Pts',(110.259807621135,25.75,41.55));
#109520=CARTESIAN_POINT('Ctrl Pts',(110.19388584401,25.7170391114376,41.55));
#109521=CARTESIAN_POINT('Ctrl Pts',(110.134307392845,25.7,41.55));
#109522=CARTESIAN_POINT('',(110.32255773528,25.7,41.6586863858798));
#109523=CARTESIAN_POINT('Ctrl Pts',(110.32255773528,25.7,41.6586863858798));
#109524=CARTESIAN_POINT('Ctrl Pts',(110.292768509698,25.7170391114376,41.6070899336528));
#109525=CARTESIAN_POINT('Ctrl Pts',(110.259807621135,25.75,41.55));
#109526=CARTESIAN_POINT('',(110.456865128126,25.7,41.8913136141202));
#109527=CARTESIAN_POINT('Origin',(110.,25.7,42.));
#109528=CARTESIAN_POINT('',(110.519615242271,25.75,42.));
#109529=CARTESIAN_POINT('Ctrl Pts',(110.519615242271,25.75,42.));
#109530=CARTESIAN_POINT('Ctrl Pts',(110.486654353708,25.7170391114376,41.9429100663472));
#109531=CARTESIAN_POINT('Ctrl Pts',(110.456865128126,25.7,41.8913136141202));
#109532=CARTESIAN_POINT('',(110.456865128126,25.7,42.1086863858798));
#109533=CARTESIAN_POINT('Ctrl Pts',(110.456865128126,25.7,42.1086863858798));
#109534=CARTESIAN_POINT('Ctrl Pts',(110.486654353708,25.7170391114376,42.0570899336529));
#109535=CARTESIAN_POINT('Ctrl Pts',(110.519615242271,25.75,42.));
#109536=CARTESIAN_POINT('',(110.32255773528,25.7,42.3413136141202));
#109537=CARTESIAN_POINT('Origin',(110.,25.7,42.));
#109538=CARTESIAN_POINT('',(110.259807621135,25.75,42.45));
#109539=CARTESIAN_POINT('Ctrl Pts',(110.259807621135,25.75,42.45));
#109540=CARTESIAN_POINT('Ctrl Pts',(110.292768509698,25.7170391114376,42.3929100663471));
#109541=CARTESIAN_POINT('Ctrl Pts',(110.32255773528,25.7,42.3413136141202));
#109542=CARTESIAN_POINT('',(110.134307392845,25.7,42.45));
#109543=CARTESIAN_POINT('Ctrl Pts',(110.134307392845,25.7,42.45));
#109544=CARTESIAN_POINT('Ctrl Pts',(110.19388584401,25.7170391114376,42.45));
#109545=CARTESIAN_POINT('Ctrl Pts',(110.259807621135,25.75,42.45));
#109546=CARTESIAN_POINT('',(109.865692607155,25.7,42.45));
#109547=CARTESIAN_POINT('Origin',(110.,25.7,42.));
#109548=CARTESIAN_POINT('',(109.740192378865,25.75,42.45));
#109549=CARTESIAN_POINT('Ctrl Pts',(109.740192378865,25.75,42.45));
#109550=CARTESIAN_POINT('Ctrl Pts',(109.80611415599,25.7170391114376,42.45));
#109551=CARTESIAN_POINT('Ctrl Pts',(109.865692607155,25.7,42.45));
#109552=CARTESIAN_POINT('',(109.67744226472,25.7,42.3413136141202));
#109553=CARTESIAN_POINT('Ctrl Pts',(109.67744226472,25.7,42.3413136141202));
#109554=CARTESIAN_POINT('Ctrl Pts',(109.707231490302,25.7170391114376,42.3929100663471));
#109555=CARTESIAN_POINT('Ctrl Pts',(109.740192378865,25.75,42.45));
#109556=CARTESIAN_POINT('',(109.543134871874,25.7,42.1086863858798));
#109557=CARTESIAN_POINT('Origin',(110.,25.7,42.));
#109558=CARTESIAN_POINT('Ctrl Pts',(109.480384757729,25.75,42.));
#109559=CARTESIAN_POINT('Ctrl Pts',(109.513345646292,25.7170391114376,42.0570899336528));
#109560=CARTESIAN_POINT('Ctrl Pts',(109.543134871874,25.7,42.1086863858798));
#109561=CARTESIAN_POINT('Origin',(110.,25.8,42.));
#109562=CARTESIAN_POINT('',(110.134307392845,25.9,41.55));
#109563=CARTESIAN_POINT('',(110.134307392845,25.8,41.55));
#109564=CARTESIAN_POINT('',(109.865692607155,25.9,41.55));
#109565=CARTESIAN_POINT('',(109.865692607155,25.8,41.55));
#109566=CARTESIAN_POINT('Origin',(110.,25.9,42.));
#109567=CARTESIAN_POINT('Origin',(110.,25.8,42.));
#109568=CARTESIAN_POINT('',(110.456865128126,25.9,41.8913136141202));
#109569=CARTESIAN_POINT('',(110.456865128126,25.8,41.8913136141202));
#109570=CARTESIAN_POINT('',(110.32255773528,25.9,41.6586863858798));
#109571=CARTESIAN_POINT('',(110.32255773528,25.8,41.6586863858798));
#109572=CARTESIAN_POINT('Origin',(110.,25.9,42.));
#109573=CARTESIAN_POINT('Origin',(110.,25.8,42.));
#109574=CARTESIAN_POINT('',(109.543134871874,25.9,41.8913136141202));
#109575=CARTESIAN_POINT('',(109.543134871874,25.8,41.8913136141202));
#109576=CARTESIAN_POINT('',(109.67744226472,25.9,41.6586863858798));
#109577=CARTESIAN_POINT('Origin',(110.,25.9,42.));
#109578=CARTESIAN_POINT('',(109.67744226472,25.8,41.6586863858798));
#109579=CARTESIAN_POINT('Origin',(110.,25.8,42.));
#109580=CARTESIAN_POINT('',(110.32255773528,25.9,42.3413136141202));
#109581=CARTESIAN_POINT('',(110.32255773528,25.8,42.3413136141202));
#109582=CARTESIAN_POINT('',(110.456865128126,25.9,42.1086863858798));
#109583=CARTESIAN_POINT('',(110.456865128126,25.8,42.1086863858798));
#109584=CARTESIAN_POINT('Origin',(110.,25.9,42.));
#109585=CARTESIAN_POINT('Origin',(110.,25.8,42.));
#109586=CARTESIAN_POINT('',(109.67744226472,25.9,42.3413136141202));
#109587=CARTESIAN_POINT('',(109.67744226472,25.8,42.3413136141202));
#109588=CARTESIAN_POINT('',(109.543134871874,25.9,42.1086863858798));
#109589=CARTESIAN_POINT('Origin',(110.,25.9,42.));
#109590=CARTESIAN_POINT('',(109.543134871874,25.8,42.1086863858798));
#109591=CARTESIAN_POINT('Origin',(110.,25.8,42.));
#109592=CARTESIAN_POINT('',(110.134307392845,25.9,42.45));
#109593=CARTESIAN_POINT('',(110.134307392845,25.8,42.45));
#109594=CARTESIAN_POINT('',(109.865692607155,25.9,42.45));
#109595=CARTESIAN_POINT('Origin',(110.,25.9,42.));
#109596=CARTESIAN_POINT('',(109.865692607155,25.8,42.45));
#109597=CARTESIAN_POINT('Origin',(110.519615242271,25.9,42.));
#109598=CARTESIAN_POINT('',(110.549663336987,25.9,41.947955173281));
#109599=CARTESIAN_POINT('',(110.519615242271,24.9,42.));
#109600=CARTESIAN_POINT('',(110.519615242271,25.9,42.));
#109601=CARTESIAN_POINT('',(110.259807621135,24.9,42.45));
#109602=CARTESIAN_POINT('',(110.519615242271,24.9,42.));
#109603=CARTESIAN_POINT('',(110.259807621135,25.9,42.45));
#109604=CARTESIAN_POINT('Origin',(110.259807621135,25.9,41.55));
#109605=CARTESIAN_POINT('',(110.419759526419,25.9,41.827044826719));
#109606=CARTESIAN_POINT('',(110.259807621135,24.9,41.55));
#109607=CARTESIAN_POINT('',(110.259807621135,25.9,41.55));
#109608=CARTESIAN_POINT('',(110.259807621135,24.9,41.55));
#109609=CARTESIAN_POINT('Origin',(109.740192378865,25.9,41.55));
#109610=CARTESIAN_POINT('',(110.250096189432,25.9,41.55));
#109611=CARTESIAN_POINT('',(109.740192378865,24.9,41.55));
#109612=CARTESIAN_POINT('',(109.740192378865,25.9,41.55));
#109613=CARTESIAN_POINT('',(109.740192378865,24.9,41.55));
#109614=CARTESIAN_POINT('Origin',(110.76,25.9,42.));
#109615=CARTESIAN_POINT('Origin',(110.76,25.9,42.));
#109616=CARTESIAN_POINT('Origin',(110.76,25.9,42.));
#109617=CARTESIAN_POINT('',(109.640336663013,25.9,41.722955173281));
#109618=CARTESIAN_POINT('Origin',(110.76,25.9,42.));
#109619=CARTESIAN_POINT('Origin',(110.76,25.9,42.));
#109620=CARTESIAN_POINT('',(109.770240473581,25.9,42.502044826719));
#109621=CARTESIAN_POINT('Origin',(110.76,25.9,42.));
#109622=CARTESIAN_POINT('',(110.509903810568,25.9,42.45));
#109623=CARTESIAN_POINT('Origin',(110.519615242271,24.9,42.));
#109624=CARTESIAN_POINT('',(109.480384757729,24.9,42.));
#109625=CARTESIAN_POINT('',(109.480384757729,24.9,42.));
#109626=CARTESIAN_POINT('Origin',(110.,24.9,42.));
#109627=CARTESIAN_POINT('Origin',(110.519615242271,24.9,42.));
#109628=CARTESIAN_POINT('Origin',(110.,24.9,42.));
#109629=CARTESIAN_POINT('Origin',(110.519615242271,24.9,42.));
#109630=CARTESIAN_POINT('Origin',(110.,24.9,42.));
#109631=CARTESIAN_POINT('Origin',(110.519615242271,24.9,42.));
#109632=CARTESIAN_POINT('Origin',(110.,24.9,42.));
#109633=CARTESIAN_POINT('Origin',(110.519615242271,24.9,42.));
#109634=CARTESIAN_POINT('',(109.740192378865,24.9,42.45));
#109635=CARTESIAN_POINT('',(110.259807621135,24.9,42.45));
#109636=CARTESIAN_POINT('Origin',(110.,24.9,42.));
#109637=CARTESIAN_POINT('Origin',(110.519615242271,24.9,42.));
#109638=CARTESIAN_POINT('',(109.740192378865,24.9,42.45));
#109639=CARTESIAN_POINT('Origin',(110.,24.9,42.));
#109640=CARTESIAN_POINT('Origin',(110.,24.9,42.));
#109641=CARTESIAN_POINT('',(110.,24.5877836638731,42.));
#109642=CARTESIAN_POINT('',(109.480384757729,24.9,42.));
#109643=CARTESIAN_POINT('Origin',(109.480384757729,25.9,42.));
#109644=CARTESIAN_POINT('',(109.480384757729,25.9,42.));
#109645=CARTESIAN_POINT('Origin',(109.740192378865,25.9,42.45));
#109646=CARTESIAN_POINT('',(109.740192378865,25.9,42.45));
#109647=CARTESIAN_POINT('Origin',(110.259807621135,25.9,42.45));
#109648=CARTESIAN_POINT('Origin',(110.76,25.9,42.));
#109649=CARTESIAN_POINT('',(109.24,25.9,42.));
#109650=CARTESIAN_POINT('Origin',(110.,25.9,42.));
#109651=CARTESIAN_POINT('Origin',(110.,25.78,42.));
#109652=CARTESIAN_POINT('',(109.12,25.78,42.));
#109653=CARTESIAN_POINT('Origin',(110.,24.53,42.));
#109654=CARTESIAN_POINT('Origin',(110.,23.36675,42.));
#109655=CARTESIAN_POINT('Origin',(110.,23.15,42.));
#109656=CARTESIAN_POINT('',(109.5,22.9,42.));
#109657=CARTESIAN_POINT('Origin',(110.,22.9,42.));
#109658=CARTESIAN_POINT('',(109.25,23.15,42.));
#109659=CARTESIAN_POINT('Origin',(110.,22.9,42.));
#109660=CARTESIAN_POINT('',(0.,0.,0.));
#109661=CARTESIAN_POINT('Origin',(101.5,10.2,47.3));
#109662=CARTESIAN_POINT('',(100.532241706852,10.2006700084922,45.9457359168897));
#109663=CARTESIAN_POINT('',(100.53250240679,10.200740851054,45.8877640831103));
#109664=CARTESIAN_POINT('',(100.53325,10.2,47.3));
#109665=CARTESIAN_POINT('',(101.925646819763,11.0688404025234,45.81675));
#109666=CARTESIAN_POINT('Ctrl Pts',(100.532241706852,10.2006700084922,45.9457359168897));
#109667=CARTESIAN_POINT('Ctrl Pts',(100.531939678106,10.2403060092119,45.9431182012074));
#109668=CARTESIAN_POINT('Ctrl Pts',(100.534165142082,10.2799067243431,45.940500485525));
#109669=CARTESIAN_POINT('Ctrl Pts',(100.539032731449,10.3191783203179,45.9378827698427));
#109670=CARTESIAN_POINT('Ctrl Pts',(100.578178545175,10.6350058202473,45.9168307453719));
#109671=CARTESIAN_POINT('Ctrl Pts',(100.788206315339,10.9295472277339,45.895778720901));
#109672=CARTESIAN_POINT('Ctrl Pts',(101.074083348808,11.0695984076775,45.8747266964301));
#109673=CARTESIAN_POINT('Ctrl Pts',(101.336515844848,11.1981641069922,45.8554011309534));
#109674=CARTESIAN_POINT('Ctrl Pts',(101.66286705885,11.1965397839927,45.8360755654767));
#109675=CARTESIAN_POINT('Ctrl Pts',(101.926174511012,11.0694185813664,45.81675));
#109676=CARTESIAN_POINT('',(101.074880871485,11.0682622236804,45.81675));
#109677=CARTESIAN_POINT('Origin',(101.5,10.2,45.81675));
#109678=CARTESIAN_POINT('Ctrl Pts',(101.074880871485,11.0682622236804,45.81675));
#109679=CARTESIAN_POINT('Ctrl Pts',(100.78776007547,10.9276819482162,45.8378020244709));
#109680=CARTESIAN_POINT('Ctrl Pts',(100.578312683887,10.6345304198673,45.8588540489418));
#109681=CARTESIAN_POINT('Ctrl Pts',(100.539273609597,10.3191833556862,45.8799060734127));
#109682=CARTESIAN_POINT('Ctrl Pts',(100.534416286971,10.2799472196416,45.8825254099786));
#109683=CARTESIAN_POINT('Ctrl Pts',(100.532197030409,10.2403674777756,45.8851447465444));
#109684=CARTESIAN_POINT('Ctrl Pts',(100.53250240679,10.200740851054,45.8877640831103));
#109685=CARTESIAN_POINT('Origin',(101.5,10.2,47.3));
#109686=CARTESIAN_POINT('',(100.534708414766,10.2002149330439,46.3457359168897));
#109687=CARTESIAN_POINT('',(100.534710545659,10.2002170964104,46.2877640831103));
#109688=CARTESIAN_POINT('',(100.53325,10.2,47.3));
#109689=CARTESIAN_POINT('Ctrl Pts',(100.534708414766,10.2002149330439,46.3457359168897));
#109690=CARTESIAN_POINT('Ctrl Pts',(100.534413669718,10.3471285850105,46.3360970146994));
#109691=CARTESIAN_POINT('Ctrl Pts',(100.565907422062,10.4939222620691,46.3264581125091));
#109692=CARTESIAN_POINT('Ctrl Pts',(100.629847246181,10.624873077704,46.3168192103187));
#109693=CARTESIAN_POINT('Ctrl Pts',(100.769496214025,10.9108786539404,46.2957671858479));
#109694=CARTESIAN_POINT('Ctrl Pts',(101.063918007077,11.1213113090886,46.274715161377));
#109695=CARTESIAN_POINT('Ctrl Pts',(101.379732776824,11.1608420226805,46.2536631369061));
#109696=CARTESIAN_POINT('Ctrl Pts',(101.695547546572,11.2003727362724,46.2326111124352));
#109697=CARTESIAN_POINT('Ctrl Pts',(102.032755293016,11.0690015083081,46.2115590879643));
#109698=CARTESIAN_POINT('Ctrl Pts',(102.238588515748,10.8262372585098,46.1905070634934));
#109699=CARTESIAN_POINT('Ctrl Pts',(102.444421738481,10.5834730087115,46.1694550390225));
#109700=CARTESIAN_POINT('Ctrl Pts',(102.518880437503,10.2293157370793,46.1484030145516));
#109701=CARTESIAN_POINT('Ctrl Pts',(102.42823895665,9.92422086028216,46.1273509900807));
#109702=CARTESIAN_POINT('Ctrl Pts',(102.337597475796,9.61912598348505,46.1062989656099));
#109703=CARTESIAN_POINT('Ctrl Pts',(102.081855815067,9.36309350152309,46.085246941139));
#109704=CARTESIAN_POINT('Ctrl Pts',(101.776859159505,9.27208769655593,46.0641949166681));
#109705=CARTESIAN_POINT('Ctrl Pts',(101.471862503943,9.18108189158877,46.0431428921972));
#109706=CARTESIAN_POINT('Ctrl Pts',(101.117610853547,9.2551027636164,46.0220908677263));
#109707=CARTESIAN_POINT('Ctrl Pts',(100.874616956993,9.46066999581634,46.0010388432554));
#109708=CARTESIAN_POINT('Ctrl Pts',(100.661838156121,9.64067595393337,45.9826045344668));
#109709=CARTESIAN_POINT('Ctrl Pts',(100.534368634238,9.92154791691139,45.9641702256782));
#109710=CARTESIAN_POINT('Ctrl Pts',(100.532241706852,10.2006700084922,45.9457359168897));
#109711=CARTESIAN_POINT('Ctrl Pts',(100.53250240679,10.200740851054,45.8877640831103));
#109712=CARTESIAN_POINT('Ctrl Pts',(100.534651388942,9.92188197793314,45.9061967710153));
#109713=CARTESIAN_POINT('Ctrl Pts',(100.661824251252,9.64070129142659,45.9246294589203));
#109714=CARTESIAN_POINT('Ctrl Pts',(100.874490524577,9.46060350281805,45.9430621468253));
#109715=CARTESIAN_POINT('Ctrl Pts',(101.117377270841,9.25491331414458,45.9641141712962));
#109716=CARTESIAN_POINT('Ctrl Pts',(101.471781520366,9.18107553681112,45.9851661957671));
#109717=CARTESIAN_POINT('Ctrl Pts',(101.776825995409,9.2721133102411,46.006218220238));
#109718=CARTESIAN_POINT('Ctrl Pts',(102.081870470452,9.36315108367107,46.0272702447089));
#109719=CARTESIAN_POINT('Ctrl Pts',(102.337555171014,9.61906440786449,46.0483222691798));
#109720=CARTESIAN_POINT('Ctrl Pts',(102.428200069675,9.92412653627793,46.0693742936507));
#109721=CARTESIAN_POINT('Ctrl Pts',(102.518844968337,10.2291886646914,46.0904263181216));
#109722=CARTESIAN_POINT('Ctrl Pts',(102.444450065097,10.5833995973248,46.1114783425924));
#109723=CARTESIAN_POINT('Ctrl Pts',(102.238644926451,10.8261920261445,46.1325303670633));
#109724=CARTESIAN_POINT('Ctrl Pts',(102.032839787805,11.0689844549642,46.1535823915342));
#109725=CARTESIAN_POINT('Ctrl Pts',(101.695624413753,11.2003583799702,46.1746344160051));
#109726=CARTESIAN_POINT('Ctrl Pts',(101.379802042979,11.1608458039451,46.195686440476));
#109727=CARTESIAN_POINT('Ctrl Pts',(101.063979672205,11.12133322792,46.2167384649469));
#109728=CARTESIAN_POINT('Ctrl Pts',(100.76955030471,10.910934150864,46.2377904894178));
#109729=CARTESIAN_POINT('Ctrl Pts',(100.629881698669,10.6249421244694,46.2588425138887));
#109730=CARTESIAN_POINT('Ctrl Pts',(100.565922129312,10.4939754930551,46.2684830369626));
#109731=CARTESIAN_POINT('Ctrl Pts',(100.534417015093,10.3471564714095,46.2781235600364));
#109732=CARTESIAN_POINT('Ctrl Pts',(100.534710545659,10.2002170964104,46.2877640831103));
#109733=CARTESIAN_POINT('Origin',(101.5,10.2,47.3));
#109734=CARTESIAN_POINT('',(100.532976005802,10.1991590825138,46.7457359168897));
#109735=CARTESIAN_POINT('',(100.532975287323,10.1991591673174,46.6877640831103));
#109736=CARTESIAN_POINT('',(100.53325,10.2,47.3));
#109737=CARTESIAN_POINT('Ctrl Pts',(100.532976005802,10.1991590825138,46.7457359168897));
#109738=CARTESIAN_POINT('Ctrl Pts',(100.535266693318,10.4519363514863,46.7290758281913));
#109739=CARTESIAN_POINT('Ctrl Pts',(100.63701805918,10.7063475805698,46.712415739493));
#109740=CARTESIAN_POINT('Ctrl Pts',(100.815067785654,10.8845077228383,46.6957556507947));
#109741=CARTESIAN_POINT('Ctrl Pts',(101.040055015112,11.1096344759239,46.6747036263238));
#109742=CARTESIAN_POINT('Ctrl Pts',(101.386870582805,11.2130083745455,46.653651601853));
#109743=CARTESIAN_POINT('Ctrl Pts',(101.698397381134,11.1477981944709,46.6325995773821));
#109744=CARTESIAN_POINT('Ctrl Pts',(102.009924179463,11.0825880143963,46.6115475529112));
#109745=CARTESIAN_POINT('Ctrl Pts',(102.286162208427,10.8487937556255,46.5904955284403));
#109746=CARTESIAN_POINT('Ctrl Pts',(102.401967899387,10.5523306652483,46.5694435039694));
#109747=CARTESIAN_POINT('Ctrl Pts',(102.517773590346,10.2558675748711,46.5483914794985));
#109748=CARTESIAN_POINT('Ctrl Pts',(102.473146943299,9.89673565288765,46.5273394550276));
#109749=CARTESIAN_POINT('Ctrl Pts',(102.288305150741,9.63763182842371,46.5062874305567));
#109750=CARTESIAN_POINT('Ctrl Pts',(102.103463358183,9.37852800395976,46.4852354060859));
#109751=CARTESIAN_POINT('Ctrl Pts',(101.778406420114,9.21945227701537,46.464183381615));
#109752=CARTESIAN_POINT('Ctrl Pts',(101.46039403625,9.23247007300103,46.4431313571441));
#109753=CARTESIAN_POINT('Ctrl Pts',(101.142381652385,9.24548786898669,46.4220793326731));
#109754=CARTESIAN_POINT('Ctrl Pts',(100.831413822726,9.43059918790241,46.4010273082023));
#109755=CARTESIAN_POINT('Ctrl Pts',(100.668367979214,9.70394409602264,46.3799752837314));
#109756=CARTESIAN_POINT('Ctrl Pts',(100.579974478061,9.85213501540243,46.3685621614508));
#109757=CARTESIAN_POINT('Ctrl Pts',(100.535057413148,10.0262590777531,46.3571490391703));
#109758=CARTESIAN_POINT('Ctrl Pts',(100.534708414766,10.2002149330439,46.3457359168897));
#109759=CARTESIAN_POINT('Ctrl Pts',(100.534710545659,10.2002170964104,46.2877640831103));
#109760=CARTESIAN_POINT('Ctrl Pts',(100.535057998223,10.0262847412647,46.2991755845073));
#109761=CARTESIAN_POINT('Ctrl Pts',(100.579960096027,9.85218375311567,46.3105870859043));
#109762=CARTESIAN_POINT('Ctrl Pts',(100.668329149821,9.7040063815298,46.3219985873014));
#109763=CARTESIAN_POINT('Ctrl Pts',(100.831353051604,9.43064764071791,46.3430506117722));
#109764=CARTESIAN_POINT('Ctrl Pts',(101.142308699758,9.24551513482726,46.3641026362431));
#109765=CARTESIAN_POINT('Ctrl Pts',(101.460320593408,9.23247371374772,46.385154660714));
#109766=CARTESIAN_POINT('Ctrl Pts',(101.778332487057,9.21943229266818,46.4062066851849));
#109767=CARTESIAN_POINT('Ctrl Pts',(102.103400626201,9.37848195639975,46.4272587096558));
#109768=CARTESIAN_POINT('Ctrl Pts',(102.288261961448,9.63757133787734,46.4483107341267));
#109769=CARTESIAN_POINT('Ctrl Pts',(102.473123296695,9.89666071935493,46.4693627585976));
#109770=CARTESIAN_POINT('Ctrl Pts',(102.517777828044,10.2557898185785,46.4904147830684));
#109771=CARTESIAN_POINT('Ctrl Pts',(102.401994901457,10.5522619030281,46.5114668075393));
#109772=CARTESIAN_POINT('Ctrl Pts',(102.28621197487,10.8487339874777,46.5325188320102));
#109773=CARTESIAN_POINT('Ctrl Pts',(102.009991590346,11.0825490571533,46.5535708564811));
#109774=CARTESIAN_POINT('Ctrl Pts',(101.698469721739,11.1477829573153,46.574622880952));
#109775=CARTESIAN_POINT('Ctrl Pts',(101.386947853131,11.2130168574774,46.5956749054229));
#109776=CARTESIAN_POINT('Ctrl Pts',(101.040124500441,11.109669588126,46.6167269298938));
#109777=CARTESIAN_POINT('Ctrl Pts',(100.815120106439,10.8845600595657,46.6377789543647));
#109778=CARTESIAN_POINT('Ctrl Pts',(100.637039472308,10.7063962162653,46.6544406639466));
#109779=CARTESIAN_POINT('Ctrl Pts',(100.535266170519,10.4519605571488,46.6711023735285));
#109780=CARTESIAN_POINT('Ctrl Pts',(100.532975287323,10.1991591673174,46.6877640831103));
#109781=CARTESIAN_POINT('Origin',(101.5,10.2,47.3));
#109782=CARTESIAN_POINT('',(100.532227115867,10.2006344259866,47.1457359168897));
#109783=CARTESIAN_POINT('',(100.532227739394,10.2006347153061,47.0877640831103));
#109784=CARTESIAN_POINT('',(100.53325,10.2,47.3));
#109785=CARTESIAN_POINT('Ctrl Pts',(100.532227115867,10.2006344259866,47.1457359168897));
#109786=CARTESIAN_POINT('Ctrl Pts',(100.531923761155,10.2404469978614,47.1431066661542));
#109787=CARTESIAN_POINT('Ctrl Pts',(100.53417029479,10.2802250774012,47.1404774154188));
#109788=CARTESIAN_POINT('Ctrl Pts',(100.539082845792,10.3196711352656,47.1378481646834));
#109789=CARTESIAN_POINT('Ctrl Pts',(100.578416920137,10.6355099269982,47.1167961402125));
#109790=CARTESIAN_POINT('Ctrl Pts',(100.788668560015,10.930062909731,47.0957441157416));
#109791=CARTESIAN_POINT('Ctrl Pts',(101.07458790823,11.0698893665793,47.0746920912707));
#109792=CARTESIAN_POINT('Ctrl Pts',(101.360507256445,11.2097158234276,47.0536400667998));
#109793=CARTESIAN_POINT('Ctrl Pts',(101.722094312998,11.1948157543913,47.032588042329));
#109794=CARTESIAN_POINT('Ctrl Pts',(101.995540056344,11.0319393067675,47.0115360178581));
#109795=CARTESIAN_POINT('Ctrl Pts',(102.268985799689,10.8690628591437,46.9904839933872));
#109796=CARTESIAN_POINT('Ctrl Pts',(102.454290229828,10.5582100329325,46.9694319689163));
#109797=CARTESIAN_POINT('Ctrl Pts',(102.467505271055,10.2402058276111,46.9483799444454));
#109798=CARTESIAN_POINT('Ctrl Pts',(102.480720312281,9.92220162228974,46.9273279199745));
#109799=CARTESIAN_POINT('Ctrl Pts',(102.321845964596,9.59704603785827,46.9062758955036));
#109800=CARTESIAN_POINT('Ctrl Pts',(102.06285673967,9.41204362497134,46.8852238710327));
#109801=CARTESIAN_POINT('Ctrl Pts',(101.803867514744,9.22704121208441,46.8641718465618));
#109802=CARTESIAN_POINT('Ctrl Pts',(101.444763412578,9.18219197074201,46.843119822091));
#109803=CARTESIAN_POINT('Ctrl Pts',(101.148228605385,9.29781385427975,46.8220677976201));
#109804=CARTESIAN_POINT('Ctrl Pts',(100.851693798192,9.41343573781747,46.8010157731492));
#109805=CARTESIAN_POINT('Ctrl Pts',(100.617728285971,9.68952874623533,46.7799637486783));
#109806=CARTESIAN_POINT('Ctrl Pts',(100.552324975472,10.0010150542191,46.7589117242074));
#109807=CARTESIAN_POINT('Ctrl Pts',(100.53868034289,10.0659982514689,46.7545197884348));
#109808=CARTESIAN_POINT('Ctrl Pts',(100.532372134321,10.1325218904679,46.7501278526622));
#109809=CARTESIAN_POINT('Ctrl Pts',(100.532976005802,10.1991590825138,46.7457359168897));
#109810=CARTESIAN_POINT('Ctrl Pts',(100.532975287323,10.1991591673174,46.6877640831103));
#109811=CARTESIAN_POINT('Ctrl Pts',(100.532371645869,10.1325466927522,46.6921543979993));
#109812=CARTESIAN_POINT('Ctrl Pts',(100.538675149134,10.0660476868242,46.6965447128883));
#109813=CARTESIAN_POINT('Ctrl Pts',(100.552309781337,10.0010874279596,46.7009350277773));
#109814=CARTESIAN_POINT('Ctrl Pts',(100.617689285549,9.68959611268303,46.7219870522482));
#109815=CARTESIAN_POINT('Ctrl Pts',(100.851633729287,9.41348526989917,46.7430390767191));
#109816=CARTESIAN_POINT('Ctrl Pts',(101.148159706116,9.29784074657613,46.76409110119));
#109817=CARTESIAN_POINT('Ctrl Pts',(101.444685682945,9.18219622325309,46.7851431256609));
#109818=CARTESIAN_POINT('Ctrl Pts',(101.803793192865,9.22701801939087,46.8061951501318));
#109819=CARTESIAN_POINT('Ctrl Pts',(102.06279654115,9.41200064288986,46.8272471746027));
#109820=CARTESIAN_POINT('Ctrl Pts',(102.321799889436,9.59698326638885,46.8482991990735));
#109821=CARTESIAN_POINT('Ctrl Pts',(102.480699076088,9.92212671724905,46.8693512235444));
#109822=CARTESIAN_POINT('Ctrl Pts',(102.467508326452,10.2401319283015,46.8904032480153));
#109823=CARTESIAN_POINT('Ctrl Pts',(102.454317576816,10.558137139354,46.9114552724862));
#109824=CARTESIAN_POINT('Ctrl Pts',(102.269036890894,10.8690041105988,46.9325072969571));
#109825=CARTESIAN_POINT('Ctrl Pts',(101.995603592515,11.0319014408845,46.953559321428));
#109826=CARTESIAN_POINT('Ctrl Pts',(101.722170294136,11.1947987711702,46.9746113458989));
#109827=CARTESIAN_POINT('Ctrl Pts',(101.360584383302,11.2097264604968,46.9956633703698));
#109828=CARTESIAN_POINT('Ctrl Pts',(101.074654360156,11.0699218457237,47.0167153948407));
#109829=CARTESIAN_POINT('Ctrl Pts',(100.78872433701,10.9301172309506,47.0377674193116));
#109830=CARTESIAN_POINT('Ctrl Pts',(100.578450201553,10.6355803120778,47.0588194437824));
#109831=CARTESIAN_POINT('Ctrl Pts',(100.539092003223,10.3197445300842,47.0798714682533));
#109832=CARTESIAN_POINT('Ctrl Pts',(100.534173408952,10.280274530595,47.0825023398723));
#109833=CARTESIAN_POINT('Ctrl Pts',(100.531924094728,10.2404718960613,47.0851332114913));
#109834=CARTESIAN_POINT('Ctrl Pts',(100.532227739394,10.2006347153061,47.0877640831103));
#109835=CARTESIAN_POINT('Origin',(101.5,10.2,47.3));
#109836=CARTESIAN_POINT('',(100.534709402463,10.2002118426407,47.5457359168897));
#109837=CARTESIAN_POINT('',(100.534709578762,10.2002114578675,47.4877640831103));
#109838=CARTESIAN_POINT('',(100.53325,10.2,47.3));
#109839=CARTESIAN_POINT('Ctrl Pts',(100.534709402463,10.2002118426407,47.5457359168897));
#109840=CARTESIAN_POINT('Ctrl Pts',(100.534418016928,10.3473016191035,47.5360854796462));
#109841=CARTESIAN_POINT('Ctrl Pts',(100.565990448616,10.4942727514434,47.5264350424028));
#109842=CARTESIAN_POINT('Ctrl Pts',(100.630078141595,10.6253456460443,47.5167846051594));
#109843=CARTESIAN_POINT('Ctrl Pts',(100.769882758406,10.9112756733585,47.4957325806885));
#109844=CARTESIAN_POINT('Ctrl Pts',(101.064419681572,11.1215498118811,47.4746805562176));
#109845=CARTESIAN_POINT('Ctrl Pts',(101.38025546817,11.1609080107844,47.4536285317467));
#109846=CARTESIAN_POINT('Ctrl Pts',(101.696091254768,11.2002662096876,47.4325765072758));
#109847=CARTESIAN_POINT('Ctrl Pts',(102.033225904797,11.0687084689717,47.4115244828049));
#109848=CARTESIAN_POINT('Ctrl Pts',(102.238928019467,10.8258341151079,47.390472458334));
#109849=CARTESIAN_POINT('Ctrl Pts',(102.444630134137,10.5829597612441,47.3694204338631));
#109850=CARTESIAN_POINT('Ctrl Pts',(102.518899713447,10.2287687942324,47.3483684093923));
#109851=CARTESIAN_POINT('Ctrl Pts',(102.428090566094,9.92371960069865,47.3273163849214));
#109852=CARTESIAN_POINT('Ctrl Pts',(102.337281418742,9.61867040716488,47.3062643604505));
#109853=CARTESIAN_POINT('Ctrl Pts',(102.081393544726,9.36276298710905,47.2852123359796));
#109854=CARTESIAN_POINT('Ctrl Pts',(101.776351288236,9.27193053958364,47.2641603115087));
#109855=CARTESIAN_POINT('Ctrl Pts',(101.471309031746,9.18109809205824,47.2431082870378));
#109856=CARTESIAN_POINT('Ctrl Pts',(101.117112392783,9.25534061706326,47.222056262567));
#109857=CARTESIAN_POINT('Ctrl Pts',(100.874222327708,9.46102417993194,47.2010042380961));
#109858=CARTESIAN_POINT('Ctrl Pts',(100.661667534337,9.64101930320724,47.1825814643606));
#109859=CARTESIAN_POINT('Ctrl Pts',(100.534352677778,9.92167358227858,47.1641586906251));
#109860=CARTESIAN_POINT('Ctrl Pts',(100.532227115867,10.2006344259866,47.1457359168897));
#109861=CARTESIAN_POINT('Ctrl Pts',(100.532227739394,10.2006347153061,47.0877640831103));
#109862=CARTESIAN_POINT('Ctrl Pts',(100.53435383508,9.92169795891722,47.1061852359622));
#109863=CARTESIAN_POINT('Ctrl Pts',(100.661643552647,9.64106750889965,47.1246063888141));
#109864=CARTESIAN_POINT('Ctrl Pts',(100.874165894016,9.46107199130515,47.143027541666));
#109865=CARTESIAN_POINT('Ctrl Pts',(101.117040244339,9.25536987963401,47.1640795661369));
#109866=CARTESIAN_POINT('Ctrl Pts',(101.471231206187,9.18110030140608,47.1851315906077));
#109867=CARTESIAN_POINT('Ctrl Pts',(101.776280395274,9.27190944743508,47.2061836150786));
#109868=CARTESIAN_POINT('Ctrl Pts',(102.081329584361,9.36271859346409,47.2272356395495));
#109869=CARTESIAN_POINT('Ctrl Pts',(102.337237000686,9.61860646375003,47.2482876640204));
#109870=CARTESIAN_POINT('Ctrl Pts',(102.428069446887,9.92364871579281,47.2693396884913));
#109871=CARTESIAN_POINT('Ctrl Pts',(102.518901893088,10.2286909678356,47.2903917129622));
#109872=CARTESIAN_POINT('Ctrl Pts',(102.444659369166,10.5828876016352,47.3114437374331));
#109873=CARTESIAN_POINT('Ctrl Pts',(102.238975809295,10.8257776631693,47.332495761904));
#109874=CARTESIAN_POINT('Ctrl Pts',(102.033292249425,11.0686677247035,47.3535477863749));
#109875=CARTESIAN_POINT('Ctrl Pts',(101.696167653607,11.2002512139721,47.3745998108458));
#109876=CARTESIAN_POINT('Ctrl Pts',(101.380328866479,11.1609171402,47.3956518353167));
#109877=CARTESIAN_POINT('Ctrl Pts',(101.06449007935,11.1215830664279,47.4167038597875));
#109878=CARTESIAN_POINT('Ctrl Pts',(100.769937100912,10.9113314296151,47.4377558842584));
#109879=CARTESIAN_POINT('Ctrl Pts',(100.630110646102,10.625412085568,47.4588079087293));
#109880=CARTESIAN_POINT('Ctrl Pts',(100.566002176563,10.4943220741444,47.4684599668563));
#109881=CARTESIAN_POINT('Ctrl Pts',(100.534418676151,10.3473259996625,47.4781120249833));
#109882=CARTESIAN_POINT('Ctrl Pts',(100.534709578762,10.2002114578675,47.4877640831103));
#109883=CARTESIAN_POINT('Origin',(101.5,10.2,47.3));
#109884=CARTESIAN_POINT('',(100.532970891558,10.1991597617674,47.9457359168897));
#109885=CARTESIAN_POINT('',(100.532970084924,10.1991597801972,47.8877640831103));
#109886=CARTESIAN_POINT('',(100.53325,10.2,47.3));
#109887=CARTESIAN_POINT('Ctrl Pts',(100.532970891558,10.1991597617674,47.9457359168897));
#109888=CARTESIAN_POINT('Ctrl Pts',(100.535262825522,10.4521085341167,47.9290642931383));
#109889=CARTESIAN_POINT('Ctrl Pts',(100.637170072234,10.7066933040064,47.9123926693868));
#109890=CARTESIAN_POINT('Ctrl Pts',(100.815439930465,10.8848799035489,47.8957210456354));
#109891=CARTESIAN_POINT('Ctrl Pts',(101.040549462316,11.1098843008339,47.8746690211645));
#109892=CARTESIAN_POINT('Ctrl Pts',(101.387421255122,11.2130697376435,47.8536169966936));
#109893=CARTESIAN_POINT('Ctrl Pts',(101.698912574935,11.1476902324763,47.8325649722227));
#109894=CARTESIAN_POINT('Ctrl Pts',(102.010403894747,11.0823107273092,47.8115129477518));
#109895=CARTESIAN_POINT('Ctrl Pts',(102.286514741566,10.8483662801652,47.7904609232809));
#109896=CARTESIAN_POINT('Ctrl Pts',(102.402159266578,10.5518402990146,47.76940889881));
#109897=CARTESIAN_POINT('Ctrl Pts',(102.517803791589,10.255314317864,47.7483568743392));
#109898=CARTESIAN_POINT('Ctrl Pts',(102.472981994793,9.89620680270677,47.7273048498683));
#109899=CARTESIAN_POINT('Ctrl Pts',(102.287999368596,9.63720345064479,47.7062528253974));
#109900=CARTESIAN_POINT('Ctrl Pts',(102.103016742399,9.37820009858282,47.6852008009265));
#109901=CARTESIAN_POINT('Ctrl Pts',(101.777873286802,9.21930090961613,47.6641487764556));
#109902=CARTESIAN_POINT('Ctrl Pts',(101.459868071114,9.23249165944427,47.6430967519847));
#109903=CARTESIAN_POINT('Ctrl Pts',(101.141862855427,9.24568240927242,47.6220447275138));
#109904=CARTESIAN_POINT('Ctrl Pts',(100.830995879649,9.43096309789541,47.6009927030429));
#109905=CARTESIAN_POINT('Ctrl Pts',(100.668098546988,9.70439640025984,47.579940678572));
#109906=CARTESIAN_POINT('Ctrl Pts',(100.579874815821,9.85248541906702,47.5685390913446));
#109907=CARTESIAN_POINT('Ctrl Pts',(100.535053662261,10.0264314351521,47.5571375041171));
#109908=CARTESIAN_POINT('Ctrl Pts',(100.534709402463,10.2002118426407,47.5457359168897));
#109909=CARTESIAN_POINT('Ctrl Pts',(100.534709578762,10.2002114578675,47.4877640831103));
#109910=CARTESIAN_POINT('Ctrl Pts',(100.53505316144,10.0264556844261,47.4991640494542));
#109911=CARTESIAN_POINT('Ctrl Pts',(100.579860827167,9.85253465171874,47.5105640157981));
#109912=CARTESIAN_POINT('Ctrl Pts',(100.668060705361,9.70445995088001,47.521963982142));
#109913=CARTESIAN_POINT('Ctrl Pts',(100.83093715061,9.43101421152056,47.5430160066129));
#109914=CARTESIAN_POINT('Ctrl Pts',(101.14178997229,9.24570978408305,47.5640680310838));
#109915=CARTESIAN_POINT('Ctrl Pts',(101.459794172975,9.23249474304927,47.5851200555547));
#109916=CARTESIAN_POINT('Ctrl Pts',(101.777798373661,9.21927970201549,47.6061720800255));
#109917=CARTESIAN_POINT('Ctrl Pts',(102.102953953352,9.37815404738542,47.6272241044964));
#109918=CARTESIAN_POINT('Ctrl Pts',(102.287956363542,9.63714326853569,47.6482761289673));
#109919=CARTESIAN_POINT('Ctrl Pts',(102.472958773732,9.89613248968595,47.6693281534382));
#109920=CARTESIAN_POINT('Ctrl Pts',(102.51780801442,10.2552365866165,47.6903801779091));
#109921=CARTESIAN_POINT('Ctrl Pts',(102.402186132568,10.5517713894869,47.71143220238));
#109922=CARTESIAN_POINT('Ctrl Pts',(102.286564250716,10.8483061923574,47.7324842268509));
#109923=CARTESIAN_POINT('Ctrl Pts',(102.010471246324,11.0822717011676,47.7535362513218));
#109924=CARTESIAN_POINT('Ctrl Pts',(101.698984942881,11.1476750107129,47.7745882757927));
#109925=CARTESIAN_POINT('Ctrl Pts',(101.387498639437,11.2130783202582,47.7956403002635));
#109926=CARTESIAN_POINT('Ctrl Pts',(101.040619036941,11.1099194305386,47.8166923247344));
#109927=CARTESIAN_POINT('Ctrl Pts',(100.815492287139,10.8849322043608,47.8377443492053));
#109928=CARTESIAN_POINT('Ctrl Pts',(100.637191460131,10.7067418803375,47.8544175938403));
#109929=CARTESIAN_POINT('Ctrl Pts',(100.535262192443,10.4521326485129,47.8710908384753));
#109930=CARTESIAN_POINT('Ctrl Pts',(100.532970084924,10.1991597801972,47.8877640831103));
#109931=CARTESIAN_POINT('Origin',(101.5,10.2,47.3));
#109932=CARTESIAN_POINT('',(100.532234232858,10.2006385183977,48.3457359168897));
#109933=CARTESIAN_POINT('',(100.532232424901,10.200636943667,48.2877640831103));
#109934=CARTESIAN_POINT('',(100.53325,10.2,47.3));
#109935=CARTESIAN_POINT('Ctrl Pts',(100.532234232858,10.2006385183977,48.3457359168897));
#109936=CARTESIAN_POINT('Ctrl Pts',(100.531930164216,10.240627217705,48.3430951311011));
#109937=CARTESIAN_POINT('Ctrl Pts',(100.534197686292,10.2805809022053,48.3404543453126));
#109938=CARTESIAN_POINT('Ctrl Pts',(100.539154181029,10.3201979585981,48.337813559524));
#109939=CARTESIAN_POINT('Ctrl Pts',(100.578666756778,10.6360203339923,48.3167615350531));
#109940=CARTESIAN_POINT('Ctrl Pts',(100.789065838849,10.930449706025,48.2957095105822));
#109941=CARTESIAN_POINT('Ctrl Pts',(101.075057869872,11.0701183141324,48.2746574861114));
#109942=CARTESIAN_POINT('Ctrl Pts',(101.361049900895,11.2097869222398,48.2536054616405));
#109943=CARTESIAN_POINT('Ctrl Pts',(101.722634880869,11.1946947664218,48.2325534371696));
#109944=CARTESIAN_POINT('Ctrl Pts',(101.995993625421,11.0316708622305,48.2115014126987));
#109945=CARTESIAN_POINT('Ctrl Pts',(102.269352369973,10.8686469580393,48.1904493882278));
#109946=CARTESIAN_POINT('Ctrl Pts',(102.454484879102,10.5576913054748,48.1693973637569));
#109947=CARTESIAN_POINT('Ctrl Pts',(102.467526300502,10.2396794072135,48.148345339286));
#109948=CARTESIAN_POINT('Ctrl Pts',(102.480567721901,9.92166750895226,48.1272933148151));
#109949=CARTESIAN_POINT('Ctrl Pts',(102.321518055569,9.59659936499427,48.1062412903442));
#109950=CARTESIAN_POINT('Ctrl Pts',(102.062428670247,9.41173802703683,48.0851892658734));
#109951=CARTESIAN_POINT('Ctrl Pts',(101.803339284925,9.22687668907938,48.0641372414025));
#109952=CARTESIAN_POINT('Ctrl Pts',(101.444210180611,9.18222215712248,48.0430852169316));
#109953=CARTESIAN_POINT('Ctrl Pts',(101.147738091875,9.29800508540701,48.0220331924607));
#109954=CARTESIAN_POINT('Ctrl Pts',(100.851266003139,9.41378801369153,48.0009811679898));
#109955=CARTESIAN_POINT('Ctrl Pts',(100.61745092998,9.69000840221748,47.9799291435189));
#109956=CARTESIAN_POINT('Ctrl Pts',(100.552217028849,10.0015302753606,47.958877119048));
#109957=CARTESIAN_POINT('Ctrl Pts',(100.538643482616,10.0663501998827,47.9544967183286));
#109958=CARTESIAN_POINT('Ctrl Pts',(100.532368695315,10.132698509948,47.9501163176091));
#109959=CARTESIAN_POINT('Ctrl Pts',(100.532970891558,10.1991597617674,47.9457359168897));
#109960=CARTESIAN_POINT('Ctrl Pts',(100.532970084924,10.1991597801972,47.8877640831103));
#109961=CARTESIAN_POINT('Ctrl Pts',(100.532368124453,10.1327232515517,47.8921428629462));
#109962=CARTESIAN_POINT('Ctrl Pts',(100.538638229879,10.0663995843913,47.8965216427821));
#109963=CARTESIAN_POINT('Ctrl Pts',(100.552201819349,10.0016026217589,47.900900422618));
#109964=CARTESIAN_POINT('Ctrl Pts',(100.61741199847,9.69007582797088,47.9219524470889));
#109965=CARTESIAN_POINT('Ctrl Pts',(100.851206253822,9.41383780303078,47.9430044715598));
#109966=CARTESIAN_POINT('Ctrl Pts',(101.147669339883,9.29803211376081,47.9640564960307));
#109967=CARTESIAN_POINT('Ctrl Pts',(101.444132425943,9.18222642449083,47.9851085205015));
#109968=CARTESIAN_POINT('Ctrl Pts',(101.803264342712,9.22685307089099,48.0061605449724));
#109969=CARTESIAN_POINT('Ctrl Pts',(102.062368163389,9.41169486075286,48.0272125694433));
#109970=CARTESIAN_POINT('Ctrl Pts',(102.321471984066,9.59653665061473,48.0482645939142));
#109971=CARTESIAN_POINT('Ctrl Pts',(102.480547708651,9.92159358393832,48.0693166183851));
#109972=CARTESIAN_POINT('Ctrl Pts',(102.467529912874,10.2396059631692,48.090368642856));
#109973=CARTESIAN_POINT('Ctrl Pts',(102.454512117097,10.5576183424,48.1114206673269));
#109974=CARTESIAN_POINT('Ctrl Pts',(102.269400800958,10.8685861675381,48.1324726917977));
#109975=CARTESIAN_POINT('Ctrl Pts',(101.996055896786,11.0316320086696,48.1535247162686));
#109976=CARTESIAN_POINT('Ctrl Pts',(101.722710992614,11.194677849801,48.1745767407395));
#109977=CARTESIAN_POINT('Ctrl Pts',(101.361132500409,11.2098017069258,48.1956287652104));
#109978=CARTESIAN_POINT('Ctrl Pts',(101.075126928412,11.0701527411221,48.2166807896813));
#109979=CARTESIAN_POINT('Ctrl Pts',(100.789121356414,10.9305037753184,48.2377328141522));
#109980=CARTESIAN_POINT('Ctrl Pts',(100.578688704624,10.6360819865862,48.2587848386231));
#109981=CARTESIAN_POINT('Ctrl Pts',(100.539157991476,10.3202672214402,48.279836863094));
#109982=CARTESIAN_POINT('Ctrl Pts',(100.534196177931,10.2806268037821,48.2824792697661));
#109983=CARTESIAN_POINT('Ctrl Pts',(100.531926882114,10.2406493450774,48.2851216764382));
#109984=CARTESIAN_POINT('Ctrl Pts',(100.532232424901,10.200636943667,48.2877640831103));
#109985=CARTESIAN_POINT('Origin',(101.5,10.2,47.3));
#109986=CARTESIAN_POINT('',(100.53325,10.2,48.71675));
#109987=CARTESIAN_POINT('',(100.534608987464,10.2001621159456,48.6877640831103));
#109988=CARTESIAN_POINT('',(100.53325,10.2,47.3));
#109989=CARTESIAN_POINT('',(100.631737776319,10.6251191285149,48.71675));
#109990=CARTESIAN_POINT('Origin',(101.5,10.2,48.71675));
#109991=CARTESIAN_POINT('Ctrl Pts',(100.631737776319,10.625119128515,48.71675));
#109992=CARTESIAN_POINT('Ctrl Pts',(100.772318051784,10.9122399245294,48.6956979755291));
#109993=CARTESIAN_POINT('Ctrl Pts',(101.065469648493,11.1216872926406,48.6746459510583));
#109994=CARTESIAN_POINT('Ctrl Pts',(101.38081672032,11.1607263666344,48.6535939265874));
#109995=CARTESIAN_POINT('Ctrl Pts',(101.696163792148,11.1997654406282,48.6325419021165));
#109996=CARTESIAN_POINT('Ctrl Pts',(102.033706339093,11.0683962205045,48.6114898776456));
#109997=CARTESIAN_POINT('Ctrl Pts',(102.239396511758,10.8255094805151,48.5904378531747));
#109998=CARTESIAN_POINT('Ctrl Pts',(102.445086684422,10.5826227405256,48.5693858287038));
#109999=CARTESIAN_POINT('Ctrl Pts',(102.518924482807,10.2282184806705,48.5483338042329));
#110000=CARTESIAN_POINT('Ctrl Pts',(102.427886711744,9.92317399947378,48.527281779762));
#110001=CARTESIAN_POINT('Ctrl Pts',(102.33684894068,9.61812951827702,48.5062297552911));
#110002=CARTESIAN_POINT('Ctrl Pts',(102.080935600168,9.36244481573861,48.4851777308203));
#110003=CARTESIAN_POINT('Ctrl Pts',(101.775873464374,9.2717999165515,48.4641257063494));
#110004=CARTESIAN_POINT('Ctrl Pts',(101.47081132858,9.18115501736439,48.4430736818785));
#110005=CARTESIAN_POINT('Ctrl Pts',(101.116600397504,9.25554992152858,48.4220216574076));
#110006=CARTESIAN_POINT('Ctrl Pts',(100.873807966679,9.46135506298848,48.4009696329367));
#110007=CARTESIAN_POINT('Ctrl Pts',(100.661471647179,9.64134381355782,48.3825583942544));
#110008=CARTESIAN_POINT('Ctrl Pts',(100.534354162604,9.92184215000783,48.364147155572));
#110009=CARTESIAN_POINT('Ctrl Pts',(100.532234232858,10.2006385183977,48.3457359168897));
#110010=CARTESIAN_POINT('Ctrl Pts',(100.532232424901,10.200636943667,48.2877640831103));
#110011=CARTESIAN_POINT('Ctrl Pts',(100.534361138091,9.92187098952785,48.3061737009091));
#110012=CARTESIAN_POINT('Ctrl Pts',(100.661469771119,9.64140895371578,48.3245833187079));
#110013=CARTESIAN_POINT('Ctrl Pts',(100.873762750332,9.46141149499328,48.3429929365066));
#110014=CARTESIAN_POINT('Ctrl Pts',(101.116526996838,9.25557827525217,48.3640449609775));
#110015=CARTESIAN_POINT('Ctrl Pts',(101.470684264354,9.18111957732977,48.3850969854484));
#110016=CARTESIAN_POINT('Ctrl Pts',(101.775779136246,9.27176105690851,48.4061490099193));
#110017=CARTESIAN_POINT('Ctrl Pts',(102.080874008138,9.36240253648726,48.4272010343902));
#110018=CARTESIAN_POINT('Ctrl Pts',(102.336906484406,9.61814419356716,48.4482530588611));
#110019=CARTESIAN_POINT('Ctrl Pts',(102.427912288884,9.92314084452664,48.469305083332));
#110020=CARTESIAN_POINT('Ctrl Pts',(102.518918093362,10.2281374954861,48.4903571078029));
#110021=CARTESIAN_POINT('Ctrl Pts',(102.444897226051,10.5823891403252,48.5114091322738));
#110022=CARTESIAN_POINT('Ctrl Pts',(102.239329995365,10.8253830337739,48.5324611567446));
#110023=CARTESIAN_POINT('Ctrl Pts',(102.033762764679,11.0683769272226,48.5535131812155));
#110024=CARTESIAN_POINT('Ctrl Pts',(101.696649170618,11.2001130692809,48.5745652056864));
#110025=CARTESIAN_POINT('Ctrl Pts',(101.380821678055,11.1609672548583,48.5956172301573));
#110026=CARTESIAN_POINT('Ctrl Pts',(101.064994185492,11.1218214404357,48.6166692546282));
#110027=CARTESIAN_POINT('Ctrl Pts',(100.770452794427,10.9117936695321,48.6377212790991));
#110028=CARTESIAN_POINT('Ctrl Pts',(100.630401613163,10.625916642522,48.65877330357));
#110029=CARTESIAN_POINT('Ctrl Pts',(100.566113371337,10.4946893920317,48.6684368967501));
#110030=CARTESIAN_POINT('Ctrl Pts',(100.534378091261,10.3474797829438,48.6781004899302));
#110031=CARTESIAN_POINT('Ctrl Pts',(100.534608987464,10.2001621159456,48.6877640831103));
#110032=CARTESIAN_POINT('Origin',(101.5,10.2,45.0772274406976));
#110033=CARTESIAN_POINT('',(100.76022353047,10.200488094229,48.4772274406976));
#110034=CARTESIAN_POINT('',(100.762038832931,10.2001239241621,48.5562725593024));
#110035=CARTESIAN_POINT('',(100.761,10.2,45.0772274406976));
#110036=CARTESIAN_POINT('',(102.101843294079,10.6308187385845,48.71675));
#110037=CARTESIAN_POINT('Ctrl Pts',(100.76022353047,10.200488094229,48.4772274406976));
#110038=CARTESIAN_POINT('Ctrl Pts',(100.761844040511,9.98737144955342,48.49563867938));
#110039=CARTESIAN_POINT('Ctrl Pts',(100.970123064239,9.52778148937982,48.5351019425332));
#110040=CARTESIAN_POINT('Ctrl Pts',(101.748452495356,9.36430899783289,48.5956172301573));
#110041=CARTESIAN_POINT('Ctrl Pts',(102.319282912332,9.93462942377178,48.6570468445758));
#110042=CARTESIAN_POINT('Ctrl Pts',(102.23085022002,10.4483024050457,48.6974244345233));
#110043=CARTESIAN_POINT('Ctrl Pts',(102.101843294079,10.6308187385845,48.71675));
#110044=CARTESIAN_POINT('',(102.101104350279,9.77012262204777,48.71675));
#110045=CARTESIAN_POINT('Origin',(101.5,10.2,48.71675));
#110046=CARTESIAN_POINT('Ctrl Pts',(100.762038832931,10.2001239241621,48.5562725593024));
#110047=CARTESIAN_POINT('Ctrl Pts',(100.762246837233,10.0674118742565,48.5676609905932));
#110048=CARTESIAN_POINT('Ctrl Pts',(100.859509971121,9.68904888221577,48.6001014463548));
#110049=CARTESIAN_POINT('Ctrl Pts',(101.464139111132,9.32935204372765,48.6535939265874));
#110050=CARTESIAN_POINT('Ctrl Pts',(101.958950595826,9.57134677434548,48.6956979755291));
#110051=CARTESIAN_POINT('Ctrl Pts',(102.101104350279,9.77012262204778,48.71675));
#110052=CARTESIAN_POINT('Origin',(101.5,10.2,45.0772274406976));
#110053=CARTESIAN_POINT('',(100.760786644801,10.199357707728,48.0772274406976));
#110054=CARTESIAN_POINT('',(100.760222148438,10.2004868904783,48.1562725593024));
#110055=CARTESIAN_POINT('',(100.761,10.2,45.0772274406976));
#110056=CARTESIAN_POINT('Ctrl Pts',(100.760786644801,10.199357707728,48.0772274406976));
#110057=CARTESIAN_POINT('Ctrl Pts',(100.76032631584,10.1485536062597,48.0816078414171));
#110058=CARTESIAN_POINT('Ctrl Pts',(100.788174905153,9.85408835187024,48.1070402666074));
#110059=CARTESIAN_POINT('Ctrl Pts',(101.182828978934,9.38785877941283,48.1535247162687));
#110060=CARTESIAN_POINT('Ctrl Pts',(102.006402006358,9.49026281080507,48.2166807896812));
#110061=CARTESIAN_POINT('Ctrl Pts',(102.371142746215,10.2357255210765,48.279836863094));
#110062=CARTESIAN_POINT('Ctrl Pts',(101.946587511935,10.9488247522485,48.3429929365066));
#110063=CARTESIAN_POINT('Ctrl Pts',(101.117382546223,10.9834348473594,48.4061490099193));
#110064=CARTESIAN_POINT('Ctrl Pts',(100.775542341,10.5050687063655,48.4508938446496));
#110065=CARTESIAN_POINT('Ctrl Pts',(100.759991095274,10.2310561302136,48.474586654909));
#110066=CARTESIAN_POINT('Ctrl Pts',(100.76022353047,10.200488094229,48.4772274406976));
#110067=CARTESIAN_POINT('Ctrl Pts',(100.760222148438,10.2004868904783,48.1562725593024));
#110068=CARTESIAN_POINT('Ctrl Pts',(100.761849372691,9.98739349496877,48.1746821771012));
#110069=CARTESIAN_POINT('Ctrl Pts',(100.970123675266,9.5278414290224,48.2141438193708));
#110070=CARTESIAN_POINT('Ctrl Pts',(101.74831434399,9.3642331418485,48.2746574861114));
#110071=CARTESIAN_POINT('Ctrl Pts',(102.335460969162,9.95071284574935,48.337813559524));
#110072=CARTESIAN_POINT('Ctrl Pts',(102.165712572132,10.7631006363966,48.4009696329368));
#110073=CARTESIAN_POINT('Ctrl Pts',(101.392626626404,11.065204620822,48.4641257063493));
#110074=CARTESIAN_POINT('Ctrl Pts',(100.838969225623,10.6704097524001,48.5158933484713));
#110075=CARTESIAN_POINT('Ctrl Pts',(100.76186233198,10.3127360326821,48.5466089661223));
#110076=CARTESIAN_POINT('Ctrl Pts',(100.762038832931,10.2001239241621,48.5562725593024));
#110077=CARTESIAN_POINT('Origin',(101.5,10.2,45.0772274406976));
#110078=CARTESIAN_POINT('',(100.762115591849,10.2001619360863,47.6772274406976));
#110079=CARTESIAN_POINT('',(100.760786028196,10.1993577218161,47.7562725593024));
#110080=CARTESIAN_POINT('',(100.761,10.2,45.0772274406976));
#110081=CARTESIAN_POINT('Ctrl Pts',(100.762115591849,10.2001619360863,47.6772274406976));
#110082=CARTESIAN_POINT('Ctrl Pts',(100.762378749843,10.0673212625574,47.6886290279251));
#110083=CARTESIAN_POINT('Ctrl Pts',(100.859902638249,9.68884167169019,47.7210826396234));
#110084=CARTESIAN_POINT('Ctrl Pts',(101.463865885969,9.32887186093604,47.7745882757927));
#110085=CARTESIAN_POINT('Ctrl Pts',(102.209501304701,9.69326751848885,47.8377443492053));
#110086=CARTESIAN_POINT('Ctrl Pts',(102.312288916283,10.5167910365686,47.900900422618));
#110087=CARTESIAN_POINT('Ctrl Pts',(101.679097556161,11.0532842761012,47.9640564960306));
#110088=CARTESIAN_POINT('Ctrl Pts',(100.9388056778,10.8330664826122,48.0228321687239));
#110089=CARTESIAN_POINT('Ctrl Pts',(100.762538637766,10.3927160141838,48.0605558169462));
#110090=CARTESIAN_POINT('Ctrl Pts',(100.760786644801,10.199357707728,48.0772274406976));
#110091=CARTESIAN_POINT('Ctrl Pts',(100.760786028196,10.1993577218161,47.7562725593024));
#110092=CARTESIAN_POINT('Ctrl Pts',(100.760325879463,10.1485725191587,47.7606513391383));
#110093=CARTESIAN_POINT('Ctrl Pts',(100.788162216564,9.8541264402612,47.7860821434451));
#110094=CARTESIAN_POINT('Ctrl Pts',(101.182767392066,9.3878833576509,47.8325649722227));
#110095=CARTESIAN_POINT('Ctrl Pts',(102.006346869156,9.49022344047391,47.8957210456354));
#110096=CARTESIAN_POINT('Ctrl Pts',(102.371147367118,10.2356604419514,47.958877119048));
#110097=CARTESIAN_POINT('Ctrl Pts',(101.946640733675,10.9487875878849,48.0220331924607));
#110098=CARTESIAN_POINT('Ctrl Pts',(101.117450646044,10.9834703820361,48.0851892658734));
#110099=CARTESIAN_POINT('Ctrl Pts',(100.775543514179,10.5050992334164,48.1299357214873));
#110100=CARTESIAN_POINT('Ctrl Pts',(100.759988586379,10.2310730447501,48.1536301526303));
#110101=CARTESIAN_POINT('Ctrl Pts',(100.760222148438,10.2004868904783,48.1562725593024));
#110102=CARTESIAN_POINT('Origin',(101.5,10.2,45.0772274406976));
#110103=CARTESIAN_POINT('',(100.760218090122,10.2004849659209,47.2772274406976));
#110104=CARTESIAN_POINT('',(100.762115726615,10.2001616419592,47.3562725593024));
#110105=CARTESIAN_POINT('',(100.761,10.2,45.0772274406976));
#110106=CARTESIAN_POINT('Ctrl Pts',(100.760218090122,10.2004849659209,47.2772274406976));
#110107=CARTESIAN_POINT('Ctrl Pts',(100.761842905485,9.98724259353902,47.2956502144331));
#110108=CARTESIAN_POINT('Ctrl Pts',(100.970375642338,9.52755072013085,47.3351250126394));
#110109=CARTESIAN_POINT('Ctrl Pts',(101.748822022916,9.36438196436754,47.3956518353166));
#110110=CARTESIAN_POINT('Ctrl Pts',(102.335637038891,9.95124180430941,47.4588079087293));
#110111=CARTESIAN_POINT('Ctrl Pts',(102.165318282924,10.7634904454937,47.521963982142));
#110112=CARTESIAN_POINT('Ctrl Pts',(101.392184050584,11.0651853109369,47.5851200555546));
#110113=CARTESIAN_POINT('Ctrl Pts',(100.838675749468,10.670027787286,47.6368745417399));
#110114=CARTESIAN_POINT('Ctrl Pts',(100.761892851834,10.3125998412386,47.6675770034542));
#110115=CARTESIAN_POINT('Ctrl Pts',(100.762115591849,10.2001619360863,47.6772274406976));
#110116=CARTESIAN_POINT('Ctrl Pts',(100.762115726615,10.2001616419592,47.3562725593024));
#110117=CARTESIAN_POINT('Ctrl Pts',(100.762378367007,10.0673397991113,47.3676725256463));
#110118=CARTESIAN_POINT('Ctrl Pts',(100.859881900044,9.68887966549334,47.400124516461));
#110119=CARTESIAN_POINT('Ctrl Pts',(101.463799353238,9.32887464035278,47.4536285317467));
#110120=CARTESIAN_POINT('Ctrl Pts',(102.209462575557,9.69321332531287,47.5167846051594));
#110121=CARTESIAN_POINT('Ctrl Pts',(102.31231312286,10.5167290045424,47.579940678572));
#110122=CARTESIAN_POINT('Ctrl Pts',(101.679162679895,11.0532705437534,47.6430967519847));
#110123=CARTESIAN_POINT('Ctrl Pts',(100.93883371831,10.8331033354341,47.7018740455615));
#110124=CARTESIAN_POINT('Ctrl Pts',(100.76253815383,10.3927344476349,47.7395993146674));
#110125=CARTESIAN_POINT('Ctrl Pts',(100.760786028196,10.1993577218161,47.7562725593024));
#110126=CARTESIAN_POINT('Origin',(101.5,10.2,45.0772274406976));
#110127=CARTESIAN_POINT('',(100.760790554215,10.1993571884951,46.8772274406976));
#110128=CARTESIAN_POINT('',(100.760218566757,10.2004851870816,46.9562725593024));
#110129=CARTESIAN_POINT('',(100.761,10.2,45.0772274406976));
#110130=CARTESIAN_POINT('Ctrl Pts',(100.760790554216,10.1993571884951,46.8772274406976));
#110131=CARTESIAN_POINT('Ctrl Pts',(100.760328944673,10.1484185953511,46.8816193764702));
#110132=CARTESIAN_POINT('Ctrl Pts',(100.78826499662,9.8538170750545,46.9070633367136));
#110133=CARTESIAN_POINT('Ctrl Pts',(101.18327099084,9.38768686529745,46.953559321428));
#110134=CARTESIAN_POINT('Ctrl Pts',(102.006786682075,9.49053741410128,47.0167153948406));
#110135=CARTESIAN_POINT('Ctrl Pts',(102.371125372346,10.2362006472893,47.0798714682533));
#110136=CARTESIAN_POINT('Ctrl Pts',(101.946175880112,10.9490640718669,47.143027541666));
#110137=CARTESIAN_POINT('Ctrl Pts',(101.116966152284,10.983233663854,47.2061836150786));
#110138=CARTESIAN_POINT('Ctrl Pts',(100.775453563156,10.5047900625241,47.2509169147559));
#110139=CARTESIAN_POINT('Ctrl Pts',(100.759986200666,10.2309183671265,47.2745981899622));
#110140=CARTESIAN_POINT('Ctrl Pts',(100.760218090122,10.2004849659209,47.2772274406976));
#110141=CARTESIAN_POINT('Ctrl Pts',(100.760218566757,10.2004851870817,46.9562725593024));
#110142=CARTESIAN_POINT('Ctrl Pts',(100.761843790147,9.98726122745261,46.9746937121543));
#110143=CARTESIAN_POINT('Ctrl Pts',(100.970345134679,9.52758681490828,47.0141668894771));
#110144=CARTESIAN_POINT('Ctrl Pts',(101.748758192064,9.36436297329056,47.0746920912707));
#110145=CARTESIAN_POINT('Ctrl Pts',(102.335618023451,9.95117798071123,47.1378481646834));
#110146=CARTESIAN_POINT('Ctrl Pts',(102.165361312267,10.7634396172603,47.201004238096));
#110147=CARTESIAN_POINT('Ctrl Pts',(101.392250136753,11.065193530587,47.2641603115087));
#110148=CARTESIAN_POINT('Ctrl Pts',(100.838694327669,10.6700659187596,47.3159164185775));
#110149=CARTESIAN_POINT('Ctrl Pts',(100.761893355754,10.312618478149,47.3466205011754));
#110150=CARTESIAN_POINT('Ctrl Pts',(100.762115726615,10.2001616419592,47.3562725593024));
#110151=CARTESIAN_POINT('Origin',(101.5,10.2,45.0772274406976));
#110152=CARTESIAN_POINT('',(100.762114836837,10.2001642984427,46.4772274406976));
#110153=CARTESIAN_POINT('',(100.760790004998,10.1993572533204,46.5562725593024));
#110154=CARTESIAN_POINT('',(100.761,10.2,45.0772274406976));
#110155=CARTESIAN_POINT('Ctrl Pts',(100.762114836837,10.2001642984427,46.4772274406976));
#110156=CARTESIAN_POINT('Ctrl Pts',(100.762381617085,10.0671895096557,46.4886405629782));
#110157=CARTESIAN_POINT('Ctrl Pts',(100.860050119229,9.688570906901,46.5211057097297));
#110158=CARTESIAN_POINT('Ctrl Pts',(101.464339557519,9.32885262012148,46.574622880952));
#110159=CARTESIAN_POINT('Ctrl Pts',(102.209776569879,9.69365312349436,46.6377789543647));
#110160=CARTESIAN_POINT('Ctrl Pts',(102.312116654185,10.5172326125426,46.7009350277773));
#110161=CARTESIAN_POINT('Ctrl Pts',(101.678633633533,11.0533814325012,46.76409110119));
#110162=CARTESIAN_POINT('Ctrl Pts',(100.938607013354,10.8328047227516,46.8228552388301));
#110163=CARTESIAN_POINT('Ctrl Pts',(100.762541594375,10.3925843948781,46.8605673519993));
#110164=CARTESIAN_POINT('Ctrl Pts',(100.760790554216,10.1993571884951,46.8772274406976));
#110165=CARTESIAN_POINT('Ctrl Pts',(100.760790004998,10.1993572533204,46.5562725593024));
#110166=CARTESIAN_POINT('Ctrl Pts',(100.760328571292,10.1484375546355,46.5606628741914));
#110167=CARTESIAN_POINT('Ctrl Pts',(100.788252312888,9.8538551645519,46.5861052135513));
#110168=CARTESIAN_POINT('Ctrl Pts',(101.183208968053,9.38771109556577,46.6325995773821));
#110169=CARTESIAN_POINT('Ctrl Pts',(102.006732474123,9.49049870563814,46.6957556507947));
#110170=CARTESIAN_POINT('Ctrl Pts',(102.371128126366,10.2361341135068,46.7589117242074));
#110171=CARTESIAN_POINT('Ctrl Pts',(101.946233085569,10.9490299761907,46.82206779762));
#110172=CARTESIAN_POINT('Ctrl Pts',(101.11702598516,10.9832629084246,46.8852238710328));
#110173=CARTESIAN_POINT('Ctrl Pts',(100.775464480548,10.5048280645237,46.9299587915935));
#110174=CARTESIAN_POINT('Ctrl Pts',(100.759986455655,10.2309373997303,46.9536416876834));
#110175=CARTESIAN_POINT('Ctrl Pts',(100.760218566757,10.2004851870817,46.9562725593024));
#110176=CARTESIAN_POINT('Origin',(101.5,10.2,45.0772274406976));
#110177=CARTESIAN_POINT('',(100.760229243717,10.2005121657882,46.0772274406976));
#110178=CARTESIAN_POINT('',(100.762116465727,10.2001659521564,46.1562725593024));
#110179=CARTESIAN_POINT('',(100.761,10.2,45.0772274406976));
#110180=CARTESIAN_POINT('Ctrl Pts',(100.760229243717,10.2005121657882,46.0772274406976));
#110181=CARTESIAN_POINT('Ctrl Pts',(100.761855102872,9.98714653281361,46.0956617494862));
#110182=CARTESIAN_POINT('Ctrl Pts',(100.970571497003,9.52725163041578,46.1351480827457));
#110183=CARTESIAN_POINT('Ctrl Pts',(101.749287158062,9.36453901572865,46.195686440476));
#110184=CARTESIAN_POINT('Ctrl Pts',(102.335766870331,9.95168565395949,46.2588425138887));
#110185=CARTESIAN_POINT('Ctrl Pts',(102.165014415475,10.7638570231953,46.3219985873013));
#110186=CARTESIAN_POINT('Ctrl Pts',(101.39171255474,11.0651241681623,46.385154660714));
#110187=CARTESIAN_POINT('Ctrl Pts',(100.838543929659,10.669756891461,46.4368976118461));
#110188=CARTESIAN_POINT('Ctrl Pts',(100.761889528753,10.3124675710606,46.4675885385073));
#110189=CARTESIAN_POINT('Ctrl Pts',(100.762114836837,10.2001642984427,46.4772274406976));
#110190=CARTESIAN_POINT('Ctrl Pts',(100.762116465727,10.2001659521564,46.1562725593024));
#110191=CARTESIAN_POINT('Ctrl Pts',(100.762382064326,10.0672091272765,46.1676840606994));
#110192=CARTESIAN_POINT('Ctrl Pts',(100.860027014519,9.68860582926417,46.2001475865673));
#110193=CARTESIAN_POINT('Ctrl Pts',(101.464274479552,9.32885726690886,46.2536631369061));
#110194=CARTESIAN_POINT('Ctrl Pts',(102.209737178785,9.69359800080378,46.3168192103187));
#110195=CARTESIAN_POINT('Ctrl Pts',(102.312141208784,10.5171710165563,46.3799752837314));
#110196=CARTESIAN_POINT('Ctrl Pts',(101.678698651257,11.0533675611342,46.4431313571441));
#110197=CARTESIAN_POINT('Ctrl Pts',(100.938635007123,10.8328415897021,46.5018971156678));
#110198=CARTESIAN_POINT('Ctrl Pts',(100.762541194739,10.3926028980946,46.5396108497205));
#110199=CARTESIAN_POINT('Ctrl Pts',(100.760790004998,10.1993572533204,46.5562725593024));
#110200=CARTESIAN_POINT('Origin',(101.5,10.2,48.71675));
#110201=CARTESIAN_POINT('Ctrl Pts',(102.101843294079,10.6308187385845,48.71675));
#110202=CARTESIAN_POINT('Ctrl Pts',(102.092690583018,10.6489925625313,48.71675));
#110203=CARTESIAN_POINT('Ctrl Pts',(102.082761232596,10.6667230538167,48.71675));
#110204=CARTESIAN_POINT('Ctrl Pts',(102.072068380608,10.6839544004916,48.71675));
#110205=CARTESIAN_POINT('Ctrl Pts',(102.054494347484,10.7122746519614,48.71675));
#110206=CARTESIAN_POINT('Ctrl Pts',(102.034860699482,10.7392477510368,48.71675));
#110207=CARTESIAN_POINT('Ctrl Pts',(102.01341340141,10.7648111233467,48.71675));
#110208=CARTESIAN_POINT('Ctrl Pts',(102.006324556343,10.7732604294126,48.71675));
#110209=CARTESIAN_POINT('Ctrl Pts',(101.999037195898,10.7815556229965,48.71675));
#110210=CARTESIAN_POINT('Ctrl Pts',(101.991559132777,10.7896940729177,48.71675));
#110211=CARTESIAN_POINT('Ctrl Pts',(101.985554234903,10.7962292625578,48.71675));
#110212=CARTESIAN_POINT('Ctrl Pts',(101.979427179349,10.8026622683498,48.71675));
#110213=CARTESIAN_POINT('Ctrl Pts',(101.973191056542,10.8089830617106,48.71675));
#110214=CARTESIAN_POINT('Ctrl Pts',(101.948142429081,10.8343717852865,48.71675));
#110215=CARTESIAN_POINT('Ctrl Pts',(101.921302301576,10.8579911576652,48.71675));
#110216=CARTESIAN_POINT('Ctrl Pts',(101.89295359764,10.8797678614235,48.71675));
#110217=CARTESIAN_POINT('Ctrl Pts',(101.872371173306,10.8955787203034,48.71675));
#110218=CARTESIAN_POINT('Ctrl Pts',(101.850992282563,10.9104180010441,48.71675));
#110219=CARTESIAN_POINT('Ctrl Pts',(101.828910233771,10.9242499170876,48.71675));
#110220=CARTESIAN_POINT('Ctrl Pts',(101.821834677165,10.9286819562456,48.71675));
#110221=CARTESIAN_POINT('Ctrl Pts',(101.814689271962,10.9330088612385,48.71675));
#110222=CARTESIAN_POINT('Ctrl Pts',(101.807486420978,10.9372243553017,48.71675));
#110223=CARTESIAN_POINT('Ctrl Pts',(101.774891643114,10.9563005645511,48.71675));
#110224=CARTESIAN_POINT('Ctrl Pts',(101.741072447943,10.973130235416,48.71675));
#110225=CARTESIAN_POINT('Ctrl Pts',(101.706330263218,10.9876331586578,48.71675));
#110226=CARTESIAN_POINT('Ctrl Pts',(101.671325142582,11.0022458429686,48.71675));
#110227=CARTESIAN_POINT('Ctrl Pts',(101.635381961669,11.0144973135584,48.71675));
#110228=CARTESIAN_POINT('Ctrl Pts',(101.598767749634,11.0242717697334,48.71675));
#110229=CARTESIAN_POINT('Ctrl Pts',(101.579580093906,11.029394067595,48.71675));
#110230=CARTESIAN_POINT('Ctrl Pts',(101.560207566501,11.0338354689131,48.71675));
#110231=CARTESIAN_POINT('Ctrl Pts',(101.540685650761,11.0375743770417,48.71675));
#110232=CARTESIAN_POINT('Ctrl Pts',(101.53155005331,11.0393240598099,48.71675));
#110233=CARTESIAN_POINT('Ctrl Pts',(101.522380019735,11.040919918186,48.71675));
#110234=CARTESIAN_POINT('Ctrl Pts',(101.513201010965,11.0423565975106,48.71675));
#110235=CARTESIAN_POINT('Ctrl Pts',(101.473716936833,11.0485365625134,48.71675));
#110236=CARTESIAN_POINT('Ctrl Pts',(101.43398096282,11.0517930196521,48.71675));
#110237=CARTESIAN_POINT('Ctrl Pts',(101.394302526066,11.0520184237927,48.71675));
#110238=CARTESIAN_POINT('Ctrl Pts',(101.356654041365,11.052232296239,48.71675));
#110239=CARTESIAN_POINT('Ctrl Pts',(101.319055963889,11.0497182152357,48.71675));
#110240=CARTESIAN_POINT('Ctrl Pts',(101.281703678425,11.0446512493134,48.71675));
#110241=CARTESIAN_POINT('Ctrl Pts',(101.26460477746,11.0423317246196,48.71675));
#110242=CARTESIAN_POINT('Ctrl Pts',(101.24755721676,11.0394765171797,48.71675));
#110243=CARTESIAN_POINT('Ctrl Pts',(101.23057927414,11.0360989397513,48.71675));
#110244=CARTESIAN_POINT('Ctrl Pts',(101.221478845773,11.0342885082916,48.71675));
#110245=CARTESIAN_POINT('Ctrl Pts',(101.212398417896,11.0323279573613,48.71675));
#110246=CARTESIAN_POINT('Ctrl Pts',(101.203340811571,11.0302190898984,48.71675));
#110247=CARTESIAN_POINT('Ctrl Pts',(101.195132556756,11.0283079755393,48.71675));
#110248=CARTESIAN_POINT('Ctrl Pts',(101.186950940351,11.0262768354341,48.71675));
#110249=CARTESIAN_POINT('Ctrl Pts',(101.178803613277,11.024129252906,48.71675));
#110250=CARTESIAN_POINT('Ctrl Pts',(101.140506034481,11.0140342597457,48.71675));
#110251=CARTESIAN_POINT('Ctrl Pts',(101.102928410637,11.0013616719051,48.71675));
#110252=CARTESIAN_POINT('Ctrl Pts',(101.066285661362,10.9863186497589,48.71675));
#110253=CARTESIAN_POINT('Ctrl Pts',(101.028791532849,10.9709261091683,48.71675));
#110254=CARTESIAN_POINT('Ctrl Pts',(100.992275134187,10.9530515299956,48.71675));
#110255=CARTESIAN_POINT('Ctrl Pts',(100.956964088485,10.9328624060656,48.71675));
#110256=CARTESIAN_POINT('Ctrl Pts',(100.940025732422,10.9231778848934,48.71675));
#110257=CARTESIAN_POINT('Ctrl Pts',(100.923364796535,10.9129600041663,48.71675));
#110258=CARTESIAN_POINT('Ctrl Pts',(100.907007375654,10.9022231657751,48.71675));
#110259=CARTESIAN_POINT('Ctrl Pts',(100.900112212376,10.8976972533868,48.71675));
#110260=CARTESIAN_POINT('Ctrl Pts',(100.893270992315,10.8930790974484,48.71675));
#110261=CARTESIAN_POINT('Ctrl Pts',(100.88648573145,10.8883696454142,48.71675));
#110262=CARTESIAN_POINT('Ctrl Pts',(100.87935004954,10.8834169763343,48.71675));
#110263=CARTESIAN_POINT('Ctrl Pts',(100.872282874817,10.8783678650625,48.71675));
#110264=CARTESIAN_POINT('Ctrl Pts',(100.865291068121,10.8732276252648,48.71675));
#110265=CARTESIAN_POINT('Ctrl Pts',(100.831195079059,10.8481609196874,48.71675));
#110266=CARTESIAN_POINT('Ctrl Pts',(100.798854446776,10.8209060995123,48.71675));
#110267=CARTESIAN_POINT('Ctrl Pts',(100.768506288754,10.791658862854,48.71675));
#110268=CARTESIAN_POINT('Ctrl Pts',(100.738364625154,10.7626106297466,48.71675));
#110269=CARTESIAN_POINT('Ctrl Pts',(100.710187233691,10.7315964626783,48.71675));
#110270=CARTESIAN_POINT('Ctrl Pts',(100.684223172419,10.6987607209512,48.71675));
#110271=CARTESIAN_POINT('Ctrl Pts',(100.665548276792,10.6751433044338,48.71675));
#110272=CARTESIAN_POINT('Ctrl Pts',(100.648018699993,10.6505825193258,48.71675));
#110273=CARTESIAN_POINT('Ctrl Pts',(100.631737776319,10.625119128515,48.71675));
#110274=CARTESIAN_POINT('',(100.630604630375,9.77384666716111,48.71675));
#110275=CARTESIAN_POINT('Origin',(101.5,10.2,48.71675));
#110276=CARTESIAN_POINT('Ctrl Pts',(100.630581430873,9.77382549334316,48.71675));
#110277=CARTESIAN_POINT('Ctrl Pts',(100.64457938054,9.75169648824875,48.71675));
#110278=CARTESIAN_POINT('Ctrl Pts',(100.659509975824,9.73021546929278,48.71675));
#110279=CARTESIAN_POINT('Ctrl Pts',(100.675375864845,9.70945200083441,48.71675));
#110280=CARTESIAN_POINT('Ctrl Pts',(100.698139903374,9.6796610199839,48.71675));
#110281=CARTESIAN_POINT('Ctrl Pts',(100.722828987013,9.65134590823789,48.71675));
#110282=CARTESIAN_POINT('Ctrl Pts',(100.749246101771,9.62460368156239,48.71675));
#110283=CARTESIAN_POINT('Ctrl Pts',(100.759494608228,9.61422904810002,48.71675));
#110284=CARTESIAN_POINT('Ctrl Pts',(100.770003353453,9.60409144395543,48.71675));
#110285=CARTESIAN_POINT('Ctrl Pts',(100.780761309316,9.59419773022566,48.71675));
#110286=CARTESIAN_POINT('Ctrl Pts',(100.791070498368,9.58471673155325,48.71675));
#110287=CARTESIAN_POINT('Ctrl Pts',(100.801612891683,9.57545635783652,48.71675));
#110288=CARTESIAN_POINT('Ctrl Pts',(100.812354121759,9.56644314416643,48.71675));
#110289=CARTESIAN_POINT('Ctrl Pts',(100.844321982801,9.53961817532173,48.71675));
#110290=CARTESIAN_POINT('Ctrl Pts',(100.878082193053,9.51494593631547,48.71675));
#110291=CARTESIAN_POINT('Ctrl Pts',(100.913359655757,9.49256416154415,48.71675));
#110292=CARTESIAN_POINT('Ctrl Pts',(100.93382034179,9.47958288592574,48.71675));
#110293=CARTESIAN_POINT('Ctrl Pts',(100.954791816909,9.4673729974237,48.71675));
#110294=CARTESIAN_POINT('Ctrl Pts',(100.976221881509,9.45596930559344,48.71675));
#110295=CARTESIAN_POINT('Ctrl Pts',(100.984317998785,9.45166107656292,48.71675));
#110296=CARTESIAN_POINT('Ctrl Pts',(100.992479570662,9.44746797593293,48.71675));
#110297=CARTESIAN_POINT('Ctrl Pts',(101.000703773174,9.44339211164565,48.71675));
#110298=CARTESIAN_POINT('Ctrl Pts',(101.00844277817,9.43955670827007,48.71675));
#110299=CARTESIAN_POINT('Ctrl Pts',(101.016232654013,9.43582746843061,48.71675));
#110300=CARTESIAN_POINT('Ctrl Pts',(101.024063874372,9.43220886794855,48.71675));
#110301=CARTESIAN_POINT('Ctrl Pts',(101.060487154985,9.41537863016349,48.71675));
#110302=CARTESIAN_POINT('Ctrl Pts',(101.097850508457,9.40091469113947,48.71675));
#110303=CARTESIAN_POINT('Ctrl Pts',(101.135908601312,9.38894508905378,48.71675));
#110304=CARTESIAN_POINT('Ctrl Pts',(101.173086380745,9.37725235321574,48.71675));
#110305=CARTESIAN_POINT('Ctrl Pts',(101.210928218599,9.36793981658584,48.71675));
#110306=CARTESIAN_POINT('Ctrl Pts',(101.249203335133,9.36117504344504,48.71675));
#110307=CARTESIAN_POINT('Ctrl Pts',(101.26756945998,9.35792900060259,48.71675));
#110308=CARTESIAN_POINT('Ctrl Pts',(101.286035216727,9.3552703122121,48.71675));
#110309=CARTESIAN_POINT('Ctrl Pts',(101.304573852963,9.35322165048947,48.71675));
#110310=CARTESIAN_POINT('Ctrl Pts',(101.312743136943,9.35231888185126,48.71675));
#110311=CARTESIAN_POINT('Ctrl Pts',(101.320926558308,9.35153460646509,48.71675));
#110312=CARTESIAN_POINT('Ctrl Pts',(101.32912174998,9.35087093707399,48.71675));
#110313=CARTESIAN_POINT('Ctrl Pts',(101.337079548327,9.35022649245393,48.71675));
#110314=CARTESIAN_POINT('Ctrl Pts',(101.345042813093,9.34969629700434,48.71675));
#110315=CARTESIAN_POINT('Ctrl Pts',(101.353001912458,9.34928206049807,48.71675));
#110316=CARTESIAN_POINT('Ctrl Pts',(101.39019525861,9.34734630859198,48.71675));
#110317=CARTESIAN_POINT('Ctrl Pts',(101.427349750722,9.34793465249878,48.71675));
#110318=CARTESIAN_POINT('Ctrl Pts',(101.464257143167,9.35118601291411,48.71675));
#110319=CARTESIAN_POINT('Ctrl Pts',(101.497915149683,9.35415111835223,48.71675));
#110320=CARTESIAN_POINT('Ctrl Pts',(101.53136812566,9.35933215400883,48.71675));
#110321=CARTESIAN_POINT('Ctrl Pts',(101.564442234567,9.36663343101134,48.71675));
#110322=CARTESIAN_POINT('Ctrl Pts',(101.581998310551,9.37050902367491,48.71675));
#110323=CARTESIAN_POINT('Ctrl Pts',(101.599447362032,9.37498247030888,48.71675));
#110324=CARTESIAN_POINT('Ctrl Pts',(101.61676102719,9.38004213013849,48.71675));
#110325=CARTESIAN_POINT('Ctrl Pts',(101.627764250115,9.38325765755686,48.71675));
#110326=CARTESIAN_POINT('Ctrl Pts',(101.638712756026,9.38670998442451,48.71675));
#110327=CARTESIAN_POINT('Ctrl Pts',(101.649598833322,9.39039643608377,48.71675));
#110328=CARTESIAN_POINT('Ctrl Pts',(101.657334704852,9.39301610482793,48.71675));
#110329=CARTESIAN_POINT('Ctrl Pts',(101.665031702681,9.39575158311581,48.71675));
#110330=CARTESIAN_POINT('Ctrl Pts',(101.672681658731,9.39859908201335,48.71675));
#110331=CARTESIAN_POINT('Ctrl Pts',(101.707638773391,9.4116109666317,48.71675));
#110332=CARTESIAN_POINT('Ctrl Pts',(101.741655218118,9.42697182351799,48.71675));
#110333=CARTESIAN_POINT('Ctrl Pts',(101.774500046676,9.44453787650665,48.71675));
#110334=CARTESIAN_POINT('Ctrl Pts',(101.806936769189,9.46188566644687,48.71675));
#110335=CARTESIAN_POINT('Ctrl Pts',(101.838231681605,9.48138516613843,48.71675));
#110336=CARTESIAN_POINT('Ctrl Pts',(101.86812362857,9.50292993629208,48.71675));
#110337=CARTESIAN_POINT('Ctrl Pts',(101.882249726167,9.51311139172793,48.71675));
#110338=CARTESIAN_POINT('Ctrl Pts',(101.896061863265,9.52374998245355,48.71675));
#110339=CARTESIAN_POINT('Ctrl Pts',(101.909528589229,9.53483608185471,48.71675));
#110340=CARTESIAN_POINT('Ctrl Pts',(101.916887297398,9.54089392920632,48.71675));
#110341=CARTESIAN_POINT('Ctrl Pts',(101.924145165926,9.54708773163212,48.71675));
#110342=CARTESIAN_POINT('Ctrl Pts',(101.931278238249,9.55339893605095,48.71675));
#110343=CARTESIAN_POINT('Ctrl Pts',(101.957731009864,9.57680383670771,48.71675));
#110344=CARTESIAN_POINT('Ctrl Pts',(101.982525561837,9.60186412427372,48.71675));
#110345=CARTESIAN_POINT('Ctrl Pts',(102.005439886383,9.62847142275743,48.71675));
#110346=CARTESIAN_POINT('Ctrl Pts',(102.027519731796,9.65410975375978,48.71675));
#110347=CARTESIAN_POINT('Ctrl Pts',(102.047854190426,9.68118532379663,48.71675));
#110348=CARTESIAN_POINT('Ctrl Pts',(102.066199893377,9.70961703269809,48.71675));
#110349=CARTESIAN_POINT('Ctrl Pts',(102.078805695628,9.72915318789655,48.71675));
#110350=CARTESIAN_POINT('Ctrl Pts',(102.090471602248,9.74932995292834,48.71675));
#110351=CARTESIAN_POINT('Ctrl Pts',(102.101104350279,9.77012262204778,48.71675));
#110352=CARTESIAN_POINT('Ctrl Pts',(101.175031770393,10.8637142832168,45.6852584761921));
#110353=CARTESIAN_POINT('Ctrl Pts',(100.955551792886,10.756252350382,45.706310500663));
#110354=CARTESIAN_POINT('Ctrl Pts',(100.635341557809,10.3080724084119,45.7484145496047));
#110355=CARTESIAN_POINT('Ctrl Pts',(100.936604150766,9.53400264453299,45.8115706230174));
#110356=CARTESIAN_POINT('Ctrl Pts',(101.749341902197,9.36467411870078,45.8747266964301));
#110357=CARTESIAN_POINT('Ctrl Pts',(102.33569099053,9.95154749830959,45.9378827698427));
#110358=CARTESIAN_POINT('Ctrl Pts',(102.165084835389,10.7638419256677,46.0010388432554));
#110359=CARTESIAN_POINT('Ctrl Pts',(101.391765482636,11.0651152556269,46.0641949166681));
#110360=CARTESIAN_POINT('Ctrl Pts',(100.716565164316,10.5826174497482,46.1273509900807));
#110361=CARTESIAN_POINT('Ctrl Pts',(100.751175258495,9.75341249376129,46.1905070634934));
#110362=CARTESIAN_POINT('Ctrl Pts',(101.464274479552,9.32885726690886,46.2536631369061));
#110363=CARTESIAN_POINT('Ctrl Pts',(102.209737178785,9.69359800080378,46.3168192103187));
#110364=CARTESIAN_POINT('Ctrl Pts',(102.312141208784,10.5171710165563,46.3799752837314));
#110365=CARTESIAN_POINT('Ctrl Pts',(101.678698651257,11.0533675611342,46.4431313571441));
#110366=CARTESIAN_POINT('Ctrl Pts',(100.883345795901,10.8163663755618,46.5062874305568));
#110367=CARTESIAN_POINT('Ctrl Pts',(100.646715736332,10.020902446434,46.5694435039694));
#110368=CARTESIAN_POINT('Ctrl Pts',(101.183208968053,9.38771109556577,46.6325995773821));
#110369=CARTESIAN_POINT('Ctrl Pts',(102.006732474123,9.49049870563814,46.6957556507947));
#110370=CARTESIAN_POINT('Ctrl Pts',(102.371128126366,10.2361341135068,46.7589117242074));
#110371=CARTESIAN_POINT('Ctrl Pts',(101.946233085569,10.9490299761907,46.82206779762));
#110372=CARTESIAN_POINT('Ctrl Pts',(101.11702598516,10.9832629084246,46.8852238710328));
#110373=CARTESIAN_POINT('Ctrl Pts',(100.634814701675,10.3078159478443,46.9483799444453));
#110374=CARTESIAN_POINT('Ctrl Pts',(100.936509562721,9.53468172677525,47.0115360178581));
#110375=CARTESIAN_POINT('Ctrl Pts',(101.748758192064,9.36436297329056,47.0746920912707));
#110376=CARTESIAN_POINT('Ctrl Pts',(102.335618023451,9.95117798071123,47.1378481646834));
#110377=CARTESIAN_POINT('Ctrl Pts',(102.165361312267,10.7634396172603,47.201004238096));
#110378=CARTESIAN_POINT('Ctrl Pts',(101.392250136753,11.065193530587,47.2641603115087));
#110379=CARTESIAN_POINT('Ctrl Pts',(100.716766347564,10.5830338421318,47.3273163849214));
#110380=CARTESIAN_POINT('Ctrl Pts',(100.750935939053,9.75382412639255,47.390472458334));
#110381=CARTESIAN_POINT('Ctrl Pts',(101.463799353238,9.32887464035278,47.4536285317467));
#110382=CARTESIAN_POINT('Ctrl Pts',(102.209462575557,9.69321332531287,47.5167846051594));
#110383=CARTESIAN_POINT('Ctrl Pts',(102.31231312286,10.5167290045424,47.579940678572));
#110384=CARTESIAN_POINT('Ctrl Pts',(101.679162679895,11.0532705437534,47.6430967519847));
#110385=CARTESIAN_POINT('Ctrl Pts',(100.883680829641,10.8167013598813,47.7062528253974));
#110386=CARTESIAN_POINT('Ctrl Pts',(100.646618579947,10.0213663690729,47.7694088988101));
#110387=CARTESIAN_POINT('Ctrl Pts',(101.182767392066,9.3878833576509,47.8325649722227));
#110388=CARTESIAN_POINT('Ctrl Pts',(102.006346869156,9.49022344047391,47.8957210456354));
#110389=CARTESIAN_POINT('Ctrl Pts',(102.371147367118,10.2356604419514,47.958877119048));
#110390=CARTESIAN_POINT('Ctrl Pts',(101.946640733675,10.9487875878849,48.0220331924607));
#110391=CARTESIAN_POINT('Ctrl Pts',(101.117450646044,10.9834703820361,48.0851892658734));
#110392=CARTESIAN_POINT('Ctrl Pts',(100.634875844886,10.3082874437177,48.148345339286));
#110393=CARTESIAN_POINT('Ctrl Pts',(100.936142984193,9.53498559418258,48.2115014126987));
#110394=CARTESIAN_POINT('Ctrl Pts',(101.74831434399,9.3642331418485,48.2746574861114));
#110395=CARTESIAN_POINT('Ctrl Pts',(102.335460969162,9.95071284574935,48.337813559524));
#110396=CARTESIAN_POINT('Ctrl Pts',(102.165712572132,10.7631006363966,48.4009696329368));
#110397=CARTESIAN_POINT('Ctrl Pts',(101.392626626404,11.065204620822,48.4641257063493));
#110398=CARTESIAN_POINT('Ctrl Pts',(100.717169409966,10.5835583129935,48.527281779762));
#110399=CARTESIAN_POINT('Ctrl Pts',(100.750281720561,9.75402930376689,48.5904378531747));
#110400=CARTESIAN_POINT('Ctrl Pts',(101.464139111132,9.32935204372765,48.6535939265874));
#110401=CARTESIAN_POINT('Ctrl Pts',(101.958950595826,9.57134677434548,48.6956979755291));
#110402=CARTESIAN_POINT('Ctrl Pts',(102.101104350279,9.77012262204778,48.71675));
#110403=CARTESIAN_POINT('Ctrl Pts',(101.141648137424,10.931896930038,45.7290889841281));
#110404=CARTESIAN_POINT('Ctrl Pts',(100.899621220414,10.81339554966,45.7501410085989));
#110405=CARTESIAN_POINT('Ctrl Pts',(100.546516135974,10.3191745694474,45.7922450575407));
#110406=CARTESIAN_POINT('Ctrl Pts',(100.878727107616,9.46558546018134,45.8554011309534));
#110407=CARTESIAN_POINT('Ctrl Pts',(101.774956524761,9.27886199895974,45.9185572043661));
#110408=CARTESIAN_POINT('Ctrl Pts',(102.421540617545,9.92602424289236,45.9817132777787));
#110409=CARTESIAN_POINT('Ctrl Pts',(102.233408277545,10.8217647937645,46.0448693511913));
#110410=CARTESIAN_POINT('Ctrl Pts',(101.380646668324,11.15398760541,46.1080254246041));
#110411=CARTESIAN_POINT('Ctrl Pts',(100.636083755282,10.6219233244348,46.1711814980167));
#110412=CARTESIAN_POINT('Ctrl Pts',(100.674249306813,9.70753504471038,46.2343375714294));
#110413=CARTESIAN_POINT('Ctrl Pts',(101.460604435672,9.23936572091811,46.297493644842));
#110414=CARTESIAN_POINT('Ctrl Pts',(102.282647707639,9.64157587391296,46.3606497182547));
#110415=CARTESIAN_POINT('Ctrl Pts',(102.395571592321,10.5497536503049,46.4238057916674));
#110416=CARTESIAN_POINT('Ctrl Pts',(101.697056169445,11.1410330830324,46.48696186508));
#110417=CARTESIAN_POINT('Ctrl Pts',(100.819997579851,10.8796850232994,46.5501179384927));
#110418=CARTESIAN_POINT('Ctrl Pts',(100.559058771492,10.0025039494449,46.6132740119053));
#110419=CARTESIAN_POINT('Ctrl Pts',(101.15066536971,9.30426553941562,46.6764300853181));
#110420=CARTESIAN_POINT('Ctrl Pts',(102.058788550343,9.41761240893498,46.7395861587307));
#110421=CARTESIAN_POINT('Ctrl Pts',(102.460618171823,10.2398461317076,46.8027422321434));
#110422=CARTESIAN_POINT('Ctrl Pts',(101.992074125369,11.0259770114083,46.865898305556));
#110423=CARTESIAN_POINT('Ctrl Pts',(101.077683480929,11.0637266555575,46.9290543789687));
#110424=CARTESIAN_POINT('Ctrl Pts',(100.545935156482,10.3188917629645,46.9922104523813));
#110425=CARTESIAN_POINT('Ctrl Pts',(100.878622802644,9.46633430380414,47.055366525794));
#110426=CARTESIAN_POINT('Ctrl Pts',(101.774312850721,9.27851888991975,47.1185225992067));
#110427=CARTESIAN_POINT('Ctrl Pts',(102.421460154638,9.9256167651528,47.1816786726194));
#110428=CARTESIAN_POINT('Ctrl Pts',(102.233713156592,10.8213211566518,47.244834746032));
#110429=CARTESIAN_POINT('Ctrl Pts',(101.381181110432,11.1540739214716,47.3079908194447));
#110430=CARTESIAN_POINT('Ctrl Pts',(100.636305605867,10.6223824923553,47.3711468928573));
#110431=CARTESIAN_POINT('Ctrl Pts',(100.673985402345,9.70798896391439,47.43430296627));
#110432=CARTESIAN_POINT('Ctrl Pts',(101.460080500149,9.23938487911703,47.4974590396827));
#110433=CARTESIAN_POINT('Ctrl Pts',(102.282344894719,9.64115168112703,47.5606151130954));
#110434=CARTESIAN_POINT('Ctrl Pts',(102.395761166942,10.5492662308773,47.623771186508));
#110435=CARTESIAN_POINT('Ctrl Pts',(101.697567867241,11.1409260991615,47.6869272599207));
#110436=CARTESIAN_POINT('Ctrl Pts',(100.820367031243,10.8800544201938,47.7500833333334));
#110437=CARTESIAN_POINT('Ctrl Pts',(100.558951634338,10.0030155303523,47.813239406746));
#110438=CARTESIAN_POINT('Ctrl Pts',(101.150178431102,9.30445549779749,47.8763954801587));
#110439=CARTESIAN_POINT('Ctrl Pts',(102.058363332597,9.41730886607965,47.9395515535713));
#110440=CARTESIAN_POINT('Ctrl Pts',(102.460639389158,10.2393238003883,48.002707626984));
#110441=CARTESIAN_POINT('Ctrl Pts',(101.992523650723,11.0257097228153,48.0658637003966));
#110442=CARTESIAN_POINT('Ctrl Pts',(101.078151766765,11.0639554427076,48.1290197738094));
#110443=CARTESIAN_POINT('Ctrl Pts',(100.546002580868,10.3194116950965,48.192175847222));
#110444=CARTESIAN_POINT('Ctrl Pts',(100.878218565903,9.46666938717991,48.2553319206347));
#110445=CARTESIAN_POINT('Ctrl Pts',(101.773823406617,9.27837572103478,48.3184879940473));
#110446=CARTESIAN_POINT('Ctrl Pts',(102.421286966332,9.92510384738192,48.38164406746));
#110447=CARTESIAN_POINT('Ctrl Pts',(102.234100501002,10.8209473526525,48.4448001408727));
#110448=CARTESIAN_POINT('Ctrl Pts',(101.381596276455,11.1540861509944,48.5079562142854));
#110449=CARTESIAN_POINT('Ctrl Pts',(100.636750074431,10.6229608415385,48.571112287698));
#110450=CARTESIAN_POINT('Ctrl Pts',(100.673263976699,9.70821521893735,48.6342683611107));
#110451=CARTESIAN_POINT('Ctrl Pts',(101.460455161001,9.23991132562163,48.6974244345233));
#110452=CARTESIAN_POINT('Ctrl Pts',(102.006098091631,9.50676591185436,48.7395284834651));
#110453=CARTESIAN_POINT('Ctrl Pts',(102.16285514675,9.72596178631092,48.760580507936));
#110454=CARTESIAN_POINT('Ctrl Pts',(101.108264504454,11.0000795768592,45.772919492064));
#110455=CARTESIAN_POINT('Ctrl Pts',(100.843690647942,10.8705387489381,45.7939715165349));
#110456=CARTESIAN_POINT('Ctrl Pts',(100.457690714139,10.330276730483,45.8360755654767));
#110457=CARTESIAN_POINT('Ctrl Pts',(100.820850064466,9.39716827582969,45.8992316388894));
#110458=CARTESIAN_POINT('Ctrl Pts',(101.800571147326,9.1930498792187,45.962387712302));
#110459=CARTESIAN_POINT('Ctrl Pts',(102.507390244561,9.90050098747513,46.0255437857147));
#110460=CARTESIAN_POINT('Ctrl Pts',(102.301731719701,10.8796876618614,46.0886998591274));
#110461=CARTESIAN_POINT('Ctrl Pts',(101.369527854013,11.242859955193,46.15185593254));
#110462=CARTESIAN_POINT('Ctrl Pts',(100.555602346249,10.6612291991214,46.2150120059527));
#110463=CARTESIAN_POINT('Ctrl Pts',(100.597323355132,9.66165759565947,46.2781680793654));
#110464=CARTESIAN_POINT('Ctrl Pts',(101.456934391792,9.14987417492735,46.341324152778));
#110465=CARTESIAN_POINT('Ctrl Pts',(102.355558236492,9.58955374702215,46.4044802261907));
#110466=CARTESIAN_POINT('Ctrl Pts',(102.479001975857,10.5823362840535,46.4676362996034));
#110467=CARTESIAN_POINT('Ctrl Pts',(101.715413687634,11.2286986049306,46.530792373016));
#110468=CARTESIAN_POINT('Ctrl Pts',(100.7566493638,10.943003671037,46.5939484464287));
#110469=CARTESIAN_POINT('Ctrl Pts',(100.471401806652,9.98410545245592,46.6571045198413));
#110470=CARTESIAN_POINT('Ctrl Pts',(101.118121771367,9.22081998326547,46.7202605932541));
#110471=CARTESIAN_POINT('Ctrl Pts',(102.110844626564,9.34472611223181,46.7834166666666));
#110472=CARTESIAN_POINT('Ctrl Pts',(102.550108217281,10.2435581499084,46.8465727400794));
#110473=CARTESIAN_POINT('Ctrl Pts',(102.03791516517,11.1029240466259,46.909728813492));
#110474=CARTESIAN_POINT('Ctrl Pts',(101.038340976698,11.1441904026905,46.9728848869047));
#110475=CARTESIAN_POINT('Ctrl Pts',(100.457055611289,10.3299675780847,47.0360409603173));
#110476=CARTESIAN_POINT('Ctrl Pts',(100.820736042567,9.39798688083304,47.09919703373));
#110477=CARTESIAN_POINT('Ctrl Pts',(101.799867509378,9.19267480654896,47.1623531071427));
#110478=CARTESIAN_POINT('Ctrl Pts',(102.507302285824,9.90005554959437,47.2255091805554));
#110479=CARTESIAN_POINT('Ctrl Pts',(102.302065000918,10.8792026960433,47.288665253968));
#110480=CARTESIAN_POINT('Ctrl Pts',(101.370112084111,11.2429543123562,47.3518213273806));
#110481=CARTESIAN_POINT('Ctrl Pts',(100.55584486417,10.6617311425788,47.4149774007933));
#110482=CARTESIAN_POINT('Ctrl Pts',(100.597034865638,9.66215380143623,47.478133474206));
#110483=CARTESIAN_POINT('Ctrl Pts',(101.456361647059,9.14989511788128,47.5412895476187));
#110484=CARTESIAN_POINT('Ctrl Pts',(102.355227213882,9.5890900369412,47.6044456210314));
#110485=CARTESIAN_POINT('Ctrl Pts',(102.479209211025,10.5818034572122,47.667601694444));
#110486=CARTESIAN_POINT('Ctrl Pts',(101.715973054587,11.2285816545697,47.7307577678567));
#110487=CARTESIAN_POINT('Ctrl Pts',(100.757053232844,10.9434074805064,47.7939138412693));
#110488=CARTESIAN_POINT('Ctrl Pts',(100.471284688728,9.98466469163163,47.857069914682));
#110489=CARTESIAN_POINT('Ctrl Pts',(101.117589470138,9.22102763794408,47.9202259880947));
#110490=CARTESIAN_POINT('Ctrl Pts',(102.110379796039,9.3443942916854,47.9833820615074));
#110491=CARTESIAN_POINT('Ctrl Pts',(102.550131411197,10.2429871588251,48.04653813492));
#110492=CARTESIAN_POINT('Ctrl Pts',(102.038406567771,11.1026318577458,48.1096942083327));
#110493=CARTESIAN_POINT('Ctrl Pts',(101.038852887485,11.1444405033791,48.1728502817453));
#110494=CARTESIAN_POINT('Ctrl Pts',(100.457129316851,10.3305359464753,48.236006355158));
#110495=CARTESIAN_POINT('Ctrl Pts',(100.820294147612,9.39835318017724,48.2991624285707));
#110496=CARTESIAN_POINT('Ctrl Pts',(101.799332469244,9.19251830022108,48.3623185019833));
#110497=CARTESIAN_POINT('Ctrl Pts',(102.507112963503,9.89949484901449,48.425474575396));
#110498=CARTESIAN_POINT('Ctrl Pts',(102.302488429871,10.8787940689084,48.4886306488086));
#110499=CARTESIAN_POINT('Ctrl Pts',(101.370565926506,11.2429676811668,48.5517867222213));
#110500=CARTESIAN_POINT('Ctrl Pts',(100.556330738897,10.6623633700836,48.614942795634));
#110501=CARTESIAN_POINT('Ctrl Pts',(100.596246232837,9.66240113410781,48.6780988690466));
#110502=CARTESIAN_POINT('Ctrl Pts',(101.45677121087,9.15047060751563,48.7412549424594));
#110503=CARTESIAN_POINT('Ctrl Pts',(102.053245587436,9.44218504936324,48.7833589914011));
#110504=CARTESIAN_POINT('Ctrl Pts',(102.224605943221,9.68180095057406,48.804411015872));
#110505=CARTESIAN_POINT('Ctrl Pts',(101.074880871485,11.0682622236804,45.81675));
#110506=CARTESIAN_POINT('Ctrl Pts',(100.78776007547,10.9276819482162,45.8378020244709));
#110507=CARTESIAN_POINT('Ctrl Pts',(100.368865292303,10.3413788915185,45.8799060734127));
#110508=CARTESIAN_POINT('Ctrl Pts',(100.762973021317,9.32875109147804,45.9430621468253));
#110509=CARTESIAN_POINT('Ctrl Pts',(101.82618576989,9.10723775947766,46.006218220238));
#110510=CARTESIAN_POINT('Ctrl Pts',(102.593239871576,9.8749777320579,46.0693742936507));
#110511=CARTESIAN_POINT('Ctrl Pts',(102.370055161857,10.9376105299583,46.1325303670633));
#110512=CARTESIAN_POINT('Ctrl Pts',(101.358409039701,11.3317323049761,46.195686440476));
#110513=CARTESIAN_POINT('Ctrl Pts',(100.475120937215,10.7005350738079,46.2588425138886));
#110514=CARTESIAN_POINT('Ctrl Pts',(100.52039740345,9.61578014660857,46.3219985873014));
#110515=CARTESIAN_POINT('Ctrl Pts',(101.453264347912,9.0603826289366,46.385154660714));
#110516=CARTESIAN_POINT('Ctrl Pts',(102.428468765346,9.53753162013133,46.4483107341267));
#110517=CARTESIAN_POINT('Ctrl Pts',(102.562432359394,10.6149189178021,46.5114668075393));
#110518=CARTESIAN_POINT('Ctrl Pts',(101.733771205822,11.3163641268288,46.574622880952));
#110519=CARTESIAN_POINT('Ctrl Pts',(100.69330114775,11.0063223187746,46.6377789543647));
#110520=CARTESIAN_POINT('Ctrl Pts',(100.383744841812,9.96570695546689,46.7009350277773));
#110521=CARTESIAN_POINT('Ctrl Pts',(101.085578173025,9.13737442711531,46.76409110119));
#110522=CARTESIAN_POINT('Ctrl Pts',(102.162900702785,9.27183981552865,46.8272471746026));
#110523=CARTESIAN_POINT('Ctrl Pts',(102.639598262739,10.2472701681092,46.8904032480154));
#110524=CARTESIAN_POINT('Ctrl Pts',(102.083756204971,11.1798710818435,46.953559321428));
#110525=CARTESIAN_POINT('Ctrl Pts',(100.998998472468,11.2246541498234,47.0167153948407));
#110526=CARTESIAN_POINT('Ctrl Pts',(100.368176066096,10.341043393205,47.0798714682533));
#110527=CARTESIAN_POINT('Ctrl Pts',(100.762849282491,9.32963945786195,47.1430275416661));
#110528=CARTESIAN_POINT('Ctrl Pts',(101.825422168035,9.10683072317815,47.2061836150786));
#110529=CARTESIAN_POINT('Ctrl Pts',(102.593144417011,9.87449433403596,47.2693396884914));
#110530=CARTESIAN_POINT('Ctrl Pts',(102.370416845243,10.9370842354348,47.3324957619039));
#110531=CARTESIAN_POINT('Ctrl Pts',(101.359043057789,11.3318347032408,47.3956518353167));
#110532=CARTESIAN_POINT('Ctrl Pts',(100.475384122473,10.7010797928023,47.4588079087293));
#110533=CARTESIAN_POINT('Ctrl Pts',(100.52008432893,9.61631863895806,47.521963982142));
#110534=CARTESIAN_POINT('Ctrl Pts',(101.452642793969,9.06040535664555,47.5851200555546));
#110535=CARTESIAN_POINT('Ctrl Pts',(102.428109533044,9.53702839275536,47.6482761289673));
#110536=CARTESIAN_POINT('Ctrl Pts',(102.562657255108,10.6143406835471,47.71143220238));
#110537=CARTESIAN_POINT('Ctrl Pts',(101.734378241932,11.3162372099778,47.7745882757927));
#110538=CARTESIAN_POINT('Ctrl Pts',(100.693739434446,11.006760540819,47.8377443492053));
#110539=CARTESIAN_POINT('Ctrl Pts',(100.383617743118,9.96631385291099,47.900900422618));
#110540=CARTESIAN_POINT('Ctrl Pts',(101.085000509175,9.13759977809068,47.9640564960307));
#110541=CARTESIAN_POINT('Ctrl Pts',(102.162396259481,9.27147971729114,48.0272125694433));
#110542=CARTESIAN_POINT('Ctrl Pts',(102.639623433236,10.2466505172619,48.090368642856));
#110543=CARTESIAN_POINT('Ctrl Pts',(102.084289484818,11.1795539926762,48.1535247162686));
#110544=CARTESIAN_POINT('Ctrl Pts',(100.999554008205,11.2249255640506,48.2166807896813));
#110545=CARTESIAN_POINT('Ctrl Pts',(100.368256052833,10.341660197854,48.2798368630939));
#110546=CARTESIAN_POINT('Ctrl Pts',(100.762369729322,9.33003697317457,48.3429929365066));
#110547=CARTESIAN_POINT('Ctrl Pts',(101.824841531871,9.10666087940736,48.4061490099193));
#110548=CARTESIAN_POINT('Ctrl Pts',(102.592938960673,9.87388585064706,48.469305083332));
#110549=CARTESIAN_POINT('Ctrl Pts',(102.37087635874,10.9366407851643,48.5324611567447));
#110550=CARTESIAN_POINT('Ctrl Pts',(101.359535576557,11.3318492113392,48.5956172301573));
#110551=CARTESIAN_POINT('Ctrl Pts',(100.475911403362,10.7017658986286,48.65877330357));
#110552=CARTESIAN_POINT('Ctrl Pts',(100.519228488975,9.61658704927828,48.7219293769826));
#110553=CARTESIAN_POINT('Ctrl Pts',(101.45308726074,9.06102988940963,48.7850854503953));
#110554=CARTESIAN_POINT('Ctrl Pts',(102.100393083241,9.37760418687212,48.8271894993371));
#110555=CARTESIAN_POINT('Ctrl Pts',(102.286356739692,9.6376401148372,48.848241523808));
#110556=CARTESIAN_POINT('Ctrl Pts',(100.534608987464,10.2001621159456,48.6877640831103));
#110557=CARTESIAN_POINT('Ctrl Pts',(100.53483984494,10.052869158678,48.6974260554069));
#110558=CARTESIAN_POINT('Ctrl Pts',(100.56702615616,9.90546817974631,48.7070880277034));
#110559=CARTESIAN_POINT('Ctrl Pts',(100.630581430873,9.77382549334327,48.71675));
#110560=CARTESIAN_POINT('',(101.070122622048,9.59889564972058,45.81675));
#110561=CARTESIAN_POINT('Ctrl Pts',(101.06918126624,9.59815671460027,45.81675));
#110562=CARTESIAN_POINT('Ctrl Pts',(101.05100744208,9.60730942634728,45.81675));
#110563=CARTESIAN_POINT('Ctrl Pts',(101.033276950503,9.61723877762716,45.81675));
#110564=CARTESIAN_POINT('Ctrl Pts',(101.016045603448,9.62793163066911,45.81675));
#110565=CARTESIAN_POINT('Ctrl Pts',(100.987725351354,9.64550566552492,45.81675));
#110566=CARTESIAN_POINT('Ctrl Pts',(100.960752251418,9.66513931578662,45.81675));
#110567=CARTESIAN_POINT('Ctrl Pts',(100.935188878082,9.6865866164717,45.81675));
#110568=CARTESIAN_POINT('Ctrl Pts',(100.92673957253,9.69367546168651,45.81675));
#110569=CARTESIAN_POINT('Ctrl Pts',(100.918444379411,9.70096282227849,45.81675));
#110570=CARTESIAN_POINT('Ctrl Pts',(100.910305929908,9.70844088554085,45.81675));
#110571=CARTESIAN_POINT('Ctrl Pts',(100.90377074013,9.71444578396391,45.81675));
#110572=CARTESIAN_POINT('Ctrl Pts',(100.897337734181,9.72057284008257,45.81675));
#110573=CARTESIAN_POINT('Ctrl Pts',(100.891016940649,9.72680896346648,45.81675));
#110574=CARTESIAN_POINT('Ctrl Pts',(100.865628216618,9.75185759301389,45.81675));
#110575=CARTESIAN_POINT('Ctrl Pts',(100.842008843511,9.77869772275828,45.81675));
#110576=CARTESIAN_POINT('Ctrl Pts',(100.820232138824,9.80704642891589,45.81675));
#110577=CARTESIAN_POINT('Ctrl Pts',(100.804421280313,9.82762885350541,45.81675));
#110578=CARTESIAN_POINT('Ctrl Pts',(100.789581999707,9.84900774438982,45.81675));
#110579=CARTESIAN_POINT('Ctrl Pts',(100.775750083582,9.87108979316409,45.81675));
#110580=CARTESIAN_POINT('Ctrl Pts',(100.771318045365,9.87816534821914,45.81675));
#110581=CARTESIAN_POINT('Ctrl Pts',(100.766991141235,9.88531075184123,45.81675));
#110582=CARTESIAN_POINT('Ctrl Pts',(100.762775647967,9.8925136012006,45.81675));
#110583=CARTESIAN_POINT('Ctrl Pts',(100.743699436389,9.92510838183202,45.81675));
#110584=CARTESIAN_POINT('Ctrl Pts',(100.726869763159,9.95892757967534,45.81675));
#110585=CARTESIAN_POINT('Ctrl Pts',(100.712366837593,9.99366976676314,45.81675));
#110586=CARTESIAN_POINT('Ctrl Pts',(100.69775415064,10.0286748904987,45.81675));
#110587=CARTESIAN_POINT('Ctrl Pts',(100.685502677547,10.0646180742379,45.81675));
#110588=CARTESIAN_POINT('Ctrl Pts',(100.675728219088,10.1012322885948,45.81675));
#110589=CARTESIAN_POINT('Ctrl Pts',(100.670605920794,10.1204199426764,45.81675));
#110590=CARTESIAN_POINT('Ctrl Pts',(100.6661645189,10.1397924682425,45.81675));
#110591=CARTESIAN_POINT('Ctrl Pts',(100.662425610055,10.1593143819321,45.81675));
#110592=CARTESIAN_POINT('Ctrl Pts',(100.660675925445,10.1684499862913,45.81675));
#110593=CARTESIAN_POINT('Ctrl Pts',(100.659080065457,10.1776200268081,45.81675));
#110594=CARTESIAN_POINT('Ctrl Pts',(100.657643384766,10.186799042495,45.81675));
#110595=CARTESIAN_POINT('Ctrl Pts',(100.651463417681,10.2262831221287,45.81675));
#110596=CARTESIAN_POINT('Ctrl Pts',(100.648206959382,10.2660191009013,45.81675));
#110597=CARTESIAN_POINT('Ctrl Pts',(100.647981555128,10.3056975413403,45.81675));
#110598=CARTESIAN_POINT('Ctrl Pts',(100.647767682598,10.3433460255231,45.81675));
#110599=CARTESIAN_POINT('Ctrl Pts',(100.650281763879,10.3809441015259,45.81675));
#110600=CARTESIAN_POINT('Ctrl Pts',(100.655348730347,10.4182963848193,45.81675));
#110601=CARTESIAN_POINT('Ctrl Pts',(100.657668255377,10.4353952854263,45.81675));
#110602=CARTESIAN_POINT('Ctrl Pts',(100.660523463249,10.4524428456175,45.81675));
#110603=CARTESIAN_POINT('Ctrl Pts',(100.663901041196,10.4694207875995,45.81675));
#110604=CARTESIAN_POINT('Ctrl Pts',(100.665711473481,10.4785212183748,45.81675));
#110605=CARTESIAN_POINT('Ctrl Pts',(100.667672025352,10.4876016486112,45.81675));
#110606=CARTESIAN_POINT('Ctrl Pts',(100.669780893868,10.4966592572468,45.81675));
#110607=CARTESIAN_POINT('Ctrl Pts',(100.671692007865,10.5048675085044,45.81675));
#110608=CARTESIAN_POINT('Ctrl Pts',(100.67372314753,10.5130491213257,45.81675));
#110609=CARTESIAN_POINT('Ctrl Pts',(100.675870729547,10.5211964448257,45.81675));
#110610=CARTESIAN_POINT('Ctrl Pts',(100.685965723623,10.559494019415,45.81675));
#110611=CARTESIAN_POINT('Ctrl Pts',(100.698638312468,10.5970716385837,45.81675));
#110612=CARTESIAN_POINT('Ctrl Pts',(100.713681335617,10.6337143830086,45.81675));
#110613=CARTESIAN_POINT('Ctrl Pts',(100.729073877235,10.6712085065637,45.81675));
#110614=CARTESIAN_POINT('Ctrl Pts',(100.746948457436,10.707724900083,45.81675));
#110615=CARTESIAN_POINT('Ctrl Pts',(100.7671375823,10.7430359407574,45.81675));
#110616=CARTESIAN_POINT('Ctrl Pts',(100.776822104117,10.7599742947513,45.81675));
#110617=CARTESIAN_POINT('Ctrl Pts',(100.787039985488,10.7766352285847,45.81675));
#110618=CARTESIAN_POINT('Ctrl Pts',(100.797776824513,10.7929926474574,45.81675));
#110619=CARTESIAN_POINT('Ctrl Pts',(100.8023027384,10.7998878117669,45.81675));
#110620=CARTESIAN_POINT('Ctrl Pts',(100.806920895886,10.8067290328366,45.81675));
#110621=CARTESIAN_POINT('Ctrl Pts',(100.811630349515,10.8135142946914,45.81675));
#110622=CARTESIAN_POINT('Ctrl Pts',(100.816583018343,10.8206499748645,45.81675));
#110623=CARTESIAN_POINT('Ctrl Pts',(100.821632129333,10.8277171478722,45.81675));
#110624=CARTESIAN_POINT('Ctrl Pts',(100.826772368825,10.8347089528894,45.81675));
#110625=CARTESIAN_POINT('Ctrl Pts',(100.851839075462,10.8688049372315,45.81675));
#110626=CARTESIAN_POINT('Ctrl Pts',(100.879093896518,10.9011455652106,45.81675));
#110627=CARTESIAN_POINT('Ctrl Pts',(100.908341133779,10.9314937196515,45.81675));
#110628=CARTESIAN_POINT('Ctrl Pts',(100.937389369515,10.9616353818016,45.81675));
#110629=CARTESIAN_POINT('Ctrl Pts',(100.968403539212,10.9898127722535,45.81675));
#110630=CARTESIAN_POINT('Ctrl Pts',(101.001239283439,11.0157768332061,45.81675));
#110631=CARTESIAN_POINT('Ctrl Pts',(101.024856698805,11.0344517262696,45.81675));
#110632=CARTESIAN_POINT('Ctrl Pts',(101.04941748246,11.051981301149,45.81675));
#110633=CARTESIAN_POINT('Ctrl Pts',(101.074880871485,11.0682622236804,45.81675));
#110634=CARTESIAN_POINT('Ctrl Pts',(101.06918126624,9.59815671460025,45.81675));
#110635=CARTESIAN_POINT('Ctrl Pts',(101.251697602369,9.46914978142767,45.8360755654767));
#110636=CARTESIAN_POINT('Ctrl Pts',(101.765370568999,9.38071711773372,45.8764531554243));
#110637=CARTESIAN_POINT('Ctrl Pts',(102.33569099053,9.95154749830959,45.9378827698427));
#110638=CARTESIAN_POINT('Ctrl Pts',(102.165084835389,10.7638419256677,46.0010388432554));
#110639=CARTESIAN_POINT('Ctrl Pts',(101.391765482636,11.0651152556269,46.0641949166681));
#110640=CARTESIAN_POINT('Ctrl Pts',(100.838565297627,10.669798683291,46.1159394886837));
#110641=CARTESIAN_POINT('Ctrl Pts',(100.761892086014,10.3124888878941,46.1466320362285));
#110642=CARTESIAN_POINT('Ctrl Pts',(100.762116465727,10.2001659521564,46.1562725593024));
#110643=CARTESIAN_POINT('Origin',(101.5,10.2,45.81675));
#110644=CARTESIAN_POINT('',(100.53325,10.2,45.81675));
#110645=CARTESIAN_POINT('Origin',(101.5,10.2,45.81675));
#110646=CARTESIAN_POINT('Origin',(101.5,10.2,45.81675));
#110647=CARTESIAN_POINT('',(101.929877377952,9.59889564972063,45.81675));
#110648=CARTESIAN_POINT('Ctrl Pts',(101.926174511012,11.0694185813664,45.81675));
#110649=CARTESIAN_POINT('Ctrl Pts',(101.948303515656,11.0554206324422,45.81675));
#110650=CARTESIAN_POINT('Ctrl Pts',(101.969784534031,11.0404900380945,45.81675));
#110651=CARTESIAN_POINT('Ctrl Pts',(101.990548001762,11.0246241502298,45.81675));
#110652=CARTESIAN_POINT('Ctrl Pts',(102.020338981568,11.001860113359,45.81675));
#110653=CARTESIAN_POINT('Ctrl Pts',(102.048654091966,10.977171031833,45.81675));
#110654=CARTESIAN_POINT('Ctrl Pts',(102.075396317082,10.9507539194945,45.81675));
#110655=CARTESIAN_POINT('Ctrl Pts',(102.085770950475,10.940505413447,45.81675));
#110656=CARTESIAN_POINT('Ctrl Pts',(102.095908554493,10.9299966686515,45.81675));
#110657=CARTESIAN_POINT('Ctrl Pts',(102.105802268045,10.919238713229,45.81675));
#110658=CARTESIAN_POINT('Ctrl Pts',(102.11528326565,10.9089295255755,45.81675));
#110659=CARTESIAN_POINT('Ctrl Pts',(102.124543638292,10.8983871337153,45.81675));
#110660=CARTESIAN_POINT('Ctrl Pts',(102.13355685089,10.8876459051365,45.81675));
#110661=CARTESIAN_POINT('Ctrl Pts',(102.16038181785,10.8556780469933,45.81675));
#110662=CARTESIAN_POINT('Ctrl Pts',(102.185054054778,10.8219178398454,45.81675));
#110663=CARTESIAN_POINT('Ctrl Pts',(102.207435827403,10.7866403802508,45.81675));
#110664=CARTESIAN_POINT('Ctrl Pts',(102.220417101675,10.7661796961809,45.81675));
#110665=CARTESIAN_POINT('Ctrl Pts',(102.232626988819,10.7452082230353,45.81675));
#110666=CARTESIAN_POINT('Ctrl Pts',(102.244030679305,10.723778160377,45.81675));
#110667=CARTESIAN_POINT('Ctrl Pts',(102.248338908853,10.7156820419094,45.81675));
#110668=CARTESIAN_POINT('Ctrl Pts',(102.252532009947,10.7075204688054,45.81675));
#110669=CARTESIAN_POINT('Ctrl Pts',(102.256607874645,10.699296265029,45.81675));
#110670=CARTESIAN_POINT('Ctrl Pts',(102.260443278273,10.6915572591171,45.81675));
#110671=CARTESIAN_POINT('Ctrl Pts',(102.26417251832,10.6837673823401,45.81675));
#110672=CARTESIAN_POINT('Ctrl Pts',(102.267791118971,10.6759361610197,45.81675));
#110673=CARTESIAN_POINT('Ctrl Pts',(102.284621354702,10.6395128820778,45.81675));
#110674=CARTESIAN_POINT('Ctrl Pts',(102.299085291605,10.6021495300482,45.81675));
#110675=CARTESIAN_POINT('Ctrl Pts',(102.311054891601,10.56409143824,45.81675));
#110676=CARTESIAN_POINT('Ctrl Pts',(102.322747625754,10.5269136586982,45.81675));
#110677=CARTESIAN_POINT('Ctrl Pts',(102.332060160583,10.4890718203185,45.81675));
#110678=CARTESIAN_POINT('Ctrl Pts',(102.338824931882,10.4507967026999,45.81675));
#110679=CARTESIAN_POINT('Ctrl Pts',(102.342070973874,10.4324305771433,45.81675));
#110680=CARTESIAN_POINT('Ctrl Pts',(102.344729661393,10.4139648195556,45.81675));
#110681=CARTESIAN_POINT('Ctrl Pts',(102.346778322229,10.3954261823324,45.81675));
#110682=CARTESIAN_POINT('Ctrl Pts',(102.347681092635,10.3872568783932,45.81675));
#110683=CARTESIAN_POINT('Ctrl Pts',(102.348465369219,10.3790734369715,45.81675));
#110684=CARTESIAN_POINT('Ctrl Pts',(102.349129039225,10.3708782251626,45.81675));
#110685=CARTESIAN_POINT('Ctrl Pts',(102.349773484486,10.3629204067042,45.81675));
#110686=CARTESIAN_POINT('Ctrl Pts',(102.35030368,10.354957121918,45.81675));
#110687=CARTESIAN_POINT('Ctrl Pts',(102.350717915998,10.3469980024824,45.81675));
#110688=CARTESIAN_POINT('Ctrl Pts',(102.35265365805,10.3098047063077,45.81675));
#110689=CARTESIAN_POINT('Ctrl Pts',(102.352065311248,10.2726502636654,45.81675));
#110690=CARTESIAN_POINT('Ctrl Pts',(102.348813955523,10.2357429191864,45.81675));
#110691=CARTESIAN_POINT('Ctrl Pts',(102.345848851563,10.2020849246283,45.81675));
#110692=CARTESIAN_POINT('Ctrl Pts',(102.34066781952,10.1686319597464,45.81675));
#110693=CARTESIAN_POINT('Ctrl Pts',(102.333366548057,10.1355578610452,45.81675));
#110694=CARTESIAN_POINT('Ctrl Pts',(102.32949095817,10.1180017897395,45.81675));
#110695=CARTESIAN_POINT('Ctrl Pts',(102.325017514806,10.1005527426951,45.81675));
#110696=CARTESIAN_POINT('Ctrl Pts',(102.319957858714,10.0832390817281,45.81675));
#110697=CARTESIAN_POINT('Ctrl Pts',(102.3167422658,10.0722356292209,45.81675));
#110698=CARTESIAN_POINT('Ctrl Pts',(102.313289863631,10.0612868959364,45.81675));
#110699=CARTESIAN_POINT('Ctrl Pts',(102.309603327023,10.0504005939673,45.81675));
#110700=CARTESIAN_POINT('Ctrl Pts',(102.306983713134,10.0426649030276,45.81675));
#110701=CARTESIAN_POINT('Ctrl Pts',(102.30424829546,10.0349680849826,45.81675));
#110702=CARTESIAN_POINT('Ctrl Pts',(102.301400862263,10.027318306124,45.81675));
#110703=CARTESIAN_POINT('Ctrl Pts',(102.288388975775,9.99236118955888,45.81675));
#110704=CARTESIAN_POINT('Ctrl Pts',(102.2730281174,9.95834474272888,45.81675));
#110705=CARTESIAN_POINT('Ctrl Pts',(102.255462063125,9.92549991214507,45.81675));
#110706=CARTESIAN_POINT('Ctrl Pts',(102.238114273384,9.89306319037982,45.81675));
#110707=CARTESIAN_POINT('Ctrl Pts',(102.218614774453,9.86176827859395,45.81675));
#110708=CARTESIAN_POINT('Ctrl Pts',(102.197070005432,9.83187633235799,45.81675));
#110709=CARTESIAN_POINT('Ctrl Pts',(102.18688854255,9.81775022402949,45.81675));
#110710=CARTESIAN_POINT('Ctrl Pts',(102.176249943744,9.80393807671464,45.81675));
#110711=CARTESIAN_POINT('Ctrl Pts',(102.165163835632,9.79047134114548,45.81675));
#110712=CARTESIAN_POINT('Ctrl Pts',(102.159106008442,9.78311265800195,45.81675));
#110713=CARTESIAN_POINT('Ctrl Pts',(102.15291222714,9.77585481388914,45.81675));
#110714=CARTESIAN_POINT('Ctrl Pts',(102.146601044657,9.76872176517651,45.81675));
#110715=CARTESIAN_POINT('Ctrl Pts',(102.123196147213,9.74226899281033,45.81675));
#110716=CARTESIAN_POINT('Ctrl Pts',(102.09813586298,9.71747444018442,45.81675));
#110717=CARTESIAN_POINT('Ctrl Pts',(102.071528567788,9.69456011526773,45.81675));
#110718=CARTESIAN_POINT('Ctrl Pts',(102.04589024096,9.67248027035965,45.81675));
#110719=CARTESIAN_POINT('Ctrl Pts',(102.018814675174,9.65214581235937,45.81675));
#110720=CARTESIAN_POINT('Ctrl Pts',(101.990382970443,9.63380011029726,45.81675));
#110721=CARTESIAN_POINT('Ctrl Pts',(101.970846814486,9.62119430631815,45.81675));
#110722=CARTESIAN_POINT('Ctrl Pts',(101.95067004842,9.60952839844149,45.81675));
#110723=CARTESIAN_POINT('Ctrl Pts',(101.929877377952,9.59889564972062,45.81675));
#110724=CARTESIAN_POINT('Origin',(101.5,10.2,45.81675));
#110725=CARTESIAN_POINT('Origin',(101.5,10.2,45.0772274406976));
#110726=CARTESIAN_POINT('Ctrl Pts',(101.929877377952,9.59889564972062,45.81675));
#110727=CARTESIAN_POINT('Ctrl Pts',(102.128653225655,9.74104940417406,45.8378020244709));
#110728=CARTESIAN_POINT('Ctrl Pts',(102.370647903658,10.23586098604,45.8799060734127));
#110729=CARTESIAN_POINT('Ctrl Pts',(101.945970715424,10.9497182652191,45.9430621468254));
#110730=CARTESIAN_POINT('Ctrl Pts',(101.116441674876,10.9828306195272,46.006218220238));
#110731=CARTESIAN_POINT('Ctrl Pts',(100.775380687848,10.5045291878666,46.0509399848621));
#110732=CARTESIAN_POINT('Ctrl Pts',(100.759998367851,10.2308105930258,46.0746097250153));
#110733=CARTESIAN_POINT('Ctrl Pts',(100.760229243717,10.2005121657882,46.0772274406976));
#110734=CARTESIAN_POINT('Ctrl Pts',(102.062359885163,9.41364326030773,45.6852584761921));
#110735=CARTESIAN_POINT('Ctrl Pts',(102.322395813128,9.5996069167595,45.706310500663));
#110736=CARTESIAN_POINT('Ctrl Pts',(102.638970041762,10.2469128663792,45.7484145496048));
#110737=CARTESIAN_POINT('Ctrl Pts',(102.083412975827,11.1807714924229,45.8115706230174));
#110738=CARTESIAN_POINT('Ctrl Pts',(100.998234085503,11.2240886352204,45.8747266964301));
#110739=CARTESIAN_POINT('Ctrl Pts',(100.36815077501,10.3404644127608,45.9378827698427));
#110740=CARTESIAN_POINT('Ctrl Pts',(100.763359203152,9.32912363564403,46.0010388432554));
#110741=CARTESIAN_POINT('Ctrl Pts',(101.826114154338,9.10706101956114,46.0641949166681));
#110742=CARTESIAN_POINT('Ctrl Pts',(102.593339136526,9.875158465447,46.1273509900807));
#110743=CARTESIAN_POINT('Ctrl Pts',(102.369963039459,10.9376302803438,46.1905070634934));
#110744=CARTESIAN_POINT('Ctrl Pts',(101.358339800128,11.3317439642367,46.2536631369061));
#110745=CARTESIAN_POINT('Ctrl Pts',(100.475074420974,10.7004459987923,46.3168192103187));
#110746=CARTESIAN_POINT('Ctrl Pts',(100.520445993066,9.61571050681813,46.3799752837314));
#110747=CARTESIAN_POINT('Ctrl Pts',(101.453349482045,9.06037655007097,46.4431313571441));
#110748=CARTESIAN_POINT('Ctrl Pts',(102.428520296253,9.53760373090416,46.5062874305568));
#110749=CARTESIAN_POINT('Ctrl Pts',(102.562400237392,10.6149994968546,46.5694435039694));
#110750=CARTESIAN_POINT('Ctrl Pts',(101.733686150498,11.3163822731671,46.6325995773821));
#110751=CARTESIAN_POINT('Ctrl Pts',(100.693239447419,11.0062605773023,46.6957556507947));
#110752=CARTESIAN_POINT('Ctrl Pts',(100.383762773751,9.96562175465318,46.7589117242074));
#110753=CARTESIAN_POINT('Ctrl Pts',(101.085659310413,9.13734272939962,46.8220677976201));
#110754=CARTESIAN_POINT('Ctrl Pts',(102.16297161691,9.2718904534268,46.8852238710327));
#110755=CARTESIAN_POINT('Ctrl Pts',(102.639594659967,10.2473572067212,46.9483799444454));
#110756=CARTESIAN_POINT('Ctrl Pts',(102.083681369551,11.179915685355,47.0115360178581));
#110757=CARTESIAN_POINT('Ctrl Pts',(100.998920199893,11.2246158924639,47.0746920912707));
#110758=CARTESIAN_POINT('Ctrl Pts',(100.36816528026,10.3409569442653,47.1378481646833));
#110759=CARTESIAN_POINT('Ctrl Pts',(100.76291575382,9.32958314206829,47.2010042380961));
#110760=CARTESIAN_POINT('Ctrl Pts',(101.825505670709,9.10685556705321,47.2641603115086));
#110761=CARTESIAN_POINT('Ctrl Pts',(102.593169292758,9.87457782722072,47.3273163849214));
#110762=CARTESIAN_POINT('Ctrl Pts',(102.370360554826,10.9371507282558,47.390472458334));
#110763=CARTESIAN_POINT('Ctrl Pts',(101.358956604738,11.3318239504036,47.4536285317468));
#110764=CARTESIAN_POINT('Ctrl Pts',(100.47534583524,10.701001534836,47.5167846051593));
#110765=CARTESIAN_POINT('Ctrl Pts',(100.520128903871,9.61624378651841,47.5799406785721));
#110766=CARTESIAN_POINT('Ctrl Pts',(101.452729831205,9.06040172064943,47.6430967519847));
#110767=CARTESIAN_POINT('Ctrl Pts',(102.428160197997,9.53709928754952,47.7062528253974));
#110768=CARTESIAN_POINT('Ctrl Pts',(102.562625588385,10.6144218330213,47.76940889881));
#110769=CARTESIAN_POINT('Ctrl Pts',(101.734293047928,11.3162551744531,47.8325649722227));
#110770=CARTESIAN_POINT('Ctrl Pts',(100.69367766951,11.0066988640243,47.8957210456354));
#110771=CARTESIAN_POINT('Ctrl Pts',(100.383635856821,9.96622879074344,47.958877119048));
#110772=CARTESIAN_POINT('Ctrl Pts',(101.085081076298,9.13756762516558,48.0220331924607));
#110773=CARTESIAN_POINT('Ctrl Pts',(102.162468389238,9.27153122103628,48.0851892658733));
#110774=CARTESIAN_POINT('Ctrl Pts',(102.639617388232,10.2467356529103,48.148345339286));
#110775=CARTESIAN_POINT('Ctrl Pts',(102.084219860843,11.1796026106038,48.2115014126987));
#110776=CARTESIAN_POINT('Ctrl Pts',(100.999464920921,11.2248790780578,48.2746574861114));
#110777=CARTESIAN_POINT('Ctrl Pts',(100.368267674707,10.3415909619596,48.337813559524));
#110778=CARTESIAN_POINT('Ctrl Pts',(100.762389466428,9.32994482569277,48.4009696329367));
#110779=CARTESIAN_POINT('Ctrl Pts',(101.825022259655,9.1067601132002,48.4641257063494));
#110780=CARTESIAN_POINT('Ctrl Pts',(102.592762281192,9.87381422081543,48.527281779762));
#110781=CARTESIAN_POINT('Ctrl Pts',(102.371248886038,10.9370270003807,48.5904378531747));
#110782=CARTESIAN_POINT('Ctrl Pts',(101.358621245203,11.3311346607519,48.6535939265874));
#110783=CARTESIAN_POINT('Ctrl Pts',(100.772318051784,10.9122399245294,48.6956979755291));
#110784=CARTESIAN_POINT('Ctrl Pts',(100.631737776319,10.6251191285149,48.71675));
#110785=CARTESIAN_POINT('Ctrl Pts',(102.018199049426,9.47539405677869,45.7290889841281));
#110786=CARTESIAN_POINT('Ctrl Pts',(102.257814950637,9.64675441256435,45.7501410085989));
#110787=CARTESIAN_POINT('Ctrl Pts',(102.549529329061,10.2432289062661,45.7922450575407));
#110788=CARTESIAN_POINT('Ctrl Pts',(102.037598889026,11.1037537500216,45.8554011309534));
#110789=CARTESIAN_POINT('Ctrl Pts',(101.037636615294,11.143669296656,45.918557204366));
#110790=CARTESIAN_POINT('Ctrl Pts',(100.457032306255,10.3294340636508,45.9817132777787));
#110791=CARTESIAN_POINT('Ctrl Pts',(100.821205920325,9.39751156495429,46.0448693511914));
#110792=CARTESIAN_POINT('Ctrl Pts',(101.800505155579,9.19288701828364,46.108025424604));
#110793=CARTESIAN_POINT('Ctrl Pts',(102.507481714461,9.90066752828449,46.1711814980167));
#110794=CARTESIAN_POINT('Ctrl Pts',(102.301646831464,10.8797058612943,46.2343375714294));
#110795=CARTESIAN_POINT('Ctrl Pts',(101.369464051665,11.2428706988786,46.297493644842));
#110796=CARTESIAN_POINT('Ctrl Pts',(100.555559482821,10.661147118963,46.3606497182547));
#110797=CARTESIAN_POINT('Ctrl Pts',(100.597368129117,9.66159342452252,46.4238057916673));
#110798=CARTESIAN_POINT('Ctrl Pts',(101.457012840536,9.14986857342115,46.48696186508));
#110799=CARTESIAN_POINT('Ctrl Pts',(102.355605720795,9.58962019510088,46.5501179384927));
#110800=CARTESIAN_POINT('Ctrl Pts',(102.478972376323,10.5824105354173,46.6132740119053));
#110801=CARTESIAN_POINT('Ctrl Pts',(101.715335311509,11.2287153262785,46.6764300853181));
#110802=CARTESIAN_POINT('Ctrl Pts',(100.756592508655,10.9429467779814,46.7395861587306));
#110803=CARTESIAN_POINT('Ctrl Pts',(100.471418330437,9.98402694226726,46.8027422321434));
#110804=CARTESIAN_POINT('Ctrl Pts',(101.118196537222,9.2207907746989,46.865898305556));
#110805=CARTESIAN_POINT('Ctrl Pts',(102.110909971965,9.34477277365162,46.9290543789687));
#110806=CARTESIAN_POINT('Ctrl Pts',(102.550104897427,10.2436383535773,46.9922104523813));
#110807=CARTESIAN_POINT('Ctrl Pts',(102.037846206404,11.1029651475256,47.0553665257941));
#110808=CARTESIAN_POINT('Ctrl Pts',(101.03826885069,11.1441551495939,47.1185225992067));
#110809=CARTESIAN_POINT('Ctrl Pts',(100.45704567244,10.3298879177826,47.1816786726194));
#110810=CARTESIAN_POINT('Ctrl Pts',(100.820797294055,9.39793498738988,47.244834746032));
#110811=CARTESIAN_POINT('Ctrl Pts',(101.799944454778,9.19269769949131,47.3079908194447));
#110812=CARTESIAN_POINT('Ctrl Pts',(102.507325208136,9.90013248625029,47.3711468928574));
#110813=CARTESIAN_POINT('Ctrl Pts',(102.302013130859,10.8792639673351,47.43430296627));
#110814=CARTESIAN_POINT('Ctrl Pts',(101.37003242002,11.2429444039147,47.4974590396827));
#110815=CARTESIAN_POINT('Ctrl Pts',(100.555809583546,10.6616590300316,47.5606151130953));
#110816=CARTESIAN_POINT('Ctrl Pts',(100.59707594021,9.66208482698747,47.623771186508));
#110817=CARTESIAN_POINT('Ctrl Pts',(101.456441849459,9.14989176741164,47.6869272599207));
#110818=CARTESIAN_POINT('Ctrl Pts',(102.355273900232,9.58915536452929,47.7500833333333));
#110819=CARTESIAN_POINT('Ctrl Pts',(102.479180031018,10.5818782342037,47.813239406746));
#110820=CARTESIAN_POINT('Ctrl Pts',(101.715894550673,11.2285982083358,47.8763954801587));
#110821=CARTESIAN_POINT('Ctrl Pts',(100.756996318167,10.9433506470493,47.9395515535714));
#110822=CARTESIAN_POINT('Ctrl Pts',(100.471301380003,9.98458630920156,48.002707626984));
#110823=CARTESIAN_POINT('Ctrl Pts',(101.11766371051,9.22099800991466,48.0658637003967));
#110824=CARTESIAN_POINT('Ctrl Pts',(102.110446261611,9.34444175095921,48.1290197738093));
#110825=CARTESIAN_POINT('Ctrl Pts',(102.550125840893,10.2430656089657,48.192175847222));
#110826=CARTESIAN_POINT('Ctrl Pts',(102.038342411207,11.1026766578187,48.2553319206346));
#110827=CARTESIAN_POINT('Ctrl Pts',(101.038770796021,11.144397667825,48.3184879940474));
#110828=CARTESIAN_POINT('Ctrl Pts',(100.457140026085,10.3304721475173,48.38164406746));
#110829=CARTESIAN_POINT('Ctrl Pts',(100.820312334809,9.39826826882645,48.4448001408727));
#110830=CARTESIAN_POINT('Ctrl Pts',(101.799499004889,9.19260974141109,48.5079562142853));
#110831=CARTESIAN_POINT('Ctrl Pts',(102.506950158257,9.89942884410974,48.571112287698));
#110832=CARTESIAN_POINT('Ctrl Pts',(102.302831703452,10.8791499555271,48.6342683611106));
#110833=CARTESIAN_POINT('Ctrl Pts',(101.369723395502,11.242309242603,48.6974244345234));
#110834=CARTESIAN_POINT('Ctrl Pts',(100.829461251062,10.8563093520575,48.7395284834651));
#110835=CARTESIAN_POINT('Ctrl Pts',(100.699920423141,10.5917354955456,48.760580507936));
#110836=CARTESIAN_POINT('Ctrl Pts',(101.974038213689,9.53714485324965,45.772919492064));
#110837=CARTESIAN_POINT('Ctrl Pts',(102.193234088146,9.69390190836921,45.7939715165349));
#110838=CARTESIAN_POINT('Ctrl Pts',(102.46008861636,10.2395449461531,45.8360755654767));
#110839=CARTESIAN_POINT('Ctrl Pts',(101.991784802225,11.0267360076204,45.8992316388894));
#110840=CARTESIAN_POINT('Ctrl Pts',(101.077039145085,11.0632499580916,45.962387712302));
#110841=CARTESIAN_POINT('Ctrl Pts',(100.545913837499,10.3184037145408,46.0255437857147));
#110842=CARTESIAN_POINT('Ctrl Pts',(100.879052637499,9.46589949426454,46.0886998591273));
#110843=CARTESIAN_POINT('Ctrl Pts',(101.77489615682,9.27871301700615,46.15185593254));
#110844=CARTESIAN_POINT('Ctrl Pts',(102.421624292396,9.92617659112199,46.2150120059527));
#110845=CARTESIAN_POINT('Ctrl Pts',(102.23333062347,10.8217814422448,46.2781680793653));
#110846=CARTESIAN_POINT('Ctrl Pts',(101.380588303203,11.1539974335205,46.3413241527781));
#110847=CARTESIAN_POINT('Ctrl Pts',(100.636044544668,10.6218482391337,46.4044802261907));
#110848=CARTESIAN_POINT('Ctrl Pts',(100.674290265167,9.70747634222691,46.4676362996034));
#110849=CARTESIAN_POINT('Ctrl Pts',(101.460676199027,9.23936059677131,46.530792373016));
#110850=CARTESIAN_POINT('Ctrl Pts',(102.282691145337,9.64163665929762,46.5939484464287));
#110851=CARTESIAN_POINT('Ctrl Pts',(102.395544515254,10.54982157398,46.6571045198413));
#110852=CARTESIAN_POINT('Ctrl Pts',(101.696984472521,11.1410483793898,46.720260593254));
#110853=CARTESIAN_POINT('Ctrl Pts',(100.819945569891,10.8796329786604,46.7834166666667));
#110854=CARTESIAN_POINT('Ctrl Pts',(100.559073887122,10.0024321298813,46.8465727400793));
#110855=CARTESIAN_POINT('Ctrl Pts',(101.150733764031,9.30423881999818,46.909728813492));
#110856=CARTESIAN_POINT('Ctrl Pts',(102.05884832702,9.41765509387644,46.9728848869047));
#110857=CARTESIAN_POINT('Ctrl Pts',(102.460615134887,10.2399195004333,47.0360409603174));
#110858=CARTESIAN_POINT('Ctrl Pts',(101.992011043258,11.0260146096962,47.09919703373));
#110859=CARTESIAN_POINT('Ctrl Pts',(101.077617501487,11.063694406724,47.1623531071427));
#110860=CARTESIAN_POINT('Ctrl Pts',(100.54592606462,10.3188188912999,47.2255091805553));
#110861=CARTESIAN_POINT('Ctrl Pts',(100.878678834291,9.46628683271147,47.288665253968));
#110862=CARTESIAN_POINT('Ctrl Pts',(101.774383238847,9.27853983192942,47.3518213273807));
#110863=CARTESIAN_POINT('Ctrl Pts',(102.421481123513,9.92568714527985,47.4149774007933));
#110864=CARTESIAN_POINT('Ctrl Pts',(102.233665706891,10.8213772064144,47.478133474206));
#110865=CARTESIAN_POINT('Ctrl Pts',(101.381108235302,11.1540648574258,47.5412895476186));
#110866=CARTESIAN_POINT('Ctrl Pts',(100.636273331852,10.6223165252273,47.6044456210313));
#110867=CARTESIAN_POINT('Ctrl Pts',(100.67402297655,9.70792586745655,47.667601694444));
#110868=CARTESIAN_POINT('Ctrl Pts',(101.460153867714,9.23938181417384,47.7307577678567));
#110869=CARTESIAN_POINT('Ctrl Pts',(102.282387602466,9.64121144150907,47.7939138412693));
#110870=CARTESIAN_POINT('Ctrl Pts',(102.395734473651,10.5493346353862,47.857069914682));
#110871=CARTESIAN_POINT('Ctrl Pts',(101.697496053417,11.1409412422185,47.9202259880946));
#110872=CARTESIAN_POINT('Ctrl Pts',(100.820314966825,10.8800024300744,47.9833820615074));
#110873=CARTESIAN_POINT('Ctrl Pts',(100.558966903185,10.0029438276597,48.04653813492));
#110874=CARTESIAN_POINT('Ctrl Pts',(101.150246344722,9.30442839466375,48.1096942083327));
#110875=CARTESIAN_POINT('Ctrl Pts',(102.058424133985,9.41735228088214,48.1728502817453));
#110876=CARTESIAN_POINT('Ctrl Pts',(102.460634293554,10.2393955650211,48.236006355158));
#110877=CARTESIAN_POINT('Ctrl Pts',(101.992464961571,11.0257507050336,48.2991624285706));
#110878=CARTESIAN_POINT('Ctrl Pts',(101.078076671122,11.0639162575922,48.3623185019834));
#110879=CARTESIAN_POINT('Ctrl Pts',(100.546012377464,10.319353333075,48.425474575396));
#110880=CARTESIAN_POINT('Ctrl Pts',(100.878235203189,9.46659171196013,48.4886306488087));
#110881=CARTESIAN_POINT('Ctrl Pts',(101.773975750122,9.27845936962199,48.5517867222213));
#110882=CARTESIAN_POINT('Ctrl Pts',(102.421138035323,9.92504346740403,48.614942795634));
#110883=CARTESIAN_POINT('Ctrl Pts',(102.234414520866,10.8212729106735,48.6780988690466));
#110884=CARTESIAN_POINT('Ctrl Pts',(101.380825545801,11.1534838244542,48.7412549424593));
#110885=CARTESIAN_POINT('Ctrl Pts',(100.88660445034,10.8003787795856,48.7833589914011));
#110886=CARTESIAN_POINT('Ctrl Pts',(100.768103069962,10.5583518625763,48.804411015872));
#110887=CARTESIAN_POINT('Ctrl Pts',(101.929877377952,9.59889564972062,45.81675));
#110888=CARTESIAN_POINT('Ctrl Pts',(102.128653225655,9.74104940417406,45.8378020244709));
#110889=CARTESIAN_POINT('Ctrl Pts',(102.370647903658,10.23586098604,45.8799060734127));
#110890=CARTESIAN_POINT('Ctrl Pts',(101.945970715424,10.9497182652191,45.9430621468254));
#110891=CARTESIAN_POINT('Ctrl Pts',(101.116441674876,10.9828306195272,46.006218220238));
#110892=CARTESIAN_POINT('Ctrl Pts',(100.634795368743,10.3073733654308,46.0693742936507));
#110893=CARTESIAN_POINT('Ctrl Pts',(100.936899354672,9.53428742357479,46.1325303670633));
#110894=CARTESIAN_POINT('Ctrl Pts',(101.749287158062,9.36453901572865,46.195686440476));
#110895=CARTESIAN_POINT('Ctrl Pts',(102.335766870331,9.95168565395949,46.2588425138887));
#110896=CARTESIAN_POINT('Ctrl Pts',(102.165014415475,10.7638570231953,46.3219985873013));
#110897=CARTESIAN_POINT('Ctrl Pts',(101.39171255474,11.0651241681623,46.385154660714));
#110898=CARTESIAN_POINT('Ctrl Pts',(100.716529606516,10.5825493593044,46.4483107341266));
#110899=CARTESIAN_POINT('Ctrl Pts',(100.751212401217,9.7533592599313,46.5114668075394));
#110900=CARTESIAN_POINT('Ctrl Pts',(101.464339557519,9.32885262012148,46.574622880952));
#110901=CARTESIAN_POINT('Ctrl Pts',(102.209776569879,9.69365312349436,46.6377789543647));
#110902=CARTESIAN_POINT('Ctrl Pts',(102.312116654185,10.5172326125426,46.7009350277773));
#110903=CARTESIAN_POINT('Ctrl Pts',(101.678633633533,11.0533814325012,46.76409110119));
#110904=CARTESIAN_POINT('Ctrl Pts',(100.883298631127,10.8163191793394,46.8272471746026));
#110905=CARTESIAN_POINT('Ctrl Pts',(100.646729443808,10.0208373174954,46.8904032480153));
#110906=CARTESIAN_POINT('Ctrl Pts',(101.18327099084,9.38768686529745,46.953559321428));
#110907=CARTESIAN_POINT('Ctrl Pts',(102.006786682075,9.49053741410128,47.0167153948406));
#110908=CARTESIAN_POINT('Ctrl Pts',(102.371125372346,10.2362006472893,47.0798714682533));
#110909=CARTESIAN_POINT('Ctrl Pts',(101.946175880112,10.9490640718669,47.143027541666));
#110910=CARTESIAN_POINT('Ctrl Pts',(101.116966152284,10.983233663854,47.2061836150786));
#110911=CARTESIAN_POINT('Ctrl Pts',(100.6348064568,10.3077498648172,47.2693396884913));
#110912=CARTESIAN_POINT('Ctrl Pts',(100.936560374526,9.53463867803306,47.332495761904));
#110913=CARTESIAN_POINT('Ctrl Pts',(101.748822022916,9.36438196436754,47.3956518353166));
#110914=CARTESIAN_POINT('Ctrl Pts',(102.335637038891,9.95124180430941,47.4588079087293));
#110915=CARTESIAN_POINT('Ctrl Pts',(102.165318282924,10.7634904454937,47.521963982142));
#110916=CARTESIAN_POINT('Ctrl Pts',(101.392184050584,11.0651853109369,47.5851200555546));
#110917=CARTESIAN_POINT('Ctrl Pts',(100.716737080157,10.5829740204229,47.6482761289673));
#110918=CARTESIAN_POINT('Ctrl Pts',(100.750970012889,9.75376690792562,47.71143220238));
#110919=CARTESIAN_POINT('Ctrl Pts',(101.463865885969,9.32887186093604,47.7745882757927));
#110920=CARTESIAN_POINT('Ctrl Pts',(102.209501304701,9.69326751848885,47.8377443492053));
#110921=CARTESIAN_POINT('Ctrl Pts',(102.312288916283,10.5167910365686,47.900900422618));
#110922=CARTESIAN_POINT('Ctrl Pts',(101.679097556161,11.0532842761012,47.9640564960306));
#110923=CARTESIAN_POINT('Ctrl Pts',(100.883633615483,10.8166542130995,48.0272125694433));
#110924=CARTESIAN_POINT('Ctrl Pts',(100.646632426367,10.0213013461178,48.0903686428559));
#110925=CARTESIAN_POINT('Ctrl Pts',(101.182828978934,9.38785877941283,48.1535247162687));
#110926=CARTESIAN_POINT('Ctrl Pts',(102.006402006358,9.49026281080507,48.2166807896812));
#110927=CARTESIAN_POINT('Ctrl Pts',(102.371142746215,10.2357255210765,48.279836863094));
#110928=CARTESIAN_POINT('Ctrl Pts',(101.946587511935,10.9488247522485,48.3429929365066));
#110929=CARTESIAN_POINT('Ctrl Pts',(101.117382546223,10.9834348473594,48.4061490099193));
#110930=CARTESIAN_POINT('Ctrl Pts',(100.634884728842,10.3082345186327,48.4693050833319));
#110931=CARTESIAN_POINT('Ctrl Pts',(100.93615807157,9.53491515509381,48.5324611567447));
#110932=CARTESIAN_POINT('Ctrl Pts',(101.748452495356,9.36430899783289,48.5956172301573));
#110933=CARTESIAN_POINT('Ctrl Pts',(102.335325912388,9.95065809069832,48.65877330357));
#110934=CARTESIAN_POINT('Ctrl Pts',(102.16599733828,10.7633958658199,48.7219293769826));
#110935=CARTESIAN_POINT('Ctrl Pts',(101.3919276961,11.0646584063053,48.7850854503953));
#110936=CARTESIAN_POINT('Ctrl Pts',(100.943747649618,10.7444482071137,48.8271894993371));
#110937=CARTESIAN_POINT('Ctrl Pts',(100.836285716783,10.524968229607,48.848241523808));
#110938=CARTESIAN_POINT('Origin',(101.875277674973,10.85,49.65));
#110939=CARTESIAN_POINT('',(101.875277674973,10.85,49.65));
#110940=CARTESIAN_POINT('',(102.250555349947,10.2,49.65));
#110941=CARTESIAN_POINT('',(101.969097093717,10.6875,49.65));
#110942=CARTESIAN_POINT('',(101.875277674973,10.85,48.95));
#110943=CARTESIAN_POINT('',(101.875277674973,10.85,49.65));
#110944=CARTESIAN_POINT('',(102.250555349947,10.2,48.95));
#110945=CARTESIAN_POINT('',(102.250555349947,10.2,48.95));
#110946=CARTESIAN_POINT('',(102.250555349947,10.2,49.65));
#110947=CARTESIAN_POINT('Origin',(101.124722325027,10.85,49.65));
#110948=CARTESIAN_POINT('',(101.124722325027,10.85,49.65));
#110949=CARTESIAN_POINT('',(101.312361162513,10.85,49.65));
#110950=CARTESIAN_POINT('',(101.124722325027,10.85,48.95));
#110951=CARTESIAN_POINT('',(101.124722325027,10.85,49.65));
#110952=CARTESIAN_POINT('',(101.875277674973,10.85,48.95));
#110953=CARTESIAN_POINT('Origin',(100.749444650053,10.2,49.65));
#110954=CARTESIAN_POINT('',(100.749444650053,10.2,49.65));
#110955=CARTESIAN_POINT('',(100.843264068797,10.3625,49.65));
#110956=CARTESIAN_POINT('',(100.749444650053,10.2,48.95));
#110957=CARTESIAN_POINT('',(100.749444650053,10.2,49.65));
#110958=CARTESIAN_POINT('',(101.124722325027,10.85,48.95));
#110959=CARTESIAN_POINT('Origin',(101.124722325027,9.55,49.65));
#110960=CARTESIAN_POINT('',(101.124722325027,9.55,49.65));
#110961=CARTESIAN_POINT('',(101.030902906283,9.7125,49.65));
#110962=CARTESIAN_POINT('',(101.124722325027,9.55,48.95));
#110963=CARTESIAN_POINT('',(101.124722325027,9.55,49.65));
#110964=CARTESIAN_POINT('',(100.749444650053,10.2,48.95));
#110965=CARTESIAN_POINT('Origin',(101.875277674973,9.55,49.65));
#110966=CARTESIAN_POINT('',(101.875277674973,9.55,49.65));
#110967=CARTESIAN_POINT('',(101.687638837487,9.55,49.65));
#110968=CARTESIAN_POINT('',(101.875277674973,9.55,48.95));
#110969=CARTESIAN_POINT('',(101.875277674973,9.55,49.65));
#110970=CARTESIAN_POINT('',(101.124722325027,9.55,48.95));
#110971=CARTESIAN_POINT('Origin',(102.250555349947,10.2,49.65));
#110972=CARTESIAN_POINT('',(102.156735931203,10.0375,49.65));
#110973=CARTESIAN_POINT('',(101.875277674973,9.55,48.95));
#110974=CARTESIAN_POINT('Origin',(101.5,10.2,48.95));
#110975=CARTESIAN_POINT('Origin',(102.3,10.2,45.65));
#110976=CARTESIAN_POINT('',(100.7,10.2,45.65));
#110977=CARTESIAN_POINT('Origin',(101.5,10.2,45.65));
#110978=CARTESIAN_POINT('Origin',(101.5,10.2,45.75));
#110979=CARTESIAN_POINT('',(100.6,10.2,45.75));
#110980=CARTESIAN_POINT('Origin',(101.5,10.2,47.3));
#110981=CARTESIAN_POINT('Origin',(101.5,10.2,48.71675));
#110982=CARTESIAN_POINT('Origin',(101.5,10.2,49.2));
#110983=CARTESIAN_POINT('',(99.6,10.2,49.65));
#110984=CARTESIAN_POINT('Origin',(101.5,10.2,49.65));
#110985=CARTESIAN_POINT('',(100.05,10.2,49.2));
#110986=CARTESIAN_POINT('Origin',(101.5,10.2,49.65));
#110987=CARTESIAN_POINT('',(0.,0.,0.));
#110988=CARTESIAN_POINT('Origin',(6.,11.5,28.5));
#110989=CARTESIAN_POINT('',(4.78367053658047,11.2551073498501,28.5008333383868));
#110990=CARTESIAN_POINT('',(4.78395933369915,11.3198926501499,28.50124080222));
#110991=CARTESIAN_POINT('',(4.785,11.5,28.5));
#110992=CARTESIAN_POINT('',(6.5316301394983,11.4,29.5935755465205));
#110993=CARTESIAN_POINT('Ctrl Pts',(4.78367053658047,11.2551073498501,28.5008333383868));
#110994=CARTESIAN_POINT('Ctrl Pts',(4.78333000604768,11.2578458824113,28.5471435748903));
#110995=CARTESIAN_POINT('Ctrl Pts',(4.7857463752668,11.2605844149725,28.5934160710629));
#110996=CARTESIAN_POINT('Ctrl Pts',(4.79103847843843,11.2633229475337,28.6393548443288));
#110997=CARTESIAN_POINT('Ctrl Pts',(4.83692017656987,11.2870655920405,29.0376367483577));
#110998=CARTESIAN_POINT('Ctrl Pts',(5.09895975195116,11.3108082365472,29.4108339831172));
#110999=CARTESIAN_POINT('Ctrl Pts',(5.45800228421852,11.3345508810539,29.5895156282118));
#111000=CARTESIAN_POINT('Ctrl Pts',(5.78791523044235,11.3563672540359,29.7537005998278));
#111001=CARTESIAN_POINT('Ctrl Pts',(6.19972968361632,11.378183627018,29.7536522281492));
#111002=CARTESIAN_POINT('Ctrl Pts',(6.53227676969646,11.4,29.5943192153712));
#111003=CARTESIAN_POINT('',(5.46901649069986,11.4,29.5928318776698));
#111004=CARTESIAN_POINT('Origin',(6.,11.4,28.5));
#111005=CARTESIAN_POINT('Ctrl Pts',(5.46901649069988,11.4,29.5928318776698));
#111006=CARTESIAN_POINT('Ctrl Pts',(5.10673195249988,11.3762573554933,29.4168056110598));
#111007=CARTESIAN_POINT('Ctrl Pts',(4.84192918259107,11.3525147109866,29.0480006432466));
#111008=CARTESIAN_POINT('Ctrl Pts',(4.79253458702825,11.3287720664798,28.6507530872812));
#111009=CARTESIAN_POINT('Ctrl Pts',(4.78637695817715,11.3258122610365,28.6012314142364));
#111010=CARTESIAN_POINT('Ctrl Pts',(4.78356690442832,11.3228524555932,28.5512677259328));
#111011=CARTESIAN_POINT('Ctrl Pts',(4.78395933369915,11.3198926501499,28.50124080222));
#111012=CARTESIAN_POINT('Origin',(6.,11.5,28.5));
#111013=CARTESIAN_POINT('',(4.78681310871935,10.8051073498501,28.5004280789557));
#111014=CARTESIAN_POINT('',(4.78685314888988,10.8698926501499,28.5003771245331));
#111015=CARTESIAN_POINT('',(4.785,11.5,28.5));
#111016=CARTESIAN_POINT('Ctrl Pts',(4.78681310871935,10.8051073498501,28.5004280789557));
#111017=CARTESIAN_POINT('Ctrl Pts',(4.78625720576908,10.8153900153709,28.675482357614));
#111018=CARTESIAN_POINT('Ctrl Pts',(4.82167149629011,10.8256726808918,28.8503220275809));
#111019=CARTESIAN_POINT('Ctrl Pts',(4.89417743280821,10.8359553464126,29.0081177215779));
#111020=CARTESIAN_POINT('Ctrl Pts',(5.06159342741432,10.8596979909194,29.3724675158664));
#111021=CARTESIAN_POINT('Ctrl Pts',(5.42676232515714,10.8834406354261,29.6459479071283));
#111022=CARTESIAN_POINT('Ctrl Pts',(5.82349664722961,10.9071832799328,29.7041047455662));
#111023=CARTESIAN_POINT('Ctrl Pts',(6.22023096930208,10.9309259244395,29.762261584004));
#111024=CARTESIAN_POINT('Ctrl Pts',(6.64853071570421,10.9546685689463,29.6050948696179));
#111025=CARTESIAN_POINT('Ctrl Pts',(6.91347199143402,10.978411213453,29.3041169995649));
#111026=CARTESIAN_POINT('Ctrl Pts',(7.17841326716384,11.0021538579597,29.0031391295119));
#111027=CARTESIAN_POINT('Ctrl Pts',(7.27999607222133,11.0258965024664,28.558350103792));
#111028=CARTESIAN_POINT('Ctrl Pts',(7.17199676483148,11.0496391469732,28.1722029684367));
#111029=CARTESIAN_POINT('Ctrl Pts',(7.06399745744163,11.0733817914799,27.7860558330813));
#111030=CARTESIAN_POINT('Ctrl Pts',(6.74641603760442,11.0971244359866,27.4585505880904));
#111031=CARTESIAN_POINT('Ctrl Pts',(6.36377108114857,11.1208670804934,27.338680374029));
#111032=CARTESIAN_POINT('Ctrl Pts',(5.98112612469273,11.1446097250001,27.2188101599676));
#111033=CARTESIAN_POINT('Ctrl Pts',(5.53341763161827,11.1683523695068,27.3065749768356));
#111034=CARTESIAN_POINT('Ctrl Pts',(5.22442529552183,11.1920950140135,27.5621406719187));
#111035=CARTESIAN_POINT('Ctrl Pts',(4.95107286353664,11.213099125959,27.788228817552));
#111036=CARTESIAN_POINT('Ctrl Pts',(4.78628235194937,11.2341032379046,28.1456411432977));
#111037=CARTESIAN_POINT('Ctrl Pts',(4.78367053658047,11.2551073498501,28.5008333383868));
#111038=CARTESIAN_POINT('Ctrl Pts',(4.78395933369915,11.3198926501499,28.50124080222));
#111039=CARTESIAN_POINT('Ctrl Pts',(4.7867148507545,11.2991098110865,28.149967205262));
#111040=CARTESIAN_POINT('Ctrl Pts',(4.94736605064105,11.2783269720231,27.795575840609));
#111041=CARTESIAN_POINT('Ctrl Pts',(5.21568227798337,11.2575441329596,27.5691997084345));
#111042=CARTESIAN_POINT('Ctrl Pts',(5.52221098571815,11.2338014884529,27.3105840296708));
#111043=CARTESIAN_POINT('Ctrl Pts',(5.96925482240456,11.2100588439462,27.219042816261));
#111044=CARTESIAN_POINT('Ctrl Pts',(6.35303532139312,11.1863161994395,27.335452288796));
#111045=CARTESIAN_POINT('Ctrl Pts',(6.73681582038168,11.1625735549327,27.451861761331));
#111046=CARTESIAN_POINT('Ctrl Pts',(7.05733298167239,11.138830910426,27.7762219198108));
#111047=CARTESIAN_POINT('Ctrl Pts',(7.16888570291544,11.1150882659193,28.1613057291473));
#111048=CARTESIAN_POINT('Ctrl Pts',(7.2804384241585,11.0913456214126,28.5463895384839));
#111049=CARTESIAN_POINT('Ctrl Pts',(7.1830267053539,11.0676029769058,28.992196998677));
#111050=CARTESIAN_POINT('Ctrl Pts',(6.92089719776952,11.0438603323991,29.2956409119842));
#111051=CARTESIAN_POINT('Ctrl Pts',(6.65876769018514,11.0201176878924,29.5990848252914));
#111052=CARTESIAN_POINT('Ctrl Pts',(6.23192039382099,10.9963750433856,29.7601651917126));
#111053=CARTESIAN_POINT('Ctrl Pts',(5.83465859429877,10.9726323988789,29.7056760033484));
#111054=CARTESIAN_POINT('Ctrl Pts',(5.43739679477654,10.9488897543722,29.6511868149842));
#111055=CARTESIAN_POINT('Ctrl Pts',(5.06972049209625,10.9251471098655,29.3811280718347));
#111056=CARTESIAN_POINT('Ctrl Pts',(4.89893754845613,10.9014044653587,29.0183518086313));
#111057=CARTESIAN_POINT('Ctrl Pts',(4.8233817897133,10.8909005269558,28.8578566488922));
#111058=CARTESIAN_POINT('Ctrl Pts',(4.78636297044207,10.8803965885529,28.6792143587691));
#111059=CARTESIAN_POINT('Ctrl Pts',(4.78685314888988,10.8698926501499,28.5003771245331));
#111060=CARTESIAN_POINT('Origin',(6.,11.5,28.5));
#111061=CARTESIAN_POINT('',(4.78518722151686,10.3551073498501,28.4989078916254));
#111062=CARTESIAN_POINT('',(4.78507578420029,10.4198926501499,28.4989065979813));
#111063=CARTESIAN_POINT('',(4.785,11.5,28.5));
#111064=CARTESIAN_POINT('Ctrl Pts',(4.78518722151686,10.3551073498501,28.4989078916254));
#111065=CARTESIAN_POINT('Ctrl Pts',(4.78789665453853,10.3729341483306,28.8013698915326));
#111066=CARTESIAN_POINT('Ctrl Pts',(4.90234790879614,10.3907609468111,29.1056620640487));
#111067=CARTESIAN_POINT('Ctrl Pts',(5.10684325164102,10.4085877452916,29.3266182276633));
#111068=CARTESIAN_POINT('Ctrl Pts',(5.37920063727921,10.4323303897983,29.6208989786355));
#111069=CARTESIAN_POINT('Ctrl Pts',(5.81128073514232,10.456073034305,29.7673559959613));
#111070=CARTESIAN_POINT('Ctrl Pts',(6.20644280658897,10.4798156788117,29.6993364484615));
#111071=CARTESIAN_POINT('Ctrl Pts',(6.60160487803562,10.5035583233185,29.6313169009617));
#111072=CARTESIAN_POINT('Ctrl Pts',(6.95984892306582,10.5273009678252,29.3488207886363));
#111073=CARTESIAN_POINT('Ctrl Pts',(7.11813708317254,10.5510436123319,28.9804125574957));
#111074=CARTESIAN_POINT('Ctrl Pts',(7.27642524327927,10.5747862568386,28.6120043263552));
#111075=CARTESIAN_POINT('Ctrl Pts',(7.23475751846253,10.5985289013454,28.1576839763995));
#111076=CARTESIAN_POINT('Ctrl Pts',(7.01209712549708,10.6222715458521,27.8242143957805));
#111077=CARTESIAN_POINT('Ctrl Pts',(6.78943673253163,10.6460141903588,27.4907448151614));
#111078=CARTESIAN_POINT('Ctrl Pts',(6.38578367141748,10.6697568348655,27.2781260038789));
#111079=CARTESIAN_POINT('Ctrl Pts',(5.98484124835373,10.6934994793723,27.2831203215813));
#111080=CARTESIAN_POINT('Ctrl Pts',(5.58389882528997,10.717242123879,27.2881146392838));
#111081=CARTESIAN_POINT('Ctrl Pts',(5.18566704027662,10.7409847683857,27.5107220859713));
#111082=CARTESIAN_POINT('Ctrl Pts',(4.97138269350465,10.7647274128924,27.8496354079726));
#111083=CARTESIAN_POINT('Ctrl Pts',(4.84990242605869,10.7781873918783,28.0417692787753));
#111084=CARTESIAN_POINT('Ctrl Pts',(4.7875407840496,10.7916473708642,28.2712825419986));
#111085=CARTESIAN_POINT('Ctrl Pts',(4.78681310871935,10.8051073498501,28.5004280789557));
#111086=CARTESIAN_POINT('Ctrl Pts',(4.78685314888988,10.8698926501499,28.5003771245331));
#111087=CARTESIAN_POINT('Ctrl Pts',(4.78747094843896,10.8566539440461,28.2749784698909));
#111088=CARTESIAN_POINT('Ctrl Pts',(4.84767172642457,10.8434152379423,28.0492701468604));
#111089=CARTESIAN_POINT('Ctrl Pts',(4.96539746739741,10.8301765318386,27.8591937606951));
#111090=CARTESIAN_POINT('Ctrl Pts',(5.17652991457877,10.8064338873318,27.5183057592197));
#111091=CARTESIAN_POINT('Ctrl Pts',(5.57268439354146,10.7826912428251,27.292023539526));
#111092=CARTESIAN_POINT('Ctrl Pts',(5.97356402380349,10.7589485983184,27.2833149153006));
#111093=CARTESIAN_POINT('Ctrl Pts',(6.37444365406551,10.7352059538117,27.2746062910752));
#111094=CARTESIAN_POINT('Ctrl Pts',(6.78004843562688,10.7114633093049,27.483471262318));
#111095=CARTESIAN_POINT('Ctrl Pts',(7.0057896364173,10.6877206647982,27.8148619299256));
#111096=CARTESIAN_POINT('Ctrl Pts',(7.23153083720772,10.6639780202915,28.1462525975332));
#111097=CARTESIAN_POINT('Ctrl Pts',(7.27740845722719,10.6402353757847,28.6001689615056));
#111098=CARTESIAN_POINT('Ctrl Pts',(7.12254190425398,10.616492731278,28.9700288680826));
#111099=CARTESIAN_POINT('Ctrl Pts',(6.96767535128077,10.5927500867713,29.3398887746596));
#111100=CARTESIAN_POINT('Ctrl Pts',(6.61206462531487,10.5690074422646,29.6256922238413));
#111101=CARTESIAN_POINT('Ctrl Pts',(6.21754989447942,10.5452647977578,29.697371194261));
#111102=CARTESIAN_POINT('Ctrl Pts',(5.82303516364397,10.5215221532511,29.7690501646807));
#111103=CARTESIAN_POINT('Ctrl Pts',(5.38961642793897,10.4977795087444,29.6266046563385));
#111104=CARTESIAN_POINT('Ctrl Pts',(5.11454326365905,10.4740368642377,29.33486102967));
#111105=CARTESIAN_POINT('Ctrl Pts',(4.90544523763903,10.4559887928751,29.1130908813533));
#111106=CARTESIAN_POINT('Ctrl Pts',(4.78784473538313,10.4379407215125,28.8050511392199));
#111107=CARTESIAN_POINT('Ctrl Pts',(4.78507578420029,10.4198926501499,28.4989065979813));
#111108=CARTESIAN_POINT('Origin',(6.,11.5,28.5));
#111109=CARTESIAN_POINT('',(4.78326855736707,9.90510734985006,28.5004863587445));
#111110=CARTESIAN_POINT('',(4.78333364803414,9.96989265014994,28.5005459760334));
#111111=CARTESIAN_POINT('',(4.785,11.5,28.5));
#111112=CARTESIAN_POINT('Ctrl Pts',(4.78326855736707,9.90510734985006,28.5004863587445));
#111113=CARTESIAN_POINT('Ctrl Pts',(4.78312813994714,9.90673563678347,28.5280000759249));
#111114=CARTESIAN_POINT('Ctrl Pts',(4.78398106663306,9.90836392371688,28.5555049348603));
#111115=CARTESIAN_POINT('Ctrl Pts',(4.78585519896961,9.90999221065029,28.5829400337243));
#111116=CARTESIAN_POINT('Ctrl Pts',(4.81318260479242,9.93373485515702,28.9829811972126));
#111117=CARTESIAN_POINT('Ctrl Pts',(5.05763485169036,9.95747749966375,29.3681902410136));
#111118=CARTESIAN_POINT('Ctrl Pts',(5.40796108834759,9.98122014417047,29.5632575298335));
#111119=CARTESIAN_POINT('Ctrl Pts',(5.75828732500482,10.0049627886772,29.7583248186535));
#111120=CARTESIAN_POINT('Ctrl Pts',(6.21448755142135,10.0287054331839,29.7632503524923));
#111121=CARTESIAN_POINT('Ctrl Pts',(6.56894386303769,10.0524480776906,29.5757925106412));
#111122=CARTESIAN_POINT('Ctrl Pts',(6.92340017465404,10.0761907221974,29.38833466879));
#111123=CARTESIAN_POINT('Ctrl Pts',(7.17611257147019,10.0999333667041,29.0084934512488));
#111124=CARTESIAN_POINT('Ctrl Pts',(7.21207098565849,10.1236760112108,28.6091355755066));
#111125=CARTESIAN_POINT('Ctrl Pts',(7.2480293998468,10.1474186557176,28.2097776997644));
#111126=CARTESIAN_POINT('Ctrl Pts',(7.06723383140724,10.1711613002243,27.7909031658212));
#111127=CARTESIAN_POINT('Ctrl Pts',(6.75196481435131,10.194903944731,27.5431428689897));
#111128=CARTESIAN_POINT('Ctrl Pts',(6.43669579729538,10.2186465892377,27.2953825721582));
#111129=CARTESIAN_POINT('Ctrl Pts',(5.98695333162308,10.2423892337445,27.2187365124384));
#111130=CARTESIAN_POINT('Ctrl Pts',(5.6074163743245,10.2661318782512,27.348086491701));
#111131=CARTESIAN_POINT('Ctrl Pts',(5.22787941702593,10.2898745227579,27.4774364709637));
#111132=CARTESIAN_POINT('Ctrl Pts',(4.91854796810108,10.3136171672646,27.8127824892088));
#111133=CARTESIAN_POINT('Ctrl Pts',(4.82019958034531,10.3373598117714,28.2015077406407));
#111134=CARTESIAN_POINT('Ctrl Pts',(4.79569456285552,10.3432756577976,28.2983646317645));
#111135=CARTESIAN_POINT('Ctrl Pts',(4.78428809268046,10.3491915038238,28.3985354875622));
#111136=CARTESIAN_POINT('Ctrl Pts',(4.78518722151686,10.3551073498501,28.4989078916254));
#111137=CARTESIAN_POINT('Ctrl Pts',(4.78507578420029,10.4198926501499,28.4989065979813));
#111138=CARTESIAN_POINT('Ctrl Pts',(4.78420211771668,10.4141980770058,28.4023110976785));
#111139=CARTESIAN_POINT('Ctrl Pts',(4.79476044511274,10.4085035038616,28.3059042730909));
#111140=CARTESIAN_POINT('Ctrl Pts',(4.81748372732635,10.4028089307175,28.2124555283066));
#111141=CARTESIAN_POINT('Ctrl Pts',(4.91222494812837,10.3790662862107,27.8228353986066));
#111142=CARTESIAN_POINT('Ctrl Pts',(5.21843498258722,10.355323641704,27.4846368842013));
#111143=CARTESIAN_POINT('Ctrl Pts',(5.59675674158146,10.3315809971973,27.3517747524404));
#111144=CARTESIAN_POINT('Ctrl Pts',(5.9750785005757,10.3078383526906,27.2189126206795));
#111145=CARTESIAN_POINT('Ctrl Pts',(6.42551198410532,10.2840957081838,27.291386871563));
#111146=CARTESIAN_POINT('Ctrl Pts',(6.74306380257482,10.2603530636771,27.5362144155618));
#111147=CARTESIAN_POINT('Ctrl Pts',(7.06061562104432,10.2366104191704,27.7810419595606));
#111148=CARTESIAN_POINT('Ctrl Pts',(7.2452857744537,10.2128677746637,28.1982227966747));
#111149=CARTESIAN_POINT('Ctrl Pts',(7.21303036873607,10.1891251301569,28.5978967802481));
#111150=CARTESIAN_POINT('Ctrl Pts',(7.18077496301845,10.1653824856502,28.9975707638215));
#111151=CARTESIAN_POINT('Ctrl Pts',(6.93159399817384,10.1416398411435,29.3797378938541));
#111152=CARTESIAN_POINT('Ctrl Pts',(6.57889039174064,10.1178971966368,29.5704729534016));
#111153=CARTESIAN_POINT('Ctrl Pts',(6.22618678530745,10.09415455213,29.7612080129492));
#111154=CARTESIAN_POINT('Ctrl Pts',(5.76996053728566,10.0704119076233,29.7605110020117));
#111155=CARTESIAN_POINT('Ctrl Pts',(5.41784138777708,10.0466692631166,29.5686991145014));
#111156=CARTESIAN_POINT('Ctrl Pts',(5.0657222382685,10.0229266186098,29.3768872269911));
#111157=CARTESIAN_POINT('Ctrl Pts',(4.81771018727311,9.99918397410312,28.993960462908));
#111158=CARTESIAN_POINT('Ctrl Pts',(4.78667616574802,9.97544132959639,28.594189793868));
#111159=CARTESIAN_POINT('Ctrl Pts',(4.78425860526484,9.97359176978091,28.5630475272744));
#111160=CARTESIAN_POINT('Ctrl Pts',(4.78315776754325,9.97174220996543,28.5318030440965));
#111161=CARTESIAN_POINT('Ctrl Pts',(4.78333364803414,9.96989265014994,28.5005459760334));
#111162=CARTESIAN_POINT('Origin',(6.,11.5,28.5));
#111163=CARTESIAN_POINT('',(4.78654814450966,9.45510734985006,28.5006898848044));
#111164=CARTESIAN_POINT('',(4.78661099114014,9.51989265014995,28.5006411245624));
#111165=CARTESIAN_POINT('',(4.785,11.5,28.5));
#111166=CARTESIAN_POINT('Ctrl Pts',(4.78654814450966,9.45510734985006,28.5006898848044));
#111167=CARTESIAN_POINT('Ctrl Pts',(4.78573643973839,9.46427976974311,28.6567574803934));
#111168=CARTESIAN_POINT('Ctrl Pts',(4.81368718036296,9.47345218963616,28.8125454468369));
#111169=CARTESIAN_POINT('Ctrl Pts',(4.87175089853111,9.48262460952921,28.9561585382471));
#111170=CARTESIAN_POINT('Ctrl Pts',(5.02204779240205,9.50636725403594,29.327898451555));
#111171=CARTESIAN_POINT('Ctrl Pts',(5.37410884694187,9.53010989854266,29.6180637866337));
#111172=CARTESIAN_POINT('Ctrl Pts',(5.76771016394421,9.55385254304938,29.6945995475735));
#111173=CARTESIAN_POINT('Ctrl Pts',(6.16131148094654,9.57759518755611,29.7711353085133));
#111174=CARTESIAN_POINT('Ctrl Pts',(6.59645306041139,9.60133783206284,29.634041495314));
#111175=CARTESIAN_POINT('Ctrl Pts',(6.87510084197326,9.62508047656957,29.3457098576534));
#111176=CARTESIAN_POINT('Ctrl Pts',(7.15374862353513,9.6488231210763,29.0573782199929));
#111177=CARTESIAN_POINT('Ctrl Pts',(7.27590260719402,9.67256576558302,28.6178087578709));
#111178=CARTESIAN_POINT('Ctrl Pts',(7.18597019843295,9.69630841008975,28.2270506724461));
#111179=CARTESIAN_POINT('Ctrl Pts',(7.09603778967188,9.72005105459647,27.8362925870213));
#111180=CARTESIAN_POINT('Ctrl Pts',(6.79401898849085,9.7437936991032,27.4943458782936));
#111181=CARTESIAN_POINT('Ctrl Pts',(6.41736333395727,9.76753634360992,27.3568313796495));
#111182=CARTESIAN_POINT('Ctrl Pts',(6.04070767942368,9.79127898811665,27.2193168810055));
#111183=CARTESIAN_POINT('Ctrl Pts',(5.58941517153755,9.81502163262338,27.2862345924451));
#111184=CARTESIAN_POINT('Ctrl Pts',(5.26887019996833,9.83876427713011,27.5271300897527));
#111185=CARTESIAN_POINT('Ctrl Pts',(4.97030842359998,9.86087863470343,27.7515048077313));
#111186=CARTESIAN_POINT('Ctrl Pts',(4.7851756174621,9.88299299227674,28.1268125501468));
#111187=CARTESIAN_POINT('Ctrl Pts',(4.78326855736707,9.90510734985006,28.5004863587445));
#111188=CARTESIAN_POINT('Ctrl Pts',(4.78333364803414,9.96989265014994,28.5005459760334));
#111189=CARTESIAN_POINT('Ctrl Pts',(4.7854155306801,9.9479995654587,28.1305586782034));
#111190=CARTESIAN_POINT('Ctrl Pts',(4.96638170498052,9.92610648076746,27.7588080795541));
#111191=CARTESIAN_POINT('Ctrl Pts',(5.25988458774409,9.90421339607621,27.533948439426));
#111192=CARTESIAN_POINT('Ctrl Pts',(5.57818302332005,9.88047075156948,27.2900923280207));
#111193=CARTESIAN_POINT('Ctrl Pts',(6.02883588652676,9.85672810706275,27.2189946792071));
#111194=CARTESIAN_POINT('Ctrl Pts',(6.40674989258746,9.83298546255602,27.3530122195701));
#111195=CARTESIAN_POINT('Ctrl Pts',(6.78466389864815,9.8092428180493,27.4870297599331));
#111196=CARTESIAN_POINT('Ctrl Pts',(7.08983904756283,9.78550017354258,27.8261624894727));
#111197=CARTESIAN_POINT('Ctrl Pts',(7.18338933774817,9.76175752903585,28.2160702229757));
#111198=CARTESIAN_POINT('Ctrl Pts',(7.2769396279335,9.73801488452913,28.6059779564786));
#111199=CARTESIAN_POINT('Ctrl Pts',(7.15886505938949,9.7142722400224,29.046660693945));
#111200=CARTESIAN_POINT('Ctrl Pts',(6.88290167449175,9.69052959551567,29.3375625802597));
#111201=CARTESIAN_POINT('Ctrl Pts',(6.606938289594,9.66678695100894,29.6284644665744));
#111202=CARTESIAN_POINT('Ctrl Pts',(6.17308608834251,9.64304430650222,29.7695855017375));
#111203=CARTESIAN_POINT('Ctrl Pts',(5.77879233160934,9.61930166199549,29.6967011366441));
#111204=CARTESIAN_POINT('Ctrl Pts',(5.38449857487616,9.59555901748876,29.6238167715508));
#111205=CARTESIAN_POINT('Ctrl Pts',(5.0297632626613,9.57181637298203,29.3369270062008));
#111206=CARTESIAN_POINT('Ctrl Pts',(4.87602735483413,9.54807372847531,28.9665961163745));
#111207=CARTESIAN_POINT('Ctrl Pts',(4.81520229020312,9.53868003570019,28.820076018195));
#111208=CARTESIAN_POINT('Ctrl Pts',(4.78584088953869,9.52928634292507,28.6604943713531));
#111209=CARTESIAN_POINT('Ctrl Pts',(4.78661099114014,9.51989265014995,28.5006411245624));
#111210=CARTESIAN_POINT('Origin',(6.,11.5,28.5));
#111211=CARTESIAN_POINT('',(4.78572353544277,9.00510734985006,28.4989685021794));
#111212=CARTESIAN_POINT('',(4.78562084144037,9.06989265014994,28.4989494257994));
#111213=CARTESIAN_POINT('',(4.785,11.5,28.5));
#111214=CARTESIAN_POINT('Ctrl Pts',(4.78572353544277,9.00510734985006,28.4989685021794));
#111215=CARTESIAN_POINT('Ctrl Pts',(4.78803916596806,9.02182390270275,28.7829119346081));
#111216=CARTESIAN_POINT('Ctrl Pts',(4.88746037938484,9.03854045555544,29.0683165908713));
#111217=CARTESIAN_POINT('Ctrl Pts',(5.06938019515906,9.05525700840813,29.2842024138066));
#111218=CARTESIAN_POINT('Ctrl Pts',(5.32776226428058,9.07899965291485,29.5908266558477));
#111219=CARTESIAN_POINT('Ctrl Pts',(5.75256655663188,9.10274229742157,29.7572124154401));
#111220=CARTESIAN_POINT('Ctrl Pts',(6.15046353798807,9.12648494192829,29.707637102245));
#111221=CARTESIAN_POINT('Ctrl Pts',(6.54836051934427,9.15022758643502,29.65806178905));
#111222=CARTESIAN_POINT('Ctrl Pts',(6.91935018970536,9.17397023094176,29.3925254030675));
#111223=CARTESIAN_POINT('Ctrl Pts',(7.09459418876182,9.19771287544849,29.0318742416312));
#111224=CARTESIAN_POINT('Ctrl Pts',(7.26983818781829,9.22145551995522,28.671223080195));
#111225=CARTESIAN_POINT('Ctrl Pts',(7.24933651557014,9.24519816446194,28.2154571433049));
#111226=CARTESIAN_POINT('Ctrl Pts',(7.04241953618214,9.26894080896866,27.8719966898433));
#111227=CARTESIAN_POINT('Ctrl Pts',(6.83550255679414,9.29268345347539,27.5285362363817));
#111228=CARTESIAN_POINT('Ctrl Pts',(6.44217027026628,9.31642609798212,27.2973812663485));
#111229=CARTESIAN_POINT('Ctrl Pts',(6.04142921942195,9.34016874248885,27.2837310055902));
#111230=CARTESIAN_POINT('Ctrl Pts',(5.64068816857763,9.36391138699558,27.2700807448319));
#111231=CARTESIAN_POINT('Ctrl Pts',(5.23253835341683,9.38765403150229,27.4739351933486));
#111232=CARTESIAN_POINT('Ctrl Pts',(5.00272981243747,9.41139667600902,27.8025196633754));
#111233=CARTESIAN_POINT('Ctrl Pts',(4.86170246987407,9.4259669006227,28.0041631463286));
#111234=CARTESIAN_POINT('Ctrl Pts',(4.78783752299161,9.44053712523638,28.2527793062262));
#111235=CARTESIAN_POINT('Ctrl Pts',(4.78654814450966,9.45510734985006,28.5006898848044));
#111236=CARTESIAN_POINT('Ctrl Pts',(4.78661099114014,9.51989265014995,28.5006411245624));
#111237=CARTESIAN_POINT('Ctrl Pts',(4.78778732838813,9.50554369841834,28.2564638263208));
#111238=CARTESIAN_POINT('Ctrl Pts',(4.85926902453589,9.49119474668674,28.0116528082032));
#111239=CARTESIAN_POINT('Ctrl Pts',(4.99630810472276,9.47684579495513,27.8117928929291));
#111240=CARTESIAN_POINT('Ctrl Pts',(5.22306126587803,9.45310315044841,27.4810925736128));
#111241=CARTESIAN_POINT('Ctrl Pts',(5.62930409162803,9.42936050594167,27.2734639492829));
#111242=CARTESIAN_POINT('Ctrl Pts',(6.03015441931446,9.40561786143494,27.2833993449339));
#111243=CARTESIAN_POINT('Ctrl Pts',(6.43100474700089,9.38187521692822,27.2933347405849));
#111244=CARTESIAN_POINT('Ctrl Pts',(6.82646257662373,9.3581325724215,27.5208341562169));
#111245=CARTESIAN_POINT('Ctrl Pts',(7.03655402518042,9.33438992791477,27.8623620182446));
#111246=CARTESIAN_POINT('Ctrl Pts',(7.24664547373712,9.31064728340805,28.2038898802724));
#111247=CARTESIAN_POINT('Ctrl Pts',(7.27137054122764,9.28690463890131,28.6594461886959));
#111248=CARTESIAN_POINT('Ctrl Pts',(7.09947678537309,9.26316199439458,29.0217060871011));
#111249=CARTESIAN_POINT('Ctrl Pts',(6.92758302951854,9.23941934988786,29.3839659855063));
#111250=CARTESIAN_POINT('Ctrl Pts',(6.55907045031891,9.21567670538114,29.6529294738932));
#111251=CARTESIAN_POINT('Ctrl Pts',(6.16165007747503,9.19193406087441,29.7061905717384));
#111252=CARTESIAN_POINT('Ctrl Pts',(5.76422970463114,9.16819141636768,29.7594516695836));
#111253=CARTESIAN_POINT('Ctrl Pts',(5.337901538143,9.14444877186095,29.597010376887));
#111254=CARTESIAN_POINT('Ctrl Pts',(5.07668863130513,9.12070612735422,29.2927941468846));
#111255=CARTESIAN_POINT('Ctrl Pts',(4.89034128931309,9.10376830161946,29.075768554474));
#111256=CARTESIAN_POINT('Ctrl Pts',(4.78802588006844,9.0868304758847,28.7865895946388));
#111257=CARTESIAN_POINT('Ctrl Pts',(4.78562084144037,9.06989265014994,28.4989494257994));
#111258=CARTESIAN_POINT('Origin',(6.,11.5,28.5));
#111259=CARTESIAN_POINT('',(4.78305239341621,8.55510734985006,28.5001606667931));
#111260=CARTESIAN_POINT('',(4.78307934473882,8.61989265014994,28.5002282550221));
#111261=CARTESIAN_POINT('',(4.785,11.5,28.5));
#111262=CARTESIAN_POINT('Ctrl Pts',(4.78305239341621,8.55510734985006,28.5001606667931));
#111263=CARTESIAN_POINT('Ctrl Pts',(4.78303604688816,8.55562539115566,28.5089100350328));
#111264=CARTESIAN_POINT('Ctrl Pts',(4.78312229599692,8.55614343246126,28.5176590726092));
#111265=CARTESIAN_POINT('Ctrl Pts',(4.7833121281823,8.55666147376686,28.5264058621149));
#111266=CARTESIAN_POINT('Ctrl Pts',(4.79201243459565,8.58040411827359,28.9272849263215));
#111267=CARTESIAN_POINT('Ctrl Pts',(5.01829235789579,8.60414676278031,29.3234418448605));
#111268=CARTESIAN_POINT('Ctrl Pts',(5.35917131864016,8.62788940728704,29.5345845775619));
#111269=CARTESIAN_POINT('Ctrl Pts',(5.70005027938453,8.65163205179376,29.7457273102633));
#111270=CARTESIAN_POINT('Ctrl Pts',(6.15552827757312,8.6753746963005,29.771855857127));
#111271=CARTESIAN_POINT('Ctrl Pts',(6.51831609597122,8.69911734080722,29.6010790487697));
#111272=CARTESIAN_POINT('Ctrl Pts',(6.88110391436932,8.72285998531395,29.4303022404123));
#111273=CARTESIAN_POINT('Ctrl Pts',(7.15120155297692,8.74660262982067,29.0626200768339));
#111274=CARTESIAN_POINT('Ctrl Pts',(7.2056868765722,8.7703452743274,28.6653656634368));
#111275=CARTESIAN_POINT('Ctrl Pts',(7.26017220016747,8.79408791883412,28.2681112500397));
#111276=CARTESIAN_POINT('Ctrl Pts',(7.09904520875042,8.81783056334086,27.8412845868238));
#111277=CARTESIAN_POINT('Ctrl Pts',(6.79563521363584,8.84157320784758,27.579135594235));
#111278=CARTESIAN_POINT('Ctrl Pts',(6.49222521852127,8.86531585235431,27.3169866016461));
#111279=CARTESIAN_POINT('Ctrl Pts',(6.04653221970919,8.88905849686104,27.2195152796843));
#111280=CARTESIAN_POINT('Ctrl Pts',(5.66139225586264,8.91280114136776,27.3310810795472));
#111281=CARTESIAN_POINT('Ctrl Pts',(5.2762522920161,8.93654378587449,27.4426468794101));
#111282=CARTESIAN_POINT('Ctrl Pts',(4.9516653631351,8.96028643038121,27.7632498010979));
#111283=CARTESIAN_POINT('Ctrl Pts',(4.83535182164046,8.98402907488794,28.1469826241867));
#111284=CARTESIAN_POINT('Ctrl Pts',(4.80093149399264,8.99105516654198,28.2605395611539));
#111285=CARTESIAN_POINT('Ctrl Pts',(4.78475025868822,8.99808125819602,28.3796249629708));
#111286=CARTESIAN_POINT('Ctrl Pts',(4.78572353544277,9.00510734985006,28.4989685021794));
#111287=CARTESIAN_POINT('Ctrl Pts',(4.78562084144037,9.06989265014994,28.4989494257994));
#111288=CARTESIAN_POINT('Ctrl Pts',(4.78465461045772,9.06308783137798,28.3833891850022));
#111289=CARTESIAN_POINT('Ctrl Pts',(4.79981444337002,9.05628301260601,28.2680773132359));
#111290=CARTESIAN_POINT('Ctrl Pts',(4.8321299779901,9.04947819383405,28.1577923808764));
#111291=CARTESIAN_POINT('Ctrl Pts',(4.94488187870056,9.02573554932732,27.7729980121789));
#111292=CARTESIAN_POINT('Ctrl Pts',(5.26648332730909,9.00199290482059,27.4494004420923));
#111293=CARTESIAN_POINT('Ctrl Pts',(5.65057267120333,8.97825026031386,27.3342697632872));
#111294=CARTESIAN_POINT('Ctrl Pts',(6.03466201509756,8.95450761580713,27.2191390844821));
#111295=CARTESIAN_POINT('Ctrl Pts',(6.4812392542775,8.93076497130041,27.3124752969585));
#111296=CARTESIAN_POINT('Ctrl Pts',(6.78706592999723,8.90702232679368,27.5718008485602));
#111297=CARTESIAN_POINT('Ctrl Pts',(7.09289260571695,8.88327968228696,27.8311264001619));
#111298=CARTESIAN_POINT('Ctrl Pts',(7.25796871797646,8.85953703778023,28.2564412908888));
#111299=CARTESIAN_POINT('Ctrl Pts',(7.20716770033245,8.83579439327351,28.6541836118725));
#111300=CARTESIAN_POINT('Ctrl Pts',(7.15636668268844,8.81205174876678,29.0519259328563));
#111301=CARTESIAN_POINT('Ctrl Pts',(6.8896885351409,8.78830910426005,29.4220956840969));
#111302=CARTESIAN_POINT('Ctrl Pts',(6.52849917366942,8.76456645975332,29.5962276526009));
#111303=CARTESIAN_POINT('Ctrl Pts',(6.16730981219795,8.74082381524659,29.7703596211048));
#111304=CARTESIAN_POINT('Ctrl Pts',(5.71160923680254,8.71708117073987,29.7484538068722));
#111305=CARTESIAN_POINT('Ctrl Pts',(5.36878796018151,8.69333852623314,29.5404796027238));
#111306=CARTESIAN_POINT('Ctrl Pts',(5.02596668356048,8.66959588172642,29.3325053985753));
#111307=CARTESIAN_POINT('Ctrl Pts',(4.79602470571383,8.64585323721969,28.9384628045112));
#111308=CARTESIAN_POINT('Ctrl Pts',(4.78360921659756,8.62211059271296,28.5376816261541));
#111309=CARTESIAN_POINT('Ctrl Pts',(4.78322261487558,8.62137127852529,28.5252018364143));
#111310=CARTESIAN_POINT('Ctrl Pts',(4.78304693037956,8.62063196433762,28.5127155128334));
#111311=CARTESIAN_POINT('Ctrl Pts',(4.78307934473882,8.61989265014994,28.5002282550221));
#111312=CARTESIAN_POINT('Origin',(6.,11.5,28.5));
#111313=CARTESIAN_POINT('',(4.78616577632925,8.10510734985006,28.5008994915339));
#111314=CARTESIAN_POINT('',(4.78625043272942,8.16989265014995,28.5008628615494));
#111315=CARTESIAN_POINT('',(4.785,11.5,28.5));
#111316=CARTESIAN_POINT('Ctrl Pts',(4.78616577632925,8.10510734985006,28.5008994915339));
#111317=CARTESIAN_POINT('Ctrl Pts',(4.78521661554573,8.1131695241153,28.6379677840418));
#111318=CARTESIAN_POINT('Ctrl Pts',(4.80665227509289,8.12123169838054,28.7747480235267));
#111319=CARTESIAN_POINT('Ctrl Pts',(4.85176436536515,8.12929387264578,28.903214055232));
#111320=CARTESIAN_POINT('Ctrl Pts',(4.98461690452544,8.15303651715251,29.2815392094179));
#111321=CARTESIAN_POINT('Ctrl Pts',(5.32280778498557,8.17677916165923,29.587757817879));
#111322=CARTESIAN_POINT('Ctrl Pts',(5.71242546071077,8.20052180616595,29.6825089984159));
#111323=CARTESIAN_POINT('Ctrl Pts',(6.10204313643597,8.22426445067268,29.7772601789527));
#111324=CARTESIAN_POINT('Ctrl Pts',(6.54308760742622,8.24800709517941,29.6605439315654));
#111325=CARTESIAN_POINT('Ctrl Pts',(6.8348383920752,8.27174973968614,29.3854781228805));
#111326=CARTESIAN_POINT('Ctrl Pts',(7.12658917672417,8.29549238419287,29.1104123141956));
#111327=CARTESIAN_POINT('Ctrl Pts',(7.26904627503186,8.31923502869959,28.6769969442132));
#111328=CARTESIAN_POINT('Ctrl Pts',(7.19737709241624,8.34297767320632,28.2824804709019));
#111329=CARTESIAN_POINT('Ctrl Pts',(7.12570790980061,8.36672031771304,27.8879639975905));
#111330=CARTESIAN_POINT('Ctrl Pts',(6.83991244626166,8.39046296221977,27.5323464209502));
#111331=CARTESIAN_POINT('Ctrl Pts',(6.47005695782437,8.4142056067265,27.3774702216052));
#111332=CARTESIAN_POINT('Ctrl Pts',(6.10020146938709,8.43794825123323,27.2225940222601));
#111333=CARTESIAN_POINT('Ctrl Pts',(5.64628595605148,8.46169089573995,27.2684592002103));
#111334=CARTESIAN_POINT('Ctrl Pts',(5.31488854414695,8.48543354024668,27.4941923941224));
#111335=CARTESIAN_POINT('Ctrl Pts',(4.99072189998132,8.5086581434478,27.7150003102939));
#111336=CARTESIAN_POINT('Ctrl Pts',(4.78378523387422,8.53188274664894,28.1079127834113));
#111337=CARTESIAN_POINT('Ctrl Pts',(4.78305239341621,8.55510734985006,28.5001606667931));
#111338=CARTESIAN_POINT('Ctrl Pts',(4.78307934473882,8.61989265014994,28.5002282550221));
#111339=CARTESIAN_POINT('Ctrl Pts',(4.78408789864679,8.59688931983089,28.111694501712));
#111340=CARTESIAN_POINT('Ctrl Pts',(4.98655840647933,8.57388598951183,27.7222563134603));
#111341=CARTESIAN_POINT('Ctrl Pts',(5.3055956680209,8.55088265919278,27.5005856381737));
#111342=CARTESIAN_POINT('Ctrl Pts',(5.63488660894638,8.52714001468605,27.2717905912001));
#111343=CARTESIAN_POINT('Ctrl Pts',(6.08835749118323,8.50339737017933,27.2217202599028));
#111344=CARTESIAN_POINT('Ctrl Pts',(6.4596325411673,8.4796547256726,27.3731617818));
#111345=CARTESIAN_POINT('Ctrl Pts',(6.83090759115138,8.45591208116588,27.5246033036973));
#111346=CARTESIAN_POINT('Ctrl Pts',(7.11998680888268,8.43216943665915,27.8775566787891));
#111347=CARTESIAN_POINT('Ctrl Pts',(7.19530949329411,8.40842679215242,28.2713919114795));
#111348=CARTESIAN_POINT('Ctrl Pts',(7.27063217770554,8.38468414764569,28.6652271441699));
#111349=CARTESIAN_POINT('Ctrl Pts',(7.1321983287971,8.36094150313897,29.0999442344589));
#111350=CARTESIAN_POINT('Ctrl Pts',(6.84300954992419,8.33719885863224,29.3777023080935));
#111351=CARTESIAN_POINT('Ctrl Pts',(6.55382077105129,8.31345621412551,29.6554603817282));
#111352=CARTESIAN_POINT('Ctrl Pts',(6.11387706221393,8.28971356961879,29.7762594387086));
#111353=CARTESIAN_POINT('Ctrl Pts',(5.72339794530988,8.26597092511206,29.6851235151819));
#111354=CARTESIAN_POINT('Ctrl Pts',(5.33291882840583,8.24222828060534,29.5939875916553));
#111355=CARTESIAN_POINT('Ctrl Pts',(4.99190430343508,8.21848563609861,29.2909166876217));
#111356=CARTESIAN_POINT('Ctrl Pts',(4.85555096436684,8.19474299159188,28.9138391568403));
#111357=CARTESIAN_POINT('Ctrl Pts',(4.80797936057134,8.18645954444457,28.7822825479806));
#111358=CARTESIAN_POINT('Ctrl Pts',(4.78531923606525,8.17817609729726,28.641717809214));
#111359=CARTESIAN_POINT('Ctrl Pts',(4.78625043272942,8.16989265014995,28.5008628615494));
#111360=CARTESIAN_POINT('Origin',(6.,11.5,28.5));
#111361=CARTESIAN_POINT('',(4.78619455170653,7.65510734985006,28.4991124767033));
#111362=CARTESIAN_POINT('',(4.78610753914613,7.71989265014994,28.499077712745));
#111363=CARTESIAN_POINT('',(4.785,11.5,28.5));
#111364=CARTESIAN_POINT('Ctrl Pts',(4.78619455170653,7.65510734985006,28.4991124767033));
#111365=CARTESIAN_POINT('Ctrl Pts',(4.78800457873014,7.67071365707494,28.7644574786248));
#111366=CARTESIAN_POINT('Ctrl Pts',(4.87364547425961,7.68631996429982,29.0308656186776));
#111367=CARTESIAN_POINT('Ctrl Pts',(5.03392952076701,7.7019262715247,29.2400908566776));
#111368=CARTESIAN_POINT('Ctrl Pts',(5.27777754205026,7.72566891603142,29.5583955251741));
#111369=CARTESIAN_POINT('Ctrl Pts',(5.69438741094785,7.74941156053815,29.7443501564449));
#111370=CARTESIAN_POINT('Ctrl Pts',(6.09415889663745,7.77315420504487,29.7133263160167));
#111371=CARTESIAN_POINT('Ctrl Pts',(6.49393038232705,7.7968968495516,29.6823024755884));
#111372=CARTESIAN_POINT('Ctrl Pts',(6.87686348480867,7.82063949405833,29.4343001634611));
#111373=CARTESIAN_POINT('Ctrl Pts',(7.06868435683791,7.84438213856505,29.082185874483));
#111374=CARTESIAN_POINT('Ctrl Pts',(7.26050522886715,7.86812478307178,28.730071585505));
#111375=CARTESIAN_POINT('Ctrl Pts',(7.26121387044402,7.8918674275785,28.273845319676));
#111376=CARTESIAN_POINT('Ctrl Pts',(7.07048777696507,7.91561007208523,27.9211368327925));
#111377=CARTESIAN_POINT('Ctrl Pts',(6.87976168348613,7.93935271659196,27.568428345909));
#111378=CARTESIAN_POINT('Ctrl Pts',(6.49760085495136,7.96309536109869,27.3192376379709));
#111379=CARTESIAN_POINT('Ctrl Pts',(6.09792767469521,7.98683800560542,27.2869720458671));
#111380=CARTESIAN_POINT('Ctrl Pts',(5.69825449443906,8.01058065011215,27.2547064537634));
#111381=CARTESIAN_POINT('Ctrl Pts',(5.28106896246153,8.03432329461887,27.4393659774941));
#111382=CARTESIAN_POINT('Ctrl Pts',(5.03623329540298,8.0580659391256,27.7569115893148));
#111383=CARTESIAN_POINT('Ctrl Pts',(4.87453528445568,8.07374640936708,27.9666297828824));
#111384=CARTESIAN_POINT('Ctrl Pts',(4.78801184004987,8.08942687960857,28.2343094612255));
#111385=CARTESIAN_POINT('Ctrl Pts',(4.78616577632925,8.10510734985006,28.5008994915339));
#111386=CARTESIAN_POINT('Ctrl Pts',(4.78625043272942,8.16989265014995,28.5008628615494));
#111387=CARTESIAN_POINT('Ctrl Pts',(4.78798830257463,8.15443345279053,28.2379886744783));
#111388=CARTESIAN_POINT('Ctrl Pts',(4.87189440305332,8.13897425543111,27.9741036940105));
#111389=CARTESIAN_POINT('Ctrl Pts',(5.02938742677268,8.1235150580717,27.7658762532179));
#111390=CARTESIAN_POINT('Ctrl Pts',(5.27126938141252,8.09977241356497,27.4460750379062));
#111391=CARTESIAN_POINT('Ctrl Pts',(5.68672544385794,8.07602976905825,27.2575567648121));
#111392=CARTESIAN_POINT('Ctrl Pts',(6.08668048353732,8.05228712455152,27.2861165885187));
#111393=CARTESIAN_POINT('Ctrl Pts',(6.48663552321671,8.02854448004479,27.3146764122254));
#111394=CARTESIAN_POINT('Ctrl Pts',(6.87108954013006,8.00480183553806,27.5603143327329));
#111395=CARTESIAN_POINT('Ctrl Pts',(7.0650765149634,7.98105919103133,27.9112398959091));
#111396=CARTESIAN_POINT('Ctrl Pts',(7.25906348979675,7.95731654652461,28.2621654590854));
#111397=CARTESIAN_POINT('Ctrl Pts',(7.26258342255009,7.93357390201789,28.7183786649305));
#111398=CARTESIAN_POINT('Ctrl Pts',(7.07403438270397,7.90983125751116,29.0722557012979));
#111399=CARTESIAN_POINT('Ctrl Pts',(6.88548534285785,7.88608861300444,29.4261327376653));
#111400=CARTESIAN_POINT('Ctrl Pts',(6.50486733041225,7.86234596849771,29.6776736045549));
#111401=CARTESIAN_POINT('Ctrl Pts',(6.10540058911368,7.83860332399098,29.7124014016435));
#111402=CARTESIAN_POINT('Ctrl Pts',(5.70593384781511,7.81486067948425,29.7471291987322));
#111403=CARTESIAN_POINT('Ctrl Pts',(5.28761837766355,7.79111803497753,29.5650439260198));
#111404=CARTESIAN_POINT('Ctrl Pts',(5.04083063307749,7.7673753904708,29.2490130629383));
#111405=CARTESIAN_POINT('Ctrl Pts',(4.87631430063006,7.75154781036385,29.0383371291655));
#111406=CARTESIAN_POINT('Ctrl Pts',(4.78802432957745,7.73572023025689,28.7681362122154));
#111407=CARTESIAN_POINT('Ctrl Pts',(4.78610753914613,7.71989265014994,28.499077712745));
#111408=CARTESIAN_POINT('Origin',(6.,11.5,28.5));
#111409=CARTESIAN_POINT('',(4.78306041506863,7.20510734985006,28.4998165775134));
#111410=CARTESIAN_POINT('',(4.78303957841512,7.26989265014994,28.4998847090757));
#111411=CARTESIAN_POINT('',(4.785,11.5,28.5));
#111412=CARTESIAN_POINT('Ctrl Pts',(4.78306041506863,7.20510734985006,28.4998165775134));
#111413=CARTESIAN_POINT('Ctrl Pts',(4.78388808820232,7.22825779003458,28.8908188285037));
#111414=CARTESIAN_POINT('Ctrl Pts',(4.98932111084564,7.25140823021909,29.2825688683523));
#111415=CARTESIAN_POINT('Ctrl Pts',(5.31176728118342,7.27455867040361,29.5036744356945));
#111416=CARTESIAN_POINT('Ctrl Pts',(5.64246184827877,7.29830131491034,29.7304360368572));
#111417=CARTESIAN_POINT('Ctrl Pts',(6.09623268819263,7.32204395941706,29.7777110925591));
#111418=CARTESIAN_POINT('Ctrl Pts',(6.46656751884371,7.34578660392379,29.6239846064782));
#111419=CARTESIAN_POINT('Ctrl Pts',(6.83690234949481,7.36952924843052,29.4702581203973));
#111420=CARTESIAN_POINT('Ctrl Pts',(7.12380117088312,7.39327189293724,29.1155300925335));
#111421=CARTESIAN_POINT('Ctrl Pts',(7.1966955844278,7.41701453744397,28.7212381654897));
#111422=CARTESIAN_POINT('Ctrl Pts',(7.26958999797249,7.4407571819507,28.3269462384458));
#111423=CARTESIAN_POINT('Ctrl Pts',(7.12848000367358,7.46449982645743,27.8930904122219));
#111424=CARTESIAN_POINT('Ctrl Pts',(6.83758512637848,7.48824247096415,27.6171195986246));
#111425=CARTESIAN_POINT('Ctrl Pts',(6.54669024908336,7.51198511547088,27.3411487850273));
#111426=CARTESIAN_POINT('Ctrl Pts',(6.10601048879204,7.5357277599776,27.2230629840567));
#111427=CARTESIAN_POINT('Ctrl Pts',(5.71610034592059,7.55947040448433,27.3166033491798));
#111428=CARTESIAN_POINT('Ctrl Pts',(5.32619020304914,7.58321304899106,27.4101437143029));
#111429=CARTESIAN_POINT('Ctrl Pts',(4.98704967759756,7.60695569349778,27.7153102455197));
#111430=CARTESIAN_POINT('Ctrl Pts',(4.85302250170622,7.63069833800451,28.0932208639892));
#111431=CARTESIAN_POINT('Ctrl Pts',(4.80709289568964,7.63883467528636,28.2227265832611));
#111432=CARTESIAN_POINT('Ctrl Pts',(4.78525089539238,7.64697101256821,28.3607750468054));
#111433=CARTESIAN_POINT('Ctrl Pts',(4.78619455170653,7.65510734985006,28.4991124767033));
#111434=CARTESIAN_POINT('Ctrl Pts',(4.78610753914613,7.71989265014994,28.499077712745));
#111435=CARTESIAN_POINT('Ctrl Pts',(4.78514898960146,7.71197758575017,28.364526799957));
#111436=CARTESIAN_POINT('Ctrl Pts',(4.80579069004693,7.70406252135039,28.2302615835272));
#111437=CARTESIAN_POINT('Ctrl Pts',(4.84930160570745,7.69614745695062,28.103869152572));
#111438=CARTESIAN_POINT('Ctrl Pts',(4.97982034194404,7.67240481244389,27.7247325587378));
#111439=CARTESIAN_POINT('Ctrl Pts',(5.31611783343779,7.64866216793716,27.4164358245197));
#111440=CARTESIAN_POINT('Ctrl Pts',(5.70514422034347,7.62491952343044,27.3192855925029));
#111441=CARTESIAN_POINT('Ctrl Pts',(6.09417060724916,7.60117687892371,27.2221353604861));
#111442=CARTESIAN_POINT('Ctrl Pts',(6.5359258895668,7.57743423441699,27.3361316306704));
#111443=CARTESIAN_POINT('Ctrl Pts',(6.82936609368032,7.55369158991026,27.6093944051656));
#111444=CARTESIAN_POINT('Ctrl Pts',(7.12280629779385,7.52994894540353,27.8826571796608));
#111445=CARTESIAN_POINT('Ctrl Pts',(7.26793142370327,7.5062063008968,28.3151864584669));
#111446=CARTESIAN_POINT('Ctrl Pts',(7.19869465042118,7.48246365639008,28.7101370458817));
#111447=CARTESIAN_POINT('Ctrl Pts',(7.12945787713909,7.45872101188335,29.1050876332965));
#111448=CARTESIAN_POINT('Ctrl Pts',(6.84585920466548,7.43497836737663,29.4624595293201));
#111449=CARTESIAN_POINT('Ctrl Pts',(6.47696512397243,7.4112357228699,29.619611858273));
#111450=CARTESIAN_POINT('Ctrl Pts',(6.10807104327939,7.38749307836317,29.7767641872259));
#111451=CARTESIAN_POINT('Ctrl Pts',(5.65388155436692,7.36375043385644,29.7336969491082));
#111452=CARTESIAN_POINT('Ctrl Pts',(5.3210994700661,7.34000778934971,29.5100101551136));
#111453=CARTESIAN_POINT('Ctrl Pts',(4.99351644174012,7.31663607628312,29.2898180208909));
#111454=CARTESIAN_POINT('Ctrl Pts',(4.78357695409633,7.29326436321653,28.8946058857237));
#111455=CARTESIAN_POINT('Ctrl Pts',(4.78303957841512,7.26989265014994,28.4998847090757));
#111456=CARTESIAN_POINT('Origin',(6.,11.5,28.5));
#111457=CARTESIAN_POINT('',(4.78568939793849,6.75510734985006,28.5010383098413));
#111458=CARTESIAN_POINT('',(4.7857905243208,6.81989265014994,28.5010169731875));
#111459=CARTESIAN_POINT('',(4.785,11.5,28.5));
#111460=CARTESIAN_POINT('Ctrl Pts',(4.78568939793849,6.75510734985006,28.5010383098413));
#111461=CARTESIAN_POINT('Ctrl Pts',(4.7847179759516,6.76205927848748,28.6191136444317));
#111462=CARTESIAN_POINT('Ctrl Pts',(4.80055291679293,6.76901120712491,28.7369340126475));
#111463=CARTESIAN_POINT('Ctrl Pts',(4.83426069151918,6.77596313576234,28.8493975371586));
#111464=CARTESIAN_POINT('Ctrl Pts',(4.94938150966584,6.79970578026907,29.2334897253414));
#111465=CARTESIAN_POINT('Ctrl Pts',(5.27297109019361,6.8234484247758,29.5550996801765));
#111466=CARTESIAN_POINT('Ctrl Pts',(5.65776265710716,6.84719106928253,29.6678614486722));
#111467=CARTESIAN_POINT('Ctrl Pts',(6.04255422402072,6.87093371378926,29.780623217168));
#111468=CARTESIAN_POINT('Ctrl Pts',(6.48854777732007,6.89467635829598,29.6845367993243));
#111469=CARTESIAN_POINT('Ctrl Pts',(6.79277065916322,6.91841900280271,29.4233315931834));
#111470=CARTESIAN_POINT('Ctrl Pts',(7.09699354100638,6.94216164730943,29.1621263870424));
#111471=CARTESIAN_POINT('Ctrl Pts',(7.25944575139334,6.96590429181616,28.7358023926042));
#111472=CARTESIAN_POINT('Ctrl Pts',(7.20619478426713,6.98964693632289,28.3383806513713));
#111473=CARTESIAN_POINT('Ctrl Pts',(7.15294381714092,7.01338958082961,27.9409589101385));
#111474=CARTESIAN_POINT('Ctrl Pts',(6.88398967250154,7.03713222533635,27.572439422111));
#111475=CARTESIAN_POINT('Ctrl Pts',(6.52173412170005,7.06087486984307,27.4005364192623));
#111476=CARTESIAN_POINT('Ctrl Pts',(6.15947857089856,7.0846175143498,27.2286334164135));
#111477=CARTESIAN_POINT('Ctrl Pts',(5.70392161393496,7.10836015885652,27.2533468987435));
#111478=CARTESIAN_POINT('Ctrl Pts',(5.36238838021367,7.13210280336325,27.4634296666103));
#111479=CARTESIAN_POINT('Ctrl Pts',(5.02085514649238,7.15584544786997,27.6735124344772));
#111480=CARTESIAN_POINT('Ctrl Pts',(4.79334563601341,7.1795880923767,28.0689644878809));
#111481=CARTESIAN_POINT('Ctrl Pts',(4.78340002791233,7.20333073688343,28.4698145878945));
#111482=CARTESIAN_POINT('Ctrl Pts',(4.78315195815318,7.20392294120564,28.4798128491126));
#111483=CARTESIAN_POINT('Ctrl Pts',(4.78303924261562,7.20451514552785,28.489814468647));
#111484=CARTESIAN_POINT('Ctrl Pts',(4.78306041506863,7.20510734985006,28.4998165775134));
#111485=CARTESIAN_POINT('Ctrl Pts',(4.78303957841512,7.26989265014994,28.4998847090757));
#111486=CARTESIAN_POINT('Ctrl Pts',(4.78303104974909,7.26952171870981,28.493620106473));
#111487=CARTESIAN_POINT('Ctrl Pts',(4.78307526680697,7.26915078726967,28.4873556275365));
#111488=CARTESIAN_POINT('Ctrl Pts',(4.78317259641123,7.26877985582953,28.4810919739049));
#111489=CARTESIAN_POINT('Ctrl Pts',(4.78940248674633,7.24503721132281,28.0801669365623));
#111490=CARTESIAN_POINT('Ctrl Pts',(5.01323694710571,7.22129456681608,27.6826232117484));
#111491=CARTESIAN_POINT('Ctrl Pts',(5.35280833269681,7.19755192230936,27.4693839769732));
#111492=CARTESIAN_POINT('Ctrl Pts',(5.69237971828791,7.17380927780263,27.256144742198));
#111493=CARTESIAN_POINT('Ctrl Pts',(6.14768802911073,7.1500666332959,27.2272099974613));
#111494=CARTESIAN_POINT('Ctrl Pts',(6.51152127673494,7.12632398878917,27.3957480235561));
#111495=CARTESIAN_POINT('Ctrl Pts',(6.87535452435914,7.10258134428244,27.5642860496508));
#111496=CARTESIAN_POINT('Ctrl Pts',(7.14771270878473,7.07883869977572,27.9302968465769));
#111497=CARTESIAN_POINT('Ctrl Pts',(7.20464490743174,7.05509605526899,28.3272079454368));
#111498=CARTESIAN_POINT('Ctrl Pts',(7.26157710607875,7.03135341076227,28.7241190442966));
#111499=CARTESIAN_POINT('Ctrl Pts',(7.10308331894717,7.00761076625553,29.1519304450902));
#111500=CARTESIAN_POINT('Ctrl Pts',(6.80129449308499,6.98386812174881,29.4159440839734));
#111501=CARTESIAN_POINT('Ctrl Pts',(6.4995056672228,6.96012547724208,29.6799577228565));
#111502=CARTESIAN_POINT('Ctrl Pts',(6.05442180263,6.93638283273536,29.7801735998292));
#111503=CARTESIAN_POINT('Ctrl Pts',(5.66860169247643,6.91264018822864,29.6709831838372));
#111504=CARTESIAN_POINT('Ctrl Pts',(5.28278158232287,6.88889754372191,29.5617927678452));
#111505=CARTESIAN_POINT('Ctrl Pts',(4.95622522660852,6.86515489921517,29.2431960588884));
#111506=CARTESIAN_POINT('Ctrl Pts',(4.83754932146633,6.84141225470845,28.8601872949515));
#111507=CARTESIAN_POINT('Ctrl Pts',(4.80169458831506,6.83423905318894,28.7444714972999));
#111508=CARTESIAN_POINT('Ctrl Pts',(4.78481484417915,6.82706585166944,28.6228762721584));
#111509=CARTESIAN_POINT('Ctrl Pts',(4.7857905243208,6.81989265014994,28.5010169731875));
#111510=CARTESIAN_POINT('Origin',(6.,11.5,28.5));
#111511=CARTESIAN_POINT('',(4.78657973631996,6.30510734985006,28.4993396990272));
#111512=CARTESIAN_POINT('',(4.7865055641924,6.36989265014994,28.4992804641432));
#111513=CARTESIAN_POINT('',(4.785,11.5,28.5));
#111514=CARTESIAN_POINT('Ctrl Pts',(4.78657973631996,6.30510734985006,28.4993396990272));
#111515=CARTESIAN_POINT('Ctrl Pts',(4.78782730054607,6.31960341144713,28.7459941216511));
#111516=CARTESIAN_POINT('Ctrl Pts',(4.86088012182984,6.3340994730442,28.9933240138827));
#111517=CARTESIAN_POINT('Ctrl Pts',(5.00056288347954,6.34859553464127,29.1943722062399));
#111518=CARTESIAN_POINT('Ctrl Pts',(5.2293448965359,6.37233817914799,29.5236627330422));
#111519=CARTESIAN_POINT('Ctrl Pts',(5.63686929643189,6.39608082365472,29.7287973404918));
#111520=CARTESIAN_POINT('Ctrl Pts',(6.03765321153539,6.41982346816145,29.716395274483));
#111521=CARTESIAN_POINT('Ctrl Pts',(6.4384371266389,6.44356611266817,29.7039932084742));
#111522=CARTESIAN_POINT('Ctrl Pts',(6.83248055694992,6.4673087571749,29.4740544690069));
#111523=CARTESIAN_POINT('Ctrl Pts',(7.04046227913832,6.49105140168162,29.1312368157233));
#111524=CARTESIAN_POINT('Ctrl Pts',(7.24844400132672,6.51479404618835,28.7884191624396));
#111525=CARTESIAN_POINT('Ctrl Pts',(7.2703640153925,6.53853669069508,28.3327225953394));
#111526=CARTESIAN_POINT('Ctrl Pts',(7.09624186544805,6.56227933520181,27.9715296209521));
#111527=CARTESIAN_POINT('Ctrl Pts',(6.92211971550361,6.58602197970853,27.6103366465647));
#111528=CARTESIAN_POINT('Ctrl Pts',(6.55195540154897,6.60976462421526,27.34364726489));
#111529=CARTESIAN_POINT('Ctrl Pts',(6.15421402361284,6.63350726872199,27.2928356778359));
#111530=CARTESIAN_POINT('Ctrl Pts',(5.75647264567669,6.65724991322871,27.2420240907819));
#111531=CARTESIAN_POINT('Ctrl Pts',(5.33115420375906,6.68099255773544,27.4070902983484));
#111532=CARTESIAN_POINT('Ctrl Pts',(5.07182101068302,6.70473520224217,27.7129106128969));
#111533=CARTESIAN_POINT('Ctrl Pts',(4.88842147575827,6.72152591811147,27.9291856789363));
#111534=CARTESIAN_POINT('Ctrl Pts',(4.78803563470554,6.73831663398076,28.2158556651857));
#111535=CARTESIAN_POINT('Ctrl Pts',(4.78568939793849,6.75510734985006,28.5010383098413));
#111536=CARTESIAN_POINT('Ctrl Pts',(4.7857905243208,6.81989265014994,28.5010169731875));
#111537=CARTESIAN_POINT('Ctrl Pts',(4.78804425669356,6.80332320716271,28.2195330777089));
#111538=CARTESIAN_POINT('Ctrl Pts',(4.88556881466696,6.78675376417549,27.9366401688485));
#111539=CARTESIAN_POINT('Ctrl Pts',(5.0645656358046,6.77018432118827,27.7215471145434));
#111540=CARTESIAN_POINT('Ctrl Pts',(5.32105330985508,6.74644167668155,27.4133365169892));
#111541=CARTESIAN_POINT('Ctrl Pts',(5.74482411252607,6.72269903217482,27.2443361407978));
#111542=CARTESIAN_POINT('Ctrl Pts',(6.14301905243894,6.69895638766809,27.2914586854481));
#111543=CARTESIAN_POINT('Ctrl Pts',(6.54121399235184,6.67521374316136,27.3385812300984));
#111544=CARTESIAN_POINT('Ctrl Pts',(6.91383306950661,6.65147109865463,27.6018266955903));
#111545=CARTESIAN_POINT('Ctrl Pts',(7.09129598870183,6.62772845414791,27.9613910176794));
#111546=CARTESIAN_POINT('Ctrl Pts',(7.26875890789705,6.60398580964118,28.3209553397684));
#111547=CARTESIAN_POINT('Ctrl Pts',(7.25106566913272,6.58024316513446,28.7768385184546));
#111548=CARTESIAN_POINT('Ctrl Pts',(7.04626926625309,6.55650052062773,29.1215676599761));
#111549=CARTESIAN_POINT('Ctrl Pts',(6.84147286337347,6.532757876121,29.4662968014976));
#111550=CARTESIAN_POINT('Ctrl Pts',(6.44957329637856,6.50901523161427,29.6998719058545));
#111551=CARTESIAN_POINT('Ctrl Pts',(6.04892360307319,6.48527258710755,29.7159909311749));
#111552=CARTESIAN_POINT('Ctrl Pts',(5.64827390976782,6.46152994260082,29.7321099564952));
#111553=CARTESIAN_POINT('Ctrl Pts',(5.238874090152,6.43778729809409,29.5307729027791));
#111554=CARTESIAN_POINT('Ctrl Pts',(5.00704592749372,6.41404465358737,29.2036115246945));
#111555=CARTESIAN_POINT('Ctrl Pts',(4.86334278564024,6.39932731910822,29.0008142571633));
#111556=CARTESIAN_POINT('Ctrl Pts',(4.78786939497795,6.38460998462908,28.7496705221128));
#111557=CARTESIAN_POINT('Ctrl Pts',(4.7865055641924,6.36989265014994,28.4992804641432));
#111558=CARTESIAN_POINT('Origin',(6.,11.5,28.5));
#111559=CARTESIAN_POINT('',(4.78521076863826,5.85510734985006,28.4999698544854));
#111560=CARTESIAN_POINT('',(4.78332770288896,5.91989265014994,28.4996492411853));
#111561=CARTESIAN_POINT('',(4.785,11.5,28.5));
#111562=CARTESIAN_POINT('Ctrl Pts',(4.78521076863826,5.85510734985006,28.4999698544854));
#111563=CARTESIAN_POINT('Ctrl Pts',(4.78688595225555,5.87714754440676,28.8736362294688));
#111564=CARTESIAN_POINT('Ctrl Pts',(4.9692800988606,5.89918773896347,29.2462280232147));
#111565=CARTESIAN_POINT('Ctrl Pts',(5.26571199057474,5.92122793352018,29.4703193131787));
#111566=CARTESIAN_POINT('Ctrl Pts',(5.58504116016609,5.94497057802691,29.7117200785386));
#111567=CARTESIAN_POINT('Ctrl Pts',(6.03670570510543,5.96871322253364,29.7807930774338));
#111568=CARTESIAN_POINT('Ctrl Pts',(6.41393766043131,5.99245586704037,29.6446392534136));
#111569=CARTESIAN_POINT('Ctrl Pts',(6.7911696157572,6.01619851154709,29.5084854293935));
#111570=CARTESIAN_POINT('Ctrl Pts',(7.09396898146964,6.03994115605382,29.1671047824581));
#111571=CARTESIAN_POINT('Ctrl Pts',(7.18504576598691,6.06368380056054,28.7765363638774));
#111572=CARTESIAN_POINT('Ctrl Pts',(7.27612255050417,6.08742644506727,28.3859679452967));
#111573=CARTESIAN_POINT('Ctrl Pts',(7.15547675382629,6.11116908957399,27.9462117550706));
#111574=CARTESIAN_POINT('Ctrl Pts',(6.8777606839509,6.13491173408072,27.6570623303207));
#111575=CARTESIAN_POINT('Ctrl Pts',(6.6000446140755,6.15865437858745,27.3679129055707));
#111576=CARTESIAN_POINT('Ctrl Pts',(6.16525827100258,6.18239702309418,27.2293702462968));
#111577=CARTESIAN_POINT('Ctrl Pts',(5.7714033811428,6.2061396676009,27.3046591166773));
#111578=CARTESIAN_POINT('Ctrl Pts',(5.37754849128302,6.22988231210763,27.3799479870579));
#111579=CARTESIAN_POINT('Ctrl Pts',(5.02462505463636,6.25362495661436,27.6690683870929));
#111580=CARTESIAN_POINT('Ctrl Pts',(4.8731831494214,6.27736760112108,28.0403518101878));
#111581=CARTESIAN_POINT('Ctrl Pts',(4.81420403560912,6.28661418403074,28.1849482957923));
#111582=CARTESIAN_POINT('Ctrl Pts',(4.7857839542398,6.2958607669404,28.3420065810935));
#111583=CARTESIAN_POINT('Ctrl Pts',(4.78657973631996,6.30510734985006,28.4993396990272));
#111584=CARTESIAN_POINT('Ctrl Pts',(4.7865055641924,6.36989265014994,28.4992804641432));
#111585=CARTESIAN_POINT('Ctrl Pts',(4.78566920379832,6.36086734012235,28.3457303831688));
#111586=CARTESIAN_POINT('Ctrl Pts',(4.81270304898673,6.35184203009477,28.1924637357382));
#111587=CARTESIAN_POINT('Ctrl Pts',(4.86896310729236,6.34281672006719,28.0508040477679));
#111588=CARTESIAN_POINT('Ctrl Pts',(5.01696495545002,6.31907407556046,27.6781436513788));
#111589=CARTESIAN_POINT('Ctrl Pts',(5.36722515746609,6.29533143105373,27.3858085610538));
#111590=CARTESIAN_POINT('Ctrl Pts',(5.76035025534992,6.27158878654701,27.3068516283844));
#111591=CARTESIAN_POINT('Ctrl Pts',(6.15347535323376,6.24784614204028,27.2278946957151));
#111592=CARTESIAN_POINT('Ctrl Pts',(6.58946534698536,6.22410349753355,27.3623159207015));
#111593=CARTESIAN_POINT('Ctrl Pts',(6.86987889282973,6.20036085302683,27.6489196092493));
#111594=CARTESIAN_POINT('Ctrl Pts',(7.15029243867409,6.1766182085201,27.9355232977971));
#111595=CARTESIAN_POINT('Ctrl Pts',(7.27512953661121,6.15287556401338,28.3743094499063));
#111596=CARTESIAN_POINT('Ctrl Pts',(7.18761773225989,6.12913291950665,28.76562478708));
#111597=CARTESIAN_POINT('Ctrl Pts',(7.10010592790856,6.10539027499992,29.1569401242537));
#111598=CARTESIAN_POINT('Ctrl Pts',(6.80024522126877,6.08164763049319,29.500784646492));
#111599=CARTESIAN_POINT('Ctrl Pts',(6.42442266508831,6.05790498598646,29.6405969976474));
#111600=CARTESIAN_POINT('Ctrl Pts',(6.04860010890784,6.03416234147974,29.7804093488027));
#111601=CARTESIAN_POINT('Ctrl Pts',(5.5968157031867,6.01041969697301,29.7161895288751));
#111602=CARTESIAN_POINT('Ctrl Pts',(5.27483437848997,5.98667705246629,29.4773138784283));
#111603=CARTESIAN_POINT('Ctrl Pts',(4.97293975282596,5.96441558502751,29.2533404068618));
#111604=CARTESIAN_POINT('Ctrl Pts',(4.78515793691401,5.94215411758873,28.8758230640495));
#111605=CARTESIAN_POINT('Ctrl Pts',(4.78332770288896,5.91989265014994,28.4996492411853));
#111606=CARTESIAN_POINT('Origin',(6.,12.2318726682356,28.5));
#111607=CARTESIAN_POINT('',(5.04299591138157,6.15687266823562,28.4994792317636));
#111608=CARTESIAN_POINT('',(5.04043108748423,6.06812733176437,28.4997233624409));
#111609=CARTESIAN_POINT('',(5.04175,12.2318726682356,28.4999999999999));
#111610=CARTESIAN_POINT('',(6.39740818880394,5.85,29.3719574496336));
#111611=CARTESIAN_POINT('Ctrl Pts',(5.04299591138157,6.15687266823562,28.4994792317636));
#111612=CARTESIAN_POINT('Ctrl Pts',(5.04236829148172,6.14762608532596,28.375393256241));
#111613=CARTESIAN_POINT('Ctrl Pts',(5.12233675351758,6.11463685790957,27.9334624481512));
#111614=CARTESIAN_POINT('Ctrl Pts',(5.78742775715113,6.05790498598646,27.388609494045));
#111615=CARTESIAN_POINT('Ctrl Pts',(6.81615371579216,5.98667705246629,27.7164082674999));
#111616=CARTESIAN_POINT('Ctrl Pts',(7.09388787989744,5.91737539047079,28.7287545013986));
#111617=CARTESIAN_POINT('Ctrl Pts',(6.66163337938062,5.87181637298203,29.2514323241542));
#111618=CARTESIAN_POINT('Ctrl Pts',(6.39766230306601,5.85,29.3734910038904));
#111619=CARTESIAN_POINT('',(6.95384139680377,5.85,28.4081868623593));
#111620=CARTESIAN_POINT('Origin',(6.,5.85,28.5));
#111621=CARTESIAN_POINT('Ctrl Pts',(5.04043108748423,6.06812733176437,28.4997233624409));
#111622=CARTESIAN_POINT('Ctrl Pts',(5.04033504522546,6.06664615469643,28.479983491394));
#111623=CARTESIAN_POINT('Ctrl Pts',(5.0497558598512,6.04142233312176,28.1439016856491));
#111624=CARTESIAN_POINT('Ctrl Pts',(5.44295412205162,5.99245586704036,27.5143710763459));
#111625=CARTESIAN_POINT('Ctrl Pts',(6.52391074184675,5.92122793352018,27.4975948676703));
#111626=CARTESIAN_POINT('Ctrl Pts',(6.92340443678229,5.87374264450673,28.0919790384314));
#111627=CARTESIAN_POINT('Ctrl Pts',(6.95384139680377,5.85,28.4081868623593));
#111628=CARTESIAN_POINT('Origin',(6.,12.2318726682356,28.5));
#111629=CARTESIAN_POINT('',(5.04229371652227,6.60687266823562,28.500818897453));
#111630=CARTESIAN_POINT('',(5.04293741307602,6.51812733176437,28.49943251421));
#111631=CARTESIAN_POINT('',(5.04175,12.2318726682356,28.4999999999999));
#111632=CARTESIAN_POINT('Ctrl Pts',(5.04229371652227,6.60687266823562,28.500818897453));
#111633=CARTESIAN_POINT('Ctrl Pts',(5.04414415387375,6.59008195236632,28.2759001573367));
#111634=CARTESIAN_POINT('Ctrl Pts',(5.23526955473714,6.5495485919903,27.7301068914455));
#111635=CARTESIAN_POINT('Ctrl Pts',(6.14337556352862,6.48527258710754,27.3776706926676));
#111636=CARTESIAN_POINT('Ctrl Pts',(7.01920261006453,6.41404465358737,28.0086709395559));
#111637=CARTESIAN_POINT('Ctrl Pts',(6.96733877431504,6.34281672006719,29.0868715208489));
#111638=CARTESIAN_POINT('Ctrl Pts',(6.03501255926435,6.271588786547,29.630917933428));
#111639=CARTESIAN_POINT('Ctrl Pts',(5.19596203684428,6.20960743593649,29.2085670273447));
#111640=CARTESIAN_POINT('Ctrl Pts',(5.04397984423725,6.17136872983269,28.6940114132281));
#111641=CARTESIAN_POINT('Ctrl Pts',(5.04299591138157,6.15687266823562,28.4994792317636));
#111642=CARTESIAN_POINT('Ctrl Pts',(5.04293741307602,6.51812733176437,28.49943251421));
#111643=CARTESIAN_POINT('Ctrl Pts',(5.04227778974465,6.50910202173679,28.3783301561082));
#111644=CARTESIAN_POINT('Ctrl Pts',(5.11968788031139,6.47633406720248,27.9394586239317));
#111645=CARTESIAN_POINT('Ctrl Pts',(5.77718546973152,6.41982346816144,27.3906962578813));
#111646=CARTESIAN_POINT('Ctrl Pts',(6.80875932531787,6.34859553464126,27.7087435142843));
#111647=CARTESIAN_POINT('Ctrl Pts',(7.10413006383205,6.27736760112109,28.7469332186266));
#111648=CARTESIAN_POINT('Ctrl Pts',(6.39464482398617,6.2061396676009,29.5604863382188));
#111649=CARTESIAN_POINT('Ctrl Pts',(5.34792918744311,6.13639291114867,29.4116987996429));
#111650=CARTESIAN_POINT('Ctrl Pts',(5.04187456217927,6.09038879920316,28.7964053095682));
#111651=CARTESIAN_POINT('Ctrl Pts',(5.04043108748423,6.06812733176437,28.4997233624409));
#111652=CARTESIAN_POINT('Origin',(6.,12.2318726682356,28.5));
#111653=CARTESIAN_POINT('',(5.04022028209014,7.05687266823562,28.4998553377795));
#111654=CARTESIAN_POINT('',(5.04237347319375,6.96812733176437,28.500802069594));
#111655=CARTESIAN_POINT('',(5.04175,12.2318726682356,28.4999999999999));
#111656=CARTESIAN_POINT('Ctrl Pts',(5.04022028209014,7.05687266823562,28.4998553377795));
#111657=CARTESIAN_POINT('Ctrl Pts',(5.04020358373367,7.05628046391341,28.4919668432765));
#111658=CARTESIAN_POINT('Ctrl Pts',(5.04385653111531,7.03194561508447,28.1678288346137));
#111659=CARTESIAN_POINT('Ctrl Pts',(5.40719788686653,6.98386812174881,27.5362768396409));
#111660=CARTESIAN_POINT('Ctrl Pts',(6.48506814368224,6.91264018822863,27.4778035200293));
#111661=CARTESIAN_POINT('Ctrl Pts',(7.12142693158516,6.84141225470845,28.3497388271955));
#111662=CARTESIAN_POINT('Ctrl Pts',(6.73705697947822,6.77018432118827,29.3584424510732));
#111663=CARTESIAN_POINT('Ctrl Pts',(5.68181420799896,6.6989563876681,29.5857876606995));
#111664=CARTESIAN_POINT('Ctrl Pts',(5.09666865493704,6.6445191700172,29.0042218556903));
#111665=CARTESIAN_POINT('Ctrl Pts',(5.04152757239145,6.61382459687305,28.5939429216269));
#111666=CARTESIAN_POINT('Ctrl Pts',(5.04229371652227,6.60687266823562,28.500818897453));
#111667=CARTESIAN_POINT('Ctrl Pts',(5.04237347319375,6.96812733176437,28.500802069594));
#111668=CARTESIAN_POINT('Ctrl Pts',(5.04415095389023,6.95155788877715,28.2788004705469));
#111669=CARTESIAN_POINT('Ctrl Pts',(5.23128117013677,6.9112458012832,27.7359852831753));
#111670=CARTESIAN_POINT('Ctrl Pts',(6.13296796501039,6.84719106928253,27.3763913550898));
#111671=CARTESIAN_POINT('Ctrl Pts',(7.01460310250063,6.77596313576235,27.9992431262198));
#111672=CARTESIAN_POINT('Ctrl Pts',(6.97274002584404,6.70473520224217,29.0778852397409));
#111673=CARTESIAN_POINT('Ctrl Pts',(6.04548629726899,6.63350726872199,29.6305354712223));
#111674=CARTESIAN_POINT('Ctrl Pts',(5.19956529207796,6.57130464522939,29.2145234587558));
#111675=CARTESIAN_POINT('Ctrl Pts',(5.04401304340543,6.53284466624352,28.6969109282424));
#111676=CARTESIAN_POINT('Ctrl Pts',(5.04293741307602,6.51812733176437,28.49943251421));
#111677=CARTESIAN_POINT('Origin',(6.,12.2318726682356,28.5));
#111678=CARTESIAN_POINT('',(5.04269212277596,7.50687266823562,28.4993000253505));
#111679=CARTESIAN_POINT('',(5.04020384857308,7.41812733176437,28.4999090719931));
#111680=CARTESIAN_POINT('',(5.04175,12.2318726682356,28.4999999999999));
#111681=CARTESIAN_POINT('Ctrl Pts',(5.04269212277596,7.50687266823562,28.4993000253505));
#111682=CARTESIAN_POINT('Ctrl Pts',(5.04194787696276,7.49873633095377,28.3901956284784));
#111683=CARTESIAN_POINT('Ctrl Pts',(5.10944269904413,7.4668573491652,27.9636066549997));
#111684=CARTESIAN_POINT('Ctrl Pts',(5.73605199225171,7.41123572286989,27.399769041722));
#111685=CARTESIAN_POINT('Ctrl Pts',(6.77872206706446,7.34000778934971,27.679165878216));
#111686=CARTESIAN_POINT('Ctrl Pts',(7.11259528197041,7.26877985582954,28.705690188041));
#111687=CARTESIAN_POINT('Ctrl Pts',(6.43377850272267,7.19755192230935,29.5449942194001));
#111688=CARTESIAN_POINT('Ctrl Pts',(5.36906079542399,7.12691619311139,29.4340690904762));
#111689=CARTESIAN_POINT('Ctrl Pts',(5.0408730539258,7.08002310842014,28.8082322159783));
#111690=CARTESIAN_POINT('Ctrl Pts',(5.04022028209014,7.05687266823562,28.4998553377795));
#111691=CARTESIAN_POINT('Ctrl Pts',(5.04020384857308,7.41812733176437,28.4999090719931));
#111692=CARTESIAN_POINT('Ctrl Pts',(5.04019712215809,7.41775640032424,28.4949682856195));
#111693=CARTESIAN_POINT('Ctrl Pts',(5.04246416833165,7.39364282437738,28.1737831212255));
#111694=CARTESIAN_POINT('Ctrl Pts',(5.39829109152546,7.34578660392379,27.5418126900042));
#111695=CARTESIAN_POINT('Ctrl Pts',(6.47557303929329,7.27455867040361,27.4733516550811));
#111696=CARTESIAN_POINT('Ctrl Pts',(7.1199859534311,7.20333073688343,28.3393512752155));
#111697=CARTESIAN_POINT('Ctrl Pts',(6.7449818262241,7.13210280336324,29.351574175982));
#111698=CARTESIAN_POINT('Ctrl Pts',(5.69189142314743,7.06087486984307,29.5886898898316));
#111699=CARTESIAN_POINT('Ctrl Pts',(5.09898079581291,7.00621637931011,29.0102311605227));
#111700=CARTESIAN_POINT('Ctrl Pts',(5.04160397072811,6.97530053328388,28.5969104426302));
#111701=CARTESIAN_POINT('Ctrl Pts',(5.04237347319375,6.96812733176437,28.500802069594));
#111702=CARTESIAN_POINT('Origin',(6.,12.2318726682356,28.5));
#111703=CARTESIAN_POINT('',(5.04266942812141,7.95687266823562,28.5007094137961));
#111704=CARTESIAN_POINT('',(5.04262349743768,7.86812733176438,28.4992726076031));
#111705=CARTESIAN_POINT('',(5.04175,12.2318726682356,28.4999999999999));
#111706=CARTESIAN_POINT('Ctrl Pts',(5.04266942812141,7.95687266823562,28.5007094137961));
#111707=CARTESIAN_POINT('Ctrl Pts',(5.04412538743029,7.94119219799413,28.290454354913));
#111708=CARTESIAN_POINT('Ctrl Pts',(5.21569019260146,7.90176908324592,27.7596801563291));
#111709=CARTESIAN_POINT('Ctrl Pts',(6.09104560108126,7.83860332399098,27.372220140497));
#111710=CARTESIAN_POINT('Ctrl Pts',(6.99525699353418,7.76737539047079,27.9618176611926));
#111711=CARTESIAN_POINT('Ctrl Pts',(6.99358031256864,7.69614745695062,29.041271535836));
#111712=CARTESIAN_POINT('Ctrl Pts',(6.08754168182046,7.62491952343044,29.6280572533568));
#111713=CARTESIAN_POINT('Ctrl Pts',(5.2144204906732,7.56182792719211,29.2383378989303));
#111714=CARTESIAN_POINT('Ctrl Pts',(5.04411966054992,7.5224789754605,28.7085731513516));
#111715=CARTESIAN_POINT('Ctrl Pts',(5.04269212277596,7.50687266823562,28.4993000253505));
#111716=CARTESIAN_POINT('Ctrl Pts',(5.04262349743768,7.86812733176438,28.4992726076031));
#111717=CARTESIAN_POINT('Ctrl Pts',(5.04186750558486,7.8602122673646,28.3931545728878));
#111718=CARTESIAN_POINT('Ctrl Pts',(5.10698130687874,7.8285545584581,27.9696178276289));
#111719=CARTESIAN_POINT('Ctrl Pts',(5.72586583137092,7.77315420504486,27.4022627845939));
#111720=CARTESIAN_POINT('Ctrl Pts',(6.7710806444101,7.7019262715247,27.6719835892955));
#111721=CARTESIAN_POINT('Ctrl Pts',(7.11445385898466,7.6306983380045,28.6953692224212));
#111722=CARTESIAN_POINT('Ctrl Pts',(6.44344539503938,7.55947040448434,29.5409287764079));
#111723=CARTESIAN_POINT('Ctrl Pts',(5.37440697636399,7.48861340240428,29.4395602215249));
#111724=CARTESIAN_POINT('Ctrl Pts',(5.04062766770599,7.44149904483097,28.8112190041108));
#111725=CARTESIAN_POINT('Ctrl Pts',(5.04020384857308,7.41812733176437,28.4999090719931));
#111726=CARTESIAN_POINT('Origin',(6.,12.2318726682356,28.5));
#111727=CARTESIAN_POINT('',(5.04021395554822,8.40687266823562,28.5001267151889));
#111728=CARTESIAN_POINT('',(5.04273619519586,8.31812733176437,28.5006805243453));
#111729=CARTESIAN_POINT('',(5.04175,12.2318726682356,28.4999999999999));
#111730=CARTESIAN_POINT('Ctrl Pts',(5.04021395554822,8.40687266823562,28.5001267151889));
#111731=CARTESIAN_POINT('Ctrl Pts',(5.04079193445267,8.38364806503449,28.1907674277398));
#111732=CARTESIAN_POINT('Ctrl Pts',(5.37084730702173,8.33668081732663,27.564088380757));
#111733=CARTESIAN_POINT('Ctrl Pts',(6.43702271497452,8.26597092511206,27.4563583663045));
#111734=CARTESIAN_POINT('Ctrl Pts',(7.11322889506391,8.19474299159188,28.2977671139973));
#111735=CARTESIAN_POINT('Ctrl Pts',(6.77616836554943,8.1235150580717,29.3232492826038));
#111736=CARTESIAN_POINT('Ctrl Pts',(5.73263536721262,8.05228712455152,29.5994056876876));
#111737=CARTESIAN_POINT('Ctrl Pts',(5.10861382433492,7.99673966127282,29.0343785992878));
#111738=CARTESIAN_POINT('Ctrl Pts',(5.04192084102608,7.96493484250086,28.6088128634222));
#111739=CARTESIAN_POINT('Ctrl Pts',(5.04266942812141,7.95687266823562,28.5007094137961));
#111740=CARTESIAN_POINT('Ctrl Pts',(5.04273619519585,8.31812733176437,28.5006805243453));
#111741=CARTESIAN_POINT('Ctrl Pts',(5.04410682382072,8.30266813440496,28.2933560883282));
#111742=CARTESIAN_POINT('Ctrl Pts',(5.21191596650108,8.26346629253882,27.7655957456847));
#111743=CARTESIAN_POINT('Ctrl Pts',(6.08058882997138,8.20052180616596,27.3714248022129));
#111744=CARTESIAN_POINT('Ctrl Pts',(6.99022601937189,8.12929387264577,27.9526162524013));
#111745=CARTESIAN_POINT('Ctrl Pts',(6.99855435409013,8.0580659391256,29.032039226478));
#111746=CARTESIAN_POINT('Ctrl Pts',(6.09799334069262,7.98683800560541,29.62719733931));
#111747=CARTESIAN_POINT('Ctrl Pts',(5.21822287040342,7.92352513648501,29.2442489249259));
#111748=CARTESIAN_POINT('Ctrl Pts',(5.04413523770993,7.88395491187133,28.7114745064653));
#111749=CARTESIAN_POINT('Ctrl Pts',(5.04262349743768,7.86812733176438,28.4992726076031));
#111750=CARTESIAN_POINT('Origin',(6.,12.2318726682356,28.5));
#111751=CARTESIAN_POINT('',(5.04232064019591,8.85687266823562,28.4991864750727));
#111752=CARTESIAN_POINT('',(5.04023521160163,8.76812733176438,28.5001800208846));
#111753=CARTESIAN_POINT('',(5.04175,12.2318726682356,28.4999999999999));
#111754=CARTESIAN_POINT('Ctrl Pts',(5.04232064019591,8.85687266823562,28.4991864750727));
#111755=CARTESIAN_POINT('Ctrl Pts',(5.04155303324115,8.84984657658158,28.4050622393142));
#111756=CARTESIAN_POINT('Ctrl Pts',(5.09743993967769,8.81907784042081,27.9937639308669));
#111757=CARTESIAN_POINT('Ctrl Pts',(5.68518862833307,8.76456645975332,27.4132293189198));
#111758=CARTESIAN_POINT('Ctrl Pts',(6.73972027305326,8.69333852623316,27.6438512800801));
#111759=CARTESIAN_POINT('Ctrl Pts',(7.12095469163445,8.62211059271294,28.6537442431088));
#111760=CARTESIAN_POINT('Ctrl Pts',(6.48189034053387,8.5508826591928,29.5236983992791));
#111761=CARTESIAN_POINT('Ctrl Pts',(5.40420690407899,8.47965472567259,29.4618769671009));
#111762=CARTESIAN_POINT('Ctrl Pts',(5.04338669711544,8.43165139535355,28.8301752268289));
#111763=CARTESIAN_POINT('Ctrl Pts',(5.04020106331735,8.40739070954122,28.5070271942964));
#111764=CARTESIAN_POINT('Ctrl Pts',(5.04021395554822,8.40687266823562,28.5001267151889));
#111765=CARTESIAN_POINT('Ctrl Pts',(5.04023521160163,8.76812733176438,28.5001800208846));
#111766=CARTESIAN_POINT('Ctrl Pts',(5.04103064105211,8.74512400144532,28.1937500051567));
#111767=CARTESIAN_POINT('Ctrl Pts',(5.36553297683283,8.69837802661954,27.5695919335309));
#111768=CARTESIAN_POINT('Ctrl Pts',(6.42733089615622,8.62788940728704,27.4523527111821));
#111769=CARTESIAN_POINT('Ctrl Pts',(7.1113066008254,8.55666147376686,28.2874578264456));
#111770=CARTESIAN_POINT('Ctrl Pts',(6.78376527806854,8.48543354024668,29.3160199295799));
#111771=CARTESIAN_POINT('Ctrl Pts',(5.7428367373441,8.41420560672649,29.601836463781));
#111772=CARTESIAN_POINT('Ctrl Pts',(5.11109853529383,8.35843687056573,29.040389798058));
#111773=CARTESIAN_POINT('Ctrl Pts',(5.04200177609836,8.32641077891169,28.6117704450034));
#111774=CARTESIAN_POINT('Ctrl Pts',(5.04273619519585,8.31812733176437,28.5006805243453));
#111775=CARTESIAN_POINT('Origin',(6.,12.2318726682356,28.5));
#111776=CARTESIAN_POINT('',(5.04297099545381,9.30687266823563,28.5005441005051));
#111777=CARTESIAN_POINT('',(5.04223964716892,9.21812733176437,28.4991714298536));
#111778=CARTESIAN_POINT('',(5.04175,12.2318726682356,28.4999999999999));
#111779=CARTESIAN_POINT('Ctrl Pts',(5.04297099545381,9.30687266823563,28.5005441005051));
#111780=CARTESIAN_POINT('Ctrl Pts',(5.0439879065076,9.29230244362195,28.3050212100339));
#111781=CARTESIAN_POINT('Ctrl Pts',(5.19717400985829,9.25398957450154,27.7894242676125));
#111782=CARTESIAN_POINT('Ctrl Pts',(6.03851769375916,9.19193406087441,27.3692068711474));
#111783=CARTESIAN_POINT('Ctrl Pts',(6.96916130750066,9.12070612735422,27.9161309453062));
#111784=CARTESIAN_POINT('Ctrl Pts',(7.01766927646803,9.04947819383405,28.9944956589479));
#111785=CARTESIAN_POINT('Ctrl Pts',(6.13988939591615,8.97825026031386,29.6227678610904));
#111786=CARTESIAN_POINT('Ctrl Pts',(5.23392768359053,8.91404841844773,29.2679241592235));
#111787=CARTESIAN_POINT('Ctrl Pts',(5.04414693892089,8.87358922108831,28.7231278694141));
#111788=CARTESIAN_POINT('Ctrl Pts',(5.04232064019591,8.85687266823562,28.4991864750727));
#111789=CARTESIAN_POINT('Ctrl Pts',(5.04223964716892,9.21812733176438,28.4991714298536));
#111790=CARTESIAN_POINT('Ctrl Pts',(5.04147759709558,9.21132251299241,28.4080310177188));
#111791=CARTESIAN_POINT('Ctrl Pts',(5.09515055781774,9.18077504971372,27.9997725890198));
#111792=CARTESIAN_POINT('Ctrl Pts',(5.6751294127762,9.1264849419283,27.416193911193));
#111793=CARTESIAN_POINT('Ctrl Pts',(6.73175321387293,9.05525700840812,27.6370319991079));
#111794=CARTESIAN_POINT('Ctrl Pts',(7.1223314473857,8.98402907488794,28.6433480337722));
#111795=CARTESIAN_POINT('Ctrl Pts',(6.49135778099696,8.91280114136776,29.5191879451952));
#111796=CARTESIAN_POINT('Ctrl Pts',(5.41314771587932,8.84157320784758,29.4673577069521));
#111797=CARTESIAN_POINT('Ctrl Pts',(5.044797960694,8.79334860464645,28.8361311061575));
#111798=CARTESIAN_POINT('Ctrl Pts',(5.04020964694338,8.76886664595205,28.5100285104301));
#111799=CARTESIAN_POINT('Ctrl Pts',(5.04023521160163,8.76812733176438,28.5001800208846));
#111800=CARTESIAN_POINT('Origin',(6.,12.2318726682356,28.5));
#111801=CARTESIAN_POINT('',(5.04038444040905,9.75687266823562,28.5003835829357));
#111802=CARTESIAN_POINT('',(5.0430205615309,9.66812733176438,28.500505644125));
#111803=CARTESIAN_POINT('',(5.04175,12.2318726682356,28.4999999999999));
#111804=CARTESIAN_POINT('Ctrl Pts',(5.04038444040905,9.75687266823562,28.5003835829357));
#111805=CARTESIAN_POINT('Ctrl Pts',(5.04188850652928,9.73475831066231,28.2056733548791));
#111806=CARTESIAN_POINT('Ctrl Pts',(5.34466159125839,9.68890130858227,27.5918810980426));
#111807=CARTESIAN_POINT('Ctrl Pts',(6.38803224649353,9.61930166199549,27.4371699623346));
#111808=CARTESIAN_POINT('Ctrl Pts',(7.10262364459654,9.54807372847531,28.2462327614415));
#111809=CARTESIAN_POINT('Ctrl Pts',(6.8136012869641,9.47684579495514,29.286275815956));
#111810=CARTESIAN_POINT('Ctrl Pts',(5.78403482147721,9.40561786143493,29.6106465480502));
#111811=CARTESIAN_POINT('Ctrl Pts',(5.12143631245245,9.34896015252845,29.0645392296898));
#111812=CARTESIAN_POINT('Ctrl Pts',(5.04233081759613,9.31604508812868,28.6236319799069));
#111813=CARTESIAN_POINT('Ctrl Pts',(5.04297099545381,9.30687266823563,28.5005441005051));
#111814=CARTESIAN_POINT('Ctrl Pts',(5.0430205615309,9.66812733176438,28.500505644125));
#111815=CARTESIAN_POINT('Ctrl Pts',(5.04394831887074,9.65377838003277,28.3079271288657));
#111816=CARTESIAN_POINT('Ctrl Pts',(5.193608544855,9.61568678379445,27.7953697292877));
#111817=CARTESIAN_POINT('Ctrl Pts',(6.02803525397329,9.55385254304938,27.3688985186306));
#111818=CARTESIAN_POINT('Ctrl Pts',(6.96370800764262,9.48262460952921,27.9071733705549));
#111819=CARTESIAN_POINT('Ctrl Pts',(7.0222087383162,9.41139667600901,28.9850420928927));
#111820=CARTESIAN_POINT('Ctrl Pts',(6.1502897777778,9.34016874248886,29.6214229885637));
#111821=CARTESIAN_POINT('Ctrl Pts',(5.23794454979289,9.27574562774062,29.2737974975242));
#111822=CARTESIAN_POINT('Ctrl Pts',(5.04413646055601,9.23506515749913,28.7260283778292));
#111823=CARTESIAN_POINT('Ctrl Pts',(5.04223964716892,9.21812733176438,28.4991714298536));
#111824=CARTESIAN_POINT('Origin',(6.,12.2318726682356,28.5));
#111825=CARTESIAN_POINT('',(5.04189765845147,10.2068726682356,28.4991386725514));
#111826=CARTESIAN_POINT('',(5.04043577631992,10.1181273317644,28.5004306020855));
#111827=CARTESIAN_POINT('',(5.04175,12.2318726682356,28.4999999999999));
#111828=CARTESIAN_POINT('Ctrl Pts',(5.04189765845147,10.2068726682356,28.4991386725514));
#111829=CARTESIAN_POINT('Ctrl Pts',(5.04118853070869,10.2009568222094,28.4199766509929));
#111830=CARTESIAN_POINT('Ctrl Pts',(5.08628951303429,10.1712983316764,28.0239028501118));
#111831=CARTESIAN_POINT('Ctrl Pts',(5.63500601835172,10.1178971966368,27.4290396512902));
#111832=CARTESIAN_POINT('Ctrl Pts',(6.69911890163688,10.0466692631166,27.6103880135778));
#111833=CARTESIAN_POINT('Ctrl Pts',(7.12689014474107,9.97544132959639,28.6014658460497));
#111834=CARTESIAN_POINT('Ctrl Pts',(6.52896013424947,9.9042133960762,29.5001889243431));
#111835=CARTESIAN_POINT('Ctrl Pts',(5.44956787014175,9.83298546255604,29.4885348680441));
#111836=CARTESIAN_POINT('Ctrl Pts',(5.05075510596856,9.78387188660917,28.8600837677074));
#111837=CARTESIAN_POINT('Ctrl Pts',(5.04027369555913,9.75850095516903,28.5220831874526));
#111838=CARTESIAN_POINT('Ctrl Pts',(5.04038444040905,9.75687266823562,28.5003835829357));
#111839=CARTESIAN_POINT('Ctrl Pts',(5.04043577631992,10.1181273317644,28.5004306020855));
#111840=CARTESIAN_POINT('Ctrl Pts',(5.04207772203641,10.0962342470731,28.2086278628711));
#111841=CARTESIAN_POINT('Ctrl Pts',(5.33958527277428,10.0505985178752,27.5974716038793));
#111842=CARTESIAN_POINT('Ctrl Pts',(6.37816468677541,9.98122014417046,27.4336192011314));
#111843=CARTESIAN_POINT('Ctrl Pts',(7.10022415948525,9.90999221065029,28.2360239865173));
#111844=CARTESIAN_POINT('Ctrl Pts',(6.82085389946722,9.83876427713011,29.2787011054732));
#111845=CARTESIAN_POINT('Ctrl Pts',(5.79433816650613,9.76753634360992,29.6126004436091));
#111846=CARTESIAN_POINT('Ctrl Pts',(5.12409916514403,9.71065736182135,29.070549220604));
#111847=CARTESIAN_POINT('Ctrl Pts',(5.04241319539131,9.6775210245395,28.6265792027564));
#111848=CARTESIAN_POINT('Ctrl Pts',(5.0430205615309,9.66812733176438,28.500505644125));
#111849=CARTESIAN_POINT('Origin',(6.,12.2318726682356,28.5));
#111850=CARTESIAN_POINT('',(5.0431799682554,10.6568726682356,28.5003376186496));
#111851=CARTESIAN_POINT('',(5.04180976972011,10.5681273317644,28.4991376522761));
#111852=CARTESIAN_POINT('',(5.04175,12.2318726682356,28.4999999999999));
#111853=CARTESIAN_POINT('Ctrl Pts',(5.0431799682554,10.6568726682356,28.5003376186496));
#111854=CARTESIAN_POINT('Ctrl Pts',(5.04375387351073,10.6434126892498,28.3196143998931));
#111855=CARTESIAN_POINT('Ctrl Pts',(5.1796945030962,10.6062100657572,27.8193040088319));
#111856=CARTESIAN_POINT('Ctrl Pts',(5.98590671384625,10.5452647977578,27.3686397261773));
#111857=CARTESIAN_POINT('Ctrl Pts',(6.94096978992682,10.4740368642377,27.8717063333662));
#111858=CARTESIAN_POINT('Ctrl Pts',(7.03955768450863,10.4028089307175,28.9466507169341));
#111859=CARTESIAN_POINT('Ctrl Pts',(6.19193458290324,10.3315809971973,29.6150504691213));
#111860=CARTESIAN_POINT('Ctrl Pts',(5.25452090191919,10.2662689097034,29.2973065776616));
#111861=CARTESIAN_POINT('Ctrl Pts',(5.04403454256094,10.2246994667161,28.73768534861));
#111862=CARTESIAN_POINT('Ctrl Pts',(5.04189765845147,10.2068726682356,28.4991386725514));
#111863=CARTESIAN_POINT('Ctrl Pts',(5.04180976972011,10.5681273317644,28.4991376522761));
#111864=CARTESIAN_POINT('Ctrl Pts',(5.04112072370537,10.5624327586202,28.4229544109879));
#111865=CARTESIAN_POINT('Ctrl Pts',(5.08416676895765,10.5329955409693,28.0299061204628));
#111866=CARTESIAN_POINT('Ctrl Pts',(5.62509554533696,10.4798156788117,27.4324687801292));
#111867=CARTESIAN_POINT('Ctrl Pts',(6.69084341099689,10.4085877452916,27.6039464366949));
#111868=CARTESIAN_POINT('Ctrl Pts',(7.12778211347718,10.3373598117714,28.5910168988298));
#111869=CARTESIAN_POINT('Ctrl Pts',(6.53820764542198,10.2661318782512,29.4952432009378));
#111870=CARTESIAN_POINT('Ctrl Pts',(5.45875381291119,10.194903944731,29.4935940386394));
#111871=CARTESIAN_POINT('Ctrl Pts',(5.05231044100045,10.1455690959021,28.8660517697691));
#111872=CARTESIAN_POINT('Ctrl Pts',(5.04029706234429,10.1199768915799,28.5250825242843));
#111873=CARTESIAN_POINT('Ctrl Pts',(5.04043577631992,10.1181273317644,28.5004306020855));
#111874=CARTESIAN_POINT('Origin',(6.,12.2318726682356,28.5));
#111875=CARTESIAN_POINT('',(5.04070147463229,11.1068726682356,28.5006572399252));
#111876=CARTESIAN_POINT('',(5.04321154726233,11.0181273317644,28.5002974317561));
#111877=CARTESIAN_POINT('',(5.04175,12.2318726682356,28.4999999999999));
#111878=CARTESIAN_POINT('Ctrl Pts',(5.04070147463229,11.1068726682356,28.5006572399252));
#111879=CARTESIAN_POINT('Ctrl Pts',(5.04276136934609,11.0858685562901,28.2205231486132));
#111880=CARTESIAN_POINT('Ctrl Pts',(5.31964162539148,11.0411217998379,27.6200006105552));
#111881=CARTESIAN_POINT('Ctrl Pts',(6.3382146275518,10.9726323988789,27.4203285596915));
#111882=CARTESIAN_POINT('Ctrl Pts',(7.08962794991972,10.9014044653588,28.1952221424384));
#111883=CARTESIAN_POINT('Ctrl Pts',(6.84927801671883,10.8301765318385,29.2476149421817));
#111884=CARTESIAN_POINT('Ctrl Pts',(5.83589966612663,10.7589485983184,29.6194791497386));
#111885=CARTESIAN_POINT('Ctrl Pts',(5.13516398712787,10.7011806437841,29.0946878303018));
#111886=CARTESIAN_POINT('Ctrl Pts',(5.04274153697795,10.6671553337565,28.6383999746367));
#111887=CARTESIAN_POINT('Ctrl Pts',(5.0431799682554,10.6568726682356,28.5003376186496));
#111888=CARTESIAN_POINT('Ctrl Pts',(5.04321154726233,11.0181273317644,28.5002974317561));
#111889=CARTESIAN_POINT('Ctrl Pts',(5.04369879534293,11.0048886256606,28.3225293158624));
#111890=CARTESIAN_POINT('Ctrl Pts',(5.17632882931575,10.9679072750501,27.8252649356805));
#111891=CARTESIAN_POINT('Ctrl Pts',(5.97542374450792,10.9071832799328,27.3688243783781));
#111892=CARTESIAN_POINT('Ctrl Pts',(6.93510468754786,10.8359553464126,27.8630092146581));
#111893=CARTESIAN_POINT('Ctrl Pts',(7.04365340207539,10.7647274128925,28.9369977474397));
#111894=CARTESIAN_POINT('Ctrl Pts',(6.20226086341658,10.6934994793723,29.6132228219541));
#111895=CARTESIAN_POINT('Ctrl Pts',(5.25875722564617,10.6279661189962,29.30313503794));
#111896=CARTESIAN_POINT('Ctrl Pts',(5.04399359479906,10.5861754031269,28.7405886865493));
#111897=CARTESIAN_POINT('Ctrl Pts',(5.04180976972011,10.5681273317644,28.4991376522761));
#111898=CARTESIAN_POINT('Origin',(6.,5.85,28.5));
#111899=CARTESIAN_POINT('',(4.78808807722243,5.85,28.4134292692097));
#111900=CARTESIAN_POINT('Ctrl Pts',(6.39766230306601,5.85,29.3734910038904));
#111901=CARTESIAN_POINT('Ctrl Pts',(6.37560479125928,5.85,29.3873944122752));
#111902=CARTESIAN_POINT('Ctrl Pts',(6.35299337898576,5.85,29.4003106730031));
#111903=CARTESIAN_POINT('Ctrl Pts',(6.32987567746936,5.85,29.41218723318));
#111904=CARTESIAN_POINT('Ctrl Pts',(6.29181373748265,5.85,29.4317412931018));
#111905=CARTESIAN_POINT('Ctrl Pts',(6.25238143582705,5.85,29.4484799626506));
#111906=CARTESIAN_POINT('Ctrl Pts',(6.21188608599289,5.85,29.4624912035614));
#111907=CARTESIAN_POINT('Ctrl Pts',(6.1972630931679,5.85,29.4675507048657));
#111908=CARTESIAN_POINT('Ctrl Pts',(6.18250111093423,5.85,29.4722541335282));
#111909=CARTESIAN_POINT('Ctrl Pts',(6.16761349718974,5.85,29.4766041506807));
#111910=CARTESIAN_POINT('Ctrl Pts',(6.1588421883919,5.85,29.4791670425165));
#111911=CARTESIAN_POINT('Ctrl Pts',(6.15002899407694,5.85,29.481606645163));
#111912=CARTESIAN_POINT('Ctrl Pts',(6.14118581535311,5.85,29.4839213855223));
#111913=CARTESIAN_POINT('Ctrl Pts',(6.09925348827685,5.85,29.4948973538789));
#111914=CARTESIAN_POINT('Ctrl Pts',(6.05659373646623,5.85,29.5030859829525));
#111915=CARTESIAN_POINT('Ctrl Pts',(6.01351014174746,5.85,29.5085736858683));
#111916=CARTESIAN_POINT('Ctrl Pts',(5.98459026202491,5.85,29.5122573085862));
#111917=CARTESIAN_POINT('Ctrl Pts',(5.95547858940136,5.85,29.5147230779385));
#111918=CARTESIAN_POINT('Ctrl Pts',(5.92626036763772,5.85,29.5159859100061));
#111919=CARTESIAN_POINT('Ctrl Pts',(5.91602556356871,5.85,29.5164282654269));
#111920=CARTESIAN_POINT('Ctrl Pts',(5.90577765162887,5.85,29.5167229354698));
#111921=CARTESIAN_POINT('Ctrl Pts',(5.89552020384814,5.85,29.5168702916139));
#111922=CARTESIAN_POINT('Ctrl Pts',(5.88632379011673,5.85,29.517002405186));
#111923=CARTESIAN_POINT('Ctrl Pts',(5.87712958144482,5.85,29.5170159601235));
#111924=CARTESIAN_POINT('Ctrl Pts',(5.86794035624245,5.85,29.5169118945272));
#111925=CARTESIAN_POINT('Ctrl Pts',(5.82159506309469,5.85,29.5163870460814));
#111926=CARTESIAN_POINT('Ctrl Pts',(5.77537862895158,5.85,29.5128744891163));
#111927=CARTESIAN_POINT('Ctrl Pts',(5.72962637037788,5.85,29.506463984083));
#111928=CARTESIAN_POINT('Ctrl Pts',(5.68423642305929,5.85,29.5001042437157));
#111929=CARTESIAN_POINT('Ctrl Pts',(5.63930198692769,5.85,29.4908923183959));
#111930=CARTESIAN_POINT('Ctrl Pts',(5.5951346086702,5.85,29.4788648298534));
#111931=CARTESIAN_POINT('Ctrl Pts',(5.57278650518548,5.85,29.4727790812939));
#111932=CARTESIAN_POINT('Ctrl Pts',(5.55063465678426,5.85,29.4659716680212));
#111933=CARTESIAN_POINT('Ctrl Pts',(5.52871953745136,5.85,29.4584422336643));
#111934=CARTESIAN_POINT('Ctrl Pts',(5.51918689020667,5.85,29.4551670773402));
#111935=CARTESIAN_POINT('Ctrl Pts',(5.50969904152047,5.85,29.4517552645103));
#111936=CARTESIAN_POINT('Ctrl Pts',(5.50025937223982,5.85,29.4482065595265));
#111937=CARTESIAN_POINT('Ctrl Pts',(5.4913953109182,5.85,29.4448742458985));
#111938=CARTESIAN_POINT('Ctrl Pts',(5.48258062850377,5.85,29.4414237433841));
#111939=CARTESIAN_POINT('Ctrl Pts',(5.47382484858967,5.85,29.4378583479916));
#111940=CARTESIAN_POINT('Ctrl Pts',(5.43006407079472,5.85,29.4200387503027));
#111941=CARTESIAN_POINT('Ctrl Pts',(5.38772146838542,5.85,29.3993333169208));
#111942=CARTESIAN_POINT('Ctrl Pts',(5.34712310967584,5.85,29.3758018262265));
#111943=CARTESIAN_POINT('Ctrl Pts',(5.34483356399201,5.85,29.3744747670876));
#111944=CARTESIAN_POINT('Ctrl Pts',(5.3425495652097,5.85,29.3731387061964));
#111945=CARTESIAN_POINT('Ctrl Pts',(5.34027117186927,5.85,29.3717936493299));
#111946=CARTESIAN_POINT('Ctrl Pts',(5.30129849569172,5.85,29.3487860040878));
#111947=CARTESIAN_POINT('Ctrl Pts',(5.26396449537708,5.85,29.3231503642922));
#111948=CARTESIAN_POINT('Ctrl Pts',(5.22835390321961,5.85,29.2951545084538));
#111949=CARTESIAN_POINT('Ctrl Pts',(5.21129296197096,5.85,29.281741767392));
#111950=CARTESIAN_POINT('Ctrl Pts',(5.19462785867648,5.85,29.2677865410265));
#111951=CARTESIAN_POINT('Ctrl Pts',(5.17836963742877,5.85,29.2533145725815));
#111952=CARTESIAN_POINT('Ctrl Pts',(5.16945924558658,5.85,29.2453831446837));
#111953=CARTESIAN_POINT('Ctrl Pts',(5.1606710885947,5.85,29.2372964671565));
#111954=CARTESIAN_POINT('Ctrl Pts',(5.15200716210713,5.85,29.2290585117669));
#111955=CARTESIAN_POINT('Ctrl Pts',(5.14507713634318,5.85,29.2224692080402));
#111956=CARTESIAN_POINT('Ctrl Pts',(5.13822590803877,5.85,29.2157822542096));
#111957=CARTESIAN_POINT('Ctrl Pts',(5.13146656977552,5.85,29.2090121450337));
#111958=CARTESIAN_POINT('Ctrl Pts',(5.0979881630321,5.85,29.1754803909094));
#111959=CARTESIAN_POINT('Ctrl Pts',(5.06669143674257,5.85,29.1398468622296));
#111960=CARTESIAN_POINT('Ctrl Pts',(5.03765905964773,5.85,29.1024199304065));
#111961=CARTESIAN_POINT('Ctrl Pts',(5.00796455502298,5.85,29.0641394204614));
#111962=CARTESIAN_POINT('Ctrl Pts',(4.98063808722797,5.85,29.0239820965496));
#111963=CARTESIAN_POINT('Ctrl Pts',(4.9557940804241,5.85,28.9822296267095));
#111964=CARTESIAN_POINT('Ctrl Pts',(4.94304363266272,5.85,28.960801413064));
#111965=CARTESIAN_POINT('Ctrl Pts',(4.93094754092183,5.85,28.9389523366623));
#111966=CARTESIAN_POINT('Ctrl Pts',(4.91952488154216,5.85,28.9167166416882));
#111967=CARTESIAN_POINT('Ctrl Pts',(4.91126860137239,5.85,28.9006447164584));
#111968=CARTESIAN_POINT('Ctrl Pts',(4.90336419933965,5.85,28.8843707542884));
#111969=CARTESIAN_POINT('Ctrl Pts',(4.89581982809443,5.85,28.8679070326234));
#111970=CARTESIAN_POINT('Ctrl Pts',(4.89200657492442,5.85,28.8595855520403));
#111971=CARTESIAN_POINT('Ctrl Pts',(4.88828572317409,5.85,28.8512162354605));
#111972=CARTESIAN_POINT('Ctrl Pts',(4.88466340885467,5.85,28.8428131220479));
#111973=CARTESIAN_POINT('Ctrl Pts',(4.86467997843789,5.85,28.7964551814171));
#111974=CARTESIAN_POINT('Ctrl Pts',(4.84764801395987,5.85,28.7489758153047));
#111975=CARTESIAN_POINT('Ctrl Pts',(4.83367739160128,5.85,28.7006828495529));
#111976=CARTESIAN_POINT('Ctrl Pts',(4.81980755282921,5.85,28.6527382675857));
#111977=CARTESIAN_POINT('Ctrl Pts',(4.80895438505048,5.85,28.603990769008));
#111978=CARTESIAN_POINT('Ctrl Pts',(4.80126408485538,5.85,28.554709425276));
#111979=CARTESIAN_POINT('Ctrl Pts',(4.79397897921633,5.85,28.5080246683726));
#111980=CARTESIAN_POINT('Ctrl Pts',(4.78953199468363,5.85,28.4608598822724));
#111981=CARTESIAN_POINT('Ctrl Pts',(4.78808807722243,5.85,28.4134292692097));
#111982=CARTESIAN_POINT('',(4.785,5.85,28.5));
#111983=CARTESIAN_POINT('Origin',(6.,5.85,28.5));
#111984=CARTESIAN_POINT('',(5.31875076891147,5.85,27.492807053794));
#111985=CARTESIAN_POINT('Origin',(6.,5.85,28.5));
#111986=CARTESIAN_POINT('Ctrl Pts',(5.31842995130037,5.85,27.4918752544675));
#111987=CARTESIAN_POINT('Ctrl Pts',(5.34708224593995,5.85,27.4762949324899));
#111988=CARTESIAN_POINT('Ctrl Pts',(5.37635092494107,5.85,27.461973165142));
#111989=CARTESIAN_POINT('Ctrl Pts',(5.40619692851071,5.85,27.4489852785675));
#111990=CARTESIAN_POINT('Ctrl Pts',(5.44976279004565,5.85,27.4300270127878));
#111991=CARTESIAN_POINT('Ctrl Pts',(5.49455904383828,5.85,27.4139090963492));
#111992=CARTESIAN_POINT('Ctrl Pts',(5.54030432571948,5.85,27.4006115881595));
#111993=CARTESIAN_POINT('Ctrl Pts',(5.55672681328631,5.85,27.3958378026688));
#111994=CARTESIAN_POINT('Ctrl Pts',(5.57327162018282,5.85,27.3914278984493));
#111995=CARTESIAN_POINT('Ctrl Pts',(5.58992562620212,5.85,27.3873822307481));
#111996=CARTESIAN_POINT('Ctrl Pts',(5.60099327874898,5.85,27.384693625713));
#111997=CARTESIAN_POINT('Ctrl Pts',(5.61211166023121,5.85,27.3821653739662));
#111998=CARTESIAN_POINT('Ctrl Pts',(5.62326865569075,5.85,27.3797994609335));
#111999=CARTESIAN_POINT('Ctrl Pts',(5.67204924285268,5.85,27.369455221991));
#112000=CARTESIAN_POINT('Ctrl Pts',(5.72146861995573,5.85,27.362229542462));
#112001=CARTESIAN_POINT('Ctrl Pts',(5.7711989464513,5.85,27.3580931321149));
#112002=CARTESIAN_POINT('Ctrl Pts',(5.80313722508088,5.85,27.3554366077061));
#112003=CARTESIAN_POINT('Ctrl Pts',(5.8352038278478,5.85,27.3540553674492));
#112004=CARTESIAN_POINT('Ctrl Pts',(5.86730952534731,5.85,27.3539527284191));
#112005=CARTESIAN_POINT('Ctrl Pts',(5.88111738432143,5.85,27.3539085859347));
#112006=CARTESIAN_POINT('Ctrl Pts',(5.8949324342615,5.85,27.3541010447302));
#112007=CARTESIAN_POINT('Ctrl Pts',(5.9087473532397,5.85,27.354530837349));
#112008=CARTESIAN_POINT('Ctrl Pts',(5.92273505299603,5.85,27.354966005309));
#112009=CARTESIAN_POINT('Ctrl Pts',(5.93672831021879,5.85,27.3556450340852));
#112010=CARTESIAN_POINT('Ctrl Pts',(5.95068702636896,5.85,27.3565663028577));
#112011=CARTESIAN_POINT('Ctrl Pts',(5.99984799299835,5.85,27.3598109037862));
#112012=CARTESIAN_POINT('Ctrl Pts',(6.04864581675033,5.85,27.3660555953942));
#112013=CARTESIAN_POINT('Ctrl Pts',(6.09676290916412,5.85,27.375282453497));
#112014=CARTESIAN_POINT('Ctrl Pts',(6.1428988501221,5.85,27.3841294091069));
#112015=CARTESIAN_POINT('Ctrl Pts',(6.18840989818999,5.85,27.3957185910204));
#112016=CARTESIAN_POINT('Ctrl Pts',(6.23299382807648,5.85,27.4100776452759));
#112017=CARTESIAN_POINT('Ctrl Pts',(6.2567216722242,5.85,27.4177196230546));
#112018=CARTESIAN_POINT('Ctrl Pts',(6.28018645016525,5.85,27.4261468450586));
#112019=CARTESIAN_POINT('Ctrl Pts',(6.30333855317582,5.85,27.4353680192718));
#112020=CARTESIAN_POINT('Ctrl Pts',(6.31558983623641,5.85,27.4402475421119));
#112021=CARTESIAN_POINT('Ctrl Pts',(6.32775351143813,5.85,27.4453494353354));
#112022=CARTESIAN_POINT('Ctrl Pts',(6.33982182839314,5.85,27.4506753268719));
#112023=CARTESIAN_POINT('Ctrl Pts',(6.34965281523833,5.85,27.4550138580714));
#112024=CARTESIAN_POINT('Ctrl Pts',(6.35942225137347,5.85,27.4595020494353));
#112025=CARTESIAN_POINT('Ctrl Pts',(6.36910587695464,5.85,27.4641308184335));
#112026=CARTESIAN_POINT('Ctrl Pts',(6.41003918384822,5.85,27.4836969220953));
#112027=CARTESIAN_POINT('Ctrl Pts',(6.44952349193045,5.85,27.5058062551903));
#112028=CARTESIAN_POINT('Ctrl Pts',(6.48728357592312,5.85,27.5304740913914));
#112029=CARTESIAN_POINT('Ctrl Pts',(6.49179366527091,5.85,27.5334204340242));
#112030=CARTESIAN_POINT('Ctrl Pts',(6.49627911696747,5.85,27.5364033231456));
#112031=CARTESIAN_POINT('Ctrl Pts',(6.50073942778498,5.85,27.5394228222158));
#112032=CARTESIAN_POINT('Ctrl Pts',(6.53921831223448,5.85,27.5654718938107));
#112033=CARTESIAN_POINT('Ctrl Pts',(6.57582986883405,5.85,27.5942433472433));
#112034=CARTESIAN_POINT('Ctrl Pts',(6.61041251906095,5.85,27.6254667472186));
#112035=CARTESIAN_POINT('Ctrl Pts',(6.62591613035989,5.85,27.6394643863086));
#112036=CARTESIAN_POINT('Ctrl Pts',(6.64101135713831,5.85,27.6539551741822));
#112037=CARTESIAN_POINT('Ctrl Pts',(6.65568044111702,5.85,27.6689160312498));
#112038=CARTESIAN_POINT('Ctrl Pts',(6.66377388965348,5.85,27.677170461241));
#112039=CARTESIAN_POINT('Ctrl Pts',(6.67173757874651,5.85,27.6855679955746));
#112040=CARTESIAN_POINT('Ctrl Pts',(6.67956824603633,5.85,27.6941048065658));
#112041=CARTESIAN_POINT('Ctrl Pts',(6.68537015773566,5.85,27.700429915491));
#112042=CARTESIAN_POINT('Ctrl Pts',(6.69109781697112,5.85,27.7068302913327));
#112043=CARTESIAN_POINT('Ctrl Pts',(6.69674235679888,5.85,27.7132951997147));
#112044=CARTESIAN_POINT('Ctrl Pts',(6.72642364311295,5.85,27.7472903175694));
#112045=CARTESIAN_POINT('Ctrl Pts',(6.75387231476421,5.85,27.7831346316721));
#112046=CARTESIAN_POINT('Ctrl Pts',(6.77895793001658,5.85,27.8205659891986));
#112047=CARTESIAN_POINT('Ctrl Pts',(6.80387458551433,5.85,27.8577452343922));
#112048=CARTESIAN_POINT('Ctrl Pts',(6.82646026031466,5.85,27.8964914210295));
#112049=CARTESIAN_POINT('Ctrl Pts',(6.84653849813131,5.85,27.9365623451875));
#112050=CARTESIAN_POINT('Ctrl Pts',(6.85571490799722,5.85,27.9548760651034));
#112051=CARTESIAN_POINT('Ctrl Pts',(6.86436686272691,5.85,27.9734665875714));
#112052=CARTESIAN_POINT('Ctrl Pts',(6.87247380103991,5.85,27.992310794561));
#112053=CARTESIAN_POINT('Ctrl Pts',(6.87709299377136,5.85,28.0030478966082));
#112054=CARTESIAN_POINT('Ctrl Pts',(6.88153520171541,5.85,28.01386735387));
#112055=CARTESIAN_POINT('Ctrl Pts',(6.88579626268239,5.85,28.0247648298098));
#112056=CARTESIAN_POINT('Ctrl Pts',(6.8895914343642,5.85,28.0344708144015));
#112057=CARTESIAN_POINT('Ctrl Pts',(6.89324350585179,5.85,28.0442408696217));
#112058=CARTESIAN_POINT('Ctrl Pts',(6.89674209830408,5.85,28.0540500724342));
#112059=CARTESIAN_POINT('Ctrl Pts',(6.91122096775626,5.85,28.094645302913));
#112060=CARTESIAN_POINT('Ctrl Pts',(6.92310787725967,5.85,28.1359903692491));
#112061=CARTESIAN_POINT('Ctrl Pts',(6.93225669319789,5.85,28.1778617780855));
#112062=CARTESIAN_POINT('Ctrl Pts',(6.94107840482362,5.85,28.218236127795));
#112063=CARTESIAN_POINT('Ctrl Pts',(6.9473542837777,5.85,28.25910076306));
#112064=CARTESIAN_POINT('Ctrl Pts',(6.95090629581674,5.85,28.3002511157192));
#112065=CARTESIAN_POINT('Ctrl Pts',(6.95399736759412,5.85,28.3360614374006));
#112066=CARTESIAN_POINT('Ctrl Pts',(6.95502502661388,5.85,28.3720884051317));
#112067=CARTESIAN_POINT('Ctrl Pts',(6.95384139680377,5.85,28.4081868623593));
#112068=CARTESIAN_POINT('Ctrl Pts',(5.58122226519601,11.5482346816144,29.361898063191));
#112069=CARTESIAN_POINT('Ctrl Pts',(5.29549456253745,11.5244920371077,29.2230691167062));
#112070=CARTESIAN_POINT('Ctrl Pts',(4.87780360901464,11.4770067480943,28.6413286057481));
#112071=CARTESIAN_POINT('Ctrl Pts',(5.27059993461702,11.4057788145741,27.6341247030305));
#112072=CARTESIAN_POINT('Ctrl Pts',(6.32832772845592,11.3345508810539,27.417533671549));
#112073=CARTESIAN_POINT('Ctrl Pts',(7.08668716007769,11.2633229475337,28.1849858242981));
#112074=CARTESIAN_POINT('Ctrl Pts',(6.85620622293074,11.1920950140135,29.2397882902982));
#112075=CARTESIAN_POINT('Ctrl Pts',(5.84626444085431,11.1208670804934,29.6209123918368));
#112076=CARTESIAN_POINT('Ctrl Pts',(4.97632415185831,11.0496391469732,28.9819400693107));
#112077=CARTESIAN_POINT('Ctrl Pts',(5.03810268409804,10.978411213453,27.9042192846039));
#112078=CARTESIAN_POINT('Ctrl Pts',(5.97542374450792,10.9071832799328,27.3688243783781));
#112079=CARTESIAN_POINT('Ctrl Pts',(6.93510468754786,10.8359553464126,27.8630092146581));
#112080=CARTESIAN_POINT('Ctrl Pts',(7.04365340207539,10.7647274128925,28.9369977474397));
#112081=CARTESIAN_POINT('Ctrl Pts',(6.20226086341658,10.6934994793723,29.6132228219541));
#112082=CARTESIAN_POINT('Ctrl Pts',(5.17677073134417,10.6222715458521,29.2761897148703));
#112083=CARTESIAN_POINT('Ctrl Pts',(4.90058748232414,10.5510436123319,28.2326631663733));
#112084=CARTESIAN_POINT('Ctrl Pts',(5.62509554533696,10.4798156788117,27.4324687801292));
#112085=CARTESIAN_POINT('Ctrl Pts',(6.69084341099689,10.4085877452916,27.6039464366949));
#112086=CARTESIAN_POINT('Ctrl Pts',(7.12778211347718,10.3373598117714,28.5910168988298));
#112087=CARTESIAN_POINT('Ctrl Pts',(6.53820764542198,10.2661318782512,29.4952432009378));
#112088=CARTESIAN_POINT('Ctrl Pts',(5.45875381291119,10.194903944731,29.4935940386394));
#112089=CARTESIAN_POINT('Ctrl Pts',(4.87194505274743,10.1236760112108,28.5875704048551));
#112090=CARTESIAN_POINT('Ctrl Pts',(5.31189775796595,10.0524480776906,27.6018397492193));
#112091=CARTESIAN_POINT('Ctrl Pts',(6.37816468677541,9.98122014417046,27.4336192011314));
#112092=CARTESIAN_POINT('Ctrl Pts',(7.10022415948525,9.90999221065029,28.2360239865173));
#112093=CARTESIAN_POINT('Ctrl Pts',(6.82085389946722,9.83876427713011,29.2787011054732));
#112094=CARTESIAN_POINT('Ctrl Pts',(5.79433816650613,9.76753634360992,29.6126004436091));
#112095=CARTESIAN_POINT('Ctrl Pts',(4.95501690001259,9.69630841008975,28.9338050913953));
#112096=CARTESIAN_POINT('Ctrl Pts',(5.06684466687464,9.62508047656957,27.8601580970606));
#112097=CARTESIAN_POINT('Ctrl Pts',(6.02803525397329,9.55385254304938,27.3688985186306));
#112098=CARTESIAN_POINT('Ctrl Pts',(6.96370800764262,9.48262460952921,27.9071733705549));
#112099=CARTESIAN_POINT('Ctrl Pts',(7.0222087383162,9.41139667600901,28.9850420928927));
#112100=CARTESIAN_POINT('Ctrl Pts',(6.1502897777778,9.34016874248886,29.6214229885637));
#112101=CARTESIAN_POINT('Ctrl Pts',(5.14157628262408,9.26894080896865,29.2370788682514));
#112102=CARTESIAN_POINT('Ctrl Pts',(4.91420450381539,9.19771287544849,28.1818417421448));
#112103=CARTESIAN_POINT('Ctrl Pts',(5.6751294127762,9.1264849419283,27.416193911193));
#112104=CARTESIAN_POINT('Ctrl Pts',(6.73175321387293,9.05525700840812,27.6370319991079));
#112105=CARTESIAN_POINT('Ctrl Pts',(7.1223314473857,8.98402907488794,28.6433480337722));
#112106=CARTESIAN_POINT('Ctrl Pts',(6.49135778099696,8.91280114136776,29.5191879451952));
#112107=CARTESIAN_POINT('Ctrl Pts',(5.41314771587932,8.84157320784758,29.4673577069521));
#112108=CARTESIAN_POINT('Ctrl Pts',(4.86909364113474,8.7703452743274,28.5350334705028));
#112109=CARTESIAN_POINT('Ctrl Pts',(5.35439639516002,8.69911734080722,27.5708215876404));
#112110=CARTESIAN_POINT('Ctrl Pts',(6.42733089615622,8.62788940728704,27.4523527111821));
#112111=CARTESIAN_POINT('Ctrl Pts',(7.1113066008254,8.55666147376686,28.2874578264456));
#112112=CARTESIAN_POINT('Ctrl Pts',(6.78376527806854,8.48543354024668,29.3160199295799));
#112113=CARTESIAN_POINT('Ctrl Pts',(5.7428367373441,8.41420560672649,29.601836463781));
#112114=CARTESIAN_POINT('Ctrl Pts',(4.93597953103987,8.34297767320632,28.8847557383731));
#112115=CARTESIAN_POINT('Ctrl Pts',(5.09759926987673,8.27174973968613,27.817468345898));
#112116=CARTESIAN_POINT('Ctrl Pts',(6.08058882997138,8.20052180616596,27.3714248022129));
#112117=CARTESIAN_POINT('Ctrl Pts',(6.99022601937189,8.12929387264577,27.9526162524013));
#112118=CARTESIAN_POINT('Ctrl Pts',(6.99855435409013,8.0580659391256,29.032039226478));
#112119=CARTESIAN_POINT('Ctrl Pts',(6.09799334069262,7.98683800560541,29.62719733931));
#112120=CARTESIAN_POINT('Ctrl Pts',(5.10823828075997,7.91561007208523,29.1963745922073));
#112121=CARTESIAN_POINT('Ctrl Pts',(4.93016935921317,7.84438213856506,28.1317080822838));
#112122=CARTESIAN_POINT('Ctrl Pts',(5.72586583137092,7.77315420504486,27.4022627845939));
#112123=CARTESIAN_POINT('Ctrl Pts',(6.7710806444101,7.7019262715247,27.6719835892955));
#112124=CARTESIAN_POINT('Ctrl Pts',(7.11445385898466,7.6306983380045,28.6953692224212));
#112125=CARTESIAN_POINT('Ctrl Pts',(6.44344539503938,7.55947040448434,29.5409287764079));
#112126=CARTESIAN_POINT('Ctrl Pts',(5.36881063516189,7.48824247096415,29.4390295642441));
#112127=CARTESIAN_POINT('Ctrl Pts',(4.86868770476157,7.41701453744397,28.4824207747026));
#112128=CARTESIAN_POINT('Ctrl Pts',(5.39829109152546,7.34578660392379,27.5418126900042));
#112129=CARTESIAN_POINT('Ctrl Pts',(6.47557303929329,7.27455867040361,27.4733516550811));
#112130=CARTESIAN_POINT('Ctrl Pts',(7.1199859534311,7.20333073688343,28.3393512752155));
#112131=CARTESIAN_POINT('Ctrl Pts',(6.7449818262241,7.13210280336324,29.351574175982));
#112132=CARTESIAN_POINT('Ctrl Pts',(5.69189142314743,7.06087486984307,29.5886898898316));
#112133=CARTESIAN_POINT('Ctrl Pts',(4.91924295928752,6.98964693632289,28.8348743432691));
#112134=CARTESIAN_POINT('Ctrl Pts',(5.13030531893757,6.91841900280271,27.7762545908562));
#112135=CARTESIAN_POINT('Ctrl Pts',(6.13296796501039,6.84719106928253,27.3763913550898));
#112136=CARTESIAN_POINT('Ctrl Pts',(7.01460310250063,6.77596313576235,27.9992431262198));
#112137=CARTESIAN_POINT('Ctrl Pts',(6.97274002584404,6.70473520224217,29.0778852397409));
#112138=CARTESIAN_POINT('Ctrl Pts',(6.04548629726899,6.63350726872199,29.6305354712223));
#112139=CARTESIAN_POINT('Ctrl Pts',(5.07682610678296,6.56227933520181,29.1541620595593));
#112140=CARTESIAN_POINT('Ctrl Pts',(4.94845253496139,6.49105140168163,28.0823755178912));
#112141=CARTESIAN_POINT('Ctrl Pts',(5.77718546973152,6.41982346816144,27.3906962578813));
#112142=CARTESIAN_POINT('Ctrl Pts',(6.80875932531787,6.34859553464126,27.7087435142843));
#112143=CARTESIAN_POINT('Ctrl Pts',(7.10413006383205,6.27736760112109,28.7469332186266));
#112144=CARTESIAN_POINT('Ctrl Pts',(6.39464482398617,6.2061396676009,29.5604863382188));
#112145=CARTESIAN_POINT('Ctrl Pts',(5.32570060970894,6.13491173408073,29.4085390729209));
#112146=CARTESIAN_POINT('Ctrl Pts',(4.87099739489662,6.06368380056054,28.4301031676476));
#112147=CARTESIAN_POINT('Ctrl Pts',(5.44295412205162,5.99245586704036,27.5143710763459));
#112148=CARTESIAN_POINT('Ctrl Pts',(6.52391074184675,5.92122793352018,27.4975948676703));
#112149=CARTESIAN_POINT('Ctrl Pts',(6.92340443678229,5.87374264450673,28.0919790384314));
#112150=CARTESIAN_POINT('Ctrl Pts',(6.95384139680377,5.85,28.4081868623593));
#112151=CARTESIAN_POINT('Ctrl Pts',(5.54382034036397,11.4988231210763,29.4388760013506));
#112152=CARTESIAN_POINT('Ctrl Pts',(5.23257369252493,11.4750804765696,29.2876479481574));
#112153=CARTESIAN_POINT('Ctrl Pts',(4.77757787690384,11.4275951875561,28.6539509623099));
#112154=CARTESIAN_POINT('Ctrl Pts',(5.20545567275527,11.3563672540359,27.5567915497139));
#112155=CARTESIAN_POINT('Ctrl Pts',(6.35765137200092,11.2851393205157,27.3208563153164));
#112156=CARTESIAN_POINT('Ctrl Pts',(7.18374148770617,11.2139113869956,28.1568512422956));
#112157=CARTESIAN_POINT('Ctrl Pts',(6.93267581080359,11.1426834534754,29.3058603464889));
#112158=CARTESIAN_POINT('Ctrl Pts',(5.83253399305515,11.0714555199552,29.7210234472691));
#112159=CARTESIAN_POINT('Ctrl Pts',(4.88489749771086,11.000227586435,29.0249831557688));
#112160=CARTESIAN_POINT('Ctrl Pts',(4.95219360127073,10.9289996529149,27.8510088493737));
#112161=CARTESIAN_POINT('Ctrl Pts',(5.97322878717331,10.8577717193947,27.2677966921962));
#112162=CARTESIAN_POINT('Ctrl Pts',(7.01862086409466,10.7865437858745,27.806118220959));
#112163=CARTESIAN_POINT('Ctrl Pts',(7.13686429379914,10.7153158523543,28.9760269401191));
#112164=CARTESIAN_POINT('Ctrl Pts',(6.22032520872738,10.6440879188341,29.7126471056437));
#112165=CARTESIAN_POINT('Ctrl Pts',(5.1032463849741,10.5728599853139,29.3455128592456));
#112166=CARTESIAN_POINT('Ctrl Pts',(4.80239662610593,10.5016320517938,28.2087867485862));
#112167=CARTESIAN_POINT('Ctrl Pts',(5.59161203590667,10.4304041182736,27.3371253100181));
#112168=CARTESIAN_POINT('Ctrl Pts',(6.7525440965429,10.3591761847534,27.5239179986121));
#112169=CARTESIAN_POINT('Ctrl Pts',(7.22850671827248,10.2879482512332,28.5991458104828));
#112170=CARTESIAN_POINT('Ctrl Pts',(6.58627610805773,10.216720317713,29.5841304752541));
#112171=CARTESIAN_POINT('Ctrl Pts',(5.41041397169542,10.1454923841929,29.5823340227843));
#112172=CARTESIAN_POINT('Ctrl Pts',(4.77119608059086,10.0742644506727,28.595391502845));
#112173=CARTESIAN_POINT('Ctrl Pts',(5.25044189201508,10.0030365171525,27.5216231584244));
#112174=CARTESIAN_POINT('Ctrl Pts',(6.4119393744281,9.93180858363231,27.338378477552));
#112175=CARTESIAN_POINT('Ctrl Pts',(7.19848750514933,9.86058065011214,28.2124477306823));
#112176=CARTESIAN_POINT('Ctrl Pts',(6.89416609659331,9.78935271659197,29.3482485474525));
#112177=CARTESIAN_POINT('Ctrl Pts',(5.77597007336775,9.71812478307177,29.711969141373));
#112178=CARTESIAN_POINT('Ctrl Pts',(4.86168725015721,9.64689684955161,28.9725491412138));
#112179=CARTESIAN_POINT('Ctrl Pts',(4.98350259129244,9.57566891603142,27.8030124640213));
#112180=CARTESIAN_POINT('Ctrl Pts',(6.03053914177487,9.50444098251124,27.2678774540714));
#112181=CARTESIAN_POINT('Ctrl Pts',(7.04977880717729,9.43321304899106,27.8542267709862));
#112182=CARTESIAN_POINT('Ctrl Pts',(7.11350436178351,9.36198511547088,29.028362227635));
#112183=CARTESIAN_POINT('Ctrl Pts',(6.1637124755583,9.2907571819507,29.7215796464692));
#112184=CARTESIAN_POINT('Ctrl Pts',(5.06490864563433,9.21952924843051,29.3029089402312));
#112185=CARTESIAN_POINT('Ctrl Pts',(4.81722981257427,9.14830131491035,28.1534263555184));
#112186=CARTESIAN_POINT('Ctrl Pts',(5.64611453382333,9.07707338139014,27.3193968981306));
#112187=CARTESIAN_POINT('Ctrl Pts',(6.79710764040111,9.00584544786999,27.5599585025503));
#112188=CARTESIAN_POINT('Ctrl Pts',(7.22256924166911,8.93461751434979,28.65615074972));
#112189=CARTESIAN_POINT('Ctrl Pts',(6.53524198319577,8.86338958082962,29.6102137752426));
#112190=CARTESIAN_POINT('Ctrl Pts',(5.36073469772192,8.79216164730942,29.5537544688479));
#112191=CARTESIAN_POINT('Ctrl Pts',(4.76809000337889,8.72093371378926,28.5381623838175));
#112192=CARTESIAN_POINT('Ctrl Pts',(5.29673617234319,8.64970578026907,27.4878346992595));
#112193=CARTESIAN_POINT('Ctrl Pts',(6.46549672191084,8.57847784674889,27.3587851169898));
#112194=CARTESIAN_POINT('Ctrl Pts',(7.21055974275493,8.50724991322871,28.2684752355907));
#112195=CARTESIAN_POINT('Ctrl Pts',(6.85376501200857,8.43602197970853,29.3889003946359));
#112196=CARTESIAN_POINT('Ctrl Pts',(5.71986894268827,8.36479404618835,29.7002438077503));
#112197=CARTESIAN_POINT('Ctrl Pts',(4.84094961351468,8.29356611266817,28.9191190867781));
#112198=CARTESIAN_POINT('Ctrl Pts',(5.01700395290686,8.22233817914799,27.7565100009321));
#112199=CARTESIAN_POINT('Ctrl Pts',(6.0877863887487,8.15111024562781,27.2706293653813));
#112200=CARTESIAN_POINT('Ctrl Pts',(7.07866519859573,8.07988231210763,27.9037282526809));
#112201=CARTESIAN_POINT('Ctrl Pts',(7.08773735449456,8.00865437858745,29.0795567745772));
#112202=CARTESIAN_POINT('Ctrl Pts',(6.10674533311731,7.93742644506727,29.7278697166882));
#112203=CARTESIAN_POINT('Ctrl Pts',(5.02859315634396,7.86619851154709,29.2585692792406));
#112204=CARTESIAN_POINT('Ctrl Pts',(4.83462052295889,7.79497057802691,28.0988151525079));
#112205=CARTESIAN_POINT('Ctrl Pts',(5.70138232922444,7.72374264450673,27.3042215531631));
#112206=CARTESIAN_POINT('Ctrl Pts',(6.83994748690155,7.65251471098655,27.5980316931486));
#112207=CARTESIAN_POINT('Ctrl Pts',(7.213988089194,7.58128677746637,28.7128180607051));
#112208=CARTESIAN_POINT('Ctrl Pts',(6.48305044075688,7.51005884394619,29.6338963260532));
#112209=CARTESIAN_POINT('Ctrl Pts',(5.31243777859274,7.438830910426,29.5228962798262));
#112210=CARTESIAN_POINT('Ctrl Pts',(4.76764781197003,7.36760297690583,28.4808507369271));
#112211=CARTESIAN_POINT('Ctrl Pts',(5.34455119683868,7.29637504338564,27.4562349556476));
#112212=CARTESIAN_POINT('Ctrl Pts',(6.51804747284004,7.22514710986547,27.3816595209623));
#112213=CARTESIAN_POINT('Ctrl Pts',(7.22001426669085,7.15391917634529,28.325003397978));
#112214=CARTESIAN_POINT('Ctrl Pts',(6.81151772808792,7.0826912428251,29.4276300659493));
#112215=CARTESIAN_POINT('Ctrl Pts',(5.66437359477736,7.01146330930493,29.6859230854884));
#112216=CARTESIAN_POINT('Ctrl Pts',(4.82271826315641,6.94023537578474,28.8647826788233));
#112217=CARTESIAN_POINT('Ctrl Pts',(5.05263104835308,6.86900744226457,27.7116153582976));
#112218=CARTESIAN_POINT('Ctrl Pts',(6.14484361507261,6.79777950874438,27.2760394915954));
#112219=CARTESIAN_POINT('Ctrl Pts',(7.10521945055422,6.7265515752242,27.9545194711739));
#112220=CARTESIAN_POINT('Ctrl Pts',(7.05961749401882,6.65532364170402,29.1294973922076));
#112221=CARTESIAN_POINT('Ctrl Pts',(6.04954877464054,6.58409570818384,29.7315059842186));
#112222=CARTESIAN_POINT('Ctrl Pts',(4.9943754947007,6.51286777466365,29.2125866560605));
#112223=CARTESIAN_POINT('Ctrl Pts',(4.85453660778559,6.44163984114349,28.0450765924954));
#112224=CARTESIAN_POINT('Ctrl Pts',(5.75728543298173,6.37041190762328,27.2916219954971));
#112225=CARTESIAN_POINT('Ctrl Pts',(6.88099133045757,6.29918397410313,27.6380747247521));
#112226=CARTESIAN_POINT('Ctrl Pts',(7.20274225407082,6.22795604058293,28.7689873464229));
#112227=CARTESIAN_POINT('Ctrl Pts',(6.42989138753377,6.15672810706276,29.6552006150559));
#112228=CARTESIAN_POINT('Ctrl Pts',(5.26547750562782,6.08550017354258,29.4896826182632));
#112229=CARTESIAN_POINT('Ctrl Pts',(4.77016378541396,6.01427224002239,28.4238605337815));
#112230=CARTESIAN_POINT('Ctrl Pts',(5.39320317704308,5.94304430650222,27.4263424734594));
#112231=CARTESIAN_POINT('Ctrl Pts',(6.57070231779914,5.87181637298204,27.4080679461204));
#112232=CARTESIAN_POINT('Ctrl Pts',(7.00587563919775,5.82433108396858,28.0555378237578));
#112233=CARTESIAN_POINT('Ctrl Pts',(7.03903098846544,5.80058843946186,28.3999868369348));
#112234=CARTESIAN_POINT('Ctrl Pts',(5.50641841553193,11.4494115605381,29.5158539395102));
#112235=CARTESIAN_POINT('Ctrl Pts',(5.1696528225124,11.4256689160314,29.3522267796086));
#112236=CARTESIAN_POINT('Ctrl Pts',(4.67735214479306,11.378183627018,28.6665733188716));
#112237=CARTESIAN_POINT('Ctrl Pts',(5.1403114108935,11.3069556934978,27.4794583963973));
#112238=CARTESIAN_POINT('Ctrl Pts',(6.38697501554594,11.2357277599776,27.2241789590838));
#112239=CARTESIAN_POINT('Ctrl Pts',(7.28079581533463,11.1644998264574,28.1287166602932));
#112240=CARTESIAN_POINT('Ctrl Pts',(7.00914539867645,11.0932718929372,29.3719324026795));
#112241=CARTESIAN_POINT('Ctrl Pts',(5.81880354525599,11.0220439594171,29.8211345027015));
#112242=CARTESIAN_POINT('Ctrl Pts',(4.79347084356342,10.9508160258969,29.0680262422269));
#112243=CARTESIAN_POINT('Ctrl Pts',(4.8662845184434,10.8795880923767,27.7977984141436));
#112244=CARTESIAN_POINT('Ctrl Pts',(5.97103382983874,10.8083601588565,27.1667690060142));
#112245=CARTESIAN_POINT('Ctrl Pts',(7.10213704064145,10.7371322253364,27.7492272272599));
#112246=CARTESIAN_POINT('Ctrl Pts',(7.2300751855229,10.6659042918162,29.0150561327986));
#112247=CARTESIAN_POINT('Ctrl Pts',(6.23838955403818,10.594676358296,29.8120713893333));
#112248=CARTESIAN_POINT('Ctrl Pts',(5.02972203860402,10.5234484247758,29.414836003621));
#112249=CARTESIAN_POINT('Ctrl Pts',(4.70420576988773,10.4522204912556,28.184910330799));
#112250=CARTESIAN_POINT('Ctrl Pts',(5.55812852647635,10.3809925577354,27.2417818399071));
#112251=CARTESIAN_POINT('Ctrl Pts',(6.81424478208894,10.3097646242153,27.4438895605293));
#112252=CARTESIAN_POINT('Ctrl Pts',(7.32923132306776,10.2385366906951,28.6072747221359));
#112253=CARTESIAN_POINT('Ctrl Pts',(6.63434457069349,10.1673087571749,29.6730177495704));
#112254=CARTESIAN_POINT('Ctrl Pts',(5.36207413047964,10.0960808236547,29.6710740069293));
#112255=CARTESIAN_POINT('Ctrl Pts',(4.6704471084343,10.0248528901345,28.6032126008349));
#112256=CARTESIAN_POINT('Ctrl Pts',(5.18898602606421,9.95362495661436,27.4414065676294));
#112257=CARTESIAN_POINT('Ctrl Pts',(6.44571406208079,9.88239702309417,27.2431377539727));
#112258=CARTESIAN_POINT('Ctrl Pts',(7.29675085081342,9.811169089574,28.1888714748473));
#112259=CARTESIAN_POINT('Ctrl Pts',(6.9674782937194,9.73994115605381,29.4177959894319));
#112260=CARTESIAN_POINT('Ctrl Pts',(5.75760198022939,9.66871322253364,29.8113378391368));
#112261=CARTESIAN_POINT('Ctrl Pts',(4.76835760030182,9.59748528901345,29.0112931910323));
#112262=CARTESIAN_POINT('Ctrl Pts',(4.90016051571024,9.52625735549328,27.745866830982));
#112263=CARTESIAN_POINT('Ctrl Pts',(6.03304302957645,9.45502942197309,27.1668563895122));
#112264=CARTESIAN_POINT('Ctrl Pts',(7.13584960671193,9.38380148845291,27.8012801714175));
#112265=CARTESIAN_POINT('Ctrl Pts',(7.20479998525085,9.31257355493274,29.0716823623772));
#112266=CARTESIAN_POINT('Ctrl Pts',(6.17713517333878,9.24134562141255,29.8217363043746));
#112267=CARTESIAN_POINT('Ctrl Pts',(4.98824100864461,9.17011768789238,29.3687390122108));
#112268=CARTESIAN_POINT('Ctrl Pts',(4.72025512133315,9.09888975437219,28.125010968892));
#112269=CARTESIAN_POINT('Ctrl Pts',(5.61709965487048,9.02766182085201,27.2225998850682));
#112270=CARTESIAN_POINT('Ctrl Pts',(6.86246206692927,8.95643388733183,27.4828850059926));
#112271=CARTESIAN_POINT('Ctrl Pts',(7.32280703595254,8.88520595381165,28.6689534656679));
#112272=CARTESIAN_POINT('Ctrl Pts',(6.57912618539456,8.81397802029147,29.7012396052901));
#112273=CARTESIAN_POINT('Ctrl Pts',(5.30832167956453,8.74275008677129,29.6401512307437));
#112274=CARTESIAN_POINT('Ctrl Pts',(4.66708636562304,8.67152215325111,28.5412912971322));
#112275=CARTESIAN_POINT('Ctrl Pts',(5.23907594952635,8.60029421973092,27.4048478108784));
#112276=CARTESIAN_POINT('Ctrl Pts',(6.50366254766546,8.52906628621076,27.2652175227977));
#112277=CARTESIAN_POINT('Ctrl Pts',(7.30981288468446,8.45783835269056,28.2494926447358));
#112278=CARTESIAN_POINT('Ctrl Pts',(6.92376474594862,8.3866104191704,29.4617808596919));
#112279=CARTESIAN_POINT('Ctrl Pts',(5.69690114803242,8.3153824856502,29.7986511517196));
#112280=CARTESIAN_POINT('Ctrl Pts',(4.74591969598952,8.24415455213003,28.9534824351831));
#112281=CARTESIAN_POINT('Ctrl Pts',(4.93640863593697,8.17292661860984,27.6955516559662));
#112282=CARTESIAN_POINT('Ctrl Pts',(6.09498394752603,8.10169868508967,27.1698339285496));
#112283=CARTESIAN_POINT('Ctrl Pts',(7.16710437781957,8.03047075156948,27.8548402529606));
#112284=CARTESIAN_POINT('Ctrl Pts',(7.176920354899,7.95924281804931,29.1270743226765));
#112285=CARTESIAN_POINT('Ctrl Pts',(6.11549732554199,7.88801488452911,29.8285420940663));
#112286=CARTESIAN_POINT('Ctrl Pts',(4.94894803192798,7.81678695100895,29.320763966274));
#112287=CARTESIAN_POINT('Ctrl Pts',(4.73907168670459,7.74555901748876,28.0659222227318));
#112288=CARTESIAN_POINT('Ctrl Pts',(5.67689882707798,7.67433108396858,27.2061803217325));
#112289=CARTESIAN_POINT('Ctrl Pts',(6.908814329393,7.6031031504484,27.5240797970017));
#112290=CARTESIAN_POINT('Ctrl Pts',(7.31352231940335,7.53187521692822,28.730266898989));
#112291=CARTESIAN_POINT('Ctrl Pts',(6.52265548647438,7.46064728340804,29.7268638756984));
#112292=CARTESIAN_POINT('Ctrl Pts',(5.25606492202359,7.38941934988787,29.6067629954084));
#112293=CARTESIAN_POINT('Ctrl Pts',(4.6666079191785,7.31819141636767,28.4792806991516));
#112294=CARTESIAN_POINT('Ctrl Pts',(5.29081130215188,7.24696348284751,27.3706572212911));
#112295=CARTESIAN_POINT('Ctrl Pts',(6.56052190638679,7.17573554932731,27.2899673868435));
#112296=CARTESIAN_POINT('Ctrl Pts',(7.32004257995058,7.10450761580715,28.3106555207405));
#112297=CARTESIAN_POINT('Ctrl Pts',(6.87805362995176,7.03327968228694,29.5036859559166));
#112298=CARTESIAN_POINT('Ctrl Pts',(5.63685576640728,6.96205174876679,29.7831562811451));
#112299=CARTESIAN_POINT('Ctrl Pts',(4.7261935670253,6.89082381524659,28.8946910143775));
#112300=CARTESIAN_POINT('Ctrl Pts',(4.97495677776857,6.81959588172642,27.6469761257391));
#112301=CARTESIAN_POINT('Ctrl Pts',(6.15671926513484,6.74836794820624,27.1756876281009));
#112302=CARTESIAN_POINT('Ctrl Pts',(7.19583579860778,6.67714001468605,27.9097958161281));
#112303=CARTESIAN_POINT('Ctrl Pts',(7.14649496219362,6.60591208116588,29.1811095446742));
#112304=CARTESIAN_POINT('Ctrl Pts',(6.05361125201206,6.53468414764569,29.832476497215));
#112305=CARTESIAN_POINT('Ctrl Pts',(4.91192488261846,6.46345621412551,29.2710112525617));
#112306=CARTESIAN_POINT('Ctrl Pts',(4.76062068060977,6.39222828060534,28.0077776670997));
#112307=CARTESIAN_POINT('Ctrl Pts',(5.73738539623194,6.32100034708514,27.1925477331129));
#112308=CARTESIAN_POINT('Ctrl Pts',(6.95322333559726,6.24977241356498,27.56740593522));
#112309=CARTESIAN_POINT('Ctrl Pts',(7.30135444430958,6.17854448004478,28.7910414742192));
#112310=CARTESIAN_POINT('Ctrl Pts',(6.46513795108138,6.10731654652461,29.7499148918931));
#112311=CARTESIAN_POINT('Ctrl Pts',(5.20525440154669,6.03608861300443,29.5708261636053));
#112312=CARTESIAN_POINT('Ctrl Pts',(4.66933017593129,5.96486067948426,28.4176178999154));
#112313=CARTESIAN_POINT('Ctrl Pts',(5.34345223203455,5.89363274596406,27.3383138705728));
#112314=CARTESIAN_POINT('Ctrl Pts',(6.61749389375153,5.82240481244389,27.3185410245704));
#112315=CARTESIAN_POINT('Ctrl Pts',(7.08834684161321,5.77491952343044,28.0190966090843));
#112316=CARTESIAN_POINT('Ctrl Pts',(7.1242205801271,5.75117687892371,28.3917868115102));
#112317=CARTESIAN_POINT('Ctrl Pts',(5.46901649069989,11.4,29.5928318776698));
#112318=CARTESIAN_POINT('Ctrl Pts',(5.10673195249988,11.3762573554933,29.4168056110598));
#112319=CARTESIAN_POINT('Ctrl Pts',(4.57712641268226,11.3287720664798,28.6791956754334));
#112320=CARTESIAN_POINT('Ctrl Pts',(5.07516714903175,11.2575441329596,27.4021252430807));
#112321=CARTESIAN_POINT('Ctrl Pts',(6.41629865909096,11.1863161994395,27.1275016028511));
#112322=CARTESIAN_POINT('Ctrl Pts',(7.3778501429631,11.1150882659193,28.1005820782907));
#112323=CARTESIAN_POINT('Ctrl Pts',(7.0856149865493,11.0438603323991,29.4380044588702));
#112324=CARTESIAN_POINT('Ctrl Pts',(5.80507309745684,10.9726323988789,29.9212455581337));
#112325=CARTESIAN_POINT('Ctrl Pts',(4.70204418941597,10.9014044653588,29.1110693286851));
#112326=CARTESIAN_POINT('Ctrl Pts',(4.78037543561609,10.8301765318385,27.7445879789133));
#112327=CARTESIAN_POINT('Ctrl Pts',(5.96883887250414,10.7589485983184,27.0657413198323));
#112328=CARTESIAN_POINT('Ctrl Pts',(7.18565321718825,10.6877206647982,27.6923362335609));
#112329=CARTESIAN_POINT('Ctrl Pts',(7.32328607724665,10.616492731278,29.0540853254779));
#112330=CARTESIAN_POINT('Ctrl Pts',(6.25645389934898,10.5452647977578,29.9114956730229));
#112331=CARTESIAN_POINT('Ctrl Pts',(4.95619769223396,10.4740368642377,29.4841591479963));
#112332=CARTESIAN_POINT('Ctrl Pts',(4.60601491366951,10.4028089307175,28.1610339130119));
#112333=CARTESIAN_POINT('Ctrl Pts',(5.52464501704607,10.3315809971973,27.1464383697959));
#112334=CARTESIAN_POINT('Ctrl Pts',(6.87594546763495,10.2603530636771,27.3638611224465));
#112335=CARTESIAN_POINT('Ctrl Pts',(7.42995592786307,10.1891251301569,28.6154036337889));
#112336=CARTESIAN_POINT('Ctrl Pts',(6.68241303332923,10.1178971966367,29.7619050238867));
#112337=CARTESIAN_POINT('Ctrl Pts',(5.31373428926388,10.0466692631166,29.7598139910742));
#112338=CARTESIAN_POINT('Ctrl Pts',(4.56969813627773,9.97544132959639,28.6110336988249));
#112339=CARTESIAN_POINT('Ctrl Pts',(5.12753016011334,9.90421339607621,27.3611899768344));
#112340=CARTESIAN_POINT('Ctrl Pts',(6.47948874973347,9.83298546255602,27.1478970303935));
#112341=CARTESIAN_POINT('Ctrl Pts',(7.39501419647751,9.76175752903586,28.1652952190123));
#112342=CARTESIAN_POINT('Ctrl Pts',(7.04079049084549,9.69052959551567,29.4873434314113));
#112343=CARTESIAN_POINT('Ctrl Pts',(5.73923388709102,9.61930166199549,29.9107065369007));
#112344=CARTESIAN_POINT('Ctrl Pts',(4.67502795044644,9.5480737284753,29.0500372408509));
#112345=CARTESIAN_POINT('Ctrl Pts',(4.81681844012803,9.47684579495514,27.6887211979427));
#112346=CARTESIAN_POINT('Ctrl Pts',(6.03554691737803,9.40561786143494,27.065835324953));
#112347=CARTESIAN_POINT('Ctrl Pts',(7.22192040624659,9.33438992791478,27.7483335718489));
#112348=CARTESIAN_POINT('Ctrl Pts',(7.29609560871817,9.26316199439458,29.1150024971194));
#112349=CARTESIAN_POINT('Ctrl Pts',(6.19055787111928,9.19193406087441,29.9218929622801));
#112350=CARTESIAN_POINT('Ctrl Pts',(4.91157337165486,9.12070612735422,29.4345690841905));
#112351=CARTESIAN_POINT('Ctrl Pts',(4.62328043009203,9.04947819383405,28.0965955822655));
#112352=CARTESIAN_POINT('Ctrl Pts',(5.58808477591762,8.97825026031386,27.1258028720057));
#112353=CARTESIAN_POINT('Ctrl Pts',(6.92781649345744,8.90702232679368,27.405811509435));
#112354=CARTESIAN_POINT('Ctrl Pts',(7.42304483023598,8.83579439327351,28.6817561816157));
#112355=CARTESIAN_POINT('Ctrl Pts',(6.62301038759335,8.76456645975332,29.7922654353375));
#112356=CARTESIAN_POINT('Ctrl Pts',(5.25590866140714,8.69333852623314,29.7265479926395));
#112357=CARTESIAN_POINT('Ctrl Pts',(4.56608272786717,8.62211059271296,28.544420210447));
#112358=CARTESIAN_POINT('Ctrl Pts',(5.18141572670952,8.55088265919278,27.3218609224974));
#112359=CARTESIAN_POINT('Ctrl Pts',(6.54182837342008,8.4796547256726,27.1716499286054));
#112360=CARTESIAN_POINT('Ctrl Pts',(7.40906602661399,8.40842679215242,28.230510053881));
#112361=CARTESIAN_POINT('Ctrl Pts',(6.99376447988865,8.33719885863224,29.5346613247478));
#112362=CARTESIAN_POINT('Ctrl Pts',(5.67393335337658,8.26597092511206,29.8970584956889));
#112363=CARTESIAN_POINT('Ctrl Pts',(4.65088977846434,8.19474299159189,28.9878457835881));
#112364=CARTESIAN_POINT('Ctrl Pts',(4.85581331896708,8.12351505807169,27.6345933110003));
#112365=CARTESIAN_POINT('Ctrl Pts',(6.10218150630337,8.05228712455152,27.069038491718));
#112366=CARTESIAN_POINT('Ctrl Pts',(7.2555435570434,7.98105919103133,27.8059522532403));
#112367=CARTESIAN_POINT('Ctrl Pts',(7.26610335530344,7.90983125751117,29.1745918707756));
#112368=CARTESIAN_POINT('Ctrl Pts',(6.12424931796667,7.83860332399097,29.9292144714445));
#112369=CARTESIAN_POINT('Ctrl Pts',(4.86930290751199,7.7673753904708,29.3829586533074));
#112370=CARTESIAN_POINT('Ctrl Pts',(4.64352285045029,7.69614745695061,28.0330292929558));
#112371=CARTESIAN_POINT('Ctrl Pts',(5.65241532493153,7.62491952343044,27.1081390903017));
#112372=CARTESIAN_POINT('Ctrl Pts',(6.97768117188443,7.55369158991026,27.4501279008548));
#112373=CARTESIAN_POINT('Ctrl Pts',(7.41305654961269,7.48246365639007,28.7477157372729));
#112374=CARTESIAN_POINT('Ctrl Pts',(6.56226053219187,7.4112357228699,29.8198314253437));
#112375=CARTESIAN_POINT('Ctrl Pts',(5.19969206545444,7.34000778934971,29.6906297109905));
#112376=CARTESIAN_POINT('Ctrl Pts',(4.56556802638696,7.26877985582953,28.4777106613761));
#112377=CARTESIAN_POINT('Ctrl Pts',(5.23707140746509,7.19755192230936,27.2850794869346));
#112378=CARTESIAN_POINT('Ctrl Pts',(6.60299633993354,7.12632398878917,27.1982752527247));
#112379=CARTESIAN_POINT('Ctrl Pts',(7.42007089321032,7.055096055269,28.296307643503));
#112380=CARTESIAN_POINT('Ctrl Pts',(6.94458953181559,6.9838681217488,29.5797418458838));
#112381=CARTESIAN_POINT('Ctrl Pts',(5.60933793803721,6.91264018822865,29.8803894768019));
#112382=CARTESIAN_POINT('Ctrl Pts',(4.62966887089418,6.84141225470844,28.9245993499317));
#112383=CARTESIAN_POINT('Ctrl Pts',(4.89728250718407,6.77018432118827,27.5823368931806));
#112384=CARTESIAN_POINT('Ctrl Pts',(6.16859491519707,6.69895638766809,27.0753357646064));
#112385=CARTESIAN_POINT('Ctrl Pts',(7.28645214666137,6.62772845414791,27.8650721610822));
#112386=CARTESIAN_POINT('Ctrl Pts',(7.23337243036839,6.55650052062773,29.2327216971408));
#112387=CARTESIAN_POINT('Ctrl Pts',(6.05767372938362,6.48527258710755,29.9334470102113));
#112388=CARTESIAN_POINT('Ctrl Pts',(4.82947427053619,6.41404465358737,29.329435849063));
#112389=CARTESIAN_POINT('Ctrl Pts',(4.66670475343396,6.34281672006718,27.9704787417039));
#112390=CARTESIAN_POINT('Ctrl Pts',(5.71748535948215,6.27158878654701,27.0934734707287));
#112391=CARTESIAN_POINT('Ctrl Pts',(7.02545534073696,6.20036085302682,27.4967371456878));
#112392=CARTESIAN_POINT('Ctrl Pts',(7.39996663454834,6.12913291950666,28.8130956020155));
#112393=CARTESIAN_POINT('Ctrl Pts',(6.50038451462898,6.05790498598646,29.8446291687303));
#112394=CARTESIAN_POINT('Ctrl Pts',(5.14503129746557,5.98667705246629,29.6519697089475));
#112395=CARTESIAN_POINT('Ctrl Pts',(4.56849656644862,5.91544911894611,28.4113752660494));
#112396=CARTESIAN_POINT('Ctrl Pts',(5.29370128702602,5.84422118542592,27.2502852676862));
#112397=CARTESIAN_POINT('Ctrl Pts',(6.66428546970392,5.77299325190575,27.2290141030205));
#112398=CARTESIAN_POINT('Ctrl Pts',(7.17081804402867,5.72550796289229,27.9826553944107));
#112399=CARTESIAN_POINT('Ctrl Pts',(7.20941017178877,5.70176531838556,28.3835867860857));
#112400=CARTESIAN_POINT('Ctrl Pts',(4.78332770288896,5.91989265014994,28.4996492411853));
#112401=CARTESIAN_POINT('Ctrl Pts',(4.78320592741866,5.918411473082,28.4746203412927));
#112402=CARTESIAN_POINT('Ctrl Pts',(4.78390735364816,5.91693029601405,28.4495973891199));
#112403=CARTESIAN_POINT('Ctrl Pts',(4.78545314171435,5.91544911894611,28.4246260068052));
#112404=CARTESIAN_POINT('Ctrl Pts',(4.80822117514724,5.89363274596407,28.056820561903));
#112405=CARTESIAN_POINT('Ctrl Pts',(5.01416991798751,5.87181637298203,27.7002029783913));
#112406=CARTESIAN_POINT('Ctrl Pts',(5.31842995130037,5.85,27.4918752544675));
#112407=CARTESIAN_POINT('',(5.44356679200015,11.4,27.719855688007));
#112408=CARTESIAN_POINT('Ctrl Pts',(5.44236585452934,11.4,27.7188687169901));
#112409=CARTESIAN_POINT('Ctrl Pts',(5.41929639243372,11.4,27.7310193813045));
#112410=CARTESIAN_POINT('Ctrl Pts',(5.39680487402872,11.4,27.7441433138064));
#112411=CARTESIAN_POINT('Ctrl Pts',(5.37496061693956,11.4,27.758225558774));
#112412=CARTESIAN_POINT('Ctrl Pts',(5.33899532853094,11.4,27.781411149368));
#112413=CARTESIAN_POINT('Ctrl Pts',(5.30478305575494,11.4,27.8071912108618));
#112414=CARTESIAN_POINT('Ctrl Pts',(5.27240127912232,11.4,27.8352556189204));
#112415=CARTESIAN_POINT('Ctrl Pts',(5.26070812807527,11.4,27.8453897559753));
#112416=CARTESIAN_POINT('Ctrl Pts',(5.2492538497354,11.4,27.8558222981223));
#112417=CARTESIAN_POINT('Ctrl Pts',(5.23804281847565,11.4,27.8665403464387));
#112418=CARTESIAN_POINT('Ctrl Pts',(5.23143763632547,11.4,27.8728550787576));
#112419=CARTESIAN_POINT('Ctrl Pts',(5.22491828276335,11.4,27.8792677296922));
#112420=CARTESIAN_POINT('Ctrl Pts',(5.21849207070704,11.4,27.8857687790983));
#112421=CARTESIAN_POINT('Ctrl Pts',(5.18802043682045,11.4,27.916595274652));
#112422=CARTESIAN_POINT('Ctrl Pts',(5.15959899380616,11.4,27.9494454109169));
#112423=CARTESIAN_POINT('Ctrl Pts',(5.13330469735818,11.4,27.9840130699589));
#112424=CARTESIAN_POINT('Ctrl Pts',(5.11565463130143,11.4,28.0072166368133));
#112425=CARTESIAN_POINT('Ctrl Pts',(5.09896336056599,11.4,28.0311952291343));
#112426=CARTESIAN_POINT('Ctrl Pts',(5.08326058957769,11.4,28.0558675649596));
#112427=CARTESIAN_POINT('Ctrl Pts',(5.07776016491816,11.4,28.0645098819418));
#112428=CARTESIAN_POINT('Ctrl Pts',(5.072381082364,11.4,28.0732373911495));
#112429=CARTESIAN_POINT('Ctrl Pts',(5.06712480617071,11.4,28.0820468134777));
#112430=CARTESIAN_POINT('Ctrl Pts',(5.06241211437772,11.4,28.0899451983382));
#112431=CARTESIAN_POINT('Ctrl Pts',(5.05780320235102,11.4,28.0979009550975));
#112432=CARTESIAN_POINT('Ctrl Pts',(5.05329864744776,11.4,28.1059112074879));
#112433=CARTESIAN_POINT('Ctrl Pts',(5.0305805054366,11.4,28.1463098828861));
#112434=CARTESIAN_POINT('Ctrl Pts',(5.01051422554295,11.4,28.1880908178382));
#112435=CARTESIAN_POINT('Ctrl Pts',(4.99318973218758,11.4,28.2309187368455));
#112436=CARTESIAN_POINT('Ctrl Pts',(4.97600243405743,11.4,28.2734074952278));
#112437=CARTESIAN_POINT('Ctrl Pts',(4.9615129573089,11.4,28.3169278593784));
#112438=CARTESIAN_POINT('Ctrl Pts',(4.94984536082048,11.4,28.3611917087713));
#112439=CARTESIAN_POINT('Ctrl Pts',(4.94394171134737,11.4,28.383588631));
#112440=CARTESIAN_POINT('Ctrl Pts',(4.93876117027847,11.4,28.406176422574));
#112441=CARTESIAN_POINT('Ctrl Pts',(4.93432428336464,11.4,28.4289202098503));
#112442=CARTESIAN_POINT('Ctrl Pts',(4.93239433792724,11.4,28.4388132428114));
#112443=CARTESIAN_POINT('Ctrl Pts',(4.93060513801621,11.4,28.4487358066513));
#112444=CARTESIAN_POINT('Ctrl Pts',(4.92895857810374,11.4,28.4586850913254));
#112445=CARTESIAN_POINT('Ctrl Pts',(4.92741239852659,11.4,28.4680278310908));
#112446=CARTESIAN_POINT('Ctrl Pts',(4.92599326509749,11.4,28.4773869022515));
#112447=CARTESIAN_POINT('Ctrl Pts',(4.92470308531398,11.4,28.4867524084507));
#112448=CARTESIAN_POINT('Ctrl Pts',(4.91825490900801,11.4,28.533560175817));
#112449=CARTESIAN_POINT('Ctrl Pts',(4.91501503058571,11.4,28.5805826774575));
#112450=CARTESIAN_POINT('Ctrl Pts',(4.91509471552749,11.4,28.6275076383839));
#112451=CARTESIAN_POINT('Ctrl Pts',(4.91509920937683,11.4,28.6301539815936));
#112452=CARTESIAN_POINT('Ctrl Pts',(4.91511427250471,11.4,28.632800021888));
#112453=CARTESIAN_POINT('Ctrl Pts',(4.9151399291788,11.4,28.6354457056802));
#112454=CARTESIAN_POINT('Ctrl Pts',(4.91557879360603,11.4,28.6807008505191));
#112455=CARTESIAN_POINT('Ctrl Pts',(4.91911290856199,11.4,28.7258508482717));
#112456=CARTESIAN_POINT('Ctrl Pts',(4.9255527364275,11.4,28.7706884317727));
#112457=CARTESIAN_POINT('Ctrl Pts',(4.92863804253891,11.4,28.7921700106729));
#112458=CARTESIAN_POINT('Ctrl Pts',(4.93239107473155,11.4,28.8135800248162));
#112459=CARTESIAN_POINT('Ctrl Pts',(4.93679506065869,11.4,28.8348960383463));
#112460=CARTESIAN_POINT('Ctrl Pts',(4.93920868546902,11.4,28.846578377928));
#112461=CARTESIAN_POINT('Ctrl Pts',(4.94181787816965,11.4,28.8582324833904));
#112462=CARTESIAN_POINT('Ctrl Pts',(4.9446201969184,11.4,28.8698546405969));
#112463=CARTESIAN_POINT('Ctrl Pts',(4.94686168957134,11.4,28.8791508635913));
#112464=CARTESIAN_POINT('Ctrl Pts',(4.94922714845825,11.4,28.8884276707925));
#112465=CARTESIAN_POINT('Ctrl Pts',(4.951710567034,11.4,28.8976664763574));
#112466=CARTESIAN_POINT('Ctrl Pts',(4.9640107207681,11.4,28.943425467563));
#112467=CARTESIAN_POINT('Ctrl Pts',(4.97922190573704,11.4,28.9883459503613));
#112468=CARTESIAN_POINT('Ctrl Pts',(4.99711839802598,11.4,29.03220214847));
#112469=CARTESIAN_POINT('Ctrl Pts',(5.0154230471994,11.4,29.0770585542674));
#112470=CARTESIAN_POINT('Ctrl Pts',(5.03653708345249,11.4,29.1208025845277));
#112471=CARTESIAN_POINT('Ctrl Pts',(5.06027378632928,11.4,29.1631943136911));
#112472=CARTESIAN_POINT('Ctrl Pts',(5.07245594705277,11.4,29.184950614922));
#112473=CARTESIAN_POINT('Ctrl Pts',(5.08532976385118,11.4,29.2063506584299));
#112474=CARTESIAN_POINT('Ctrl Pts',(5.09887511842553,11.4,29.2273608018555));
#112475=CARTESIAN_POINT('Ctrl Pts',(5.10866570028309,11.4,29.2425469328584));
#112476=CARTESIAN_POINT('Ctrl Pts',(5.11880719188057,11.4,29.2575293461396));
#112477=CARTESIAN_POINT('Ctrl Pts',(5.12929303687149,11.4,29.272294842613));
#112478=CARTESIAN_POINT('Ctrl Pts',(5.13459302453246,11.4,29.2797579463671));
#112479=CARTESIAN_POINT('Ctrl Pts',(5.13998063995912,11.4,29.2871649462043));
#112480=CARTESIAN_POINT('Ctrl Pts',(5.14544679291759,11.4,29.2945035086901));
#112481=CARTESIAN_POINT('Ctrl Pts',(5.1756022432867,11.4,29.3349885918014));
#112482=CARTESIAN_POINT('Ctrl Pts',(5.20820460790424,11.4,29.3734783462811));
#112483=CARTESIAN_POINT('Ctrl Pts',(5.2430422389611,11.4,29.4097237064037));
#112484=CARTESIAN_POINT('Ctrl Pts',(5.27762857250277,11.4,29.4457076145086));
#112485=CARTESIAN_POINT('Ctrl Pts',(5.31441858772413,11.4,29.4794804704309));
#112486=CARTESIAN_POINT('Ctrl Pts',(5.35325235903682,11.4,29.5107811307126));
#112487=CARTESIAN_POINT('Ctrl Pts',(5.39003997418695,11.4,29.5404325553737));
#112488=CARTESIAN_POINT('Ctrl Pts',(5.42866236215027,11.4,29.5678661195985));
#112489=CARTESIAN_POINT('Ctrl Pts',(5.46901649069989,11.4,29.5928318776698));
#112490=CARTESIAN_POINT('Ctrl Pts',(5.44236585452935,11.4,27.7188687169901));
#112491=CARTESIAN_POINT('Ctrl Pts',(5.68005732911861,11.378183627018,27.551292360927));
#112492=CARTESIAN_POINT('Ctrl Pts',(6.34883662302045,11.3326246095292,27.4382884675306));
#112493=CARTESIAN_POINT('Ctrl Pts',(7.08668716007769,11.2633229475337,28.1849858242981));
#112494=CARTESIAN_POINT('Ctrl Pts',(6.85620622293074,11.1920950140135,29.2397882902982));
#112495=CARTESIAN_POINT('Ctrl Pts',(5.84626444085431,11.1208670804934,29.6209123918368));
#112496=CARTESIAN_POINT('Ctrl Pts',(5.13801470280774,11.062877853077,29.1007019983506));
#112497=CARTESIAN_POINT('Ctrl Pts',(5.04282495179103,11.0286312701673,28.6413433409797));
#112498=CARTESIAN_POINT('Ctrl Pts',(5.04321154726233,11.0181273317644,28.5002974317561));
#112499=CARTESIAN_POINT('Origin',(6.,11.4,28.5));
#112500=CARTESIAN_POINT('',(6.,11.4,27.285));
#112501=CARTESIAN_POINT('Origin',(6.,11.4,28.5));
#112502=CARTESIAN_POINT('',(6.55643320799983,11.4,27.719855688007));
#112503=CARTESIAN_POINT('Ctrl Pts',(6.53227676969645,11.4,29.5943192153712));
#112504=CARTESIAN_POINT('Ctrl Pts',(6.56009586842551,11.4,29.5772957655189));
#112505=CARTESIAN_POINT('Ctrl Pts',(6.58713321731184,11.4,29.559109236633));
#112506=CARTESIAN_POINT('Ctrl Pts',(6.61330405187189,11.4,29.5397557928319));
#112507=CARTESIAN_POINT('Ctrl Pts',(6.65150531228641,11.4,29.5115057977901));
#112508=CARTESIAN_POINT('Ctrl Pts',(6.68786194993602,11.4,29.4807700839748));
#112509=CARTESIAN_POINT('Ctrl Pts',(6.72225055334609,11.4,29.4478022886025));
#112510=CARTESIAN_POINT('Ctrl Pts',(6.73459601655902,11.4,29.4359668935989));
#112511=CARTESIAN_POINT('Ctrl Pts',(6.74668750835909,11.4,29.4238436266695));
#112512=CARTESIAN_POINT('Ctrl Pts',(6.758518161031,11.4,29.4114436725547));
#112513=CARTESIAN_POINT('Ctrl Pts',(6.76638038812047,11.4,29.4032031081621));
#112514=CARTESIAN_POINT('Ctrl Pts',(6.77412910935597,11.4,29.3948384346475));
#112515=CARTESIAN_POINT('Ctrl Pts',(6.78175654779426,11.4,29.3863591511914));
#112516=CARTESIAN_POINT('Ctrl Pts',(6.8151051921031,11.4,29.3492860747895));
#112517=CARTESIAN_POINT('Ctrl Pts',(6.84607247709509,11.4,29.3101005145376));
#112518=CARTESIAN_POINT('Ctrl Pts',(6.87451984987947,11.4,29.2691010316144));
#112519=CARTESIAN_POINT('Ctrl Pts',(6.89278958823532,11.4,29.2427699594479));
#112520=CARTESIAN_POINT('Ctrl Pts',(6.91001905979329,11.4,29.2156901141727));
#112521=CARTESIAN_POINT('Ctrl Pts',(6.9261607775362,11.4,29.1879371115855));
#112522=CARTESIAN_POINT('Ctrl Pts',(6.93310293612802,11.4,29.1760012229504));
#112523=CARTESIAN_POINT('Ctrl Pts',(6.93984378696841,11.4,29.1639408058629));
#112524=CARTESIAN_POINT('Ctrl Pts',(6.94637903470487,11.4,29.1517618350014));
#112525=CARTESIAN_POINT('Ctrl Pts',(6.95299599440079,11.4,29.1394305871928));
#112526=CARTESIAN_POINT('Ctrl Pts',(6.95940454410974,11.4,29.1269725966841));
#112527=CARTESIAN_POINT('Ctrl Pts',(6.96558603837658,11.4,29.1144233999878));
#112528=CARTESIAN_POINT('Ctrl Pts',(6.98735658913844,11.4,29.0702264935599));
#112529=CARTESIAN_POINT('Ctrl Pts',(7.00634741419601,11.4,29.0248440317963));
#112530=CARTESIAN_POINT('Ctrl Pts',(7.02241524341161,11.4,28.9785600143272));
#112531=CARTESIAN_POINT('Ctrl Pts',(7.0378215111397,11.4,28.9341816508849));
#112532=CARTESIAN_POINT('Ctrl Pts',(7.05054049359629,11.4,28.8889733437029));
#112533=CARTESIAN_POINT('Ctrl Pts',(7.06039713686446,11.4,28.8431830029673));
#112534=CARTESIAN_POINT('Ctrl Pts',(7.06564289954092,11.4,28.8188131182268));
#112535=CARTESIAN_POINT('Ctrl Pts',(7.07007708883368,11.4,28.7942784321479));
#112536=CARTESIAN_POINT('Ctrl Pts',(7.07366735925498,11.4,28.769617552813));
#112537=CARTESIAN_POINT('Ctrl Pts',(7.07556720571225,11.4,28.7565678716638));
#112538=CARTESIAN_POINT('Ctrl Pts',(7.0772306699916,11.4,28.7434828754754));
#112539=CARTESIAN_POINT('Ctrl Pts',(7.07865246709527,11.4,28.7303684622724));
#112540=CARTESIAN_POINT('Ctrl Pts',(7.07981067743981,11.4,28.7196853282338));
#112541=CARTESIAN_POINT('Ctrl Pts',(7.08080850347668,11.4,28.7089806683397));
#112542=CARTESIAN_POINT('Ctrl Pts',(7.08164168102371,11.4,28.6982800333765));
#112543=CARTESIAN_POINT('Ctrl Pts',(7.08516358169497,11.4,28.65304768933));
#112544=CARTESIAN_POINT('Ctrl Pts',(7.08575848266697,11.4,28.6077985937119));
#112545=CARTESIAN_POINT('Ctrl Pts',(7.08327554477619,11.4,28.5627634602742));
#112546=CARTESIAN_POINT('Ctrl Pts',(7.08297898295393,11.4,28.5573844690045));
#112547=CARTESIAN_POINT('Ctrl Pts',(7.08263845271376,11.4,28.5520085411666));
#112548=CARTESIAN_POINT('Ctrl Pts',(7.08225364749099,11.4,28.5466360808279));
#112549=CARTESIAN_POINT('Ctrl Pts',(7.07893395049718,11.4,28.5002881120886));
#112550=CARTESIAN_POINT('Ctrl Pts',(7.07232298042015,11.4,28.4541960936328));
#112551=CARTESIAN_POINT('Ctrl Pts',(7.06257414795014,11.4,28.408635171883));
#112552=CARTESIAN_POINT('Ctrl Pts',(7.05820362076849,11.4,28.3882096237426));
#112553=CARTESIAN_POINT('Ctrl Pts',(7.05320181052273,11.4,28.36789117292));
#112554=CARTESIAN_POINT('Ctrl Pts',(7.04757982578894,11.4,28.3477067393106));
#112555=CARTESIAN_POINT('Ctrl Pts',(7.04447805167662,11.4,28.3365705380212));
#112556=CARTESIAN_POINT('Ctrl Pts',(7.04118747121866,11.4,28.3254751580379));
#112557=CARTESIAN_POINT('Ctrl Pts',(7.03770976801826,11.4,28.3144253383296));
#112558=CARTESIAN_POINT('Ctrl Pts',(7.03513303023879,11.4,28.3062381854135));
#112559=CARTESIAN_POINT('Ctrl Pts',(7.03245398332033,11.4,28.2980777026375));
#112560=CARTESIAN_POINT('Ctrl Pts',(7.02967749022565,11.4,28.289956936927));
#112561=CARTESIAN_POINT('Ctrl Pts',(7.01507754006223,11.4,28.2472545888136));
#112562=CARTESIAN_POINT('Ctrl Pts',(6.99775983297723,11.4,28.2055611382969));
#112563=CARTESIAN_POINT('Ctrl Pts',(6.97788617801526,11.4,28.1651206298401));
#112564=CARTESIAN_POINT('Ctrl Pts',(6.95814638641366,11.4,28.1249525172947));
#112565=CARTESIAN_POINT('Ctrl Pts',(6.93588409561569,11.4,28.0860196184813));
#112566=CARTESIAN_POINT('Ctrl Pts',(6.91122083093872,11.4,28.0485958527553));
#112567=CARTESIAN_POINT('Ctrl Pts',(6.89994882389591,11.4,28.0314918336258));
#112568=CARTESIAN_POINT('Ctrl Pts',(6.88817486340293,11.4,28.0147036092703));
#112569=CARTESIAN_POINT('Ctrl Pts',(6.87590868972221,11.4,27.9982605461768));
#112570=CARTESIAN_POINT('Ctrl Pts',(6.86891967402599,11.4,27.9888916240462));
#112571=CARTESIAN_POINT('Ctrl Pts',(6.86177084341387,11.4,27.9796347982128));
#112572=CARTESIAN_POINT('Ctrl Pts',(6.85446387232953,11.4,27.9704958415884));
#112573=CARTESIAN_POINT('Ctrl Pts',(6.84795581120752,11.4,27.9623560956367));
#112574=CARTESIAN_POINT('Ctrl Pts',(6.84132071214378,11.4,27.9543082434474));
#112575=CARTESIAN_POINT('Ctrl Pts',(6.83457496983701,11.4,27.9463737351544));
#112576=CARTESIAN_POINT('Ctrl Pts',(6.80665793921521,11.4,27.9135370359579));
#112577=CARTESIAN_POINT('Ctrl Pts',(6.77679555241335,11.4,27.8825701223949));
#112578=CARTESIAN_POINT('Ctrl Pts',(6.74510829213929,11.4,27.8537112982286));
#112579=CARTESIAN_POINT('Ctrl Pts',(6.71455398152641,11.4,27.8258842955191));
#112580=CARTESIAN_POINT('Ctrl Pts',(6.68230215548925,11.4,27.8000169061952));
#112581=CARTESIAN_POINT('Ctrl Pts',(6.64844095673588,11.4,27.7763655977035));
#112582=CARTESIAN_POINT('Ctrl Pts',(6.61897378626944,11.4,27.7557834220943));
#112583=CARTESIAN_POINT('Ctrl Pts',(6.58828727976892,11.4,27.7368799036835));
#112584=CARTESIAN_POINT('Ctrl Pts',(6.55643320799986,11.4,27.719855688007));
#112585=CARTESIAN_POINT('Origin',(6.,11.4,28.5));
#112586=CARTESIAN_POINT('Origin',(6.,11.4,28.5));
#112587=CARTESIAN_POINT('Origin',(6.,12.2318726682356,28.5));
#112588=CARTESIAN_POINT('Ctrl Pts',(6.55643320799984,11.4,27.719855688007));
#112589=CARTESIAN_POINT('Ctrl Pts',(6.81505873638613,11.3762573554933,27.9043187805636));
#112590=CARTESIAN_POINT('Ctrl Pts',(7.13006311729091,11.3287720664798,28.5474835379439));
#112591=CARTESIAN_POINT('Ctrl Pts',(6.57505709906184,11.2575441329596,29.4752298620382));
#112592=CARTESIAN_POINT('Ctrl Pts',(5.49603095095993,11.1863161994395,29.5126937568152));
#112593=CARTESIAN_POINT('Ctrl Pts',(5.05886120171314,11.1360923778648,28.8900758133155));
#112594=CARTESIAN_POINT('Ctrl Pts',(5.04043290394666,11.1096112007968,28.5371813420894));
#112595=CARTESIAN_POINT('Ctrl Pts',(5.04070147463229,11.1068726682356,28.5006572399252));
#112596=CARTESIAN_POINT('Ctrl Pts',(6.70552188648034,11.5482346816144,27.5108266745928));
#112597=CARTESIAN_POINT('Ctrl Pts',(7.03344259296544,11.5244920371077,27.7447141334565));
#112598=CARTESIAN_POINT('Ctrl Pts',(7.43284809549538,11.4770067480942,28.5602061034195));
#112599=CARTESIAN_POINT('Ctrl Pts',(6.72913579479277,11.4057788145741,29.7365293841653));
#112600=CARTESIAN_POINT('Ctrl Pts',(5.36099932733244,11.3345508810539,29.7840312178768));
#112601=CARTESIAN_POINT('Ctrl Pts',(4.57488060118859,11.2633229475337,28.6644395135981));
#112602=CARTESIAN_POINT('Ctrl Pts',(5.08570913854379,11.1920950140135,27.3943397937036));
#112603=CARTESIAN_POINT('Ctrl Pts',(6.42883461776721,11.1208670804934,27.1310453430996));
#112604=CARTESIAN_POINT('Ctrl Pts',(7.38157887727883,11.0496391469732,28.1135610780722));
#112605=CARTESIAN_POINT('Ctrl Pts',(7.07683046210633,10.978411213453,29.4479281552317));
#112606=CARTESIAN_POINT('Ctrl Pts',(5.79193122289995,10.9071832799328,29.9194282983902));
#112607=CARTESIAN_POINT('Ctrl Pts',(4.69642452967151,10.8359553464126,29.0989871246045));
#112608=CARTESIAN_POINT('Ctrl Pts',(4.78743525526326,10.7647274128924,27.7333295326587));
#112609=CARTESIAN_POINT('Ctrl Pts',(5.98213061030333,10.6934994793723,27.0655071925963));
#112610=CARTESIAN_POINT('Ctrl Pts',(7.19308979364578,10.6222715458521,27.7033636264439));
#112611=CARTESIAN_POINT('Ctrl Pts',(7.31809296809601,10.5510436123319,29.0663246763108));
#112612=CARTESIAN_POINT('Ctrl Pts',(6.24336083300543,10.4798156788117,29.9138130132872));
#112613=CARTESIAN_POINT('Ctrl Pts',(4.94712053941611,10.4085877452916,29.4744419613097));
#112614=CARTESIAN_POINT('Ctrl Pts',(4.60921651917625,10.3373598117713,28.148128507454));
#112615=CARTESIAN_POINT('Ctrl Pts',(5.53721086595077,10.2661318782512,27.1420904527186));
#112616=CARTESIAN_POINT('Ctrl Pts',(6.88643826296769,10.194903944731,27.372028631878));
#112617=CARTESIAN_POINT('Ctrl Pts',(7.42882496828635,10.1236760112108,28.6286522337076));
#112618=CARTESIAN_POINT('Ctrl Pts',(6.67068777783787,10.0524480776906,29.7681758863312));
#112619=CARTESIAN_POINT('Ctrl Pts',(5.3020870985883,9.98122014417048,29.7533992848146));
#112620=CARTESIAN_POINT('Ctrl Pts',(4.56873035789448,9.90999221065029,28.5977721534116));
#112621=CARTESIAN_POINT('Ctrl Pts',(5.13812266365143,9.83876427713011,27.3531523038847));
#112622=CARTESIAN_POINT('Ctrl Pts',(6.49200018730981,9.76753634360992,27.1523991695659));
#112623=CARTESIAN_POINT('Ctrl Pts',(7.39805659085291,9.69630841008975,28.178239295749));
#112624=CARTESIAN_POINT('Ctrl Pts',(7.03159463987624,9.62508047656957,29.4969476821148));
#112625=CARTESIAN_POINT('Ctrl Pts',(5.7261699014817,9.55385254304938,29.9082291217125));
#112626=CARTESIAN_POINT('Ctrl Pts',(4.66998673786223,9.48262460952922,29.0377331164763));
#112627=CARTESIAN_POINT('Ctrl Pts',(4.82438853825604,9.41139667600901,27.6777896418652));
#112628=CARTESIAN_POINT('Ctrl Pts',(6.04883798373843,9.34016874248886,27.0662262963153));
#112629=CARTESIAN_POINT('Ctrl Pts',(7.22883484332198,9.26894080896865,27.7596912064148));
#112630=CARTESIAN_POINT('Ctrl Pts',(7.29033986006644,9.1977128754485,29.1269890170851));
#112631=CARTESIAN_POINT('Ctrl Pts',(6.17737084898319,9.12648494192828,29.9235981750324));
#112632=CARTESIAN_POINT('Ctrl Pts',(4.90295797192927,9.05525700840813,29.4244408962554));
#112633=CARTESIAN_POINT('Ctrl Pts',(4.6270784342541,8.98402907488794,28.0838527227856));
#112634=CARTESIAN_POINT('Ctrl Pts',(5.60083922089711,8.91280114136776,27.1220439577224));
#112635=CARTESIAN_POINT('Ctrl Pts',(6.93791821733336,8.84157320784759,27.414457923608));
#112636=CARTESIAN_POINT('Ctrl Pts',(7.42129919158453,8.77034527432739,28.6949379132555));
#112637=CARTESIAN_POINT('Ctrl Pts',(6.61100627576171,8.69911734080723,29.7979844039908));
#112638=CARTESIAN_POINT('Ctrl Pts',(5.24457228119594,8.62788940728703,29.7195987633995));
#112639=CARTESIAN_POINT('Ctrl Pts',(4.5657325112955,8.55666147376687,28.5311280077824));
#112640=CARTESIAN_POINT('Ctrl Pts',(5.19237044271588,8.48543354024667,27.3143243781604));
#112641=CARTESIAN_POINT('Ctrl Pts',(6.5541169827227,8.4142056067265,27.1767288443099));
#112642=CARTESIAN_POINT('Ctrl Pts',(7.41150337333956,8.34297767320631,28.2435815742308));
#112643=CARTESIAN_POINT('Ctrl Pts',(6.98413207841647,8.27174973968614,29.543827684178));
#112644=CARTESIAN_POINT('Ctrl Pts',(5.66099866544571,8.20052180616594,29.8939764263401));
#112645=CARTESIAN_POINT('Ctrl Pts',(4.6464260240653,8.12929387264578,28.9753206009569));
#112646=CARTESIAN_POINT('Ctrl Pts',(4.86388343048399,8.05806593912559,27.6240255012248));
#112647=CARTESIAN_POINT('Ctrl Pts',(6.11544002641659,7.98683800560542,27.0700469300327));
#112648=CARTESIAN_POINT('Ctrl Pts',(7.26192251202089,7.91561007208523,27.8176190538471));
#112649=CARTESIAN_POINT('Ctrl Pts',(7.25979658729028,7.84438213856505,29.1862978513339));
#112650=CARTESIAN_POINT('Ctrl Pts',(6.11099727984544,7.77315420504487,29.9303047877157));
#112651=CARTESIAN_POINT('Ctrl Pts',(4.86116767315267,7.7019262715247,29.3724408939033));
#112652=CARTESIAN_POINT('Ctrl Pts',(4.64790915214598,7.63069833800451,28.0204767767365));
#112653=CARTESIAN_POINT('Ctrl Pts',(5.66533072850072,7.55947040448433,27.104977183086));
#112654=CARTESIAN_POINT('Ctrl Pts',(6.98737000937468,7.48824247096415,27.4592345859979));
#112655=CARTESIAN_POINT('Ctrl Pts',(7.4106999922714,7.41701453744397,28.7608020646698));
#112656=CARTESIAN_POINT('Ctrl Pts',(6.55000352810652,7.34578660392379,29.824986148261));
#112657=CARTESIAN_POINT('Ctrl Pts',(5.18869100836491,7.27455867040361,29.6831609811553));
#112658=CARTESIAN_POINT('Ctrl Pts',(4.56583612553444,7.20333073688343,28.4644165412846));
#112659=CARTESIAN_POINT('Ctrl Pts',(5.24836465697135,7.13210280336324,27.2780603810734));
#112660=CARTESIAN_POINT('Ctrl Pts',(6.61503552786216,7.06087486984307,27.2039199340835));
#112661=CARTESIAN_POINT('Ctrl Pts',(7.4218979617803,6.98964693632288,28.3094783981659));
#112662=CARTESIAN_POINT('Ctrl Pts',(6.93454133061941,6.91841900280271,29.5884503814807));
#112663=CARTESIAN_POINT('Ctrl Pts',(5.59656067072138,6.84719106928253,29.8767096350116));
#112664=CARTESIAN_POINT('Ctrl Pts',(4.62579192913807,6.77596313576234,28.9118797705062));
#112665=CARTESIAN_POINT('Ctrl Pts',(4.90583576184143,6.70473520224217,27.5721565059149));
#112666=CARTESIAN_POINT('Ctrl Pts',(6.18179108759432,6.63350726872198,27.0769578832154));
#112667=CARTESIAN_POINT('Ctrl Pts',(7.29228402945827,6.56227933520181,27.8770260282393));
#112668=CARTESIAN_POINT('Ctrl Pts',(7.22652398726094,6.49105140168162,29.2441157295397));
#112669=CARTESIAN_POINT('Ctrl Pts',(6.04439369632789,6.41982346816145,29.9339319479415));
#112670=CARTESIAN_POINT('Ctrl Pts',(4.82182049663989,6.34859553464126,29.3185281255925));
#112671=CARTESIAN_POINT('Ctrl Pts',(4.67170161798971,6.27736760112108,27.9581887871279));
#112672=CARTESIAN_POINT('Ctrl Pts',(5.73047192792967,6.2061396676009,27.0908275870229));
#112673=CARTESIAN_POINT('Ctrl Pts',(7.0348309571484,6.13491173408072,27.5064555648446));
#112674=CARTESIAN_POINT('Ctrl Pts',(7.39676834718207,6.06368380056054,28.8257241355228));
#112675=CARTESIAN_POINT('Ctrl Pts',(6.48837025004477,5.99245586704037,29.8498660763289));
#112676=CARTESIAN_POINT('Ctrl Pts',(5.13337661522674,5.92122793352017,29.6426470796435));
#112677=CARTESIAN_POINT('Ctrl Pts',(4.75938902674003,5.87374264450673,28.8151900159942));
#112678=CARTESIAN_POINT('Ctrl Pts',(4.78808807722243,5.85,28.4134292692096));
#112679=CARTESIAN_POINT('Ctrl Pts',(6.65582566032017,11.4988231210763,27.5805030123975));
#112680=CARTESIAN_POINT('Ctrl Pts',(6.96064797410567,11.4750804765696,27.7979156824922));
#112681=CARTESIAN_POINT('Ctrl Pts',(7.33191976942723,11.4275951875561,28.5559652482609));
#112682=CARTESIAN_POINT('Ctrl Pts',(6.67777622954912,11.3563672540359,29.6494295434563));
#112683=CARTESIAN_POINT('Ctrl Pts',(5.40600986854162,11.2851393205158,29.6935853975229));
#112684=CARTESIAN_POINT('Ctrl Pts',(4.67526452591967,11.2139113869956,28.6528565656924));
#112685=CARTESIAN_POINT('Ctrl Pts',(5.15011083365461,11.1426834534754,27.4722213459578));
#112686=CARTESIAN_POINT('Ctrl Pts',(6.39862795436207,11.0714555199552,27.2274730819635));
#112687=CARTESIAN_POINT('Ctrl Pts',(7.28426190149246,11.000227586435,28.140781432861));
#112688=CARTESIAN_POINT('Ctrl Pts',(7.00097964697716,10.9289996529148,29.381157084215));
#112689=CARTESIAN_POINT('Ctrl Pts',(5.80658737064218,10.8577717193947,29.8194452488397));
#112690=CARTESIAN_POINT('Ctrl Pts',(4.78824702679272,10.7865437858745,29.0567950960058));
#112691=CARTESIAN_POINT('Ctrl Pts',(4.87284705175466,10.7153158523543,27.7873330011059));
#112692=CARTESIAN_POINT('Ctrl Pts',(5.9833893114843,10.6440879188341,27.1665513704566));
#112693=CARTESIAN_POINT('Ctrl Pts',(7.10904979240614,10.5728599853139,27.7594778620847));
#112694=CARTESIAN_POINT('Ctrl Pts',(7.22524787356688,10.5016320517938,29.0264333565185));
#112695=CARTESIAN_POINT('Ctrl Pts',(6.22621874963804,10.4304041182736,29.8142254985652));
#112696=CARTESIAN_POINT('Ctrl Pts',(5.02128427096752,10.3591761847534,29.4058032854341));
#112697=CARTESIAN_POINT('Ctrl Pts',(4.70718185764031,10.2879482512332,28.1729139685544));
#112698=CARTESIAN_POINT('Ctrl Pts',(5.56980925008441,10.2167203177131,27.2377401855758));
#112699=CARTESIAN_POINT('Ctrl Pts',(6.82399847585742,10.1454923841929,27.4514817591112));
#112700=CARTESIAN_POINT('Ctrl Pts',(7.32818002710458,10.0742644506727,28.6195901044883));
#112701=CARTESIAN_POINT('Ctrl Pts',(6.62344522997508,10.0030365171525,29.6788468990019));
#112702=CARTESIAN_POINT('Ctrl Pts',(5.35124735577278,9.93180858363233,29.6651111458911));
#112703=CARTESIAN_POINT('Ctrl Pts',(4.66954749935143,9.86058065011214,28.5908851848551));
#112704=CARTESIAN_POINT('Ctrl Pts',(5.19883240469601,9.78935271659197,27.4339350599828));
#112705=CARTESIAN_POINT('Ctrl Pts',(6.45734420703772,9.71812478307177,27.2473227671554));
#112706=CARTESIAN_POINT('Ctrl Pts',(7.29957894210078,9.6468968495516,28.2009037843132));
#112707=CARTESIAN_POINT('Ctrl Pts',(6.95893018890553,9.57566891603142,29.4267237267286));
#112708=CARTESIAN_POINT('Ctrl Pts',(5.74545820814686,9.50444098251123,29.8090349304917));
#112709=CARTESIAN_POINT('Ctrl Pts',(4.76367148547647,9.43321304899107,28.9998557563513));
#112710=CARTESIAN_POINT('Ctrl Pts',(4.90719738401812,9.36198511547087,27.7357052823182));
#112711=CARTESIAN_POINT('Ctrl Pts',(6.04539788707867,9.2907571819507,27.1672198212593));
#112712=CARTESIAN_POINT('Ctrl Pts',(7.14227699804821,9.21952924843051,27.8118377860453));
#112713=CARTESIAN_POINT('Ctrl Pts',(7.19944966553364,9.14830131491035,29.0828245643727));
#112714=CARTESIAN_POINT('Ctrl Pts',(6.16487703129417,9.07707338139014,29.8233214037184));
#112715=CARTESIAN_POINT('Ctrl Pts',(4.98023246869392,9.00584544786998,29.359324243275));
#112716=CARTESIAN_POINT('Ctrl Pts',(4.72378559804155,8.93461751434979,28.1131657031491));
#112717=CARTESIAN_POINT('Ctrl Pts',(5.62895569004243,8.86338958082961,27.2191057447881));
#112718=CARTESIAN_POINT('Ctrl Pts',(6.87185223590666,8.79216164730945,27.4909223757654));
#112719=CARTESIAN_POINT('Ctrl Pts',(7.32118435826784,8.72093371378924,28.6812066898732));
#112720=CARTESIAN_POINT('Ctrl Pts',(6.56796763068576,8.64970578026909,29.7065557357536));
#112721=CARTESIAN_POINT('Ctrl Pts',(5.29778382215697,8.57847784674889,29.6336914979667));
#112722=CARTESIAN_POINT('Ctrl Pts',(4.66676081794155,8.50724991322872,28.5289353833659));
#112723=CARTESIAN_POINT('Ctrl Pts',(5.24925902675779,8.43602197970853,27.3978421328676));
#112724=CARTESIAN_POINT('Ctrl Pts',(6.51508556013996,8.36479404618836,27.2699386849748));
#112725=CARTESIAN_POINT('Ctrl Pts',(7.31207854724769,8.29356611266817,28.2616434208196));
#112726=CARTESIAN_POINT('Ctrl Pts',(6.91481084079411,8.222338179148,29.4703015503199));
#112727=CARTESIAN_POINT('Ctrl Pts',(5.68487756603469,8.15111024562781,29.7957861801226));
#112728=CARTESIAN_POINT('Ctrl Pts',(4.74177036379677,8.07988231210764,28.9418395133586));
#112729=CARTESIAN_POINT('Ctrl Pts',(4.94391029721191,8.00865437858744,27.685728231694));
#112730=CARTESIAN_POINT('Ctrl Pts',(6.10730855130481,7.93742644506728,27.1707713335208));
#112731=CARTESIAN_POINT('Ctrl Pts',(7.17303400585866,7.86619851154708,27.8656852562957));
#112732=CARTESIAN_POINT('Ctrl Pts',(7.17105782904973,7.79497057802691,29.1379557461679));
#112733=CARTESIAN_POINT('Ctrl Pts',(6.10317874717044,7.72374264450673,29.829555609596));
#112734=CARTESIAN_POINT('Ctrl Pts',(4.94138583499576,7.65251471098655,29.3109870668774));
#112735=CARTESIAN_POINT('Ctrl Pts',(4.74314902188165,7.58128677746636,28.0542538926687));
#112736=CARTESIAN_POINT('Ctrl Pts',(5.68890448308438,7.51005884394619,27.2032411359647));
#112737=CARTESIAN_POINT('Ctrl Pts',(6.91782069527128,7.43883091042601,27.5325450167373));
#112738=CARTESIAN_POINT('Ctrl Pts',(7.3113317555044,7.36760297690582,28.7424314391268));
#112739=CARTESIAN_POINT('Ctrl Pts',(6.51126185297857,7.29637504338565,29.7316555053074));
#112740=CARTESIAN_POINT('Ctrl Pts',(5.24583876792657,7.22514710986546,29.5998203551165));
#112741=CARTESIAN_POINT('Ctrl Pts',(4.66685713370152,7.15391917634529,28.4669230030199));
#112742=CARTESIAN_POINT('Ctrl Pts',(5.30130906693641,7.0826912428251,27.3641325339293));
#112743=CARTESIAN_POINT('Ctrl Pts',(6.57171306646886,7.01146330930493,27.2952144627321));
#112744=CARTESIAN_POINT('Ctrl Pts',(7.32174095171524,6.94023537578474,28.3228985411758));
#112745=CARTESIAN_POINT('Ctrl Pts',(6.86871321357235,6.86900744226456,29.5117810713448));
#112746=CARTESIAN_POINT('Ctrl Pts',(5.62497851648057,6.79777950874438,29.7797356435743));
#112747=CARTESIAN_POINT('Ctrl Pts',(4.72258971300468,6.72655157522421,28.8828673888663));
#112748=CARTESIAN_POINT('Ctrl Pts',(4.98290755008484,6.65532364170402,27.6375128343392));
#112749=CARTESIAN_POINT('Ctrl Pts',(6.16898591290576,6.58409570818384,27.1771954863661));
#112750=CARTESIAN_POINT('Ctrl Pts',(7.20125688966036,6.51286777466366,27.9209076653449));
#112751=CARTESIAN_POINT('Ctrl Pts',(7.14012891627897,6.44163984114348,29.1917009933094));
#112752=CARTESIAN_POINT('Ctrl Pts',(6.04126665064005,6.37041190762329,29.832927276437));
#112753=CARTESIAN_POINT('Ctrl Pts',(4.90481023257615,6.29918397410313,29.2608718577609));
#112754=CARTESIAN_POINT('Ctrl Pts',(4.76526557123557,6.22795604058293,27.9963534041114));
#112755=CARTESIAN_POINT('Ctrl Pts',(5.74945720433682,6.15672810706276,27.1900882226969));
#112756=CARTESIAN_POINT('Ctrl Pts',(6.96193854336298,6.08550017354258,27.576439799063));
#112757=CARTESIAN_POINT('Ctrl Pts',(7.29838144097109,6.01427224002239,28.8027804669918));
#112758=CARTESIAN_POINT('Ctrl Pts',(6.45396995876933,5.94304430650222,29.7547829171801));
#112759=CARTESIAN_POINT('Ctrl Pts',(5.19442066297447,5.87181637298203,29.5621602105904));
#112760=CARTESIAN_POINT('Ctrl Pts',(4.84677637032974,5.82433108396858,28.7929883598607));
#112761=CARTESIAN_POINT('Ctrl Pts',(4.87345388961561,5.80058843946185,28.4195272212344));
#112762=CARTESIAN_POINT('Ctrl Pts',(6.60612943416,11.4494115605381,27.6501793502023));
#112763=CARTESIAN_POINT('Ctrl Pts',(6.8878533552459,11.4256689160314,27.8511172315279));
#112764=CARTESIAN_POINT('Ctrl Pts',(7.23099144335906,11.378183627018,28.5517243931024));
#112765=CARTESIAN_POINT('Ctrl Pts',(6.62641666430548,11.3069556934978,29.5623297027472));
#112766=CARTESIAN_POINT('Ctrl Pts',(5.45102040975077,11.2357277599776,29.6031395771691));
#112767=CARTESIAN_POINT('Ctrl Pts',(4.77564845065076,11.1644998264574,28.6412736177867));
#112768=CARTESIAN_POINT('Ctrl Pts',(5.21451252876542,11.0932718929373,27.550102898212));
#112769=CARTESIAN_POINT('Ctrl Pts',(6.36842129095693,11.0220439594171,27.3239008208275));
#112770=CARTESIAN_POINT('Ctrl Pts',(7.18694492570609,10.9508160258969,28.1680017876497));
#112771=CARTESIAN_POINT('Ctrl Pts',(6.925128831848,10.8795880923767,29.3143860131983));
#112772=CARTESIAN_POINT('Ctrl Pts',(5.8212435183844,10.8083601588565,29.7194621992891));
#112773=CARTESIAN_POINT('Ctrl Pts',(4.88006952391394,10.7371322253364,29.0146030674072));
#112774=CARTESIAN_POINT('Ctrl Pts',(4.95825884824606,10.6659042918161,27.841336469553));
#112775=CARTESIAN_POINT('Ctrl Pts',(5.98464801266528,10.594676358296,27.267595548317));
#112776=CARTESIAN_POINT('Ctrl Pts',(7.02500979116647,10.5234484247758,27.8155920977254));
#112777=CARTESIAN_POINT('Ctrl Pts',(7.13240277903776,10.4522204912556,28.9865420367263));
#112778=CARTESIAN_POINT('Ctrl Pts',(6.20907666627063,10.3809925577354,29.7146379838433));
#112779=CARTESIAN_POINT('Ctrl Pts',(5.09544800251893,10.3097646242153,29.3371646095586));
#112780=CARTESIAN_POINT('Ctrl Pts',(4.80514719610438,10.2385366906951,28.1976994296549));
#112781=CARTESIAN_POINT('Ctrl Pts',(5.60240763421806,10.1673087571749,27.333389918433));
#112782=CARTESIAN_POINT('Ctrl Pts',(6.76155868874716,10.0960808236547,27.5309348863446));
#112783=CARTESIAN_POINT('Ctrl Pts',(7.22753508592282,10.0248528901345,28.610527975269));
#112784=CARTESIAN_POINT('Ctrl Pts',(6.57620268211228,9.95362495661436,29.5895179116725));
#112785=CARTESIAN_POINT('Ctrl Pts',(5.40040761295726,9.88239702309417,29.5768230069675));
#112786=CARTESIAN_POINT('Ctrl Pts',(4.77036464080839,9.811169089574,28.5839982162986));
#112787=CARTESIAN_POINT('Ctrl Pts',(5.2595421457406,9.73994115605382,27.5147178160809));
#112788=CARTESIAN_POINT('Ctrl Pts',(6.42268822676563,9.66871322253363,27.342246364745));
#112789=CARTESIAN_POINT('Ctrl Pts',(7.20110129334866,9.59748528901346,28.2235682728773));
#112790=CARTESIAN_POINT('Ctrl Pts',(6.88626573793482,9.52625735549327,29.3564997713423));
#112791=CARTESIAN_POINT('Ctrl Pts',(5.76474651481203,9.45502942197309,29.7098407392709));
#112792=CARTESIAN_POINT('Ctrl Pts',(4.8573562330907,9.38380148845293,28.9619783962264));
#112793=CARTESIAN_POINT('Ctrl Pts',(4.99000622978019,9.31257355493272,27.7936209227711));
#112794=CARTESIAN_POINT('Ctrl Pts',(6.04195779041892,9.24134562141256,27.2682133462034));
#112795=CARTESIAN_POINT('Ctrl Pts',(7.05571915277443,9.17011768789236,27.8639843656757));
#112796=CARTESIAN_POINT('Ctrl Pts',(7.10855947100084,9.0988897543722,29.0386601116603));
#112797=CARTESIAN_POINT('Ctrl Pts',(6.15238321360516,9.027661820852,29.7230446324044));
#112798=CARTESIAN_POINT('Ctrl Pts',(5.05750696545857,8.95643388733184,29.2942075902946));
#112799=CARTESIAN_POINT('Ctrl Pts',(4.820492761829,8.88520595381164,28.1424786835125));
#112800=CARTESIAN_POINT('Ctrl Pts',(5.65707215918775,8.81397802029147,27.3161675318539));
#112801=CARTESIAN_POINT('Ctrl Pts',(6.80578625447995,8.74275008677129,27.5673868279228));
#112802=CARTESIAN_POINT('Ctrl Pts',(7.22106952495115,8.67152215325111,28.667475466491));
#112803=CARTESIAN_POINT('Ctrl Pts',(6.52492898560981,8.60029421973093,29.6151270675163));
#112804=CARTESIAN_POINT('Ctrl Pts',(5.35099536311798,8.52906628621074,29.5477842325338));
#112805=CARTESIAN_POINT('Ctrl Pts',(4.76778912458761,8.45783835269057,28.5267427589494));
#112806=CARTESIAN_POINT('Ctrl Pts',(5.30614761079969,8.38661041917038,27.4813598875746));
#112807=CARTESIAN_POINT('Ctrl Pts',(6.47605413755724,8.31538248565021,27.3631485256397));
#112808=CARTESIAN_POINT('Ctrl Pts',(7.2126537211558,8.24415455213002,28.2797052674085));
#112809=CARTESIAN_POINT('Ctrl Pts',(6.84548960317178,8.17292661860985,29.3967754164618));
#112810=CARTESIAN_POINT('Ctrl Pts',(5.70875646662365,8.10169868508966,29.6975959339051));
#112811=CARTESIAN_POINT('Ctrl Pts',(4.83711470352825,8.03047075156948,28.9083584257603));
#112812=CARTESIAN_POINT('Ctrl Pts',(5.02393716393983,7.95924281804931,27.7474309621633));
#112813=CARTESIAN_POINT('Ctrl Pts',(6.09917707619303,7.88801488452912,27.2714957370089));
#112814=CARTESIAN_POINT('Ctrl Pts',(7.08414549969642,7.81678695100894,27.9137514587441));
#112815=CARTESIAN_POINT('Ctrl Pts',(7.08231907080919,7.74555901748876,29.0896136410019));
#112816=CARTESIAN_POINT('Ctrl Pts',(6.09536021449545,7.67433108396859,29.7288064314764));
#112817=CARTESIAN_POINT('Ctrl Pts',(5.02160399683884,7.60310315044839,29.2495332398514));
#112818=CARTESIAN_POINT('Ctrl Pts',(4.83838889161733,7.53187521692823,28.0880310086008));
#112819=CARTESIAN_POINT('Ctrl Pts',(5.71247823766805,7.46064728340803,27.3015050888434));
#112820=CARTESIAN_POINT('Ctrl Pts',(6.84827138116787,7.38941934988786,27.6058554474766));
#112821=CARTESIAN_POINT('Ctrl Pts',(7.21196351873741,7.31819141636768,28.724060813584));
#112822=CARTESIAN_POINT('Ctrl Pts',(6.47252017785062,7.24696348284751,29.6383248623537));
#112823=CARTESIAN_POINT('Ctrl Pts',(5.30298652748825,7.17573554932731,29.5164797290777));
#112824=CARTESIAN_POINT('Ctrl Pts',(4.76787814186861,7.10450761580714,28.4694294647551));
#112825=CARTESIAN_POINT('Ctrl Pts',(5.35425347690147,7.03327968228695,27.4502046867851));
#112826=CARTESIAN_POINT('Ctrl Pts',(6.52839060507555,6.96205174876678,27.3865089913807));
#112827=CARTESIAN_POINT('Ctrl Pts',(7.22158394165021,6.89082381524659,28.3363186841856));
#112828=CARTESIAN_POINT('Ctrl Pts',(6.80288509652527,6.81959588172642,29.435111761209));
#112829=CARTESIAN_POINT('Ctrl Pts',(5.65339636223977,6.74836794820623,29.6827616521368));
#112830=CARTESIAN_POINT('Ctrl Pts',(4.81938749687129,6.67714001468605,28.8538550072264));
#112831=CARTESIAN_POINT('Ctrl Pts',(5.05997933832825,6.60591208116587,27.7028691627634));
#112832=CARTESIAN_POINT('Ctrl Pts',(6.15618073821719,6.5346841476457,27.2774330895168));
#112833=CARTESIAN_POINT('Ctrl Pts',(7.11022974986244,6.46345621412551,27.9647893024504));
#112834=CARTESIAN_POINT('Ctrl Pts',(7.05373384529701,6.39222828060534,29.1392862570791));
#112835=CARTESIAN_POINT('Ctrl Pts',(6.0381396049522,6.32100034708515,29.7319226049325));
#112836=CARTESIAN_POINT('Ctrl Pts',(4.98779996851242,6.24977241356497,29.2032155899294));
#112837=CARTESIAN_POINT('Ctrl Pts',(4.85882952448143,6.17854448004479,28.034518021095));
#112838=CARTESIAN_POINT('Ctrl Pts',(5.76844248074397,6.10731654652461,27.289348858371));
#112839=CARTESIAN_POINT('Ctrl Pts',(6.88904612957757,6.03608861300443,27.6464240332814));
#112840=CARTESIAN_POINT('Ctrl Pts',(7.19999453476011,5.96486067948425,28.7798367984608));
#112841=CARTESIAN_POINT('Ctrl Pts',(6.41956966749388,5.89363274596407,29.6596997580312));
#112842=CARTESIAN_POINT('Ctrl Pts',(5.25546471072222,5.82240481244388,29.4816733415374));
#112843=CARTESIAN_POINT('Ctrl Pts',(4.93416371391945,5.77491952343044,28.7707867037272));
#112844=CARTESIAN_POINT('Ctrl Pts',(4.95881970200879,5.75117687892371,28.4256251732592));
#112845=CARTESIAN_POINT('Ctrl Pts',(6.55643320799984,11.4,27.719855688007));
#112846=CARTESIAN_POINT('Ctrl Pts',(6.81505873638613,11.3762573554933,27.9043187805636));
#112847=CARTESIAN_POINT('Ctrl Pts',(7.13006311729091,11.3287720664798,28.5474835379439));
#112848=CARTESIAN_POINT('Ctrl Pts',(6.57505709906184,11.2575441329596,29.4752298620382));
#112849=CARTESIAN_POINT('Ctrl Pts',(5.49603095095993,11.1863161994395,29.5126937568152));
#112850=CARTESIAN_POINT('Ctrl Pts',(4.87603237538185,11.1150882659193,28.629690669881));
#112851=CARTESIAN_POINT('Ctrl Pts',(5.27891422387623,11.0438603323991,27.6279844504662));
#112852=CARTESIAN_POINT('Ctrl Pts',(6.3382146275518,10.9726323988789,27.4203285596915));
#112853=CARTESIAN_POINT('Ctrl Pts',(7.08962794991972,10.9014044653588,28.1952221424384));
#112854=CARTESIAN_POINT('Ctrl Pts',(6.84927801671883,10.8301765318385,29.2476149421817));
#112855=CARTESIAN_POINT('Ctrl Pts',(5.83589966612663,10.7589485983184,29.6194791497386));
#112856=CARTESIAN_POINT('Ctrl Pts',(4.97189202103516,10.6877206647982,28.9724110388085));
#112857=CARTESIAN_POINT('Ctrl Pts',(5.04367064473747,10.616492731278,27.8953399380002));
#112858=CARTESIAN_POINT('Ctrl Pts',(5.98590671384625,10.5452647977578,27.3686397261773));
#112859=CARTESIAN_POINT('Ctrl Pts',(6.94096978992682,10.4740368642377,27.8717063333662));
#112860=CARTESIAN_POINT('Ctrl Pts',(7.03955768450863,10.4028089307175,28.9466507169341));
#112861=CARTESIAN_POINT('Ctrl Pts',(6.19193458290324,10.3315809971973,29.6150504691213));
#112862=CARTESIAN_POINT('Ctrl Pts',(5.16961173407035,10.2603530636771,29.2685259336831));
#112863=CARTESIAN_POINT('Ctrl Pts',(4.90311253456843,10.1891251301569,28.2224848907553));
#112864=CARTESIAN_POINT('Ctrl Pts',(5.63500601835172,10.1178971966368,27.4290396512902));
#112865=CARTESIAN_POINT('Ctrl Pts',(6.69911890163688,10.0466692631166,27.6103880135778));
#112866=CARTESIAN_POINT('Ctrl Pts',(7.12689014474107,9.97544132959639,28.6014658460497));
#112867=CARTESIAN_POINT('Ctrl Pts',(6.52896013424947,9.9042133960762,29.5001889243431));
#112868=CARTESIAN_POINT('Ctrl Pts',(5.44956787014175,9.83298546255604,29.4885348680441));
#112869=CARTESIAN_POINT('Ctrl Pts',(4.87118178226534,9.76175752903585,28.5771112477421));
#112870=CARTESIAN_POINT('Ctrl Pts',(5.32025188678519,9.69052959551568,27.595500572179));
#112871=CARTESIAN_POINT('Ctrl Pts',(6.38803224649353,9.61930166199549,27.4371699623346));
#112872=CARTESIAN_POINT('Ctrl Pts',(7.10262364459654,9.54807372847531,28.2462327614415));
#112873=CARTESIAN_POINT('Ctrl Pts',(6.8136012869641,9.47684579495514,29.286275815956));
#112874=CARTESIAN_POINT('Ctrl Pts',(5.78403482147721,9.40561786143493,29.6106465480502));
#112875=CARTESIAN_POINT('Ctrl Pts',(4.95104098070492,9.33438992791478,28.9241010361015));
#112876=CARTESIAN_POINT('Ctrl Pts',(5.07281507554227,9.26316199439458,27.8515365632241));
#112877=CARTESIAN_POINT('Ctrl Pts',(6.03851769375916,9.19193406087441,27.3692068711474));
#112878=CARTESIAN_POINT('Ctrl Pts',(6.96916130750066,9.12070612735422,27.9161309453062));
#112879=CARTESIAN_POINT('Ctrl Pts',(7.01766927646803,9.04947819383405,28.9944956589479));
#112880=CARTESIAN_POINT('Ctrl Pts',(6.13988939591615,8.97825026031386,29.6227678610904));
#112881=CARTESIAN_POINT('Ctrl Pts',(5.13478146222322,8.90702232679369,29.2290909373142));
#112882=CARTESIAN_POINT('Ctrl Pts',(4.91719992561646,8.8357943932735,28.1717916638759));
#112883=CARTESIAN_POINT('Ctrl Pts',(5.68518862833307,8.76456645975332,27.4132293189198));
#112884=CARTESIAN_POINT('Ctrl Pts',(6.73972027305326,8.69333852623316,27.6438512800801));
#112885=CARTESIAN_POINT('Ctrl Pts',(7.12095469163445,8.62211059271294,28.6537442431088));
#112886=CARTESIAN_POINT('Ctrl Pts',(6.48189034053387,8.5508826591928,29.5236983992791));
#112887=CARTESIAN_POINT('Ctrl Pts',(5.40420690407899,8.47965472567259,29.4618769671009));
#112888=CARTESIAN_POINT('Ctrl Pts',(4.86881743123368,8.40842679215243,28.5245501345329));
#112889=CARTESIAN_POINT('Ctrl Pts',(5.36303619484158,8.33719885863223,27.5648776422817));
#112890=CARTESIAN_POINT('Ctrl Pts',(6.43702271497452,8.26597092511206,27.4563583663045));
#112891=CARTESIAN_POINT('Ctrl Pts',(7.11322889506391,8.19474299159188,28.2977671139973));
#112892=CARTESIAN_POINT('Ctrl Pts',(6.77616836554943,8.1235150580717,29.3232492826038));
#112893=CARTESIAN_POINT('Ctrl Pts',(5.73263536721262,8.05228712455152,29.5994056876876));
#112894=CARTESIAN_POINT('Ctrl Pts',(4.93245904325973,7.98105919103134,28.874877338162));
#112895=CARTESIAN_POINT('Ctrl Pts',(5.10396403066773,7.90983125751116,27.8091336926326));
#112896=CARTESIAN_POINT('Ctrl Pts',(6.09104560108126,7.83860332399098,27.372220140497));
#112897=CARTESIAN_POINT('Ctrl Pts',(6.99525699353418,7.76737539047079,27.9618176611926));
#112898=CARTESIAN_POINT('Ctrl Pts',(6.99358031256864,7.69614745695062,29.041271535836));
#112899=CARTESIAN_POINT('Ctrl Pts',(6.08754168182046,7.62491952343044,29.6280572533568));
#112900=CARTESIAN_POINT('Ctrl Pts',(5.10182215868192,7.55369158991026,29.1880794128254));
#112901=CARTESIAN_POINT('Ctrl Pts',(4.933628761353,7.48246365639008,28.1218081245331));
#112902=CARTESIAN_POINT('Ctrl Pts',(5.73605199225171,7.41123572286989,27.399769041722));
#112903=CARTESIAN_POINT('Ctrl Pts',(6.77872206706446,7.34000778934971,27.679165878216));
#112904=CARTESIAN_POINT('Ctrl Pts',(7.11259528197041,7.26877985582954,28.705690188041));
#112905=CARTESIAN_POINT('Ctrl Pts',(6.43377850272267,7.19755192230935,29.5449942194001));
#112906=CARTESIAN_POINT('Ctrl Pts',(5.36013428704992,7.12632398878918,29.4331391030388));
#112907=CARTESIAN_POINT('Ctrl Pts',(4.86889915003569,7.05509605526898,28.4719359264905));
#112908=CARTESIAN_POINT('Ctrl Pts',(5.40719788686653,6.98386812174881,27.5362768396409));
#112909=CARTESIAN_POINT('Ctrl Pts',(6.48506814368224,6.91264018822863,27.4778035200293));
#112910=CARTESIAN_POINT('Ctrl Pts',(7.12142693158516,6.84141225470845,28.3497388271955));
#112911=CARTESIAN_POINT('Ctrl Pts',(6.73705697947822,6.77018432118827,29.3584424510732));
#112912=CARTESIAN_POINT('Ctrl Pts',(5.68181420799896,6.6989563876681,29.5857876606995));
#112913=CARTESIAN_POINT('Ctrl Pts',(4.9161852807379,6.6277284541479,28.8248426255865));
#112914=CARTESIAN_POINT('Ctrl Pts',(5.13705112657166,6.55650052062773,27.7682254911877));
#112915=CARTESIAN_POINT('Ctrl Pts',(6.14337556352862,6.48527258710754,27.3776706926676));
#112916=CARTESIAN_POINT('Ctrl Pts',(7.01920261006453,6.41404465358737,28.0086709395559));
#112917=CARTESIAN_POINT('Ctrl Pts',(6.96733877431504,6.34281672006719,29.0868715208489));
#112918=CARTESIAN_POINT('Ctrl Pts',(6.03501255926435,6.271588786547,29.630917933428));
#112919=CARTESIAN_POINT('Ctrl Pts',(5.07078970444869,6.20036085302683,29.1455593220979));
#112920=CARTESIAN_POINT('Ctrl Pts',(4.95239347772729,6.12913291950664,28.0726826380785));
#112921=CARTESIAN_POINT('Ctrl Pts',(5.78742775715113,6.05790498598646,27.388609494045));
#112922=CARTESIAN_POINT('Ctrl Pts',(6.81615371579216,5.98667705246629,27.7164082674999));
#112923=CARTESIAN_POINT('Ctrl Pts',(7.10160762854914,5.9154491189461,28.7568931299298));
#112924=CARTESIAN_POINT('Ctrl Pts',(6.38516937621842,5.84422118542593,29.5646165988824));
#112925=CARTESIAN_POINT('Ctrl Pts',(5.31650875846996,5.77299325190574,29.4011864724843));
#112926=CARTESIAN_POINT('Ctrl Pts',(5.02155105750916,5.72550796289229,28.7485850475937));
#112927=CARTESIAN_POINT('Ctrl Pts',(5.04418551440197,5.70176531838556,28.431723125284));
#112928=CARTESIAN_POINT('Ctrl Pts',(4.78808807722243,5.85,28.4134292692097));
#112929=CARTESIAN_POINT('Ctrl Pts',(4.78603023160016,5.85170244995002,28.4422372464798));
#112930=CARTESIAN_POINT('Ctrl Pts',(4.78508137249078,5.85340489990004,28.4711067562139));
#112931=CARTESIAN_POINT('Ctrl Pts',(4.78521076863826,5.85510734985006,28.4999698544854));
#112932=CARTESIAN_POINT('Origin',(6.,11.4,28.5));
#112933=CARTESIAN_POINT('',(6.,11.5,27.185));
#112934=CARTESIAN_POINT('Origin',(6.,11.4,27.185));
#112935=CARTESIAN_POINT('Origin',(6.,11.5,28.5));
#112936=CARTESIAN_POINT('Origin',(6.,11.5,28.5));
#112937=CARTESIAN_POINT('Origin',(6.,5.85,28.5));
#112938=CARTESIAN_POINT('Origin',(6.,11.5,28.5));
#112939=CARTESIAN_POINT('',(6.,11.5,26.45));
#112940=CARTESIAN_POINT('Origin',(6.,11.5,28.5));
#112941=CARTESIAN_POINT('Origin',(6.,5.675,28.5));
#112942=CARTESIAN_POINT('',(5.135,5.5,28.5));
#112943=CARTESIAN_POINT('',(4.96,5.675,28.5));
#112944=CARTESIAN_POINT('Origin',(6.,5.5,28.5));
#112945=CARTESIAN_POINT('Origin',(6.,5.5,28.5));
#112946=CARTESIAN_POINT('Origin',(8.06809628132564,14.,28.1353388268994));
#112947=CARTESIAN_POINT('',(8.06809628132564,13.85,28.1353388268994));
#112948=CARTESIAN_POINT('',(8.20597752546084,13.7,28.0570968986768));
#112949=CARTESIAN_POINT('Ctrl Pts',(8.06809628132564,13.85,28.1353388268994));
#112950=CARTESIAN_POINT('Ctrl Pts',(8.13465964056348,13.7778888548063,28.0975668615505));
#112951=CARTESIAN_POINT('Ctrl Pts',(8.20597752546084,13.7,28.0570968986768));
#112952=CARTESIAN_POINT('',(8.06809628132564,12.1,28.1353388268994));
#112953=CARTESIAN_POINT('',(8.06809628132564,14.,28.1353388268994));
#112954=CARTESIAN_POINT('',(8.20597752546084,12.1,28.0570968986768));
#112955=CARTESIAN_POINT('',(8.06809628132564,12.1,28.1353388268994));
#112956=CARTESIAN_POINT('',(8.20597752546084,11.5,28.0570968986768));
#112957=CARTESIAN_POINT('Origin',(8.28967802575338,12.1,28.0962679869244));
#112958=CARTESIAN_POINT('',(8.22442258448904,12.1,28.1617040266052));
#112959=CARTESIAN_POINT('Origin',(6.,12.1,28.5));
#112960=CARTESIAN_POINT('',(8.53904347860784,12.1,28.2147663874313));
#112961=CARTESIAN_POINT('Origin',(8.53904347860784,14.,28.2147663874313));
#112962=CARTESIAN_POINT('',(8.22442258448904,13.7,28.1617040266052));
#112963=CARTESIAN_POINT('Ctrl Pts',(8.22442258448904,13.7,28.1617040266052));
#112964=CARTESIAN_POINT('Ctrl Pts',(8.14356415181841,13.7778888548064,28.1480668543436));
#112965=CARTESIAN_POINT('Ctrl Pts',(8.06809628132564,13.85,28.1353388268994));
#112966=CARTESIAN_POINT('',(8.22442258448904,11.5,28.1617040266052));
#112967=CARTESIAN_POINT('Origin',(6.,11.5,28.5));
#112968=CARTESIAN_POINT('',(8.24937308647232,13.7,28.4468895692543));
#112969=CARTESIAN_POINT('Origin',(6.,13.7,28.5));
#112970=CARTESIAN_POINT('',(8.24937308647232,12.1,28.4468895692543));
#112971=CARTESIAN_POINT('',(8.24937308647232,11.5,28.4468895692543));
#112972=CARTESIAN_POINT('',(8.24937308647232,12.1,28.5531104307457));
#112973=CARTESIAN_POINT('Origin',(6.,12.1,28.5));
#112974=CARTESIAN_POINT('',(8.24937308647232,13.7,28.5531104307457));
#112975=CARTESIAN_POINT('',(8.24937308647232,11.5,28.5531104307457));
#112976=CARTESIAN_POINT('',(8.22442258448904,13.7,28.8382959733948));
#112977=CARTESIAN_POINT('Origin',(6.,13.7,28.5));
#112978=CARTESIAN_POINT('',(8.22442258448904,12.1,28.8382959733948));
#112979=CARTESIAN_POINT('',(8.22442258448904,11.5,28.8382959733948));
#112980=CARTESIAN_POINT('',(8.20597752546084,12.1,28.9429031013232));
#112981=CARTESIAN_POINT('Origin',(6.,12.1,28.5));
#112982=CARTESIAN_POINT('',(8.20597752546084,13.7,28.9429031013232));
#112983=CARTESIAN_POINT('',(8.20597752546084,11.5,28.9429031013232));
#112984=CARTESIAN_POINT('',(8.1318841278882,13.7,29.2194234255697));
#112985=CARTESIAN_POINT('Origin',(6.,13.7,28.5));
#112986=CARTESIAN_POINT('',(8.1318841278882,12.1,29.2194234255697));
#112987=CARTESIAN_POINT('',(8.1318841278882,11.5,29.2194234255697));
#112988=CARTESIAN_POINT('',(8.09555445361672,12.1,29.3192383852867));
#112989=CARTESIAN_POINT('Origin',(6.,12.1,28.5));
#112990=CARTESIAN_POINT('',(8.09555445361672,13.7,29.3192383852867));
#112991=CARTESIAN_POINT('',(8.09555445361672,11.5,29.3192383852867));
#112992=CARTESIAN_POINT('',(7.97456945084689,13.7,29.5786915610044));
#112993=CARTESIAN_POINT('Origin',(6.,13.7,28.5));
#112994=CARTESIAN_POINT('',(7.97456945084689,12.1,29.5786915610044));
#112995=CARTESIAN_POINT('',(7.97456945084689,11.5,29.5786915610044));
#112996=CARTESIAN_POINT('',(7.92145902010118,12.1,29.6706815254679));
#112997=CARTESIAN_POINT('Origin',(6.,12.1,28.5));
#112998=CARTESIAN_POINT('',(7.92145902010118,13.7,29.6706815254679));
#112999=CARTESIAN_POINT('',(7.92145902010118,11.5,29.6706815254679));
#113000=CARTESIAN_POINT('',(7.75725848022197,13.7,29.9051841992024));
#113001=CARTESIAN_POINT('Origin',(6.,13.7,28.5));
#113002=CARTESIAN_POINT('',(7.75725848022197,12.1,29.9051841992024));
#113003=CARTESIAN_POINT('',(7.75725848022197,11.5,29.9051841992024));
#113004=CARTESIAN_POINT('',(7.68898102656505,12.1,29.9865540998912));
#113005=CARTESIAN_POINT('Origin',(6.,12.1,28.5));
#113006=CARTESIAN_POINT('',(7.68898102656505,13.7,29.9865540998912));
#113007=CARTESIAN_POINT('',(7.68898102656505,11.5,29.9865540998912));
#113008=CARTESIAN_POINT('',(7.48655409989118,13.7,30.188981026565));
#113009=CARTESIAN_POINT('Origin',(6.,13.7,28.5));
#113010=CARTESIAN_POINT('',(7.48655409989118,12.1,30.188981026565));
#113011=CARTESIAN_POINT('',(7.48655409989118,11.5,30.188981026565));
#113012=CARTESIAN_POINT('',(7.40518419920237,12.1,30.257258480222));
#113013=CARTESIAN_POINT('Origin',(6.,12.1,28.5));
#113014=CARTESIAN_POINT('',(7.40518419920237,13.7,30.257258480222));
#113015=CARTESIAN_POINT('',(7.40518419920237,11.5,30.257258480222));
#113016=CARTESIAN_POINT('',(7.17068152546788,13.7,30.4214590201012));
#113017=CARTESIAN_POINT('Origin',(6.,13.7,28.5));
#113018=CARTESIAN_POINT('',(7.17068152546788,12.1,30.4214590201012));
#113019=CARTESIAN_POINT('',(7.17068152546788,11.5,30.4214590201012));
#113020=CARTESIAN_POINT('',(7.07869156100444,12.1,30.4745694508469));
#113021=CARTESIAN_POINT('Origin',(6.,12.1,28.5));
#113022=CARTESIAN_POINT('',(7.07869156100444,13.7,30.4745694508469));
#113023=CARTESIAN_POINT('',(7.07869156100444,11.5,30.4745694508469));
#113024=CARTESIAN_POINT('',(6.81923838528667,13.7,30.5955544536167));
#113025=CARTESIAN_POINT('Origin',(6.,13.7,28.5));
#113026=CARTESIAN_POINT('',(6.81923838528667,12.1,30.5955544536167));
#113027=CARTESIAN_POINT('',(6.81923838528667,11.5,30.5955544536167));
#113028=CARTESIAN_POINT('',(6.71942342556966,12.1,30.6318841278882));
#113029=CARTESIAN_POINT('Origin',(6.,12.1,28.5));
#113030=CARTESIAN_POINT('',(6.71942342556966,13.7,30.6318841278882));
#113031=CARTESIAN_POINT('',(6.71942342556966,11.5,30.6318841278882));
#113032=CARTESIAN_POINT('',(6.44290310132316,13.7,30.7059775254608));
#113033=CARTESIAN_POINT('Origin',(6.,13.7,28.5));
#113034=CARTESIAN_POINT('',(6.44290310132316,12.1,30.7059775254608));
#113035=CARTESIAN_POINT('',(6.44290310132316,11.5,30.7059775254608));
#113036=CARTESIAN_POINT('',(6.33829597339476,12.1,30.724422584489));
#113037=CARTESIAN_POINT('Origin',(6.,12.1,28.5));
#113038=CARTESIAN_POINT('',(6.33829597339476,13.7,30.724422584489));
#113039=CARTESIAN_POINT('',(6.33829597339476,11.5,30.724422584489));
#113040=CARTESIAN_POINT('',(6.05311043074571,13.7,30.7493730864723));
#113041=CARTESIAN_POINT('Origin',(6.,13.7,28.5));
#113042=CARTESIAN_POINT('',(6.05311043074571,12.1,30.7493730864723));
#113043=CARTESIAN_POINT('',(6.05311043074571,11.5,30.7493730864723));
#113044=CARTESIAN_POINT('',(5.94688956925429,12.1,30.7493730864723));
#113045=CARTESIAN_POINT('Origin',(6.,12.1,28.5));
#113046=CARTESIAN_POINT('',(5.94688956925429,13.7,30.7493730864723));
#113047=CARTESIAN_POINT('',(5.94688956925429,11.5,30.7493730864723));
#113048=CARTESIAN_POINT('',(5.66170402660524,13.7,30.724422584489));
#113049=CARTESIAN_POINT('Origin',(6.,13.7,28.5));
#113050=CARTESIAN_POINT('',(5.66170402660524,12.1,30.724422584489));
#113051=CARTESIAN_POINT('',(5.66170402660524,11.5,30.724422584489));
#113052=CARTESIAN_POINT('',(5.55709689867685,12.1,30.7059775254608));
#113053=CARTESIAN_POINT('Origin',(6.,12.1,28.5));
#113054=CARTESIAN_POINT('',(5.55709689867685,13.7,30.7059775254608));
#113055=CARTESIAN_POINT('',(5.55709689867685,11.5,30.7059775254608));
#113056=CARTESIAN_POINT('',(5.28057657443035,13.7,30.6318841278882));
#113057=CARTESIAN_POINT('Origin',(6.,13.7,28.5));
#113058=CARTESIAN_POINT('',(5.28057657443035,12.1,30.6318841278882));
#113059=CARTESIAN_POINT('',(5.28057657443035,11.5,30.6318841278882));
#113060=CARTESIAN_POINT('',(5.18076161471333,12.1,30.5955544536167));
#113061=CARTESIAN_POINT('Origin',(6.,12.1,28.5));
#113062=CARTESIAN_POINT('',(5.18076161471333,13.7,30.5955544536167));
#113063=CARTESIAN_POINT('',(5.18076161471333,11.5,30.5955544536167));
#113064=CARTESIAN_POINT('',(4.92130843899556,13.7,30.4745694508469));
#113065=CARTESIAN_POINT('Origin',(6.,13.7,28.5));
#113066=CARTESIAN_POINT('',(4.92130843899556,12.1,30.4745694508469));
#113067=CARTESIAN_POINT('',(4.92130843899556,11.5,30.4745694508469));
#113068=CARTESIAN_POINT('',(4.82931847453212,12.1,30.4214590201012));
#113069=CARTESIAN_POINT('Origin',(6.,12.1,28.5));
#113070=CARTESIAN_POINT('',(4.82931847453212,13.7,30.4214590201012));
#113071=CARTESIAN_POINT('',(4.82931847453212,11.5,30.4214590201012));
#113072=CARTESIAN_POINT('',(4.59481580079764,13.7,30.257258480222));
#113073=CARTESIAN_POINT('Origin',(6.,13.7,28.5));
#113074=CARTESIAN_POINT('',(4.59481580079764,12.1,30.257258480222));
#113075=CARTESIAN_POINT('',(4.59481580079764,11.5,30.257258480222));
#113076=CARTESIAN_POINT('',(4.51344590010882,12.1,30.188981026565));
#113077=CARTESIAN_POINT('Origin',(6.,12.1,28.5));
#113078=CARTESIAN_POINT('',(4.51344590010882,13.7,30.188981026565));
#113079=CARTESIAN_POINT('',(4.51344590010882,11.5,30.188981026565));
#113080=CARTESIAN_POINT('',(4.31101897343496,13.7,29.9865540998912));
#113081=CARTESIAN_POINT('Origin',(6.,13.7,28.5));
#113082=CARTESIAN_POINT('',(4.31101897343496,12.1,29.9865540998912));
#113083=CARTESIAN_POINT('',(4.31101897343496,11.5,29.9865540998912));
#113084=CARTESIAN_POINT('',(4.24274151977804,12.1,29.9051841992024));
#113085=CARTESIAN_POINT('Origin',(6.,12.1,28.5));
#113086=CARTESIAN_POINT('',(4.24274151977804,13.7,29.9051841992024));
#113087=CARTESIAN_POINT('',(4.24274151977804,11.5,29.9051841992024));
#113088=CARTESIAN_POINT('',(4.07854097989882,13.7,29.6706815254679));
#113089=CARTESIAN_POINT('Origin',(6.,13.7,28.5));
#113090=CARTESIAN_POINT('',(4.07854097989882,12.1,29.6706815254679));
#113091=CARTESIAN_POINT('',(4.07854097989882,11.5,29.6706815254679));
#113092=CARTESIAN_POINT('',(4.0254305491531,12.1,29.5786915610044));
#113093=CARTESIAN_POINT('Origin',(6.,12.1,28.5));
#113094=CARTESIAN_POINT('',(4.0254305491531,13.7,29.5786915610044));
#113095=CARTESIAN_POINT('',(4.0254305491531,11.5,29.5786915610044));
#113096=CARTESIAN_POINT('',(3.90444554638328,13.7,29.3192383852867));
#113097=CARTESIAN_POINT('Origin',(6.,13.7,28.5));
#113098=CARTESIAN_POINT('',(3.90444554638328,12.1,29.3192383852867));
#113099=CARTESIAN_POINT('',(3.90444554638328,11.5,29.3192383852867));
#113100=CARTESIAN_POINT('',(3.8681158721118,12.1,29.2194234255697));
#113101=CARTESIAN_POINT('Origin',(6.,12.1,28.5));
#113102=CARTESIAN_POINT('',(3.8681158721118,13.7,29.2194234255697));
#113103=CARTESIAN_POINT('',(3.8681158721118,11.5,29.2194234255697));
#113104=CARTESIAN_POINT('',(3.79402247453916,13.7,28.9429031013232));
#113105=CARTESIAN_POINT('Origin',(6.,13.7,28.5));
#113106=CARTESIAN_POINT('',(3.79402247453916,12.1,28.9429031013232));
#113107=CARTESIAN_POINT('',(3.79402247453916,11.5,28.9429031013232));
#113108=CARTESIAN_POINT('',(3.77557741551096,12.1,28.8382959733948));
#113109=CARTESIAN_POINT('Origin',(6.,12.1,28.5));
#113110=CARTESIAN_POINT('',(3.77557741551096,13.7,28.8382959733948));
#113111=CARTESIAN_POINT('',(3.77557741551096,11.5,28.8382959733948));
#113112=CARTESIAN_POINT('',(3.75062691352768,13.7,28.5531104307457));
#113113=CARTESIAN_POINT('Origin',(6.,13.7,28.5));
#113114=CARTESIAN_POINT('',(3.75062691352768,12.1,28.5531104307457));
#113115=CARTESIAN_POINT('',(3.75062691352768,11.5,28.5531104307457));
#113116=CARTESIAN_POINT('',(3.75,12.1,28.5));
#113117=CARTESIAN_POINT('Origin',(6.,12.1,28.5));
#113118=CARTESIAN_POINT('',(3.75,11.7,28.5));
#113119=CARTESIAN_POINT('',(3.75,11.5,28.5));
#113120=CARTESIAN_POINT('',(6.,11.7,26.25));
#113121=CARTESIAN_POINT('Origin',(6.,11.7,28.5));
#113122=CARTESIAN_POINT('Origin',(6.,11.7,28.5));
#113123=CARTESIAN_POINT('',(3.75062691352768,12.1,28.4468895692543));
#113124=CARTESIAN_POINT('Origin',(6.,12.1,28.5));
#113125=CARTESIAN_POINT('',(3.75062691352768,13.7,28.4468895692543));
#113126=CARTESIAN_POINT('',(3.75062691352768,11.5,28.4468895692543));
#113127=CARTESIAN_POINT('',(3.77557741551096,13.7,28.1617040266052));
#113128=CARTESIAN_POINT('Origin',(6.,13.7,28.5));
#113129=CARTESIAN_POINT('',(3.77557741551096,12.1,28.1617040266052));
#113130=CARTESIAN_POINT('',(3.77557741551096,11.5,28.1617040266052));
#113131=CARTESIAN_POINT('',(3.79402247453916,12.1,28.0570968986769));
#113132=CARTESIAN_POINT('Origin',(6.,12.1,28.5));
#113133=CARTESIAN_POINT('',(3.79402247453916,13.7,28.0570968986769));
#113134=CARTESIAN_POINT('',(3.79402247453916,11.5,28.0570968986769));
#113135=CARTESIAN_POINT('',(3.8681158721118,13.7,27.7805765744303));
#113136=CARTESIAN_POINT('Origin',(6.,13.7,28.5));
#113137=CARTESIAN_POINT('',(3.8681158721118,12.1,27.7805765744303));
#113138=CARTESIAN_POINT('',(3.8681158721118,11.5,27.7805765744303));
#113139=CARTESIAN_POINT('',(3.90444554638328,12.1,27.6807616147133));
#113140=CARTESIAN_POINT('Origin',(6.,12.1,28.5));
#113141=CARTESIAN_POINT('',(3.90444554638328,13.7,27.6807616147133));
#113142=CARTESIAN_POINT('',(3.90444554638328,11.5,27.6807616147133));
#113143=CARTESIAN_POINT('',(4.0254305491531,13.7,27.4213084389956));
#113144=CARTESIAN_POINT('Origin',(6.,13.7,28.5));
#113145=CARTESIAN_POINT('',(4.0254305491531,12.1,27.4213084389956));
#113146=CARTESIAN_POINT('',(4.0254305491531,11.5,27.4213084389956));
#113147=CARTESIAN_POINT('',(4.07854097989881,12.1,27.3293184745321));
#113148=CARTESIAN_POINT('Origin',(6.,12.1,28.5));
#113149=CARTESIAN_POINT('',(4.07854097989881,13.7,27.3293184745321));
#113150=CARTESIAN_POINT('',(4.07854097989881,11.5,27.3293184745321));
#113151=CARTESIAN_POINT('',(4.24274151977803,13.7,27.0948158007976));
#113152=CARTESIAN_POINT('Origin',(6.,13.7,28.5));
#113153=CARTESIAN_POINT('',(4.24274151977803,12.1,27.0948158007976));
#113154=CARTESIAN_POINT('',(4.24274151977803,11.5,27.0948158007976));
#113155=CARTESIAN_POINT('',(4.31101897343496,12.1,27.0134459001088));
#113156=CARTESIAN_POINT('Origin',(6.,12.1,28.5));
#113157=CARTESIAN_POINT('',(4.31101897343495,13.7,27.0134459001088));
#113158=CARTESIAN_POINT('',(4.31101897343495,11.5,27.0134459001088));
#113159=CARTESIAN_POINT('',(4.51344590010881,13.7,26.811018973435));
#113160=CARTESIAN_POINT('Origin',(6.,13.7,28.5));
#113161=CARTESIAN_POINT('',(4.51344590010881,12.1,26.811018973435));
#113162=CARTESIAN_POINT('',(4.51344590010881,11.5,26.811018973435));
#113163=CARTESIAN_POINT('',(4.59481580079763,12.1,26.742741519778));
#113164=CARTESIAN_POINT('Origin',(6.,12.1,28.5));
#113165=CARTESIAN_POINT('',(4.59481580079763,13.7,26.742741519778));
#113166=CARTESIAN_POINT('',(4.59481580079763,11.5,26.742741519778));
#113167=CARTESIAN_POINT('',(4.82931847453212,13.7,26.5785409798988));
#113168=CARTESIAN_POINT('Origin',(6.,13.7,28.5));
#113169=CARTESIAN_POINT('',(4.82931847453212,12.1,26.5785409798988));
#113170=CARTESIAN_POINT('',(4.82931847453212,11.5,26.5785409798988));
#113171=CARTESIAN_POINT('',(4.92130843899556,12.1,26.5254305491531));
#113172=CARTESIAN_POINT('Origin',(6.,12.1,28.5));
#113173=CARTESIAN_POINT('',(4.92130843899556,13.7,26.5254305491531));
#113174=CARTESIAN_POINT('',(4.92130843899556,11.5,26.5254305491531));
#113175=CARTESIAN_POINT('',(5.18076161471333,13.7,26.4044455463833));
#113176=CARTESIAN_POINT('Origin',(6.,13.7,28.5));
#113177=CARTESIAN_POINT('',(5.18076161471333,12.1,26.4044455463833));
#113178=CARTESIAN_POINT('',(5.18076161471333,11.5,26.4044455463833));
#113179=CARTESIAN_POINT('',(5.28057657443034,12.1,26.3681158721118));
#113180=CARTESIAN_POINT('Origin',(6.,12.1,28.5));
#113181=CARTESIAN_POINT('',(5.28057657443034,13.7,26.3681158721118));
#113182=CARTESIAN_POINT('',(5.28057657443034,11.5,26.3681158721118));
#113183=CARTESIAN_POINT('',(5.55709689867685,13.7,26.2940224745392));
#113184=CARTESIAN_POINT('Origin',(6.,13.7,28.5));
#113185=CARTESIAN_POINT('',(5.55709689867685,12.1,26.2940224745392));
#113186=CARTESIAN_POINT('',(5.55709689867685,11.5,26.2940224745392));
#113187=CARTESIAN_POINT('',(5.66170402660524,12.1,26.275577415511));
#113188=CARTESIAN_POINT('Origin',(6.,12.1,28.5));
#113189=CARTESIAN_POINT('',(5.66170402660524,13.7,26.275577415511));
#113190=CARTESIAN_POINT('',(5.66170402660524,11.5,26.275577415511));
#113191=CARTESIAN_POINT('',(5.94688956925429,13.7,26.2506269135277));
#113192=CARTESIAN_POINT('Origin',(6.,13.7,28.5));
#113193=CARTESIAN_POINT('',(5.94688956925429,12.1,26.2506269135277));
#113194=CARTESIAN_POINT('',(5.94688956925429,11.5,26.2506269135277));
#113195=CARTESIAN_POINT('',(6.05311043074571,12.1,26.2506269135277));
#113196=CARTESIAN_POINT('Origin',(6.,12.1,28.5));
#113197=CARTESIAN_POINT('',(6.05311043074571,13.7,26.2506269135277));
#113198=CARTESIAN_POINT('',(6.05311043074571,11.5,26.2506269135277));
#113199=CARTESIAN_POINT('',(6.33829597339476,13.7,26.275577415511));
#113200=CARTESIAN_POINT('Origin',(6.,13.7,28.5));
#113201=CARTESIAN_POINT('',(6.33829597339476,12.1,26.275577415511));
#113202=CARTESIAN_POINT('',(6.33829597339476,11.5,26.275577415511));
#113203=CARTESIAN_POINT('',(6.44290310132316,12.1,26.2940224745392));
#113204=CARTESIAN_POINT('Origin',(6.,12.1,28.5));
#113205=CARTESIAN_POINT('',(6.44290310132316,13.7,26.2940224745392));
#113206=CARTESIAN_POINT('',(6.44290310132316,11.5,26.2940224745392));
#113207=CARTESIAN_POINT('',(6.71942342556966,13.7,26.3681158721118));
#113208=CARTESIAN_POINT('Origin',(6.,13.7,28.5));
#113209=CARTESIAN_POINT('',(6.71942342556966,12.1,26.3681158721118));
#113210=CARTESIAN_POINT('',(6.71942342556966,11.5,26.3681158721118));
#113211=CARTESIAN_POINT('',(6.81923838528667,12.1,26.4044455463833));
#113212=CARTESIAN_POINT('Origin',(6.,12.1,28.5));
#113213=CARTESIAN_POINT('',(6.81923838528667,13.7,26.4044455463833));
#113214=CARTESIAN_POINT('',(6.81923838528667,11.5,26.4044455463833));
#113215=CARTESIAN_POINT('',(7.07869156100444,13.7,26.5254305491531));
#113216=CARTESIAN_POINT('Origin',(6.,13.7,28.5));
#113217=CARTESIAN_POINT('',(7.07869156100444,12.1,26.5254305491531));
#113218=CARTESIAN_POINT('',(7.07869156100444,11.5,26.5254305491531));
#113219=CARTESIAN_POINT('',(7.17068152546788,12.1,26.5785409798988));
#113220=CARTESIAN_POINT('Origin',(6.,12.1,28.5));
#113221=CARTESIAN_POINT('',(7.17068152546788,13.7,26.5785409798988));
#113222=CARTESIAN_POINT('',(7.17068152546788,11.5,26.5785409798988));
#113223=CARTESIAN_POINT('',(7.40518419920236,13.7,26.742741519778));
#113224=CARTESIAN_POINT('Origin',(6.,13.7,28.5));
#113225=CARTESIAN_POINT('',(7.40518419920237,12.1,26.742741519778));
#113226=CARTESIAN_POINT('',(7.40518419920236,11.5,26.742741519778));
#113227=CARTESIAN_POINT('',(7.48655409989118,12.1,26.811018973435));
#113228=CARTESIAN_POINT('Origin',(6.,12.1,28.5));
#113229=CARTESIAN_POINT('',(7.48655409989118,13.7,26.811018973435));
#113230=CARTESIAN_POINT('',(7.48655409989118,11.5,26.811018973435));
#113231=CARTESIAN_POINT('',(7.68898102656504,13.7,27.0134459001088));
#113232=CARTESIAN_POINT('Origin',(6.,13.7,28.5));
#113233=CARTESIAN_POINT('',(7.68898102656504,12.1,27.0134459001088));
#113234=CARTESIAN_POINT('',(7.68898102656504,11.5,27.0134459001088));
#113235=CARTESIAN_POINT('',(7.75725848022196,12.1,27.0948158007976));
#113236=CARTESIAN_POINT('Origin',(6.,12.1,28.5));
#113237=CARTESIAN_POINT('',(7.75725848022196,13.7,27.0948158007976));
#113238=CARTESIAN_POINT('',(7.75725848022196,11.5,27.0948158007976));
#113239=CARTESIAN_POINT('',(7.92145902010118,13.7,27.3293184745321));
#113240=CARTESIAN_POINT('Origin',(6.,13.7,28.5));
#113241=CARTESIAN_POINT('',(7.92145902010118,12.1,27.3293184745321));
#113242=CARTESIAN_POINT('',(7.92145902010118,11.5,27.3293184745321));
#113243=CARTESIAN_POINT('',(7.97456945084689,12.1,27.4213084389956));
#113244=CARTESIAN_POINT('Origin',(6.,12.1,28.5));
#113245=CARTESIAN_POINT('',(7.97456945084689,13.7,27.4213084389956));
#113246=CARTESIAN_POINT('',(7.97456945084689,11.5,27.4213084389956));
#113247=CARTESIAN_POINT('',(8.09555445361672,13.7,27.6807616147133));
#113248=CARTESIAN_POINT('Origin',(6.,13.7,28.5));
#113249=CARTESIAN_POINT('',(8.09555445361672,12.1,27.6807616147133));
#113250=CARTESIAN_POINT('',(8.09555445361672,11.5,27.6807616147133));
#113251=CARTESIAN_POINT('',(8.1318841278882,12.1,27.7805765744303));
#113252=CARTESIAN_POINT('Origin',(6.,12.1,28.5));
#113253=CARTESIAN_POINT('',(8.1318841278882,13.7,27.7805765744303));
#113254=CARTESIAN_POINT('',(8.1318841278882,11.5,27.7805765744303));
#113255=CARTESIAN_POINT('Origin',(6.,13.7,28.5));
#113256=CARTESIAN_POINT('Origin',(7.97335450365041,14.,27.7817576990161));
#113257=CARTESIAN_POINT('',(7.97335450365041,13.85,27.7817576990161));
#113258=CARTESIAN_POINT('Ctrl Pts',(7.97335450365041,13.85,27.7817576990161));
#113259=CARTESIAN_POINT('Ctrl Pts',(8.03234758294447,13.7778888548065,27.7330009686631));
#113260=CARTESIAN_POINT('Ctrl Pts',(8.09555445361672,13.7,27.6807616147133));
#113261=CARTESIAN_POINT('',(7.97335450365041,12.1,27.7817576990161));
#113262=CARTESIAN_POINT('',(7.97335450365041,14.,27.7817576990161));
#113263=CARTESIAN_POINT('',(7.97335450365041,12.1,27.7817576990161));
#113264=CARTESIAN_POINT('Origin',(8.18478534332724,12.1,27.7048031667678));
#113265=CARTESIAN_POINT('',(8.45093940593617,12.1,27.7781994538453));
#113266=CARTESIAN_POINT('Origin',(8.45093940593617,14.,27.7781994538453));
#113267=CARTESIAN_POINT('Ctrl Pts',(8.1318841278882,13.7,27.7805765744303));
#113268=CARTESIAN_POINT('Ctrl Pts',(8.04988604638594,13.7778888548064,27.7811875009402));
#113269=CARTESIAN_POINT('Ctrl Pts',(7.97335450365041,13.85,27.7817576990161));
#113270=CARTESIAN_POINT('Origin',(7.81865334794732,14.,27.45));
#113271=CARTESIAN_POINT('',(7.81865334794732,13.85,27.45));
#113272=CARTESIAN_POINT('Ctrl Pts',(7.81865334794732,13.85,27.45));
#113273=CARTESIAN_POINT('Ctrl Pts',(7.86828367243552,13.7778888548063,27.3917399532223));
#113274=CARTESIAN_POINT('Ctrl Pts',(7.92145902010118,13.7,27.3293184745321));
#113275=CARTESIAN_POINT('',(7.81865334794732,12.1,27.45));
#113276=CARTESIAN_POINT('',(7.81865334794732,14.,27.45));
#113277=CARTESIAN_POINT('',(7.81865334794732,12.1,27.45));
#113278=CARTESIAN_POINT('Origin',(8.01350906379882,12.1,27.3375));
#113279=CARTESIAN_POINT('',(8.28836477965032,12.1,27.3635640646055));
#113280=CARTESIAN_POINT('Origin',(8.28836477965032,14.,27.3635640646055));
#113281=CARTESIAN_POINT('Ctrl Pts',(7.9745694508469,13.7,27.4213084389956));
#113282=CARTESIAN_POINT('Ctrl Pts',(7.89392319072658,13.7778888548063,27.436148901584));
#113283=CARTESIAN_POINT('Ctrl Pts',(7.81865334794732,13.85,27.45));
#113284=CARTESIAN_POINT('Origin',(7.60869333054985,14.,27.1501460196583));
#113285=CARTESIAN_POINT('',(7.60869333054985,13.85,27.1501460196583));
#113286=CARTESIAN_POINT('Ctrl Pts',(7.60869333054985,13.85,27.1501460196583));
#113287=CARTESIAN_POINT('Ctrl Pts',(7.64745290793648,13.7778888548065,27.0841528584965));
#113288=CARTESIAN_POINT('Ctrl Pts',(7.68898102656505,13.7,27.0134459001088));
#113289=CARTESIAN_POINT('',(7.60869333054985,12.1,27.1501460196583));
#113290=CARTESIAN_POINT('',(7.60869333054985,14.,27.1501460196583));
#113291=CARTESIAN_POINT('',(7.60869333054985,12.1,27.1501460196583));
#113292=CARTESIAN_POINT('Origin',(7.78105333025163,12.1,27.0055188074788));
#113293=CARTESIAN_POINT('',(8.05625934750324,12.1,26.9834587061984));
#113294=CARTESIAN_POINT('Origin',(8.05625934750324,14.,26.9834587061984));
#113295=CARTESIAN_POINT('Ctrl Pts',(7.75725848022197,13.7,27.0948158007976));
#113296=CARTESIAN_POINT('Ctrl Pts',(7.68041443728832,13.7778888548063,27.1234348795186));
#113297=CARTESIAN_POINT('Ctrl Pts',(7.60869333054985,13.85,27.1501460196583));
#113298=CARTESIAN_POINT('Origin',(7.34985398034173,14.,26.8913066694501));
#113299=CARTESIAN_POINT('',(7.34985398034173,13.85,26.8913066694501));
#113300=CARTESIAN_POINT('Ctrl Pts',(7.34985398034173,13.85,26.8913066694501));
#113301=CARTESIAN_POINT('Ctrl Pts',(7.37656512048136,13.7778888548064,26.8195855627119));
#113302=CARTESIAN_POINT('Ctrl Pts',(7.40518419920237,13.7,26.742741519778));
#113303=CARTESIAN_POINT('',(7.34985398034173,12.1,26.8913066694501));
#113304=CARTESIAN_POINT('',(7.34985398034173,14.,26.8913066694501));
#113305=CARTESIAN_POINT('',(7.34985398034173,12.1,26.8913066694501));
#113306=CARTESIAN_POINT('Origin',(7.49448119252121,12.1,26.7189466697484));
#113307=CARTESIAN_POINT('',(7.76167551559972,12.1,26.6494326875964));
#113308=CARTESIAN_POINT('Origin',(7.76167551559972,14.,26.6494326875964));
#113309=CARTESIAN_POINT('Ctrl Pts',(7.48655409989118,13.7,26.811018973435));
#113310=CARTESIAN_POINT('Ctrl Pts',(7.4158471415036,13.7778888548064,26.8525470920635));
#113311=CARTESIAN_POINT('Ctrl Pts',(7.34985398034173,13.85,26.8913066694501));
#113312=CARTESIAN_POINT('Origin',(7.05000000000001,14.,26.6813466520527));
#113313=CARTESIAN_POINT('',(7.05000000000001,13.85,26.6813466520527));
#113314=CARTESIAN_POINT('Ctrl Pts',(7.05000000000001,13.85,26.6813466520527));
#113315=CARTESIAN_POINT('Ctrl Pts',(7.06385109841592,13.7778888548066,26.6060768092737));
#113316=CARTESIAN_POINT('Ctrl Pts',(7.07869156100444,13.7,26.5254305491531));
#113317=CARTESIAN_POINT('',(7.05000000000001,12.1,26.6813466520527));
#113318=CARTESIAN_POINT('',(7.05000000000001,14.,26.6813466520527));
#113319=CARTESIAN_POINT('',(7.05000000000001,12.1,26.6813466520527));
#113320=CARTESIAN_POINT('Origin',(7.1625,12.1,26.4864909362012));
#113321=CARTESIAN_POINT('',(7.41356406460552,12.1,26.3716352203497));
#113322=CARTESIAN_POINT('Origin',(7.41356406460552,14.,26.3716352203497));
#113323=CARTESIAN_POINT('Ctrl Pts',(7.17068152546789,13.7,26.5785409798988));
#113324=CARTESIAN_POINT('Ctrl Pts',(7.10826004677746,13.7778888548066,26.6317163275647));
#113325=CARTESIAN_POINT('Ctrl Pts',(7.05000000000001,13.85,26.6813466520527));
#113326=CARTESIAN_POINT('Origin',(6.71824230098391,14.,26.5266454963496));
#113327=CARTESIAN_POINT('',(6.71824230098391,13.85,26.5266454963496));
#113328=CARTESIAN_POINT('Ctrl Pts',(6.71824230098391,13.85,26.5266454963496));
#113329=CARTESIAN_POINT('Ctrl Pts',(6.71881249905978,13.7778888548067,26.4501139536144));
#113330=CARTESIAN_POINT('Ctrl Pts',(6.71942342556966,13.7,26.3681158721118));
#113331=CARTESIAN_POINT('',(6.71824230098391,12.1,26.5266454963496));
#113332=CARTESIAN_POINT('',(6.71824230098391,14.,26.5266454963496));
#113333=CARTESIAN_POINT('',(6.71824230098391,12.1,26.5266454963496));
#113334=CARTESIAN_POINT('Origin',(6.79519683323218,12.1,26.3152146566728));
#113335=CARTESIAN_POINT('',(7.0225021848062,12.1,26.158507039928));
#113336=CARTESIAN_POINT('Origin',(7.0225021848062,14.,26.158507039928));
#113337=CARTESIAN_POINT('Ctrl Pts',(6.81923838528667,13.7,26.4044455463833));
#113338=CARTESIAN_POINT('Ctrl Pts',(6.76699903133701,13.7778888548064,26.4676524170555));
#113339=CARTESIAN_POINT('Ctrl Pts',(6.71824230098391,13.85,26.5266454963496));
#113340=CARTESIAN_POINT('Origin',(6.36466117310055,14.,26.4319037186744));
#113341=CARTESIAN_POINT('',(6.36466117310056,13.85,26.4319037186744));
#113342=CARTESIAN_POINT('Ctrl Pts',(6.36466117310056,13.85,26.4319037186744));
#113343=CARTESIAN_POINT('Ctrl Pts',(6.35193314565639,13.7778888548065,26.3564358481817));
#113344=CARTESIAN_POINT('Ctrl Pts',(6.33829597339476,13.7,26.275577415511));
#113345=CARTESIAN_POINT('',(6.36466117310055,12.1,26.4319037186744));
#113346=CARTESIAN_POINT('',(6.36466117310055,14.,26.4319037186744));
#113347=CARTESIAN_POINT('',(6.36466117310055,12.1,26.4319037186744));
#113348=CARTESIAN_POINT('Origin',(6.40373201307562,12.1,26.2103219742466));
#113349=CARTESIAN_POINT('',(6.60037209353263,12.1,26.0165239382456));
#113350=CARTESIAN_POINT('Origin',(6.60037209353263,14.,26.0165239382456));
#113351=CARTESIAN_POINT('Ctrl Pts',(6.44290310132316,13.7,26.2940224745392));
#113352=CARTESIAN_POINT('Ctrl Pts',(6.40243313844953,13.7778888548062,26.3653403594364));
#113353=CARTESIAN_POINT('Ctrl Pts',(6.36466117310056,13.85,26.4319037186744));
#113354=CARTESIAN_POINT('Origin',(6.,14.,26.4));
#113355=CARTESIAN_POINT('',(6.,13.85,26.4));
#113356=CARTESIAN_POINT('Ctrl Pts',(6.,13.85,26.4));
#113357=CARTESIAN_POINT('Ctrl Pts',(5.97436048170878,13.7778888548059,26.3278888548059));
#113358=CARTESIAN_POINT('Ctrl Pts',(5.94688956925429,13.7,26.2506269135277));
#113359=CARTESIAN_POINT('',(6.,12.1,26.4));
#113360=CARTESIAN_POINT('',(6.,14.,26.4));
#113361=CARTESIAN_POINT('',(6.,12.1,26.4));
#113362=CARTESIAN_POINT('Origin',(6.,12.1,26.175));
#113363=CARTESIAN_POINT('',(6.16,12.1,25.95));
#113364=CARTESIAN_POINT('Origin',(6.16,14.,25.95));
#113365=CARTESIAN_POINT('Ctrl Pts',(6.05311043074571,13.7,26.2506269135277));
#113366=CARTESIAN_POINT('Ctrl Pts',(6.02563951829103,13.7778888548065,26.3278888548065));
#113367=CARTESIAN_POINT('Ctrl Pts',(6.,13.85,26.4));
#113368=CARTESIAN_POINT('Origin',(5.63533882689945,14.,26.4319037186744));
#113369=CARTESIAN_POINT('',(5.63533882689945,13.85,26.4319037186744));
#113370=CARTESIAN_POINT('Ctrl Pts',(5.63533882689945,13.85,26.4319037186744));
#113371=CARTESIAN_POINT('Ctrl Pts',(5.59756686155053,13.7778888548063,26.3653403594365));
#113372=CARTESIAN_POINT('Ctrl Pts',(5.55709689867685,13.7,26.2940224745392));
#113373=CARTESIAN_POINT('',(5.63533882689945,12.1,26.4319037186744));
#113374=CARTESIAN_POINT('',(5.63533882689945,14.,26.4319037186744));
#113375=CARTESIAN_POINT('',(5.63533882689945,12.1,26.4319037186744));
#113376=CARTESIAN_POINT('Origin',(5.59626798692439,12.1,26.2103219742466));
#113377=CARTESIAN_POINT('',(5.71476638743128,12.1,25.9609565213922));
#113378=CARTESIAN_POINT('Origin',(5.71476638743128,14.,25.9609565213922));
#113379=CARTESIAN_POINT('Ctrl Pts',(5.66170402660524,13.7,26.275577415511));
#113380=CARTESIAN_POINT('Ctrl Pts',(5.64806685434361,13.7778888548065,26.3564358481818));
#113381=CARTESIAN_POINT('Ctrl Pts',(5.63533882689945,13.85,26.4319037186744));
#113382=CARTESIAN_POINT('Origin',(5.28175769901609,14.,26.5266454963496));
#113383=CARTESIAN_POINT('',(5.28175769901609,13.85,26.5266454963496));
#113384=CARTESIAN_POINT('Ctrl Pts',(5.28175769901609,13.85,26.5266454963496));
#113385=CARTESIAN_POINT('Ctrl Pts',(5.23300096866302,13.7778888548065,26.4676524170555));
#113386=CARTESIAN_POINT('Ctrl Pts',(5.18076161471333,13.7,26.4044455463833));
#113387=CARTESIAN_POINT('',(5.28175769901609,12.1,26.5266454963496));
#113388=CARTESIAN_POINT('',(5.28175769901609,14.,26.5266454963496));
#113389=CARTESIAN_POINT('',(5.28175769901609,12.1,26.5266454963496));
#113390=CARTESIAN_POINT('Origin',(5.20480316676782,12.1,26.3152146566728));
#113391=CARTESIAN_POINT('',(5.27819945384529,12.1,26.0490605940638));
#113392=CARTESIAN_POINT('Origin',(5.27819945384529,14.,26.0490605940638));
#113393=CARTESIAN_POINT('Ctrl Pts',(5.28057657443035,13.7,26.3681158721118));
#113394=CARTESIAN_POINT('Ctrl Pts',(5.28118750094021,13.7778888548061,26.4501139536138));
#113395=CARTESIAN_POINT('Ctrl Pts',(5.28175769901609,13.85,26.5266454963496));
#113396=CARTESIAN_POINT('Origin',(4.95,14.,26.6813466520527));
#113397=CARTESIAN_POINT('',(4.95,13.85,26.6813466520527));
#113398=CARTESIAN_POINT('Ctrl Pts',(4.95,13.85,26.6813466520527));
#113399=CARTESIAN_POINT('Ctrl Pts',(4.89173995322247,13.7778888548066,26.6317163275647));
#113400=CARTESIAN_POINT('Ctrl Pts',(4.82931847453212,13.7,26.5785409798988));
#113401=CARTESIAN_POINT('',(4.95,12.1,26.6813466520527));
#113402=CARTESIAN_POINT('',(4.95,14.,26.6813466520527));
#113403=CARTESIAN_POINT('',(4.95,12.1,26.6813466520527));
#113404=CARTESIAN_POINT('Origin',(4.8375,12.1,26.4864909362012));
#113405=CARTESIAN_POINT('',(4.86356406460551,12.1,26.2116352203497));
#113406=CARTESIAN_POINT('Origin',(4.86356406460551,14.,26.2116352203497));
#113407=CARTESIAN_POINT('Ctrl Pts',(4.92130843899556,13.7,26.5254305491531));
#113408=CARTESIAN_POINT('Ctrl Pts',(4.936148901584,13.7778888548062,26.6060768092732));
#113409=CARTESIAN_POINT('Ctrl Pts',(4.95,13.85,26.6813466520527));
#113410=CARTESIAN_POINT('Origin',(4.65014601965827,14.,26.8913066694501));
#113411=CARTESIAN_POINT('',(4.65014601965827,13.85,26.8913066694501));
#113412=CARTESIAN_POINT('Ctrl Pts',(4.65014601965827,13.85,26.8913066694501));
#113413=CARTESIAN_POINT('Ctrl Pts',(4.58415285849654,13.7778888548066,26.8525470920636));
#113414=CARTESIAN_POINT('Ctrl Pts',(4.51344590010882,13.7,26.811018973435));
#113415=CARTESIAN_POINT('',(4.65014601965827,12.1,26.8913066694501));
#113416=CARTESIAN_POINT('',(4.65014601965827,14.,26.8913066694501));
#113417=CARTESIAN_POINT('',(4.65014601965827,12.1,26.8913066694501));
#113418=CARTESIAN_POINT('Origin',(4.50551880747879,12.1,26.7189466697484));
#113419=CARTESIAN_POINT('',(4.48345870619836,12.1,26.4437406524968));
#113420=CARTESIAN_POINT('Origin',(4.48345870619836,14.,26.4437406524968));
#113421=CARTESIAN_POINT('Ctrl Pts',(4.59481580079763,13.7,26.742741519778));
#113422=CARTESIAN_POINT('Ctrl Pts',(4.62343487951859,13.7778888548063,26.8195855627117));
#113423=CARTESIAN_POINT('Ctrl Pts',(4.65014601965827,13.85,26.8913066694502));
#113424=CARTESIAN_POINT('Origin',(4.39130666945015,14.,27.1501460196583));
#113425=CARTESIAN_POINT('',(4.39130666945015,13.85,27.1501460196583));
#113426=CARTESIAN_POINT('Ctrl Pts',(4.39130666945015,13.85,27.1501460196583));
#113427=CARTESIAN_POINT('Ctrl Pts',(4.31958556271188,13.7778888548065,27.1234348795187));
#113428=CARTESIAN_POINT('Ctrl Pts',(4.24274151977803,13.7,27.0948158007976));
#113429=CARTESIAN_POINT('',(4.39130666945015,12.1,27.1501460196583));
#113430=CARTESIAN_POINT('',(4.39130666945015,14.,27.1501460196583));
#113431=CARTESIAN_POINT('',(4.39130666945015,12.1,27.1501460196583));
#113432=CARTESIAN_POINT('Origin',(4.21894666974837,12.1,27.0055188074788));
#113433=CARTESIAN_POINT('',(4.14943268759645,12.1,26.7383244844003));
#113434=CARTESIAN_POINT('Origin',(4.14943268759645,14.,26.7383244844003));
#113435=CARTESIAN_POINT('Ctrl Pts',(4.31101897343495,13.7,27.0134459001088));
#113436=CARTESIAN_POINT('Ctrl Pts',(4.35254709206349,13.7778888548065,27.0841528584965));
#113437=CARTESIAN_POINT('Ctrl Pts',(4.39130666945015,13.85,27.1501460196583));
#113438=CARTESIAN_POINT('Origin',(4.18134665205268,14.,27.45));
#113439=CARTESIAN_POINT('',(4.18134665205268,13.85,27.45));
#113440=CARTESIAN_POINT('Ctrl Pts',(4.18134665205268,13.85,27.45));
#113441=CARTESIAN_POINT('Ctrl Pts',(4.10607680927348,13.7778888548064,27.436148901584));
#113442=CARTESIAN_POINT('Ctrl Pts',(4.0254305491531,13.7,27.4213084389956));
#113443=CARTESIAN_POINT('',(4.18134665205268,12.1,27.45));
#113444=CARTESIAN_POINT('',(4.18134665205268,14.,27.45));
#113445=CARTESIAN_POINT('',(4.18134665205268,12.1,27.45));
#113446=CARTESIAN_POINT('Origin',(3.98649093620118,12.1,27.3375));
#113447=CARTESIAN_POINT('',(3.87163522034968,12.1,27.0864359353945));
#113448=CARTESIAN_POINT('Origin',(3.87163522034968,14.,27.0864359353945));
#113449=CARTESIAN_POINT('Ctrl Pts',(4.07854097989881,13.7,27.3293184745321));
#113450=CARTESIAN_POINT('Ctrl Pts',(4.13171632756462,13.7778888548065,27.3917399532224));
#113451=CARTESIAN_POINT('Ctrl Pts',(4.18134665205268,13.85,27.45));
#113452=CARTESIAN_POINT('Origin',(4.02664549634959,14.,27.7817576990161));
#113453=CARTESIAN_POINT('',(4.02664549634959,13.85,27.7817576990161));
#113454=CARTESIAN_POINT('Ctrl Pts',(4.02664549634959,13.85,27.7817576990161));
#113455=CARTESIAN_POINT('Ctrl Pts',(3.95011395361384,13.7778888548062,27.7811875009402));
#113456=CARTESIAN_POINT('Ctrl Pts',(3.8681158721118,13.7,27.7805765744303));
#113457=CARTESIAN_POINT('',(4.02664549634959,12.1,27.7817576990161));
#113458=CARTESIAN_POINT('',(4.02664549634959,14.,27.7817576990161));
#113459=CARTESIAN_POINT('',(4.02664549634959,12.1,27.7817576990161));
#113460=CARTESIAN_POINT('Origin',(3.81521465667276,12.1,27.7048031667678));
#113461=CARTESIAN_POINT('',(3.65850703992804,12.1,27.4774978151938));
#113462=CARTESIAN_POINT('Origin',(3.65850703992804,14.,27.4774978151938));
#113463=CARTESIAN_POINT('Ctrl Pts',(3.90444554638328,13.7,27.6807616147133));
#113464=CARTESIAN_POINT('Ctrl Pts',(3.96765241705571,13.7778888548067,27.7330009686632));
#113465=CARTESIAN_POINT('Ctrl Pts',(4.02664549634959,13.85,27.7817576990161));
#113466=CARTESIAN_POINT('Origin',(3.93190371867436,14.,28.1353388268995));
#113467=CARTESIAN_POINT('',(3.93190371867436,13.85,28.1353388268995));
#113468=CARTESIAN_POINT('Ctrl Pts',(3.93190371867436,13.85,28.1353388268995));
#113469=CARTESIAN_POINT('Ctrl Pts',(3.85643584818165,13.7778888548064,28.1480668543436));
#113470=CARTESIAN_POINT('Ctrl Pts',(3.77557741551096,13.7,28.1617040266052));
#113471=CARTESIAN_POINT('',(3.93190371867436,12.1,28.1353388268995));
#113472=CARTESIAN_POINT('',(3.93190371867436,14.,28.1353388268995));
#113473=CARTESIAN_POINT('',(3.93190371867436,12.1,28.1353388268995));
#113474=CARTESIAN_POINT('Origin',(3.71032197424662,12.1,28.0962679869244));
#113475=CARTESIAN_POINT('',(3.51652393824558,12.1,27.8996279064674));
#113476=CARTESIAN_POINT('Origin',(3.51652393824558,14.,27.8996279064674));
#113477=CARTESIAN_POINT('Ctrl Pts',(3.79402247453916,13.7,28.0570968986768));
#113478=CARTESIAN_POINT('Ctrl Pts',(3.86534035943646,13.7778888548062,28.0975668615505));
#113479=CARTESIAN_POINT('Ctrl Pts',(3.93190371867436,13.85,28.1353388268995));
#113480=CARTESIAN_POINT('Origin',(3.9,14.,28.5));
#113481=CARTESIAN_POINT('',(3.9,13.85,28.5));
#113482=CARTESIAN_POINT('Ctrl Pts',(3.9,13.85,28.5));
#113483=CARTESIAN_POINT('Ctrl Pts',(3.82788885480655,13.7778888548065,28.525639518291));
#113484=CARTESIAN_POINT('Ctrl Pts',(3.75062691352768,13.7,28.5531104307457));
#113485=CARTESIAN_POINT('',(3.9,12.1,28.5));
#113486=CARTESIAN_POINT('',(3.9,14.,28.5));
#113487=CARTESIAN_POINT('',(3.9,12.1,28.5));
#113488=CARTESIAN_POINT('Origin',(3.675,12.1,28.5));
#113489=CARTESIAN_POINT('',(3.45,12.1,28.34));
#113490=CARTESIAN_POINT('Origin',(3.45,14.,28.34));
#113491=CARTESIAN_POINT('Ctrl Pts',(3.75062691352768,13.7,28.4468895692543));
#113492=CARTESIAN_POINT('Ctrl Pts',(3.82788885480652,13.7778888548065,28.474360481709));
#113493=CARTESIAN_POINT('Ctrl Pts',(3.9,13.85,28.5));
#113494=CARTESIAN_POINT('Origin',(3.93190371867437,14.,28.8646611731006));
#113495=CARTESIAN_POINT('',(3.93190371867437,13.85,28.8646611731006));
#113496=CARTESIAN_POINT('Ctrl Pts',(3.93190371867437,13.85,28.8646611731006));
#113497=CARTESIAN_POINT('Ctrl Pts',(3.86534035943652,13.7778888548063,28.9024331384495));
#113498=CARTESIAN_POINT('Ctrl Pts',(3.79402247453916,13.7,28.9429031013232));
#113499=CARTESIAN_POINT('',(3.93190371867437,12.1,28.8646611731006));
#113500=CARTESIAN_POINT('',(3.93190371867437,14.,28.8646611731006));
#113501=CARTESIAN_POINT('',(3.93190371867437,12.1,28.8646611731006));
#113502=CARTESIAN_POINT('Origin',(3.71032197424662,12.1,28.9037320130756));
#113503=CARTESIAN_POINT('',(3.46095652139216,12.1,28.7852336125687));
#113504=CARTESIAN_POINT('Origin',(3.46095652139216,14.,28.7852336125687));
#113505=CARTESIAN_POINT('Ctrl Pts',(3.77557741551096,13.7,28.8382959733948));
#113506=CARTESIAN_POINT('Ctrl Pts',(3.8564358481818,13.7778888548066,28.8519331456564));
#113507=CARTESIAN_POINT('Ctrl Pts',(3.93190371867437,13.85,28.8646611731006));
#113508=CARTESIAN_POINT('Origin',(4.02664549634959,14.,29.2182423009839));
#113509=CARTESIAN_POINT('',(4.02664549634959,13.85,29.2182423009839));
#113510=CARTESIAN_POINT('Ctrl Pts',(4.02664549634959,13.85,29.2182423009839));
#113511=CARTESIAN_POINT('Ctrl Pts',(3.96765241705536,13.7778888548063,29.2669990313371));
#113512=CARTESIAN_POINT('Ctrl Pts',(3.90444554638327,13.7,29.3192383852867));
#113513=CARTESIAN_POINT('',(4.02664549634959,12.1,29.2182423009839));
#113514=CARTESIAN_POINT('',(4.02664549634959,14.,29.2182423009839));
#113515=CARTESIAN_POINT('',(4.02664549634959,12.1,29.2182423009839));
#113516=CARTESIAN_POINT('Origin',(3.81521465667276,12.1,29.2951968332322));
#113517=CARTESIAN_POINT('',(3.54906059406382,12.1,29.2218005461547));
#113518=CARTESIAN_POINT('Origin',(3.54906059406382,14.,29.2218005461547));
#113519=CARTESIAN_POINT('Ctrl Pts',(3.8681158721118,13.7,29.2194234255697));
#113520=CARTESIAN_POINT('Ctrl Pts',(3.95011395361416,13.7778888548065,29.2188124990598));
#113521=CARTESIAN_POINT('Ctrl Pts',(4.02664549634959,13.85,29.2182423009839));
#113522=CARTESIAN_POINT('Origin',(4.18134665205268,14.,29.55));
#113523=CARTESIAN_POINT('',(4.18134665205268,13.85,29.55));
#113524=CARTESIAN_POINT('Ctrl Pts',(4.18134665205268,13.85,29.55));
#113525=CARTESIAN_POINT('Ctrl Pts',(4.1317163275649,13.7778888548069,29.6082600467773));
#113526=CARTESIAN_POINT('Ctrl Pts',(4.07854097989881,13.7,29.6706815254679));
#113527=CARTESIAN_POINT('',(4.18134665205268,12.1,29.55));
#113528=CARTESIAN_POINT('',(4.18134665205268,14.,29.55));
#113529=CARTESIAN_POINT('',(4.18134665205268,12.1,29.55));
#113530=CARTESIAN_POINT('Origin',(3.98649093620118,12.1,29.6625));
#113531=CARTESIAN_POINT('',(3.71163522034968,12.1,29.6364359353945));
#113532=CARTESIAN_POINT('Origin',(3.71163522034968,14.,29.6364359353945));
#113533=CARTESIAN_POINT('Ctrl Pts',(4.02543054915311,13.7,29.5786915610044));
#113534=CARTESIAN_POINT('Ctrl Pts',(4.1060768092734,13.7778888548063,29.563851098416));
#113535=CARTESIAN_POINT('Ctrl Pts',(4.18134665205268,13.85,29.55));
#113536=CARTESIAN_POINT('Origin',(4.39130666945015,14.,29.8498539803417));
#113537=CARTESIAN_POINT('',(4.39130666945015,13.85,29.8498539803417));
#113538=CARTESIAN_POINT('Ctrl Pts',(4.39130666945015,13.85,29.8498539803417));
#113539=CARTESIAN_POINT('Ctrl Pts',(4.35254709206352,13.7778888548065,29.9158471415035));
#113540=CARTESIAN_POINT('Ctrl Pts',(4.31101897343496,13.7,29.9865540998912));
#113541=CARTESIAN_POINT('',(4.39130666945015,12.1,29.8498539803417));
#113542=CARTESIAN_POINT('',(4.39130666945015,14.,29.8498539803417));
#113543=CARTESIAN_POINT('',(4.39130666945015,12.1,29.8498539803417));
#113544=CARTESIAN_POINT('Origin',(4.21894666974838,12.1,29.9944811925212));
#113545=CARTESIAN_POINT('',(3.94374065249676,12.1,30.0165412938016));
#113546=CARTESIAN_POINT('Origin',(3.94374065249676,14.,30.0165412938016));
#113547=CARTESIAN_POINT('Ctrl Pts',(4.24274151977804,13.7,29.9051841992024));
#113548=CARTESIAN_POINT('Ctrl Pts',(4.31958556271157,13.7778888548062,29.8765651204815));
#113549=CARTESIAN_POINT('Ctrl Pts',(4.39130666945015,13.85,29.8498539803417));
#113550=CARTESIAN_POINT('Origin',(4.65014601965827,14.,30.1086933305499));
#113551=CARTESIAN_POINT('',(4.65014601965827,13.85,30.1086933305499));
#113552=CARTESIAN_POINT('Ctrl Pts',(4.65014601965827,13.85,30.1086933305499));
#113553=CARTESIAN_POINT('Ctrl Pts',(4.62343487951865,13.7778888548065,30.1804144372881));
#113554=CARTESIAN_POINT('Ctrl Pts',(4.59481580079763,13.7,30.257258480222));
#113555=CARTESIAN_POINT('',(4.65014601965827,12.1,30.1086933305499));
#113556=CARTESIAN_POINT('',(4.65014601965827,14.,30.1086933305499));
#113557=CARTESIAN_POINT('',(4.65014601965827,12.1,30.1086933305499));
#113558=CARTESIAN_POINT('Origin',(4.50551880747879,12.1,30.2810533302516));
#113559=CARTESIAN_POINT('',(4.23832448440029,12.1,30.3505673124035));
#113560=CARTESIAN_POINT('Origin',(4.23832448440029,14.,30.3505673124035));
#113561=CARTESIAN_POINT('Ctrl Pts',(4.51344590010882,13.7,30.188981026565));
#113562=CARTESIAN_POINT('Ctrl Pts',(4.58415285849637,13.7778888548064,30.1474529079366));
#113563=CARTESIAN_POINT('Ctrl Pts',(4.65014601965827,13.85,30.1086933305499));
#113564=CARTESIAN_POINT('Origin',(4.95,14.,30.3186533479473));
#113565=CARTESIAN_POINT('',(4.95,13.85,30.3186533479473));
#113566=CARTESIAN_POINT('Ctrl Pts',(4.95,13.85,30.3186533479473));
#113567=CARTESIAN_POINT('Ctrl Pts',(4.93614890158408,13.7778888548066,30.3939231907263));
#113568=CARTESIAN_POINT('Ctrl Pts',(4.92130843899556,13.7,30.4745694508469));
#113569=CARTESIAN_POINT('',(4.95,12.1,30.3186533479473));
#113570=CARTESIAN_POINT('',(4.95,14.,30.3186533479473));
#113571=CARTESIAN_POINT('',(4.95,12.1,30.3186533479473));
#113572=CARTESIAN_POINT('Origin',(4.8375,12.1,30.5135090637988));
#113573=CARTESIAN_POINT('',(4.5864359353945,12.1,30.6283647796503));
#113574=CARTESIAN_POINT('Origin',(4.5864359353945,14.,30.6283647796503));
#113575=CARTESIAN_POINT('Ctrl Pts',(4.82931847453212,13.7,30.4214590201012));
#113576=CARTESIAN_POINT('Ctrl Pts',(4.89173995322246,13.7778888548065,30.3682836724353));
#113577=CARTESIAN_POINT('Ctrl Pts',(4.95,13.85,30.3186533479473));
#113578=CARTESIAN_POINT('Origin',(5.2817576990161,14.,30.4733545036504));
#113579=CARTESIAN_POINT('',(5.2817576990161,13.85,30.4733545036504));
#113580=CARTESIAN_POINT('Ctrl Pts',(5.2817576990161,13.85,30.4733545036504));
#113581=CARTESIAN_POINT('Ctrl Pts',(5.28118750094022,13.7778888548068,30.5498860463855));
#113582=CARTESIAN_POINT('Ctrl Pts',(5.28057657443035,13.7,30.6318841278882));
#113583=CARTESIAN_POINT('',(5.2817576990161,12.1,30.4733545036504));
#113584=CARTESIAN_POINT('',(5.2817576990161,14.,30.4733545036504));
#113585=CARTESIAN_POINT('',(5.2817576990161,12.1,30.4733545036504));
#113586=CARTESIAN_POINT('Origin',(5.20480316676782,12.1,30.6847853433272));
#113587=CARTESIAN_POINT('',(4.97749781519381,12.1,30.841492960072));
#113588=CARTESIAN_POINT('Origin',(4.97749781519381,14.,30.841492960072));
#113589=CARTESIAN_POINT('Ctrl Pts',(5.18076161471333,13.7,30.5955544536167));
#113590=CARTESIAN_POINT('Ctrl Pts',(5.23300096866312,13.7778888548066,30.5323475829444));
#113591=CARTESIAN_POINT('Ctrl Pts',(5.2817576990161,13.85,30.4733545036504));
#113592=CARTESIAN_POINT('Origin',(5.63533882689945,14.,30.5680962813256));
#113593=CARTESIAN_POINT('',(5.63533882689945,13.85,30.5680962813256));
#113594=CARTESIAN_POINT('Ctrl Pts',(5.63533882689945,13.85,30.5680962813256));
#113595=CARTESIAN_POINT('Ctrl Pts',(5.64806685434359,13.7778888548066,30.6435641518181));
#113596=CARTESIAN_POINT('Ctrl Pts',(5.66170402660524,13.7,30.724422584489));
#113597=CARTESIAN_POINT('',(5.63533882689945,12.1,30.5680962813256));
#113598=CARTESIAN_POINT('',(5.63533882689945,14.,30.5680962813256));
#113599=CARTESIAN_POINT('',(5.63533882689945,12.1,30.5680962813256));
#113600=CARTESIAN_POINT('Origin',(5.59626798692439,12.1,30.7896780257534));
#113601=CARTESIAN_POINT('',(5.39962790646737,12.1,30.9834760617544));
#113602=CARTESIAN_POINT('Origin',(5.39962790646737,14.,30.9834760617544));
#113603=CARTESIAN_POINT('Ctrl Pts',(5.55709689867685,13.7,30.7059775254608));
#113604=CARTESIAN_POINT('Ctrl Pts',(5.59756686155053,13.7778888548063,30.6346596405635));
#113605=CARTESIAN_POINT('Ctrl Pts',(5.63533882689945,13.85,30.5680962813256));
#113606=CARTESIAN_POINT('Origin',(6.,14.,30.6));
#113607=CARTESIAN_POINT('',(6.,13.85,30.6));
#113608=CARTESIAN_POINT('Ctrl Pts',(6.,13.85,30.6));
#113609=CARTESIAN_POINT('Ctrl Pts',(6.02563951829106,13.7778888548064,30.6721111451936));
#113610=CARTESIAN_POINT('Ctrl Pts',(6.05311043074571,13.7,30.7493730864723));
#113611=CARTESIAN_POINT('',(6.,12.1,30.6));
#113612=CARTESIAN_POINT('',(6.,14.,30.6));
#113613=CARTESIAN_POINT('',(6.,12.1,30.6));
#113614=CARTESIAN_POINT('Origin',(6.,12.1,30.825));
#113615=CARTESIAN_POINT('',(5.84,12.1,31.05));
#113616=CARTESIAN_POINT('Origin',(5.84,14.,31.05));
#113617=CARTESIAN_POINT('Ctrl Pts',(5.94688956925429,13.7,30.7493730864723));
#113618=CARTESIAN_POINT('Ctrl Pts',(5.97436048170889,13.7778888548063,30.6721111451937));
#113619=CARTESIAN_POINT('Ctrl Pts',(6.,13.85,30.6));
#113620=CARTESIAN_POINT('Origin',(6.36466117310055,14.,30.5680962813256));
#113621=CARTESIAN_POINT('',(6.36466117310056,13.85,30.5680962813256));
#113622=CARTESIAN_POINT('Ctrl Pts',(6.36466117310056,13.85,30.5680962813256));
#113623=CARTESIAN_POINT('Ctrl Pts',(6.40243313844958,13.7778888548061,30.6346596405636));
#113624=CARTESIAN_POINT('Ctrl Pts',(6.44290310132316,13.7,30.7059775254608));
#113625=CARTESIAN_POINT('',(6.36466117310055,12.1,30.5680962813256));
#113626=CARTESIAN_POINT('',(6.36466117310055,14.,30.5680962813256));
#113627=CARTESIAN_POINT('',(6.36466117310055,12.1,30.5680962813256));
#113628=CARTESIAN_POINT('Origin',(6.40373201307562,12.1,30.7896780257534));
#113629=CARTESIAN_POINT('',(6.28523361256872,12.1,31.0390434786078));
#113630=CARTESIAN_POINT('Origin',(6.28523361256872,14.,31.0390434786078));
#113631=CARTESIAN_POINT('Ctrl Pts',(6.33829597339476,13.7,30.724422584489));
#113632=CARTESIAN_POINT('Ctrl Pts',(6.35193314565637,13.7778888548064,30.6435641518184));
#113633=CARTESIAN_POINT('Ctrl Pts',(6.36466117310056,13.85,30.5680962813256));
#113634=CARTESIAN_POINT('Origin',(6.71824230098391,14.,30.4733545036504));
#113635=CARTESIAN_POINT('',(6.71824230098391,13.85,30.4733545036504));
#113636=CARTESIAN_POINT('Ctrl Pts',(6.71824230098391,13.85,30.4733545036504));
#113637=CARTESIAN_POINT('Ctrl Pts',(6.76699903133736,13.7778888548059,30.532347582945));
#113638=CARTESIAN_POINT('Ctrl Pts',(6.81923838528667,13.7,30.5955544536167));
#113639=CARTESIAN_POINT('',(6.71824230098391,12.1,30.4733545036504));
#113640=CARTESIAN_POINT('',(6.71824230098391,14.,30.4733545036504));
#113641=CARTESIAN_POINT('',(6.71824230098391,12.1,30.4733545036504));
#113642=CARTESIAN_POINT('Origin',(6.79519683323218,12.1,30.6847853433272));
#113643=CARTESIAN_POINT('',(6.72180054615471,12.1,30.9509394059362));
#113644=CARTESIAN_POINT('Origin',(6.72180054615471,14.,30.9509394059362));
#113645=CARTESIAN_POINT('Ctrl Pts',(6.71942342556966,13.7,30.6318841278882));
#113646=CARTESIAN_POINT('Ctrl Pts',(6.71881249905979,13.7778888548063,30.5498860463861));
#113647=CARTESIAN_POINT('Ctrl Pts',(6.71824230098391,13.85,30.4733545036504));
#113648=CARTESIAN_POINT('Origin',(7.05000000000001,14.,30.3186533479473));
#113649=CARTESIAN_POINT('',(7.05000000000001,13.85,30.3186533479473));
#113650=CARTESIAN_POINT('Ctrl Pts',(7.05000000000001,13.85,30.3186533479473));
#113651=CARTESIAN_POINT('Ctrl Pts',(7.10826004677755,13.7778888548065,30.3682836724353));
#113652=CARTESIAN_POINT('Ctrl Pts',(7.17068152546789,13.7,30.4214590201012));
#113653=CARTESIAN_POINT('',(7.05000000000001,12.1,30.3186533479473));
#113654=CARTESIAN_POINT('',(7.05000000000001,14.,30.3186533479473));
#113655=CARTESIAN_POINT('',(7.05000000000001,12.1,30.3186533479473));
#113656=CARTESIAN_POINT('Origin',(7.1625,12.1,30.5135090637988));
#113657=CARTESIAN_POINT('',(7.13643593539449,12.1,30.7883647796503));
#113658=CARTESIAN_POINT('Origin',(7.13643593539449,14.,30.7883647796503));
#113659=CARTESIAN_POINT('Ctrl Pts',(7.07869156100444,13.7,30.4745694508469));
#113660=CARTESIAN_POINT('Ctrl Pts',(7.06385109841591,13.7778888548066,30.3939231907262));
#113661=CARTESIAN_POINT('Ctrl Pts',(7.05000000000001,13.85,30.3186533479473));
#113662=CARTESIAN_POINT('Origin',(7.34985398034173,14.,30.1086933305499));
#113663=CARTESIAN_POINT('',(7.34985398034173,13.85,30.1086933305499));
#113664=CARTESIAN_POINT('Ctrl Pts',(7.34985398034173,13.85,30.1086933305499));
#113665=CARTESIAN_POINT('Ctrl Pts',(7.41584714150318,13.7778888548069,30.1474529079363));
#113666=CARTESIAN_POINT('Ctrl Pts',(7.48655409989118,13.7,30.188981026565));
#113667=CARTESIAN_POINT('',(7.34985398034173,12.1,30.1086933305499));
#113668=CARTESIAN_POINT('',(7.34985398034173,14.,30.1086933305499));
#113669=CARTESIAN_POINT('',(7.34985398034173,12.1,30.1086933305499));
#113670=CARTESIAN_POINT('Origin',(7.4944811925212,12.1,30.2810533302516));
#113671=CARTESIAN_POINT('',(7.51654129380164,12.1,30.5562593475032));
#113672=CARTESIAN_POINT('Origin',(7.51654129380164,14.,30.5562593475032));
#113673=CARTESIAN_POINT('Ctrl Pts',(7.40518419920237,13.7,30.257258480222));
#113674=CARTESIAN_POINT('Ctrl Pts',(7.3765651204814,13.7778888548063,30.1804144372883));
#113675=CARTESIAN_POINT('Ctrl Pts',(7.34985398034173,13.85,30.1086933305499));
#113676=CARTESIAN_POINT('Origin',(7.60869333054985,14.,29.8498539803417));
#113677=CARTESIAN_POINT('',(7.60869333054985,13.85,29.8498539803417));
#113678=CARTESIAN_POINT('Ctrl Pts',(7.60869333054985,13.85,29.8498539803417));
#113679=CARTESIAN_POINT('Ctrl Pts',(7.6804144372882,13.7778888548064,29.8765651204814));
#113680=CARTESIAN_POINT('Ctrl Pts',(7.75725848022197,13.7,29.9051841992024));
#113681=CARTESIAN_POINT('',(7.60869333054985,12.1,29.8498539803417));
#113682=CARTESIAN_POINT('',(7.60869333054985,14.,29.8498539803417));
#113683=CARTESIAN_POINT('',(7.60869333054985,12.1,29.8498539803417));
#113684=CARTESIAN_POINT('Origin',(7.78105333025163,12.1,29.9944811925212));
#113685=CARTESIAN_POINT('',(7.85056731240355,12.1,30.2616755155997));
#113686=CARTESIAN_POINT('Origin',(7.85056731240355,14.,30.2616755155997));
#113687=CARTESIAN_POINT('Ctrl Pts',(7.68898102656505,13.7,29.9865540998912));
#113688=CARTESIAN_POINT('Ctrl Pts',(7.64745290793635,13.7778888548067,29.9158471415033));
#113689=CARTESIAN_POINT('Ctrl Pts',(7.60869333054985,13.85,29.8498539803417));
#113690=CARTESIAN_POINT('Origin',(7.81865334794732,14.,29.55));
#113691=CARTESIAN_POINT('',(7.81865334794732,13.85,29.55));
#113692=CARTESIAN_POINT('Ctrl Pts',(7.81865334794732,13.85,29.55));
#113693=CARTESIAN_POINT('Ctrl Pts',(7.89392319072661,13.7778888548063,29.563851098416));
#113694=CARTESIAN_POINT('Ctrl Pts',(7.9745694508469,13.7,29.5786915610044));
#113695=CARTESIAN_POINT('',(7.81865334794732,12.1,29.55));
#113696=CARTESIAN_POINT('',(7.81865334794732,14.,29.55));
#113697=CARTESIAN_POINT('',(7.81865334794732,12.1,29.55));
#113698=CARTESIAN_POINT('Origin',(8.01350906379882,12.1,29.6625));
#113699=CARTESIAN_POINT('',(8.12836477965032,12.1,29.9135640646055));
#113700=CARTESIAN_POINT('Origin',(8.12836477965032,14.,29.9135640646055));
#113701=CARTESIAN_POINT('Ctrl Pts',(7.92145902010118,13.7,29.6706815254679));
#113702=CARTESIAN_POINT('Ctrl Pts',(7.86828367243554,13.7778888548062,29.6082600467778));
#113703=CARTESIAN_POINT('Ctrl Pts',(7.81865334794732,13.85,29.55));
#113704=CARTESIAN_POINT('Origin',(7.97335450365041,14.,29.2182423009839));
#113705=CARTESIAN_POINT('',(7.97335450365041,13.85,29.2182423009839));
#113706=CARTESIAN_POINT('Ctrl Pts',(7.97335450365041,13.85,29.2182423009839));
#113707=CARTESIAN_POINT('Ctrl Pts',(8.04988604638594,13.7778888548064,29.2188124990598));
#113708=CARTESIAN_POINT('Ctrl Pts',(8.1318841278882,13.7,29.2194234255697));
#113709=CARTESIAN_POINT('',(7.97335450365041,12.1,29.2182423009839));
#113710=CARTESIAN_POINT('',(7.97335450365041,14.,29.2182423009839));
#113711=CARTESIAN_POINT('',(7.97335450365041,12.1,29.2182423009839));
#113712=CARTESIAN_POINT('Origin',(8.18478534332724,12.1,29.2951968332322));
#113713=CARTESIAN_POINT('',(8.34149296007196,12.1,29.5225021848062));
#113714=CARTESIAN_POINT('Origin',(8.34149296007196,14.,29.5225021848062));
#113715=CARTESIAN_POINT('Ctrl Pts',(8.09555445361673,13.7,29.3192383852867));
#113716=CARTESIAN_POINT('Ctrl Pts',(8.03234758294446,13.7778888548065,29.2669990313369));
#113717=CARTESIAN_POINT('Ctrl Pts',(7.97335450365041,13.85,29.2182423009839));
#113718=CARTESIAN_POINT('Origin',(8.06809628132564,14.,28.8646611731006));
#113719=CARTESIAN_POINT('',(8.06809628132564,13.85,28.8646611731006));
#113720=CARTESIAN_POINT('Ctrl Pts',(8.06809628132564,13.85,28.8646611731006));
#113721=CARTESIAN_POINT('Ctrl Pts',(8.1435641518183,13.7778888548065,28.8519331456564));
#113722=CARTESIAN_POINT('Ctrl Pts',(8.22442258448904,13.7,28.8382959733948));
#113723=CARTESIAN_POINT('',(8.06809628132564,12.1,28.8646611731006));
#113724=CARTESIAN_POINT('',(8.06809628132564,14.,28.8646611731006));
#113725=CARTESIAN_POINT('',(8.06809628132564,12.1,28.8646611731006));
#113726=CARTESIAN_POINT('Origin',(8.28967802575338,12.1,28.9037320130756));
#113727=CARTESIAN_POINT('',(8.48347606175442,12.1,29.1003720935326));
#113728=CARTESIAN_POINT('Origin',(8.48347606175442,14.,29.1003720935326));
#113729=CARTESIAN_POINT('Ctrl Pts',(8.20597752546084,13.7,28.9429031013232));
#113730=CARTESIAN_POINT('Ctrl Pts',(8.13465964056348,13.7778888548063,28.9024331384495));
#113731=CARTESIAN_POINT('Ctrl Pts',(8.06809628132564,13.85,28.8646611731006));
#113732=CARTESIAN_POINT('Origin',(8.1,14.,28.5));
#113733=CARTESIAN_POINT('',(8.1,13.85,28.5));
#113734=CARTESIAN_POINT('Ctrl Pts',(8.1,13.85,28.5));
#113735=CARTESIAN_POINT('Ctrl Pts',(8.17211114519331,13.7778888548067,28.474360481709));
#113736=CARTESIAN_POINT('Ctrl Pts',(8.24937308647232,13.7,28.4468895692543));
#113737=CARTESIAN_POINT('',(8.1,12.1,28.5));
#113738=CARTESIAN_POINT('',(8.1,14.,28.5));
#113739=CARTESIAN_POINT('',(8.1,12.1,28.5));
#113740=CARTESIAN_POINT('Origin',(8.325,12.1,28.5));
#113741=CARTESIAN_POINT('',(8.55,12.1,28.66));
#113742=CARTESIAN_POINT('Origin',(8.55,14.,28.66));
#113743=CARTESIAN_POINT('Ctrl Pts',(8.24937308647232,13.7,28.5531104307457));
#113744=CARTESIAN_POINT('Ctrl Pts',(8.17211114519331,13.7778888548067,28.525639518291));
#113745=CARTESIAN_POINT('Ctrl Pts',(8.1,13.85,28.5));
#113746=CARTESIAN_POINT('Origin',(6.,11.7,28.5));
#113747=CARTESIAN_POINT('Origin',(6.,11.7,26.45));
#113748=CARTESIAN_POINT('Origin',(6.,13.85,28.5));
#113749=CARTESIAN_POINT('',(4.05,14.,28.5));
#113750=CARTESIAN_POINT('Origin',(6.,14.,28.5));
#113751=CARTESIAN_POINT('',(3.9,13.85,28.5));
#113752=CARTESIAN_POINT('Origin',(6.,14.,28.5));
#113753=CARTESIAN_POINT('',(4.69529946162075,14.,28.5));
#113754=CARTESIAN_POINT('Origin',(6.,14.,28.5));
#113755=CARTESIAN_POINT('Origin',(6.,13.9,28.5));
#113756=CARTESIAN_POINT('',(4.84529946162075,13.85,28.5));
#113757=CARTESIAN_POINT('',(4.79529946162075,13.9,28.5));
#113758=CARTESIAN_POINT('',(4.89926025947012,13.8,28.4065371565079));
#113759=CARTESIAN_POINT('Ctrl Pts',(4.89926025947012,13.8,28.4065371565079));
#113760=CARTESIAN_POINT('Ctrl Pts',(4.87287693025568,13.8224225313651,28.4522344231802));
#113761=CARTESIAN_POINT('Ctrl Pts',(4.84529946162075,13.85,28.5));
#113762=CARTESIAN_POINT('',(5.368688932961,13.8,27.5934628434921));
#113763=CARTESIAN_POINT('Origin',(6.,13.8,28.5));
#113764=CARTESIAN_POINT('',(5.42264973081037,13.85,27.5));
#113765=CARTESIAN_POINT('Ctrl Pts',(5.42264973081037,13.85,27.5));
#113766=CARTESIAN_POINT('Ctrl Pts',(5.39507226217544,13.8224225313651,27.5477655768198));
#113767=CARTESIAN_POINT('Ctrl Pts',(5.368688932961,13.8,27.5934628434921));
#113768=CARTESIAN_POINT('',(5.53057132650912,13.8,27.5));
#113769=CARTESIAN_POINT('Ctrl Pts',(5.53057132650913,13.8,27.5));
#113770=CARTESIAN_POINT('Ctrl Pts',(5.47780466808023,13.8224225313651,27.5));
#113771=CARTESIAN_POINT('Ctrl Pts',(5.42264973081037,13.85,27.5));
#113772=CARTESIAN_POINT('',(6.46942867349088,13.8,27.5));
#113773=CARTESIAN_POINT('Origin',(6.,13.8,28.5));
#113774=CARTESIAN_POINT('',(6.57735026918963,13.85,27.5));
#113775=CARTESIAN_POINT('Ctrl Pts',(6.57735026918963,13.85,27.5));
#113776=CARTESIAN_POINT('Ctrl Pts',(6.52219533191977,13.8224225313651,27.5));
#113777=CARTESIAN_POINT('Ctrl Pts',(6.46942867349087,13.8,27.5));
#113778=CARTESIAN_POINT('',(6.631311067039,13.8,27.5934628434921));
#113779=CARTESIAN_POINT('Ctrl Pts',(6.631311067039,13.8,27.5934628434921));
#113780=CARTESIAN_POINT('Ctrl Pts',(6.60492773782455,13.8224225313651,27.5477655768198));
#113781=CARTESIAN_POINT('Ctrl Pts',(6.57735026918963,13.85,27.5));
#113782=CARTESIAN_POINT('',(7.10073974052988,13.8,28.4065371565079));
#113783=CARTESIAN_POINT('Origin',(6.,13.8,28.5));
#113784=CARTESIAN_POINT('',(7.15470053837925,13.85,28.5));
#113785=CARTESIAN_POINT('Ctrl Pts',(7.15470053837925,13.85,28.5));
#113786=CARTESIAN_POINT('Ctrl Pts',(7.12712306974432,13.8224225313651,28.4522344231802));
#113787=CARTESIAN_POINT('Ctrl Pts',(7.10073974052988,13.8,28.4065371565079));
#113788=CARTESIAN_POINT('',(7.10073974052988,13.8,28.5934628434921));
#113789=CARTESIAN_POINT('Ctrl Pts',(7.10073974052988,13.8,28.5934628434921));
#113790=CARTESIAN_POINT('Ctrl Pts',(7.12712306974432,13.8224225313651,28.5477655768198));
#113791=CARTESIAN_POINT('Ctrl Pts',(7.15470053837925,13.85,28.5));
#113792=CARTESIAN_POINT('',(6.631311067039,13.8,29.4065371565079));
#113793=CARTESIAN_POINT('Origin',(6.,13.8,28.5));
#113794=CARTESIAN_POINT('',(6.57735026918963,13.85,29.5));
#113795=CARTESIAN_POINT('Ctrl Pts',(6.57735026918963,13.85,29.5));
#113796=CARTESIAN_POINT('Ctrl Pts',(6.60492773782455,13.8224225313651,29.4522344231802));
#113797=CARTESIAN_POINT('Ctrl Pts',(6.631311067039,13.8,29.4065371565079));
#113798=CARTESIAN_POINT('',(6.46942867349088,13.8,29.5));
#113799=CARTESIAN_POINT('Ctrl Pts',(6.46942867349087,13.8,29.5));
#113800=CARTESIAN_POINT('Ctrl Pts',(6.52219533191977,13.8224225313651,29.5));
#113801=CARTESIAN_POINT('Ctrl Pts',(6.57735026918963,13.85,29.5));
#113802=CARTESIAN_POINT('',(5.53057132650912,13.8,29.5));
#113803=CARTESIAN_POINT('Origin',(6.,13.8,28.5));
#113804=CARTESIAN_POINT('',(5.42264973081037,13.85,29.5));
#113805=CARTESIAN_POINT('Ctrl Pts',(5.42264973081037,13.85,29.5));
#113806=CARTESIAN_POINT('Ctrl Pts',(5.47780466808023,13.8224225313651,29.5));
#113807=CARTESIAN_POINT('Ctrl Pts',(5.53057132650913,13.8,29.5));
#113808=CARTESIAN_POINT('',(5.368688932961,13.8,29.4065371565079));
#113809=CARTESIAN_POINT('Ctrl Pts',(5.368688932961,13.8,29.4065371565079));
#113810=CARTESIAN_POINT('Ctrl Pts',(5.39507226217544,13.8224225313651,29.4522344231802));
#113811=CARTESIAN_POINT('Ctrl Pts',(5.42264973081037,13.85,29.5));
#113812=CARTESIAN_POINT('',(4.89926025947012,13.8,28.5934628434921));
#113813=CARTESIAN_POINT('Origin',(6.,13.8,28.5));
#113814=CARTESIAN_POINT('Ctrl Pts',(4.84529946162075,13.85,28.5));
#113815=CARTESIAN_POINT('Ctrl Pts',(4.87287693025568,13.8224225313651,28.5477655768198));
#113816=CARTESIAN_POINT('Ctrl Pts',(4.89926025947012,13.8,28.5934628434921));
#113817=CARTESIAN_POINT('Origin',(6.,13.9,28.5));
#113818=CARTESIAN_POINT('',(6.46942867349088,14.,27.5));
#113819=CARTESIAN_POINT('',(6.46942867349088,13.9,27.5));
#113820=CARTESIAN_POINT('',(5.53057132650912,14.,27.5));
#113821=CARTESIAN_POINT('',(5.53057132650912,13.9,27.5));
#113822=CARTESIAN_POINT('Origin',(6.,14.,28.5));
#113823=CARTESIAN_POINT('Origin',(6.,13.9,28.5));
#113824=CARTESIAN_POINT('',(7.10073974052988,14.,28.4065371565079));
#113825=CARTESIAN_POINT('',(7.10073974052988,13.9,28.4065371565079));
#113826=CARTESIAN_POINT('',(6.631311067039,14.,27.5934628434921));
#113827=CARTESIAN_POINT('',(6.631311067039,13.9,27.5934628434921));
#113828=CARTESIAN_POINT('Origin',(6.,14.,28.5));
#113829=CARTESIAN_POINT('Origin',(6.,13.9,28.5));
#113830=CARTESIAN_POINT('',(4.89926025947012,14.,28.4065371565079));
#113831=CARTESIAN_POINT('',(4.89926025947012,13.9,28.4065371565079));
#113832=CARTESIAN_POINT('',(5.368688932961,14.,27.5934628434921));
#113833=CARTESIAN_POINT('Origin',(6.,14.,28.5));
#113834=CARTESIAN_POINT('',(5.368688932961,13.9,27.5934628434921));
#113835=CARTESIAN_POINT('Origin',(6.,13.9,28.5));
#113836=CARTESIAN_POINT('',(6.631311067039,14.,29.4065371565079));
#113837=CARTESIAN_POINT('',(6.631311067039,13.9,29.4065371565079));
#113838=CARTESIAN_POINT('',(7.10073974052988,14.,28.5934628434921));
#113839=CARTESIAN_POINT('',(7.10073974052988,13.9,28.5934628434921));
#113840=CARTESIAN_POINT('Origin',(6.,14.,28.5));
#113841=CARTESIAN_POINT('Origin',(6.,13.9,28.5));
#113842=CARTESIAN_POINT('',(5.368688932961,14.,29.4065371565079));
#113843=CARTESIAN_POINT('',(5.368688932961,13.9,29.4065371565079));
#113844=CARTESIAN_POINT('',(4.89926025947012,14.,28.5934628434921));
#113845=CARTESIAN_POINT('Origin',(6.,14.,28.5));
#113846=CARTESIAN_POINT('',(4.89926025947012,13.9,28.5934628434921));
#113847=CARTESIAN_POINT('Origin',(6.,13.9,28.5));
#113848=CARTESIAN_POINT('',(6.46942867349088,14.,29.5));
#113849=CARTESIAN_POINT('',(6.46942867349088,13.9,29.5));
#113850=CARTESIAN_POINT('',(5.53057132650912,14.,29.5));
#113851=CARTESIAN_POINT('Origin',(6.,14.,28.5));
#113852=CARTESIAN_POINT('',(5.53057132650912,13.9,29.5));
#113853=CARTESIAN_POINT('Origin',(7.15470053837925,14.,28.5));
#113854=CARTESIAN_POINT('',(7.01036297108184,14.,28.75));
#113855=CARTESIAN_POINT('',(7.15470053837925,12.9,28.5));
#113856=CARTESIAN_POINT('',(7.15470053837925,14.,28.5));
#113857=CARTESIAN_POINT('',(6.57735026918963,12.9,29.5));
#113858=CARTESIAN_POINT('',(7.15470053837925,12.9,28.5));
#113859=CARTESIAN_POINT('',(6.57735026918963,14.,29.5));
#113860=CARTESIAN_POINT('Origin',(6.57735026918963,14.,27.5));
#113861=CARTESIAN_POINT('',(6.72168783648703,14.,27.75));
#113862=CARTESIAN_POINT('',(6.57735026918963,12.9,27.5));
#113863=CARTESIAN_POINT('',(6.57735026918963,14.,27.5));
#113864=CARTESIAN_POINT('',(6.57735026918963,12.9,27.5));
#113865=CARTESIAN_POINT('Origin',(5.42264973081037,14.,27.5));
#113866=CARTESIAN_POINT('',(5.71132486540519,14.,27.5));
#113867=CARTESIAN_POINT('',(5.42264973081037,12.9,27.5));
#113868=CARTESIAN_POINT('',(5.42264973081037,14.,27.5));
#113869=CARTESIAN_POINT('',(5.42264973081037,12.9,27.5));
#113870=CARTESIAN_POINT('Origin',(6.,14.,28.5));
#113871=CARTESIAN_POINT('Origin',(6.,14.,28.5));
#113872=CARTESIAN_POINT('Origin',(6.,14.,28.5));
#113873=CARTESIAN_POINT('',(4.98963702891815,14.,28.25));
#113874=CARTESIAN_POINT('Origin',(6.,14.,28.5));
#113875=CARTESIAN_POINT('Origin',(6.,14.,28.5));
#113876=CARTESIAN_POINT('',(5.27831216351297,14.,29.25));
#113877=CARTESIAN_POINT('Origin',(6.,14.,28.5));
#113878=CARTESIAN_POINT('',(6.28867513459481,14.,29.5));
#113879=CARTESIAN_POINT('Origin',(7.15470053837925,12.9,28.5));
#113880=CARTESIAN_POINT('',(4.84529946162075,12.9,28.5));
#113881=CARTESIAN_POINT('',(4.84529946162075,12.9,28.5));
#113882=CARTESIAN_POINT('Origin',(6.,12.9,28.5));
#113883=CARTESIAN_POINT('Origin',(7.15470053837925,12.9,28.5));
#113884=CARTESIAN_POINT('Origin',(6.,12.9,28.5));
#113885=CARTESIAN_POINT('Origin',(7.15470053837925,12.9,28.5));
#113886=CARTESIAN_POINT('Origin',(6.,12.9,28.5));
#113887=CARTESIAN_POINT('Origin',(7.15470053837925,12.9,28.5));
#113888=CARTESIAN_POINT('Origin',(6.,12.9,28.5));
#113889=CARTESIAN_POINT('Origin',(7.15470053837925,12.9,28.5));
#113890=CARTESIAN_POINT('',(5.42264973081037,12.9,29.5));
#113891=CARTESIAN_POINT('',(6.57735026918963,12.9,29.5));
#113892=CARTESIAN_POINT('Origin',(6.,12.9,28.5));
#113893=CARTESIAN_POINT('Origin',(7.15470053837925,12.9,28.5));
#113894=CARTESIAN_POINT('',(5.42264973081037,12.9,29.5));
#113895=CARTESIAN_POINT('Origin',(6.,12.9,28.5));
#113896=CARTESIAN_POINT('Origin',(6.,12.9,28.5));
#113897=CARTESIAN_POINT('',(6.,12.206185919718,28.5));
#113898=CARTESIAN_POINT('',(4.84529946162075,12.9,28.5));
#113899=CARTESIAN_POINT('Origin',(4.84529946162075,14.,28.5));
#113900=CARTESIAN_POINT('',(4.84529946162075,14.,28.5));
#113901=CARTESIAN_POINT('Origin',(5.42264973081037,14.,29.5));
#113902=CARTESIAN_POINT('',(5.42264973081037,14.,29.5));
#113903=CARTESIAN_POINT('Origin',(6.57735026918963,14.,29.5));
#113904=CARTESIAN_POINT('',(0.,0.,0.));
#113905=CARTESIAN_POINT('Origin',(4.7,10.5,11.));
#113906=CARTESIAN_POINT('',(3.3,10.5,11.));
#113907=CARTESIAN_POINT('Origin',(4.,10.5,11.));
#113908=CARTESIAN_POINT('Origin',(4.,10.35,11.));
#113909=CARTESIAN_POINT('',(3.,10.2,11.));
#113910=CARTESIAN_POINT('Origin',(4.,10.2,11.));
#113911=CARTESIAN_POINT('',(3.15,10.35,11.));
#113912=CARTESIAN_POINT('Origin',(4.,7.5,11.));
#113913=CARTESIAN_POINT('',(3.,4.8,11.));
#113914=CARTESIAN_POINT('Origin',(4.,4.8,11.));
#113915=CARTESIAN_POINT('',(3.,7.5,11.));
#113916=CARTESIAN_POINT('Origin',(4.,4.65,11.));
#113917=CARTESIAN_POINT('',(3.3,4.5,11.));
#113918=CARTESIAN_POINT('Origin',(4.,4.5,11.));
#113919=CARTESIAN_POINT('',(3.15,4.65,11.));
#113920=CARTESIAN_POINT('Origin',(4.,4.5,11.));
#113921=CARTESIAN_POINT('',(0.,0.,0.));
#113922=CARTESIAN_POINT('',(0.,0.,0.));
#113923=CARTESIAN_POINT('',(0.,0.,0.));
#113924=CARTESIAN_POINT('',(0.,0.,0.));
#113925=CARTESIAN_POINT('',(0.,0.,0.));
#113926=CARTESIAN_POINT('',(0.,0.,0.));
#113927=CARTESIAN_POINT('',(0.,0.,0.));
#113928=CARTESIAN_POINT('',(0.,0.,0.));
#113929=CARTESIAN_POINT('',(0.,0.,0.));
#113930=CARTESIAN_POINT('',(0.,0.,0.));
#113931=CARTESIAN_POINT('',(0.,0.,0.));
#113932=CARTESIAN_POINT('',(0.,0.,0.));
#113933=CARTESIAN_POINT('',(0.,0.,0.));
#113934=CARTESIAN_POINT('',(0.,0.,0.));
#113935=CARTESIAN_POINT('',(0.,0.,0.));
#113936=CARTESIAN_POINT('',(0.,0.,0.));
#113937=CARTESIAN_POINT('',(0.,0.,0.));
#113938=CARTESIAN_POINT('',(0.,0.,0.));
#113939=CARTESIAN_POINT('',(24.,0.,0.));
#113940=CARTESIAN_POINT('',(0.,0.,2.5));
#113941=CARTESIAN_POINT('',(0.,0.,5.));
#113942=CARTESIAN_POINT('',(17.,0.,0.));
#113943=CARTESIAN_POINT('',(208.,0.,0.));
#113944=CARTESIAN_POINT('',(212.,0.,35.));
#113945=UNCERTAINTY_MEASURE_WITH_UNIT(LENGTH_MEASURE(0.01),#113985,
'DISTANCE_ACCURACY_VALUE',
'Maximum model space distance between geometric entities at asserted c
onnectivities');
#113946=UNCERTAINTY_MEASURE_WITH_UNIT(LENGTH_MEASURE(0.01),#113985,
'DISTANCE_ACCURACY_VALUE',
'Maximum model space distance between geometric entities at asserted c
onnectivities');
#113947=UNCERTAINTY_MEASURE_WITH_UNIT(LENGTH_MEASURE(0.01),#113985,
'DISTANCE_ACCURACY_VALUE',
'Maximum model space distance between geometric entities at asserted c
onnectivities');
#113948=UNCERTAINTY_MEASURE_WITH_UNIT(LENGTH_MEASURE(0.01),#113985,
'DISTANCE_ACCURACY_VALUE',
'Maximum model space distance between geometric entities at asserted c
onnectivities');
#113949=UNCERTAINTY_MEASURE_WITH_UNIT(LENGTH_MEASURE(0.01),#113985,
'DISTANCE_ACCURACY_VALUE',
'Maximum model space distance between geometric entities at asserted c
onnectivities');
#113950=UNCERTAINTY_MEASURE_WITH_UNIT(LENGTH_MEASURE(0.01),#113985,
'DISTANCE_ACCURACY_VALUE',
'Maximum model space distance between geometric entities at asserted c
onnectivities');
#113951=UNCERTAINTY_MEASURE_WITH_UNIT(LENGTH_MEASURE(0.01),#113985,
'DISTANCE_ACCURACY_VALUE',
'Maximum model space distance between geometric entities at asserted c
onnectivities');
#113952=UNCERTAINTY_MEASURE_WITH_UNIT(LENGTH_MEASURE(0.01),#113985,
'DISTANCE_ACCURACY_VALUE',
'Maximum model space distance between geometric entities at asserted c
onnectivities');
#113953=UNCERTAINTY_MEASURE_WITH_UNIT(LENGTH_MEASURE(0.01),#113985,
'DISTANCE_ACCURACY_VALUE',
'Maximum model space distance between geometric entities at asserted c
onnectivities');
#113954=UNCERTAINTY_MEASURE_WITH_UNIT(LENGTH_MEASURE(0.01),#113985,
'DISTANCE_ACCURACY_VALUE',
'Maximum model space distance between geometric entities at asserted c
onnectivities');
#113955=UNCERTAINTY_MEASURE_WITH_UNIT(LENGTH_MEASURE(0.01),#113985,
'DISTANCE_ACCURACY_VALUE',
'Maximum model space distance between geometric entities at asserted c
onnectivities');
#113956=UNCERTAINTY_MEASURE_WITH_UNIT(LENGTH_MEASURE(0.01),#113985,
'DISTANCE_ACCURACY_VALUE',
'Maximum model space distance between geometric entities at asserted c
onnectivities');
#113957=UNCERTAINTY_MEASURE_WITH_UNIT(LENGTH_MEASURE(0.01),#113985,
'DISTANCE_ACCURACY_VALUE',
'Maximum model space distance between geometric entities at asserted c
onnectivities');
#113958=UNCERTAINTY_MEASURE_WITH_UNIT(LENGTH_MEASURE(0.01),#113985,
'DISTANCE_ACCURACY_VALUE',
'Maximum model space distance between geometric entities at asserted c
onnectivities');
#113959=UNCERTAINTY_MEASURE_WITH_UNIT(LENGTH_MEASURE(0.01),#113985,
'DISTANCE_ACCURACY_VALUE',
'Maximum model space distance between geometric entities at asserted c
onnectivities');
#113960=UNCERTAINTY_MEASURE_WITH_UNIT(LENGTH_MEASURE(0.01),#113985,
'DISTANCE_ACCURACY_VALUE',
'Maximum model space distance between geometric entities at asserted c
onnectivities');
#113961=UNCERTAINTY_MEASURE_WITH_UNIT(LENGTH_MEASURE(0.01),#113985,
'DISTANCE_ACCURACY_VALUE',
'Maximum model space distance between geometric entities at asserted c
onnectivities');
#113962=UNCERTAINTY_MEASURE_WITH_UNIT(LENGTH_MEASURE(0.01),#113985,
'DISTANCE_ACCURACY_VALUE',
'Maximum model space distance between geometric entities at asserted c
onnectivities');
#113963=UNCERTAINTY_MEASURE_WITH_UNIT(LENGTH_MEASURE(0.01),#113985,
'DISTANCE_ACCURACY_VALUE',
'Maximum model space distance between geometric entities at asserted c
onnectivities');
#113964=UNCERTAINTY_MEASURE_WITH_UNIT(LENGTH_MEASURE(0.01),#113985,
'DISTANCE_ACCURACY_VALUE',
'Maximum model space distance between geometric entities at asserted c
onnectivities');
#113965=(
GEOMETRIC_REPRESENTATION_CONTEXT(3)
GLOBAL_UNCERTAINTY_ASSIGNED_CONTEXT((#113945))
GLOBAL_UNIT_ASSIGNED_CONTEXT((#113985,#113987,#113988))
REPRESENTATION_CONTEXT('','3D')
);
#113966=(
GEOMETRIC_REPRESENTATION_CONTEXT(3)
GLOBAL_UNCERTAINTY_ASSIGNED_CONTEXT((#113946))
GLOBAL_UNIT_ASSIGNED_CONTEXT((#113985,#113987,#113988))
REPRESENTATION_CONTEXT('','3D')
);
#113967=(
GEOMETRIC_REPRESENTATION_CONTEXT(3)
GLOBAL_UNCERTAINTY_ASSIGNED_CONTEXT((#113947))
GLOBAL_UNIT_ASSIGNED_CONTEXT((#113985,#113987,#113988))
REPRESENTATION_CONTEXT('','3D')
);
#113968=(
GEOMETRIC_REPRESENTATION_CONTEXT(3)
GLOBAL_UNCERTAINTY_ASSIGNED_CONTEXT((#113948))
GLOBAL_UNIT_ASSIGNED_CONTEXT((#113985,#113987,#113988))
REPRESENTATION_CONTEXT('','3D')
);
#113969=(
GEOMETRIC_REPRESENTATION_CONTEXT(3)
GLOBAL_UNCERTAINTY_ASSIGNED_CONTEXT((#113949))
GLOBAL_UNIT_ASSIGNED_CONTEXT((#113985,#113987,#113988))
REPRESENTATION_CONTEXT('','3D')
);
#113970=(
GEOMETRIC_REPRESENTATION_CONTEXT(3)
GLOBAL_UNCERTAINTY_ASSIGNED_CONTEXT((#113950))
GLOBAL_UNIT_ASSIGNED_CONTEXT((#113985,#113987,#113988))
REPRESENTATION_CONTEXT('','3D')
);
#113971=(
GEOMETRIC_REPRESENTATION_CONTEXT(3)
GLOBAL_UNCERTAINTY_ASSIGNED_CONTEXT((#113951))
GLOBAL_UNIT_ASSIGNED_CONTEXT((#113985,#113987,#113988))
REPRESENTATION_CONTEXT('','3D')
);
#113972=(
GEOMETRIC_REPRESENTATION_CONTEXT(3)
GLOBAL_UNCERTAINTY_ASSIGNED_CONTEXT((#113952))
GLOBAL_UNIT_ASSIGNED_CONTEXT((#113985,#113987,#113988))
REPRESENTATION_CONTEXT('','3D')
);
#113973=(
GEOMETRIC_REPRESENTATION_CONTEXT(3)
GLOBAL_UNCERTAINTY_ASSIGNED_CONTEXT((#113953))
GLOBAL_UNIT_ASSIGNED_CONTEXT((#113985,#113987,#113988))
REPRESENTATION_CONTEXT('','3D')
);
#113974=(
GEOMETRIC_REPRESENTATION_CONTEXT(3)
GLOBAL_UNCERTAINTY_ASSIGNED_CONTEXT((#113954))
GLOBAL_UNIT_ASSIGNED_CONTEXT((#113985,#113987,#113988))
REPRESENTATION_CONTEXT('','3D')
);
#113975=(
GEOMETRIC_REPRESENTATION_CONTEXT(3)
GLOBAL_UNCERTAINTY_ASSIGNED_CONTEXT((#113955))
GLOBAL_UNIT_ASSIGNED_CONTEXT((#113985,#113987,#113988))
REPRESENTATION_CONTEXT('','3D')
);
#113976=(
GEOMETRIC_REPRESENTATION_CONTEXT(3)
GLOBAL_UNCERTAINTY_ASSIGNED_CONTEXT((#113956))
GLOBAL_UNIT_ASSIGNED_CONTEXT((#113985,#113987,#113988))
REPRESENTATION_CONTEXT('','3D')
);
#113977=(
GEOMETRIC_REPRESENTATION_CONTEXT(3)
GLOBAL_UNCERTAINTY_ASSIGNED_CONTEXT((#113957))
GLOBAL_UNIT_ASSIGNED_CONTEXT((#113985,#113987,#113988))
REPRESENTATION_CONTEXT('','3D')
);
#113978=(
GEOMETRIC_REPRESENTATION_CONTEXT(3)
GLOBAL_UNCERTAINTY_ASSIGNED_CONTEXT((#113958))
GLOBAL_UNIT_ASSIGNED_CONTEXT((#113985,#113987,#113988))
REPRESENTATION_CONTEXT('','3D')
);
#113979=(
GEOMETRIC_REPRESENTATION_CONTEXT(3)
GLOBAL_UNCERTAINTY_ASSIGNED_CONTEXT((#113959))
GLOBAL_UNIT_ASSIGNED_CONTEXT((#113985,#113987,#113988))
REPRESENTATION_CONTEXT('','3D')
);
#113980=(
GEOMETRIC_REPRESENTATION_CONTEXT(3)
GLOBAL_UNCERTAINTY_ASSIGNED_CONTEXT((#113960))
GLOBAL_UNIT_ASSIGNED_CONTEXT((#113985,#113987,#113988))
REPRESENTATION_CONTEXT('','3D')
);
#113981=(
GEOMETRIC_REPRESENTATION_CONTEXT(3)
GLOBAL_UNCERTAINTY_ASSIGNED_CONTEXT((#113961))
GLOBAL_UNIT_ASSIGNED_CONTEXT((#113985,#113987,#113988))
REPRESENTATION_CONTEXT('','3D')
);
#113982=(
GEOMETRIC_REPRESENTATION_CONTEXT(3)
GLOBAL_UNCERTAINTY_ASSIGNED_CONTEXT((#113962))
GLOBAL_UNIT_ASSIGNED_CONTEXT((#113985,#113987,#113988))
REPRESENTATION_CONTEXT('','3D')
);
#113983=(
GEOMETRIC_REPRESENTATION_CONTEXT(3)
GLOBAL_UNCERTAINTY_ASSIGNED_CONTEXT((#113963))
GLOBAL_UNIT_ASSIGNED_CONTEXT((#113985,#113987,#113988))
REPRESENTATION_CONTEXT('','3D')
);
#113984=(
GEOMETRIC_REPRESENTATION_CONTEXT(3)
GLOBAL_UNCERTAINTY_ASSIGNED_CONTEXT((#113964))
GLOBAL_UNIT_ASSIGNED_CONTEXT((#113985,#113987,#113988))
REPRESENTATION_CONTEXT('','3D')
);
#113985=(
LENGTH_UNIT()
NAMED_UNIT(*)
SI_UNIT(.MILLI.,.METRE.)
);
#113986=(
LENGTH_UNIT()
NAMED_UNIT(*)
SI_UNIT($,.METRE.)
);
#113987=(
NAMED_UNIT(*)
PLANE_ANGLE_UNIT()
SI_UNIT($,.RADIAN.)
);
#113988=(
NAMED_UNIT(*)
SI_UNIT($,.STERADIAN.)
SOLID_ANGLE_UNIT()
);
#113989=SHAPE_DEFINITION_REPRESENTATION(#114008,#114051);
#113990=SHAPE_DEFINITION_REPRESENTATION(#114009,#114052);
#113991=SHAPE_DEFINITION_REPRESENTATION(#114010,#114053);
#113992=SHAPE_DEFINITION_REPRESENTATION(#114011,#114054);
#113993=SHAPE_DEFINITION_REPRESENTATION(#114012,#114055);
#113994=SHAPE_DEFINITION_REPRESENTATION(#114013,#114056);
#113995=SHAPE_DEFINITION_REPRESENTATION(#114014,#114057);
#113996=SHAPE_DEFINITION_REPRESENTATION(#114015,#114058);
#113997=SHAPE_DEFINITION_REPRESENTATION(#114016,#114059);
#113998=SHAPE_DEFINITION_REPRESENTATION(#114017,#114060);
#113999=SHAPE_DEFINITION_REPRESENTATION(#114018,#114061);
#114000=SHAPE_DEFINITION_REPRESENTATION(#114019,#114062);
#114001=SHAPE_DEFINITION_REPRESENTATION(#114020,#114063);
#114002=SHAPE_DEFINITION_REPRESENTATION(#114021,#114064);
#114003=SHAPE_DEFINITION_REPRESENTATION(#114022,#114065);
#114004=SHAPE_DEFINITION_REPRESENTATION(#114023,#114066);
#114005=SHAPE_DEFINITION_REPRESENTATION(#114024,#114067);
#114006=SHAPE_DEFINITION_REPRESENTATION(#114025,#114068);
#114007=SHAPE_DEFINITION_REPRESENTATION(#114026,#114069);
#114008=PRODUCT_DEFINITION_SHAPE('',$,#114071);
#114009=PRODUCT_DEFINITION_SHAPE('',$,#114072);
#114010=PRODUCT_DEFINITION_SHAPE('',$,#114073);
#114011=PRODUCT_DEFINITION_SHAPE('',$,#114074);
#114012=PRODUCT_DEFINITION_SHAPE('',$,#114075);
#114013=PRODUCT_DEFINITION_SHAPE('',$,#114076);
#114014=PRODUCT_DEFINITION_SHAPE('',$,#114077);
#114015=PRODUCT_DEFINITION_SHAPE('',$,#114078);
#114016=PRODUCT_DEFINITION_SHAPE('',$,#114079);
#114017=PRODUCT_DEFINITION_SHAPE('',$,#114080);
#114018=PRODUCT_DEFINITION_SHAPE('',$,#114081);
#114019=PRODUCT_DEFINITION_SHAPE('',$,#114082);
#114020=PRODUCT_DEFINITION_SHAPE('',$,#114083);
#114021=PRODUCT_DEFINITION_SHAPE('',$,#114084);
#114022=PRODUCT_DEFINITION_SHAPE('',$,#114085);
#114023=PRODUCT_DEFINITION_SHAPE('',$,#114086);
#114024=PRODUCT_DEFINITION_SHAPE('',$,#114087);
#114025=PRODUCT_DEFINITION_SHAPE('',$,#114088);
#114026=PRODUCT_DEFINITION_SHAPE('',$,#114089);
#114027=PRODUCT_DEFINITION_SHAPE($,$,#83);
#114028=PRODUCT_DEFINITION_SHAPE($,$,#84);
#114029=PRODUCT_DEFINITION_SHAPE($,$,#85);
#114030=PRODUCT_DEFINITION_SHAPE($,$,#86);
#114031=PRODUCT_DEFINITION_SHAPE($,$,#87);
#114032=PRODUCT_DEFINITION_SHAPE($,$,#88);
#114033=PRODUCT_DEFINITION_SHAPE($,$,#89);
#114034=PRODUCT_DEFINITION_SHAPE($,$,#90);
#114035=PRODUCT_DEFINITION_SHAPE($,$,#91);
#114036=PRODUCT_DEFINITION_SHAPE($,$,#92);
#114037=PRODUCT_DEFINITION_SHAPE($,$,#93);
#114038=PRODUCT_DEFINITION_SHAPE($,$,#94);
#114039=PRODUCT_DEFINITION_SHAPE($,$,#95);
#114040=PRODUCT_DEFINITION_SHAPE($,$,#96);
#114041=PRODUCT_DEFINITION_SHAPE($,$,#97);
#114042=PRODUCT_DEFINITION_SHAPE($,$,#98);
#114043=PRODUCT_DEFINITION_SHAPE($,$,#99);
#114044=PRODUCT_DEFINITION_SHAPE($,$,#100);
#114045=PRODUCT_DEFINITION_SHAPE($,$,#101);
#114046=PRODUCT_DEFINITION_SHAPE($,$,#102);
#114047=PRODUCT_DEFINITION_SHAPE($,$,#103);
#114048=PRODUCT_DEFINITION_SHAPE($,$,#104);
#114049=PRODUCT_DEFINITION_SHAPE($,$,#105);
#114050=PRODUCT_DEFINITION_SHAPE($,$,#106);
#114051=SHAPE_REPRESENTATION('',(#60609,#63752,#63753,#63754,#63755,#63756,
#63757,#63758,#63759,#63760,#63761,#63762,#63763,#63764,#63765,#63766,#63767,
#63768,#63769,#63770,#63771,#63772,#63773,#63774,#63775),#113965);
#114052=SHAPE_REPRESENTATION('',(#60610),#113966);
#114053=SHAPE_REPRESENTATION('',(#61812),#113967);
#114054=SHAPE_REPRESENTATION('',(#61948),#113968);
#114055=SHAPE_REPRESENTATION('',(#61969),#113969);
#114056=SHAPE_REPRESENTATION('',(#61989),#113970);
#114057=SHAPE_REPRESENTATION('',(#62138),#113971);
#114058=SHAPE_REPRESENTATION('',(#62375),#113972);
#114059=SHAPE_REPRESENTATION('',(#62396),#113973);
#114060=SHAPE_REPRESENTATION('',(#62923),#113974);
#114061=SHAPE_REPRESENTATION('',(#62957),#113975);
#114062=SHAPE_REPRESENTATION('',(#63058),#113976);
#114063=SHAPE_REPRESENTATION('',(#63115),#113977);
#114064=SHAPE_REPRESENTATION('',(#63188),#113978);
#114065=SHAPE_REPRESENTATION('',(#63259),#113979);
#114066=SHAPE_REPRESENTATION('',(#63344),#113980);
#114067=SHAPE_REPRESENTATION('',(#63421),#113981);
#114068=SHAPE_REPRESENTATION('',(#63462),#113982);
#114069=SHAPE_REPRESENTATION('',(#63742),#113983);
#114070=PRODUCT_DEFINITION_CONTEXT('part definition',#114129,'design');
#114071=PRODUCT_DEFINITION('2026-10-05-09-42-25-171','MAS-254',#114090,
#114070);
#114072=PRODUCT_DEFINITION('2026-10-05-09-42-27-850',
'Cast Iron Dovetail Base Block LWX40 x 220',#114091,#114070);
#114073=PRODUCT_DEFINITION('2026-10-05-09-48-36-190',
'Machined Alloy Sliding Carriage 40 x 40',#114092,#114070);
#114074=PRODUCT_DEFINITION('2026-10-05-09-48-59-239',
'Adjustable Brass Gib Strip',#114093,#114070);
#114075=PRODUCT_DEFINITION('2026-10-05-09-49-04-660',
'Precision Drive Spindle D5 (knob shaft)',#114094,#114070);
#114076=PRODUCT_DEFINITION('2026-10-05-09-49-09-808',
'Spur Pinion m0.5 z16 with Hub',#114095,#114070);
#114077=PRODUCT_DEFINITION('2026-10-05-09-49-16-336',
'Knurled Adjustment Knob D20',#114096,#114070);
#114078=PRODUCT_DEFINITION('2026-10-05-09-49-27-315',
'Sintered Bronze Flanged Bush 5 x 9.6 x 8',#114097,#114070);
#114079=PRODUCT_DEFINITION('2026-10-05-09-49-30-957',
'Carriage Drive Gear Rack m0.5 x 6 x 216',#114098,#114070);
#114080=PRODUCT_DEFINITION('2026-10-05-09-50-45-275',
'Base Lock Knob Lever (stainless, bent)',#114099,#114070);
#114081=PRODUCT_DEFINITION('2026-10-05-09-50-52-624',
'Scale Pointer - Vernier Plate',#114100,#114070);
#114082=PRODUCT_DEFINITION('2026-10-05-09-51-16-067',
'ISO 1207 - M4 x 8 - 4.8 (Lock Clamp Screw, slotted cheese head)',#114101,
#114070);
#114083=PRODUCT_DEFINITION('2026-10-05-09-51-47-617',
'ISO 4026 - M3 x 3 - 45H (Knob Set Screw)',#114102,#114070);
#114084=PRODUCT_DEFINITION('2026-10-05-09-52-00-488',
'ISO 4026 - M2 x 2 - 45H (Pinion Set Screw)',#114103,#114070);
#114085=PRODUCT_DEFINITION('2026-10-05-09-51-27-046',
'ISO 4026 - M3 x 6 - 45H (Gib Adjustment Screw)',#114104,#114070);
#114086=PRODUCT_DEFINITION('2026-10-05-09-51-36-343',
'ISO 4026 - M3 x 4 - 45H (Bush Retaining Screw)',#114105,#114070);
#114087=PRODUCT_DEFINITION('2026-10-05-09-51-21-964',
'ISO 10642 - M2 x 4 - 10.9 (Pointer Screw)',#114106,#114070);
#114088=PRODUCT_DEFINITION('2026-10-05-09-52-12-383',
'ISO 4762 - M2.5 x 6 - 12.9 (Rack Screw)',#114107,#114070);
#114089=PRODUCT_DEFINITION('2026-10-05-09-51-13-557',
'ISO 2338 - 2 m6 x 6 - St (Carriage Travel Stop Pin)',#114108,#114070);
#114090=PRODUCT_DEFINITION_FORMATION('',$,#114131);
#114091=PRODUCT_DEFINITION_FORMATION('',$,#114132);
#114092=PRODUCT_DEFINITION_FORMATION('',$,#114133);
#114093=PRODUCT_DEFINITION_FORMATION('',$,#114134);
#114094=PRODUCT_DEFINITION_FORMATION('',$,#114135);
#114095=PRODUCT_DEFINITION_FORMATION('',$,#114136);
#114096=PRODUCT_DEFINITION_FORMATION('',$,#114137);
#114097=PRODUCT_DEFINITION_FORMATION('',$,#114138);
#114098=PRODUCT_DEFINITION_FORMATION('',$,#114139);
#114099=PRODUCT_DEFINITION_FORMATION('',$,#114140);
#114100=PRODUCT_DEFINITION_FORMATION('',$,#114141);
#114101=PRODUCT_DEFINITION_FORMATION('',$,#114142);
#114102=PRODUCT_DEFINITION_FORMATION('',$,#114143);
#114103=PRODUCT_DEFINITION_FORMATION('',$,#114144);
#114104=PRODUCT_DEFINITION_FORMATION('',$,#114145);
#114105=PRODUCT_DEFINITION_FORMATION('',$,#114146);
#114106=PRODUCT_DEFINITION_FORMATION('',$,#114147);
#114107=PRODUCT_DEFINITION_FORMATION('',$,#114148);
#114108=PRODUCT_DEFINITION_FORMATION('',$,#114149);
#114109=PRODUCT_RELATED_PRODUCT_CATEGORY('MAS-254','MAS-254',(#114131));
#114110=PRODUCT_RELATED_PRODUCT_CATEGORY(
'Cast Iron Dovetail Base Block LWX40 x 220',
'Cast Iron Dovetail Base Block LWX40 x 220',(#114132));
#114111=PRODUCT_RELATED_PRODUCT_CATEGORY(
'Machined Alloy Sliding Carriage 40 x 40',
'Machined Alloy Sliding Carriage 40 x 40',(#114133));
#114112=PRODUCT_RELATED_PRODUCT_CATEGORY('Adjustable Brass Gib Strip',
'Adjustable Brass Gib Strip',(#114134));
#114113=PRODUCT_RELATED_PRODUCT_CATEGORY(
'Precision Drive Spindle D5 (knob shaft)',
'Precision Drive Spindle D5 (knob shaft)',(#114135));
#114114=PRODUCT_RELATED_PRODUCT_CATEGORY(
'Spur Pinion m0.5 z16 with Hub','Spur Pinion m0.5 z16 with Hub',(#114136));
#114115=PRODUCT_RELATED_PRODUCT_CATEGORY('Knurled Adjustment Knob D20',
'Knurled Adjustment Knob D20',(#114137));
#114116=PRODUCT_RELATED_PRODUCT_CATEGORY(
'Sintered Bronze Flanged Bush 5 x 9.6 x 8',
'Sintered Bronze Flanged Bush 5 x 9.6 x 8',(#114138));
#114117=PRODUCT_RELATED_PRODUCT_CATEGORY(
'Carriage Drive Gear Rack m0.5 x 6 x 216',
'Carriage Drive Gear Rack m0.5 x 6 x 216',(#114139));
#114118=PRODUCT_RELATED_PRODUCT_CATEGORY(
'Base Lock Knob Lever (stainless, bent)',
'Base Lock Knob Lever (stainless, bent)',(#114140));
#114119=PRODUCT_RELATED_PRODUCT_CATEGORY(
'Scale Pointer - Vernier Plate','Scale Pointer - Vernier Plate',(#114141));
#114120=PRODUCT_RELATED_PRODUCT_CATEGORY(
'ISO 1207 - M4 x 8 - 4.8 (Lock Clamp Screw, slotted cheese head)',
'ISO 1207 - M4 x 8 - 4.8 (Lock Clamp Screw, slotted cheese head)',(#114142));
#114121=PRODUCT_RELATED_PRODUCT_CATEGORY(
'ISO 4026 - M3 x 3 - 45H (Knob Set Screw)',
'ISO 4026 - M3 x 3 - 45H (Knob Set Screw)',(#114143));
#114122=PRODUCT_RELATED_PRODUCT_CATEGORY(
'ISO 4026 - M2 x 2 - 45H (Pinion Set Screw)',
'ISO 4026 - M2 x 2 - 45H (Pinion Set Screw)',(#114144));
#114123=PRODUCT_RELATED_PRODUCT_CATEGORY(
'ISO 4026 - M3 x 6 - 45H (Gib Adjustment Screw)',
'ISO 4026 - M3 x 6 - 45H (Gib Adjustment Screw)',(#114145));
#114124=PRODUCT_RELATED_PRODUCT_CATEGORY(
'ISO 4026 - M3 x 4 - 45H (Bush Retaining Screw)',
'ISO 4026 - M3 x 4 - 45H (Bush Retaining Screw)',(#114146));
#114125=PRODUCT_RELATED_PRODUCT_CATEGORY(
'ISO 10642 - M2 x 4 - 10.9 (Pointer Screw)',
'ISO 10642 - M2 x 4 - 10.9 (Pointer Screw)',(#114147));
#114126=PRODUCT_RELATED_PRODUCT_CATEGORY(
'ISO 4762 - M2.5 x 6 - 12.9 (Rack Screw)',
'ISO 4762 - M2.5 x 6 - 12.9 (Rack Screw)',(#114148));
#114127=PRODUCT_RELATED_PRODUCT_CATEGORY(
'ISO 2338 - 2 m6 x 6 - St (Carriage Travel Stop Pin)',
'ISO 2338 - 2 m6 x 6 - St (Carriage Travel Stop Pin)',(#114149));
#114128=APPLICATION_PROTOCOL_DEFINITION('international standard',
'automotive_design',2009,#114129);
#114129=APPLICATION_CONTEXT(
'Core Data for Automotive Mechanical Design Process');
#114130=PRODUCT_CONTEXT('part definition',#114129,'mechanical');
#114131=PRODUCT('2026-10-05-09-42-25-171','MAS-254',$,(#114130));
#114132=PRODUCT('2026-10-05-09-42-27-850',
'Cast Iron Dovetail Base Block LWX40 x 220',$,(#114130));
#114133=PRODUCT('2026-10-05-09-48-36-190',
'Machined Alloy Sliding Carriage 40 x 40',$,(#114130));
#114134=PRODUCT('2026-10-05-09-48-59-239','Adjustable Brass Gib Strip',
$,(#114130));
#114135=PRODUCT('2026-10-05-09-49-04-660',
'Precision Drive Spindle D5 (knob shaft)',$,(#114130));
#114136=PRODUCT('2026-10-05-09-49-09-808',
'Spur Pinion m0.5 z16 with Hub',$,(#114130));
#114137=PRODUCT('2026-10-05-09-49-16-336','Knurled Adjustment Knob D20',
$,(#114130));
#114138=PRODUCT('2026-10-05-09-49-27-315',
'Sintered Bronze Flanged Bush 5 x 9.6 x 8',$,(#114130));
#114139=PRODUCT('2026-10-05-09-49-30-957',
'Carriage Drive Gear Rack m0.5 x 6 x 216',$,(#114130));
#114140=PRODUCT('2026-10-05-09-50-45-275',
'Base Lock Knob Lever (stainless, bent)',$,(#114130));
#114141=PRODUCT('2026-10-05-09-50-52-624',
'Scale Pointer - Vernier Plate',$,(#114130));
#114142=PRODUCT('2026-10-05-09-51-16-067',
'ISO 1207 - M4 x 8 - 4.8 (Lock Clamp Screw, slotted cheese head)',$,(#114130));
#114143=PRODUCT('2026-10-05-09-51-47-617',
'ISO 4026 - M3 x 3 - 45H (Knob Set Screw)',$,(#114130));
#114144=PRODUCT('2026-10-05-09-52-00-488',
'ISO 4026 - M2 x 2 - 45H (Pinion Set Screw)',$,(#114130));
#114145=PRODUCT('2026-10-05-09-51-27-046',
'ISO 4026 - M3 x 6 - 45H (Gib Adjustment Screw)',$,(#114130));
#114146=PRODUCT('2026-10-05-09-51-36-343',
'ISO 4026 - M3 x 4 - 45H (Bush Retaining Screw)',$,(#114130));
#114147=PRODUCT('2026-10-05-09-51-21-964',
'ISO 10642 - M2 x 4 - 10.9 (Pointer Screw)',$,(#114130));
#114148=PRODUCT('2026-10-05-09-52-12-383',
'ISO 4762 - M2.5 x 6 - 12.9 (Rack Screw)',$,(#114130));
#114149=PRODUCT('2026-10-05-09-51-13-557',
'ISO 2338 - 2 m6 x 6 - St (Carriage Travel Stop Pin)',$,(#114130));
#114150=PRESENTATION_STYLE_ASSIGNMENT((#114169));
#114151=PRESENTATION_STYLE_ASSIGNMENT((#114170));
#114152=PRESENTATION_STYLE_ASSIGNMENT((#114171));
#114153=PRESENTATION_STYLE_ASSIGNMENT((#114172));
#114154=PRESENTATION_STYLE_ASSIGNMENT((#114173));
#114155=PRESENTATION_STYLE_ASSIGNMENT((#114174));
#114156=PRESENTATION_STYLE_ASSIGNMENT((#114175));
#114157=PRESENTATION_STYLE_ASSIGNMENT((#114176));
#114158=PRESENTATION_STYLE_ASSIGNMENT((#114177));
#114159=PRESENTATION_STYLE_ASSIGNMENT((#114178));
#114160=PRESENTATION_STYLE_ASSIGNMENT((#114179));
#114161=PRESENTATION_STYLE_ASSIGNMENT((#114180));
#114162=PRESENTATION_STYLE_ASSIGNMENT((#114181));
#114163=PRESENTATION_STYLE_ASSIGNMENT((#114182));
#114164=PRESENTATION_STYLE_ASSIGNMENT((#114183));
#114165=PRESENTATION_STYLE_ASSIGNMENT((#114184));
#114166=PRESENTATION_STYLE_ASSIGNMENT((#114185));
#114167=PRESENTATION_STYLE_ASSIGNMENT((#114186));
#114168=PRESENTATION_STYLE_ASSIGNMENT((#114187));
#114169=SURFACE_STYLE_USAGE(.BOTH.,#114188);
#114170=SURFACE_STYLE_USAGE(.BOTH.,#114189);
#114171=SURFACE_STYLE_USAGE(.BOTH.,#114190);
#114172=SURFACE_STYLE_USAGE(.BOTH.,#114191);
#114173=SURFACE_STYLE_USAGE(.BOTH.,#114192);
#114174=SURFACE_STYLE_USAGE(.BOTH.,#114193);
#114175=SURFACE_STYLE_USAGE(.BOTH.,#114194);
#114176=SURFACE_STYLE_USAGE(.BOTH.,#114195);
#114177=SURFACE_STYLE_USAGE(.BOTH.,#114196);
#114178=SURFACE_STYLE_USAGE(.BOTH.,#114197);
#114179=SURFACE_STYLE_USAGE(.BOTH.,#114198);
#114180=SURFACE_STYLE_USAGE(.BOTH.,#114199);
#114181=SURFACE_STYLE_USAGE(.BOTH.,#114200);
#114182=SURFACE_STYLE_USAGE(.BOTH.,#114201);
#114183=SURFACE_STYLE_USAGE(.BOTH.,#114202);
#114184=SURFACE_STYLE_USAGE(.BOTH.,#114203);
#114185=SURFACE_STYLE_USAGE(.BOTH.,#114204);
#114186=SURFACE_STYLE_USAGE(.BOTH.,#114205);
#114187=SURFACE_STYLE_USAGE(.BOTH.,#114206);
#114188=SURFACE_SIDE_STYLE('',(#114207));
#114189=SURFACE_SIDE_STYLE('',(#114208));
#114190=SURFACE_SIDE_STYLE('',(#114209));
#114191=SURFACE_SIDE_STYLE('',(#114210));
#114192=SURFACE_SIDE_STYLE('',(#114211));
#114193=SURFACE_SIDE_STYLE('',(#114212));
#114194=SURFACE_SIDE_STYLE('',(#114213));
#114195=SURFACE_SIDE_STYLE('',(#114214));
#114196=SURFACE_SIDE_STYLE('',(#114215));
#114197=SURFACE_SIDE_STYLE('',(#114216));
#114198=SURFACE_SIDE_STYLE('',(#114217));
#114199=SURFACE_SIDE_STYLE('',(#114218));
#114200=SURFACE_SIDE_STYLE('',(#114219));
#114201=SURFACE_SIDE_STYLE('',(#114220));
#114202=SURFACE_SIDE_STYLE('',(#114221));
#114203=SURFACE_SIDE_STYLE('',(#114222));
#114204=SURFACE_SIDE_STYLE('',(#114223));
#114205=SURFACE_SIDE_STYLE('',(#114224));
#114206=SURFACE_SIDE_STYLE('',(#114225));
#114207=SURFACE_STYLE_FILL_AREA(#114226);
#114208=SURFACE_STYLE_FILL_AREA(#114227);
#114209=SURFACE_STYLE_FILL_AREA(#114228);
#114210=SURFACE_STYLE_FILL_AREA(#114229);
#114211=SURFACE_STYLE_FILL_AREA(#114230);
#114212=SURFACE_STYLE_FILL_AREA(#114231);
#114213=SURFACE_STYLE_FILL_AREA(#114232);
#114214=SURFACE_STYLE_FILL_AREA(#114233);
#114215=SURFACE_STYLE_FILL_AREA(#114234);
#114216=SURFACE_STYLE_FILL_AREA(#114235);
#114217=SURFACE_STYLE_FILL_AREA(#114236);
#114218=SURFACE_STYLE_FILL_AREA(#114237);
#114219=SURFACE_STYLE_FILL_AREA(#114238);
#114220=SURFACE_STYLE_FILL_AREA(#114239);
#114221=SURFACE_STYLE_FILL_AREA(#114240);
#114222=SURFACE_STYLE_FILL_AREA(#114241);
#114223=SURFACE_STYLE_FILL_AREA(#114242);
#114224=SURFACE_STYLE_FILL_AREA(#114243);
#114225=SURFACE_STYLE_FILL_AREA(#114244);
#114226=FILL_AREA_STYLE('Steel - Satin',(#114245));
#114227=FILL_AREA_STYLE(
'MAS-255 Metallic Sheet - Cast Iron Dovetail Base Block LWX40 x 22',(#114246));
#114228=FILL_AREA_STYLE(
'MAS-255 Metallic Sheet - Machined Alloy Sliding Carriage 40 x 40',(#114247));
#114229=FILL_AREA_STYLE(
'MAS-255 Metallic Sheet - Adjustable Brass Gib Strip',(#114248));
#114230=FILL_AREA_STYLE(
'MAS-255 Metallic Sheet - Precision Drive Spindle D5 (knob shaft)',(#114249));
#114231=FILL_AREA_STYLE(
'MAS-255 Metallic Sheet - Spur Pinion m0.5 z16 with Hub',(#114250));
#114232=FILL_AREA_STYLE(
'MAS-255 Metallic Sheet - Knurled Adjustment Knob D20',(#114251));
#114233=FILL_AREA_STYLE(
'MAS-255 Metallic Sheet - Sintered Bronze Flanged Bush 5 x 9.6 x 8',(#114252));
#114234=FILL_AREA_STYLE(
'MAS-255 Metallic Sheet - Carriage Drive Gear Rack m0.5 x 6 x 216',(#114253));
#114235=FILL_AREA_STYLE(
'MAS-255 Metallic Sheet - Base Lock Knob Lever (stainless, bent)',(#114254));
#114236=FILL_AREA_STYLE(
'MAS-255 Metallic Sheet - Scale Pointer - Vernier Plate',(#114255));
#114237=FILL_AREA_STYLE(
'MAS-255 Metallic Sheet - ISO 1207 - M4 x 8 - 4.8 (Lock Clamp Scre',(#114256));
#114238=FILL_AREA_STYLE(
'MAS-255 Metallic Sheet - ISO 4026 - M3 x 3 - 45H (Knob Set Screw)',(#114257));
#114239=FILL_AREA_STYLE(
'MAS-255 Metallic Sheet - ISO 4026 - M2 x 2 - 45H (Pinion Set Scre',(#114258));
#114240=FILL_AREA_STYLE(
'MAS-255 Metallic Sheet - ISO 4026 - M3 x 6 - 45H (Gib Adjustment',(#114259));
#114241=FILL_AREA_STYLE(
'MAS-255 Metallic Sheet - ISO 4026 - M3 x 4 - 45H (Bush Retaining',(#114260));
#114242=FILL_AREA_STYLE(
'MAS-255 Metallic Sheet - ISO 10642 - M2 x 4 - 10.9 (Pointer Screw',(#114261));
#114243=FILL_AREA_STYLE(
'MAS-255 Metallic Sheet - ISO 4762 - M2.5 x 6 - 12.9 (Rack Screw)',(#114262));
#114244=FILL_AREA_STYLE(
'MAS-255 Metallic Sheet - ISO 2338 - 2 m6 x 6 - St (Carriage Trave',(#114263));
#114245=FILL_AREA_STYLE_COLOUR('Steel - Satin',#114264);
#114246=FILL_AREA_STYLE_COLOUR(
'MAS-255 Metallic Sheet - Cast Iron Dovetail Base Block LWX40 x 22',#114265);
#114247=FILL_AREA_STYLE_COLOUR(
'MAS-255 Metallic Sheet - Machined Alloy Sliding Carriage 40 x 40',#114266);
#114248=FILL_AREA_STYLE_COLOUR(
'MAS-255 Metallic Sheet - Adjustable Brass Gib Strip',#114267);
#114249=FILL_AREA_STYLE_COLOUR(
'MAS-255 Metallic Sheet - Precision Drive Spindle D5 (knob shaft)',#114268);
#114250=FILL_AREA_STYLE_COLOUR(
'MAS-255 Metallic Sheet - Spur Pinion m0.5 z16 with Hub',#114269);
#114251=FILL_AREA_STYLE_COLOUR(
'MAS-255 Metallic Sheet - Knurled Adjustment Knob D20',#114270);
#114252=FILL_AREA_STYLE_COLOUR(
'MAS-255 Metallic Sheet - Sintered Bronze Flanged Bush 5 x 9.6 x 8',#114271);
#114253=FILL_AREA_STYLE_COLOUR(
'MAS-255 Metallic Sheet - Carriage Drive Gear Rack m0.5 x 6 x 216',#114272);
#114254=FILL_AREA_STYLE_COLOUR(
'MAS-255 Metallic Sheet - Base Lock Knob Lever (stainless, bent)',#114273);
#114255=FILL_AREA_STYLE_COLOUR(
'MAS-255 Metallic Sheet - Scale Pointer - Vernier Plate',#114274);
#114256=FILL_AREA_STYLE_COLOUR(
'MAS-255 Metallic Sheet - ISO 1207 - M4 x 8 - 4.8 (Lock Clamp Scre',#114275);
#114257=FILL_AREA_STYLE_COLOUR(
'MAS-255 Metallic Sheet - ISO 4026 - M3 x 3 - 45H (Knob Set Screw)',#114276);
#114258=FILL_AREA_STYLE_COLOUR(
'MAS-255 Metallic Sheet - ISO 4026 - M2 x 2 - 45H (Pinion Set Scre',#114277);
#114259=FILL_AREA_STYLE_COLOUR(
'MAS-255 Metallic Sheet - ISO 4026 - M3 x 6 - 45H (Gib Adjustment',#114278);
#114260=FILL_AREA_STYLE_COLOUR(
'MAS-255 Metallic Sheet - ISO 4026 - M3 x 4 - 45H (Bush Retaining',#114279);
#114261=FILL_AREA_STYLE_COLOUR(
'MAS-255 Metallic Sheet - ISO 10642 - M2 x 4 - 10.9 (Pointer Screw',#114280);
#114262=FILL_AREA_STYLE_COLOUR(
'MAS-255 Metallic Sheet - ISO 4762 - M2.5 x 6 - 12.9 (Rack Screw)',#114281);
#114263=FILL_AREA_STYLE_COLOUR(
'MAS-255 Metallic Sheet - ISO 2338 - 2 m6 x 6 - St (Carriage Trave',#114282);
#114264=COLOUR_RGB('Steel - Satin',0.627450980392157,0.627450980392157,
0.627450980392157);
#114265=COLOUR_RGB(
'MAS-255 Metallic Sheet - Cast Iron Dovetail Base Block LWX40 x 22',0.807843137254902,
0.823529411764706,0.847058823529412);
#114266=COLOUR_RGB(
'MAS-255 Metallic Sheet - Machined Alloy Sliding Carriage 40 x 40',0.870588235294118,
0.882352941176471,0.901960784313726);
#114267=COLOUR_RGB(
'MAS-255 Metallic Sheet - Adjustable Brass Gib Strip',0.83921568627451,
0.698039215686274,0.4);
#114268=COLOUR_RGB(
'MAS-255 Metallic Sheet - Precision Drive Spindle D5 (knob shaft)',0.913725490196078,
0.92156862745098,0.933333333333333);
#114269=COLOUR_RGB(
'MAS-255 Metallic Sheet - Spur Pinion m0.5 z16 with Hub',0.854901960784314,
0.866666666666667,0.886274509803922);
#114270=COLOUR_RGB(
'MAS-255 Metallic Sheet - Knurled Adjustment Knob D20',0.925490196078431,
0.933333333333333,0.941176470588235);
#114271=COLOUR_RGB(
'MAS-255 Metallic Sheet - Sintered Bronze Flanged Bush 5 x 9.6 x 8',0.745098039215686,
0.556862745098039,0.36078431372549);
#114272=COLOUR_RGB(
'MAS-255 Metallic Sheet - Carriage Drive Gear Rack m0.5 x 6 x 216',0.886274509803922,
0.898039215686275,0.913725490196078);
#114273=COLOUR_RGB(
'MAS-255 Metallic Sheet - Base Lock Knob Lever (stainless, bent)',0.917647058823529,
0.925490196078431,0.937254901960784);
#114274=COLOUR_RGB(
'MAS-255 Metallic Sheet - Scale Pointer - Vernier Plate',0.933333333333333,
0.937254901960784,0.945098039215686);
#114275=COLOUR_RGB(
'MAS-255 Metallic Sheet - ISO 1207 - M4 x 8 - 4.8 (Lock Clamp Scre',0.894117647058824,
0.901960784313726,0.913725490196078);
#114276=COLOUR_RGB(
'MAS-255 Metallic Sheet - ISO 4026 - M3 x 3 - 45H (Knob Set Screw)',0.780392156862745,
0.8,0.823529411764706);
#114277=COLOUR_RGB(
'MAS-255 Metallic Sheet - ISO 4026 - M2 x 2 - 45H (Pinion Set Scre',0.780392156862745,
0.8,0.823529411764706);
#114278=COLOUR_RGB(
'MAS-255 Metallic Sheet - ISO 4026 - M3 x 6 - 45H (Gib Adjustment',0.768627450980392,
0.788235294117647,0.815686274509804);
#114279=COLOUR_RGB(
'MAS-255 Metallic Sheet - ISO 4026 - M3 x 4 - 45H (Bush Retaining',0.780392156862745,
0.8,0.823529411764706);
#114280=COLOUR_RGB(
'MAS-255 Metallic Sheet - ISO 10642 - M2 x 4 - 10.9 (Pointer Screw',0.803921568627451,
0.819607843137255,0.843137254901961);
#114281=COLOUR_RGB(
'MAS-255 Metallic Sheet - ISO 4762 - M2.5 x 6 - 12.9 (Rack Screw)',0.792156862745098,
0.807843137254902,0.835294117647059);
#114282=COLOUR_RGB(
'MAS-255 Metallic Sheet - ISO 2338 - 2 m6 x 6 - St (Carriage Trave',0.843137254901961,
0.854901960784314,0.874509803921569);
#114283=COLOUR_RGB('Dark Blue',0.08,0.2,0.34);
#114284=FILL_AREA_STYLE_COLOUR('',#114283);
#114285=FILL_AREA_STYLE('',(#114284));
#114286=SURFACE_STYLE_FILL_AREA(#114285);
#114287=SURFACE_SIDE_STYLE('',(#114286));
#114288=SURFACE_STYLE_USAGE(.BOTH.,#114287);
#114289=PRESENTATION_STYLE_ASSIGNMENT((#114288));
#114290=COLOUR_RGB('Light Blue',0.38,0.62,0.78);
#114291=FILL_AREA_STYLE_COLOUR('',#114290);
#114292=FILL_AREA_STYLE('',(#114291));
#114293=SURFACE_STYLE_FILL_AREA(#114292);
#114294=SURFACE_SIDE_STYLE('',(#114293));
#114295=SURFACE_STYLE_USAGE(.BOTH.,#114294);
#114296=PRESENTATION_STYLE_ASSIGNMENT((#114295));
#114297=COLOUR_RGB('Sky Blue',0.24,0.69,0.87);
#114298=FILL_AREA_STYLE_COLOUR('',#114297);
#114299=FILL_AREA_STYLE('',(#114298));
#114300=SURFACE_STYLE_FILL_AREA(#114299);
#114301=SURFACE_SIDE_STYLE('',(#114300));
#114302=SURFACE_STYLE_USAGE(.BOTH.,#114301);
#114303=PRESENTATION_STYLE_ASSIGNMENT((#114302));
#114304=COLOUR_RGB('Grey',0.48,0.52,0.57);
#114305=FILL_AREA_STYLE_COLOUR('',#114304);
#114306=FILL_AREA_STYLE('',(#114305));
#114307=SURFACE_STYLE_FILL_AREA(#114306);
#114308=SURFACE_SIDE_STYLE('',(#114307));
#114309=SURFACE_STYLE_USAGE(.BOTH.,#114308);
#114310=PRESENTATION_STYLE_ASSIGNMENT((#114309));
#114311=COLOUR_RGB('Black',0.12,0.14,0.17);
#114312=FILL_AREA_STYLE_COLOUR('',#114311);
#114313=FILL_AREA_STYLE('',(#114312));
#114314=SURFACE_STYLE_FILL_AREA(#114313);
#114315=SURFACE_SIDE_STYLE('',(#114314));
#114316=SURFACE_STYLE_USAGE(.BOTH.,#114315);
#114317=PRESENTATION_STYLE_ASSIGNMENT((#114316));
#114318=COLOUR_RGB('Off White',0.89,0.88,0.83);
#114319=FILL_AREA_STYLE_COLOUR('',#114318);
#114320=FILL_AREA_STYLE('',(#114319));
#114321=SURFACE_STYLE_FILL_AREA(#114320);
#114322=SURFACE_SIDE_STYLE('',(#114321));
#114323=SURFACE_STYLE_USAGE(.BOTH.,#114322);
#114324=PRESENTATION_STYLE_ASSIGNMENT((#114323));
ENDSEC;
END-ISO-10303-21;
